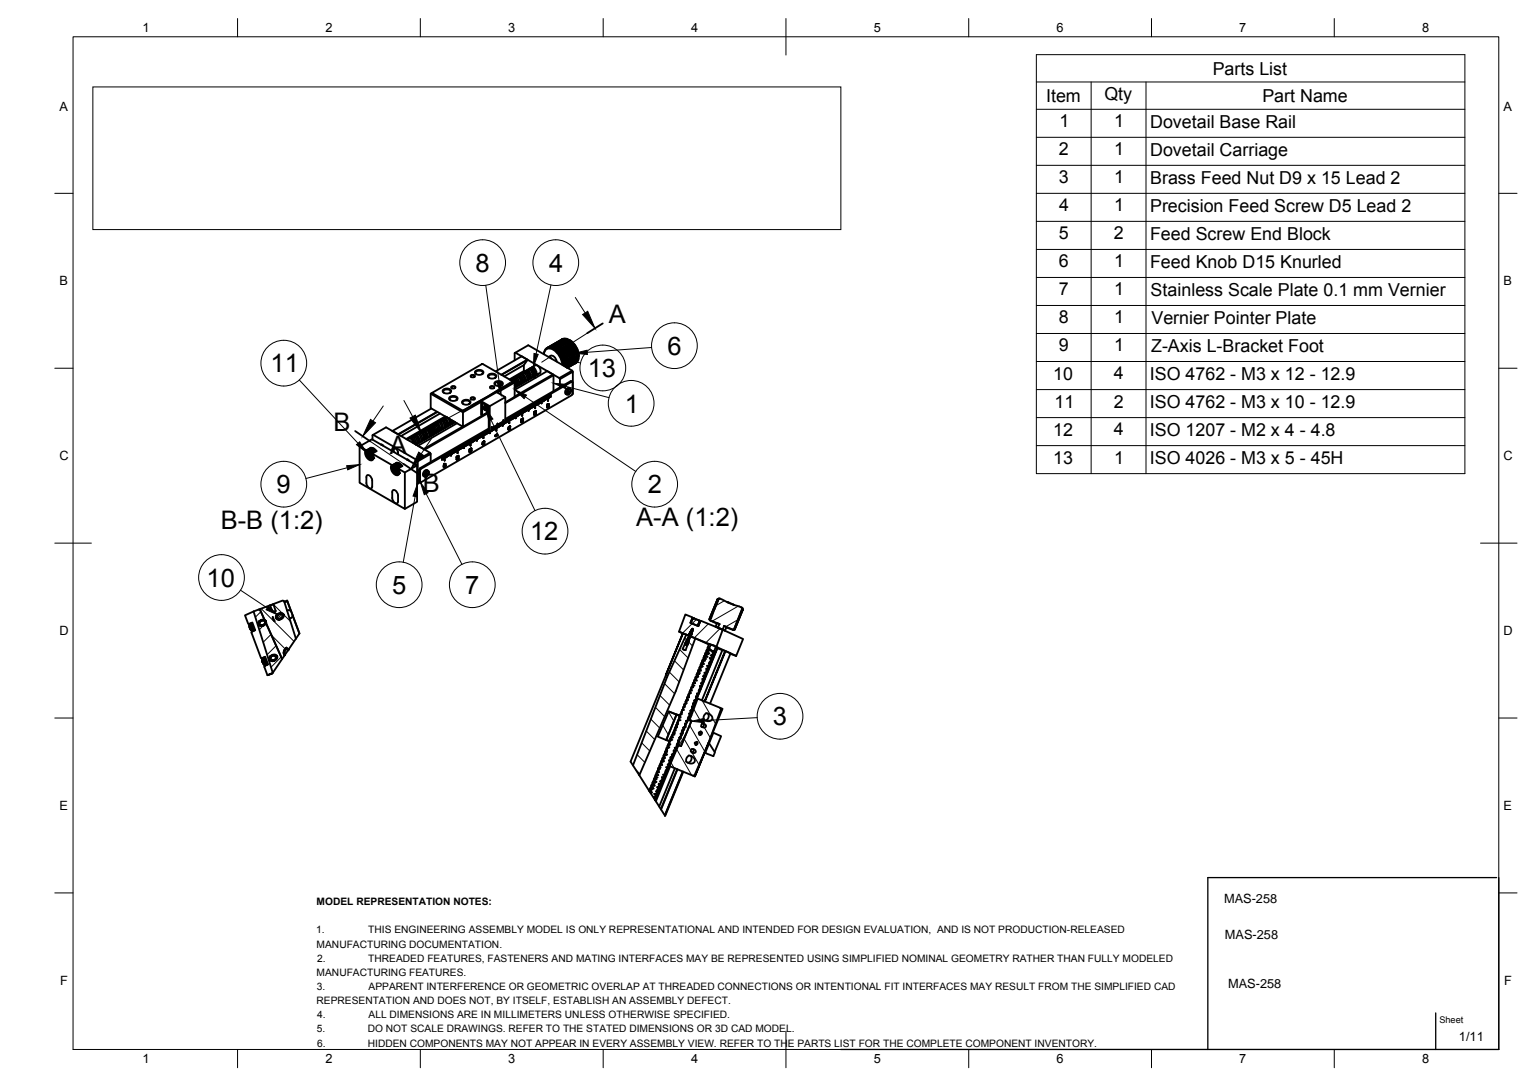
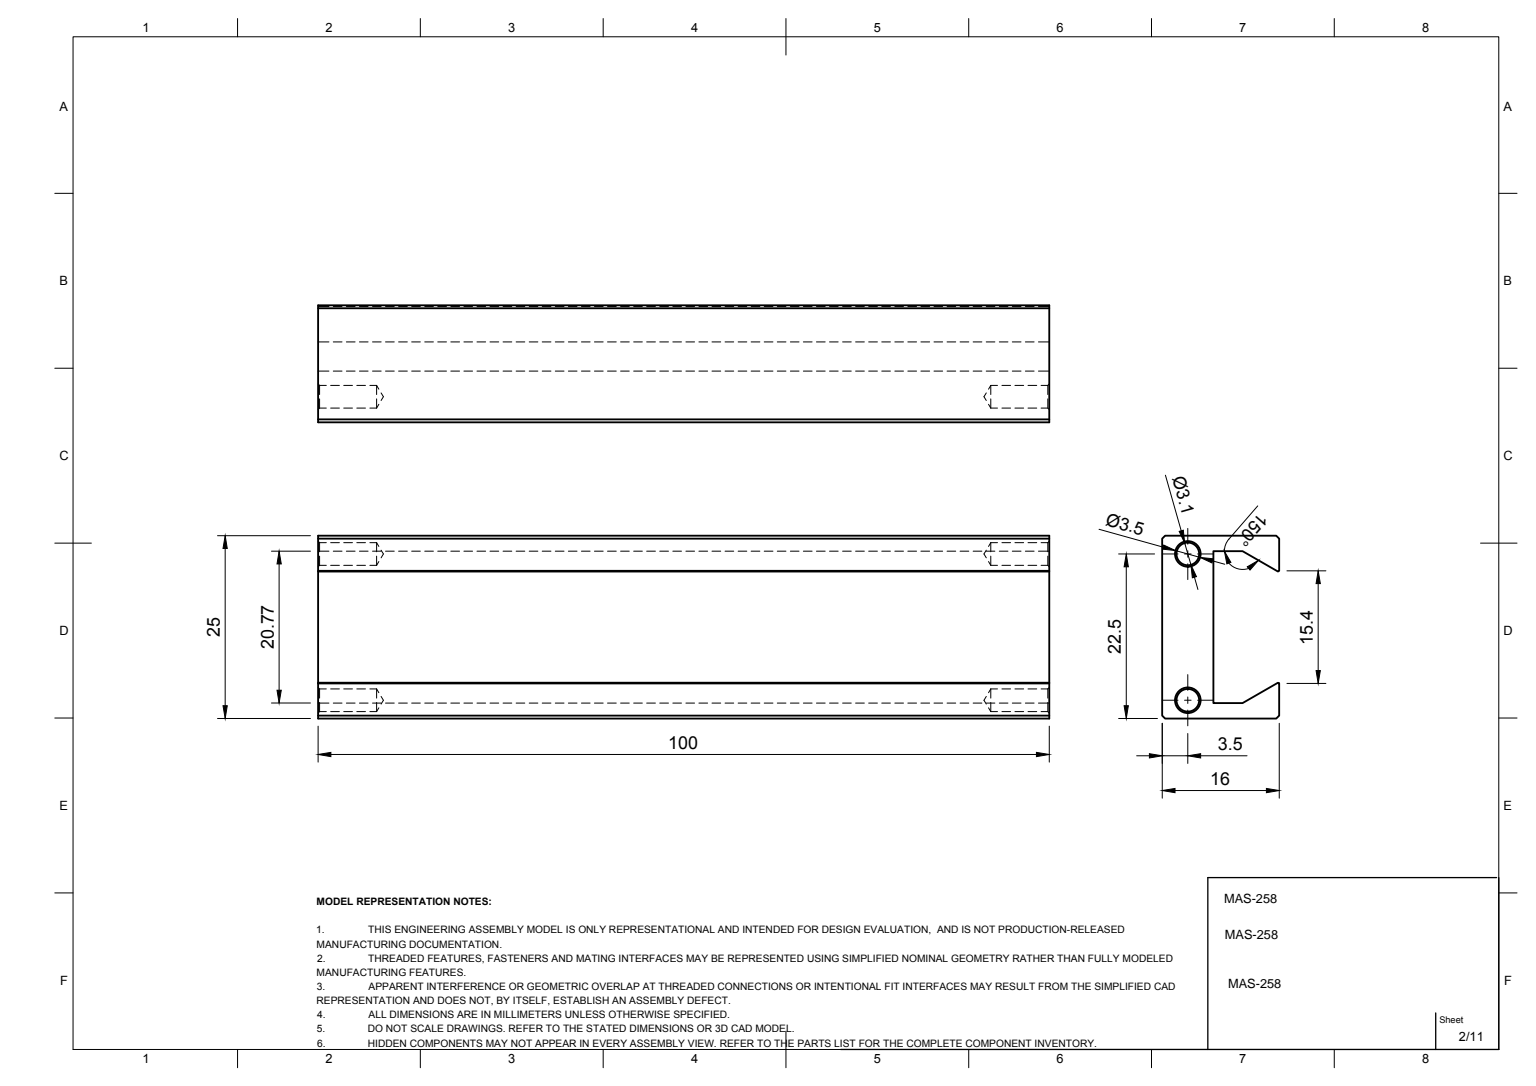
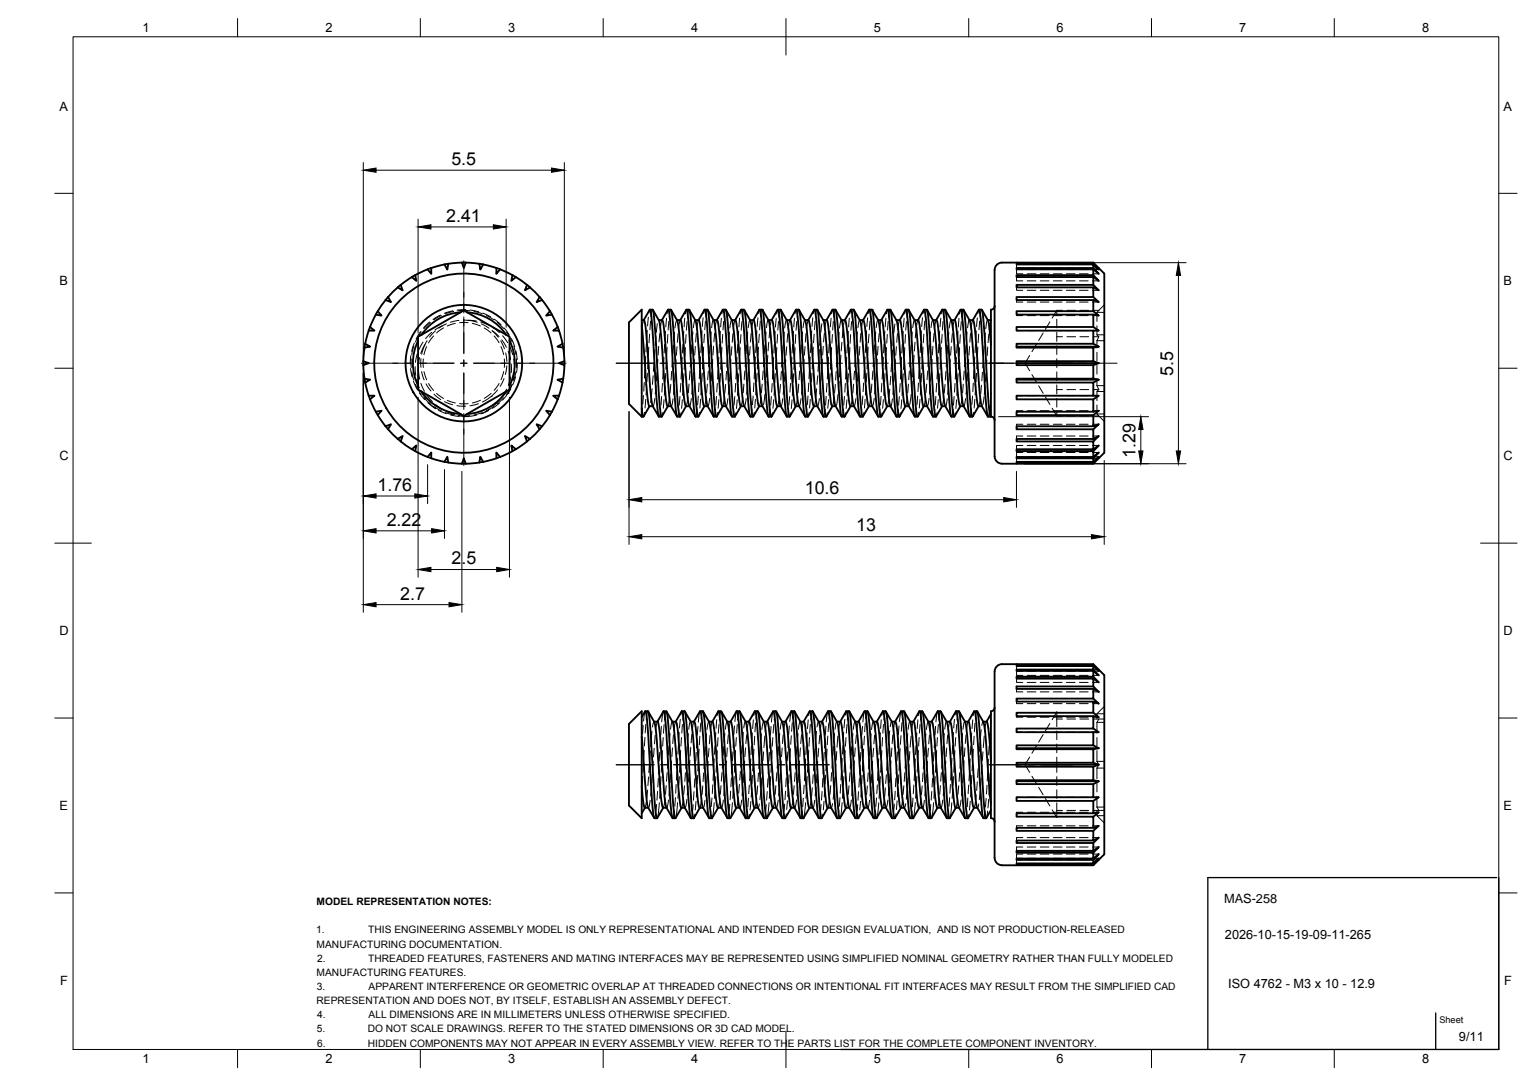
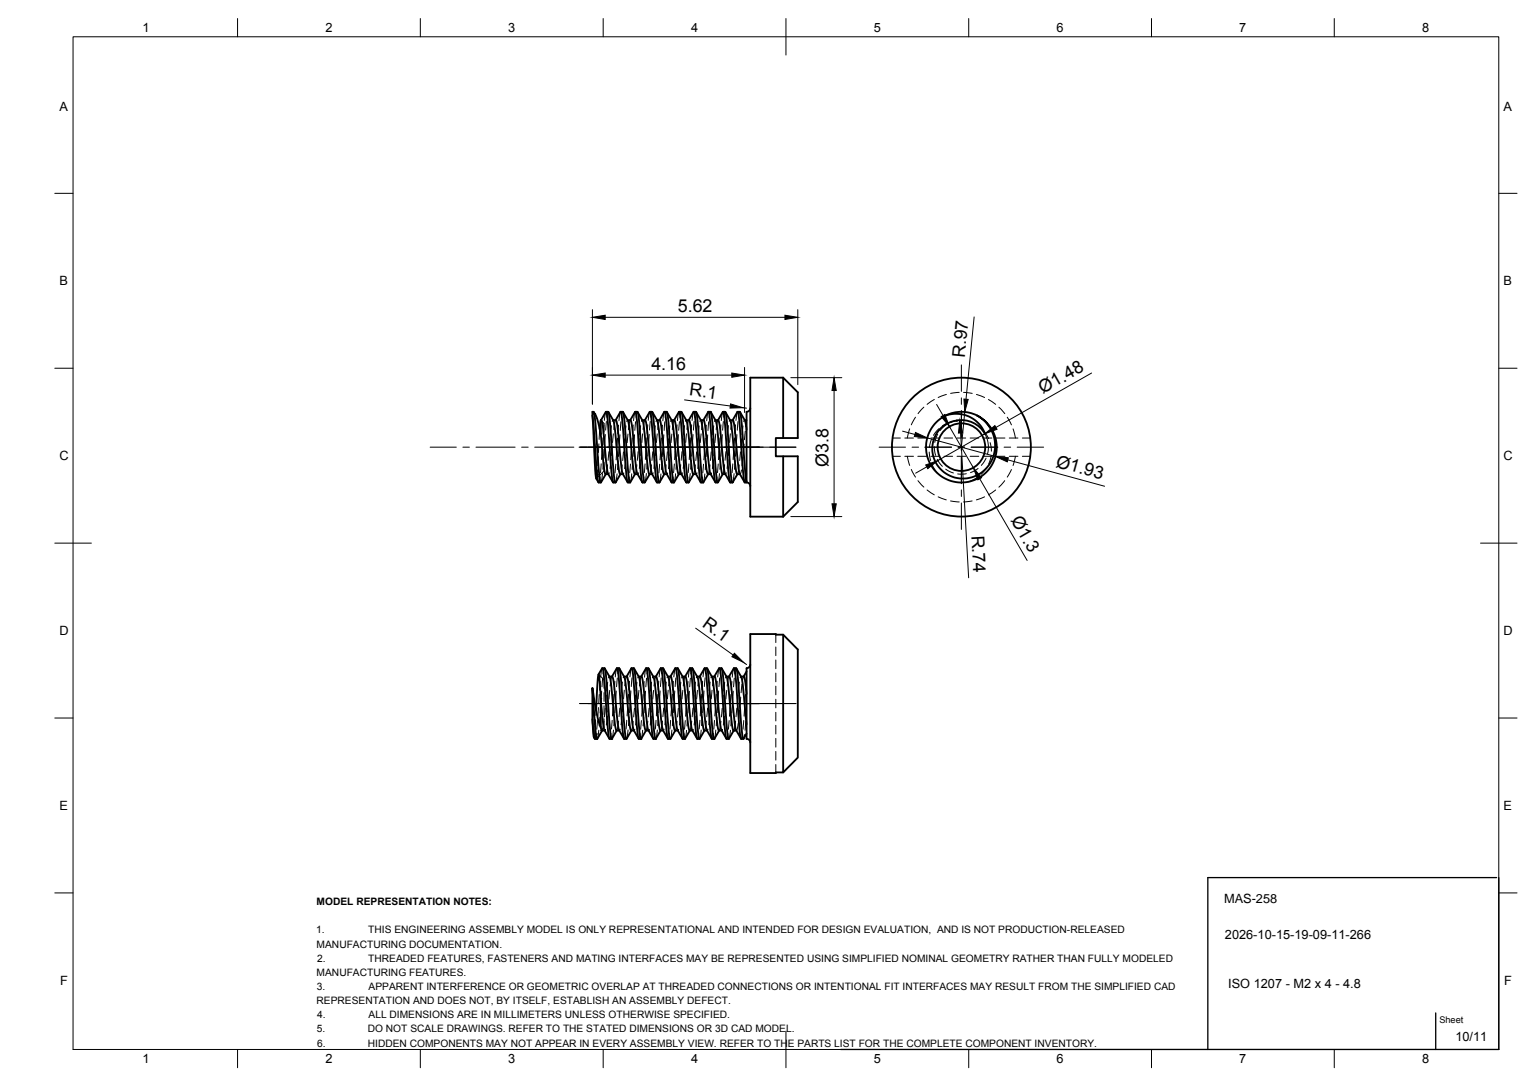
ISO-10303-21;
HEADER;
/* Generated by software containing ST-Developer
 * from STEP Tools, Inc. (www.steptools.com) 
 */

FILE_DESCRIPTION(
/* description */ (''),
/* implementation_level */ '2;1');

FILE_NAME(
/* name */ 'MAS-258',
/* time_stamp */ '2026-10-15T12:29:06-07:00',
/* author */ (''),
/* organization */ (''),
/* preprocessor_version */ 'ST-DEVELOPER v20.2',
/* originating_system */ 'Autodesk Translation Framework v15.15.0.0',
/* authorisation */ '');

FILE_SCHEMA (('AUTOMOTIVE_DESIGN { 1 0 10303 214 3 1 1 }'));
ENDSEC;

DATA;
#10=MECHANICAL_DESIGN_GEOMETRIC_PRESENTATION_REPRESENTATION('',(#1739,#1740,
#1741,#1742,#1743,#1744,#1745,#1746,#1747,#1748,#1749,#1750,#1751),#135282);
#11=ITEM_DEFINED_TRANSFORMATION($,$,#32233,#34203);
#12=ITEM_DEFINED_TRANSFORMATION($,$,#32276,#34204);
#13=ITEM_DEFINED_TRANSFORMATION($,$,#32384,#34205);
#14=ITEM_DEFINED_TRANSFORMATION($,$,#32403,#34206);
#15=ITEM_DEFINED_TRANSFORMATION($,$,#33493,#34207);
#16=ITEM_DEFINED_TRANSFORMATION($,$,#32477,#34208);
#17=ITEM_DEFINED_TRANSFORMATION($,$,#32757,#34209);
#18=ITEM_DEFINED_TRANSFORMATION($,$,#33287,#34210);
#19=ITEM_DEFINED_TRANSFORMATION($,$,#33359,#34211);
#20=ITEM_DEFINED_TRANSFORMATION($,$,#33555,#34212);
#21=ITEM_DEFINED_TRANSFORMATION($,$,#33856,#34213);
#22=ITEM_DEFINED_TRANSFORMATION($,$,#34149,#34214);
#23=ITEM_DEFINED_TRANSFORMATION($,$,#33412,#34215);
#24=ITEM_DEFINED_TRANSFORMATION($,$,#33493,#34216);
#25=ITEM_DEFINED_TRANSFORMATION($,$,#33555,#34217);
#26=ITEM_DEFINED_TRANSFORMATION($,$,#33555,#34218);
#27=ITEM_DEFINED_TRANSFORMATION($,$,#33555,#34219);
#28=ITEM_DEFINED_TRANSFORMATION($,$,#33856,#34220);
#29=ITEM_DEFINED_TRANSFORMATION($,$,#34149,#34221);
#30=ITEM_DEFINED_TRANSFORMATION($,$,#34149,#34222);
#31=ITEM_DEFINED_TRANSFORMATION($,$,#34149,#34223);
#32=(
REPRESENTATION_RELATIONSHIP($,$,#135337,#135336)
REPRESENTATION_RELATIONSHIP_WITH_TRANSFORMATION(#11)
SHAPE_REPRESENTATION_RELATIONSHIP()
);
#33=(
REPRESENTATION_RELATIONSHIP($,$,#135338,#135336)
REPRESENTATION_RELATIONSHIP_WITH_TRANSFORMATION(#12)
SHAPE_REPRESENTATION_RELATIONSHIP()
);
#34=(
REPRESENTATION_RELATIONSHIP($,$,#135339,#135336)
REPRESENTATION_RELATIONSHIP_WITH_TRANSFORMATION(#13)
SHAPE_REPRESENTATION_RELATIONSHIP()
);
#35=(
REPRESENTATION_RELATIONSHIP($,$,#135340,#135336)
REPRESENTATION_RELATIONSHIP_WITH_TRANSFORMATION(#14)
SHAPE_REPRESENTATION_RELATIONSHIP()
);
#36=(
REPRESENTATION_RELATIONSHIP($,$,#135346,#135336)
REPRESENTATION_RELATIONSHIP_WITH_TRANSFORMATION(#15)
SHAPE_REPRESENTATION_RELATIONSHIP()
);
#37=(
REPRESENTATION_RELATIONSHIP($,$,#135341,#135336)
REPRESENTATION_RELATIONSHIP_WITH_TRANSFORMATION(#16)
SHAPE_REPRESENTATION_RELATIONSHIP()
);
#38=(
REPRESENTATION_RELATIONSHIP($,$,#135342,#135336)
REPRESENTATION_RELATIONSHIP_WITH_TRANSFORMATION(#17)
SHAPE_REPRESENTATION_RELATIONSHIP()
);
#39=(
REPRESENTATION_RELATIONSHIP($,$,#135343,#135336)
REPRESENTATION_RELATIONSHIP_WITH_TRANSFORMATION(#18)
SHAPE_REPRESENTATION_RELATIONSHIP()
);
#40=(
REPRESENTATION_RELATIONSHIP($,$,#135344,#135336)
REPRESENTATION_RELATIONSHIP_WITH_TRANSFORMATION(#19)
SHAPE_REPRESENTATION_RELATIONSHIP()
);
#41=(
REPRESENTATION_RELATIONSHIP($,$,#135347,#135336)
REPRESENTATION_RELATIONSHIP_WITH_TRANSFORMATION(#20)
SHAPE_REPRESENTATION_RELATIONSHIP()
);
#42=(
REPRESENTATION_RELATIONSHIP($,$,#135348,#135336)
REPRESENTATION_RELATIONSHIP_WITH_TRANSFORMATION(#21)
SHAPE_REPRESENTATION_RELATIONSHIP()
);
#43=(
REPRESENTATION_RELATIONSHIP($,$,#135349,#135336)
REPRESENTATION_RELATIONSHIP_WITH_TRANSFORMATION(#22)
SHAPE_REPRESENTATION_RELATIONSHIP()
);
#44=(
REPRESENTATION_RELATIONSHIP($,$,#135345,#135336)
REPRESENTATION_RELATIONSHIP_WITH_TRANSFORMATION(#23)
SHAPE_REPRESENTATION_RELATIONSHIP()
);
#45=(
REPRESENTATION_RELATIONSHIP($,$,#135346,#135336)
REPRESENTATION_RELATIONSHIP_WITH_TRANSFORMATION(#24)
SHAPE_REPRESENTATION_RELATIONSHIP()
);
#46=(
REPRESENTATION_RELATIONSHIP($,$,#135347,#135336)
REPRESENTATION_RELATIONSHIP_WITH_TRANSFORMATION(#25)
SHAPE_REPRESENTATION_RELATIONSHIP()
);
#47=(
REPRESENTATION_RELATIONSHIP($,$,#135347,#135336)
REPRESENTATION_RELATIONSHIP_WITH_TRANSFORMATION(#26)
SHAPE_REPRESENTATION_RELATIONSHIP()
);
#48=(
REPRESENTATION_RELATIONSHIP($,$,#135347,#135336)
REPRESENTATION_RELATIONSHIP_WITH_TRANSFORMATION(#27)
SHAPE_REPRESENTATION_RELATIONSHIP()
);
#49=(
REPRESENTATION_RELATIONSHIP($,$,#135348,#135336)
REPRESENTATION_RELATIONSHIP_WITH_TRANSFORMATION(#28)
SHAPE_REPRESENTATION_RELATIONSHIP()
);
#50=(
REPRESENTATION_RELATIONSHIP($,$,#135349,#135336)
REPRESENTATION_RELATIONSHIP_WITH_TRANSFORMATION(#29)
SHAPE_REPRESENTATION_RELATIONSHIP()
);
#51=(
REPRESENTATION_RELATIONSHIP($,$,#135349,#135336)
REPRESENTATION_RELATIONSHIP_WITH_TRANSFORMATION(#30)
SHAPE_REPRESENTATION_RELATIONSHIP()
);
#52=(
REPRESENTATION_RELATIONSHIP($,$,#135349,#135336)
REPRESENTATION_RELATIONSHIP_WITH_TRANSFORMATION(#31)
SHAPE_REPRESENTATION_RELATIONSHIP()
);
#53=CONTEXT_DEPENDENT_SHAPE_REPRESENTATION(#32,#135315);
#54=CONTEXT_DEPENDENT_SHAPE_REPRESENTATION(#33,#135316);
#55=CONTEXT_DEPENDENT_SHAPE_REPRESENTATION(#34,#135317);
#56=CONTEXT_DEPENDENT_SHAPE_REPRESENTATION(#35,#135318);
#57=CONTEXT_DEPENDENT_SHAPE_REPRESENTATION(#36,#135319);
#58=CONTEXT_DEPENDENT_SHAPE_REPRESENTATION(#37,#135320);
#59=CONTEXT_DEPENDENT_SHAPE_REPRESENTATION(#38,#135321);
#60=CONTEXT_DEPENDENT_SHAPE_REPRESENTATION(#39,#135322);
#61=CONTEXT_DEPENDENT_SHAPE_REPRESENTATION(#40,#135323);
#62=CONTEXT_DEPENDENT_SHAPE_REPRESENTATION(#41,#135324);
#63=CONTEXT_DEPENDENT_SHAPE_REPRESENTATION(#42,#135325);
#64=CONTEXT_DEPENDENT_SHAPE_REPRESENTATION(#43,#135326);
#65=CONTEXT_DEPENDENT_SHAPE_REPRESENTATION(#44,#135327);
#66=CONTEXT_DEPENDENT_SHAPE_REPRESENTATION(#45,#135328);
#67=CONTEXT_DEPENDENT_SHAPE_REPRESENTATION(#46,#135329);
#68=CONTEXT_DEPENDENT_SHAPE_REPRESENTATION(#47,#135330);
#69=CONTEXT_DEPENDENT_SHAPE_REPRESENTATION(#48,#135331);
#70=CONTEXT_DEPENDENT_SHAPE_REPRESENTATION(#49,#135332);
#71=CONTEXT_DEPENDENT_SHAPE_REPRESENTATION(#50,#135333);
#72=CONTEXT_DEPENDENT_SHAPE_REPRESENTATION(#51,#135334);
#73=CONTEXT_DEPENDENT_SHAPE_REPRESENTATION(#52,#135335);
#74=NEXT_ASSEMBLY_USAGE_OCCURRENCE('Dovetail Base Rail:1',
'Dovetail Base Rail:1','Dovetail Base Rail:1',#135351,#135352,
'Dovetail Base Rail:1');
#75=NEXT_ASSEMBLY_USAGE_OCCURRENCE('Dovetail Carriage:1',
'Dovetail Carriage:1','Dovetail Carriage:1',#135351,#135353,
'Dovetail Carriage:1');
#76=NEXT_ASSEMBLY_USAGE_OCCURRENCE('Brass Feed Nut D9 x 15 Lead 2:1',
'Brass Feed Nut D9 x 15 Lead 2:1','Brass Feed Nut D9 x 15 Lead 2:1',#135351,
#135354,'Brass Feed Nut D9 x 15 Lead 2:1');
#77=NEXT_ASSEMBLY_USAGE_OCCURRENCE('Precision Feed Screw D5 Lead 2:1',
'Precision Feed Screw D5 Lead 2:1','Precision Feed Screw D5 Lead 2:1',#135351,
#135355,'Precision Feed Screw D5 Lead 2:1');
#78=NEXT_ASSEMBLY_USAGE_OCCURRENCE('Feed Screw End Block:1',
'Feed Screw End Block:1','Feed Screw End Block:1',#135351,#135361,
'Feed Screw End Block:1');
#79=NEXT_ASSEMBLY_USAGE_OCCURRENCE('Feed Knob D15 Knurled:1',
'Feed Knob D15 Knurled:1','Feed Knob D15 Knurled:1',#135351,#135356,
'Feed Knob D15 Knurled:1');
#80=NEXT_ASSEMBLY_USAGE_OCCURRENCE(
'Stainless Scale Plate 0.1 mm Vernier:1',
'Stainless Scale Plate 0.1 mm Vernier:1',
'Stainless Scale Plate 0.1 mm Vernier:1',#135351,#135357,
'Stainless Scale Plate 0.1 mm Vernier:1');
#81=NEXT_ASSEMBLY_USAGE_OCCURRENCE('Vernier Pointer Plate:1',
'Vernier Pointer Plate:1','Vernier Pointer Plate:1',#135351,#135358,
'Vernier Pointer Plate:1');
#82=NEXT_ASSEMBLY_USAGE_OCCURRENCE('Z-Axis L-Bracket Foot:1',
'Z-Axis L-Bracket Foot:1','Z-Axis L-Bracket Foot:1',#135351,#135359,
'Z-Axis L-Bracket Foot:1');
#83=NEXT_ASSEMBLY_USAGE_OCCURRENCE('ISO 4762 - M3 x 12 - 12.9:1',
'ISO 4762 - M3 x 12 - 12.9:1','ISO 4762 - M3 x 12 - 12.9:1',#135351,#135362,
'ISO 4762 - M3 x 12 - 12.9:1');
#84=NEXT_ASSEMBLY_USAGE_OCCURRENCE('ISO 4762 - M3 x 10 - 12.9:1',
'ISO 4762 - M3 x 10 - 12.9:1','ISO 4762 - M3 x 10 - 12.9:1',#135351,#135363,
'ISO 4762 - M3 x 10 - 12.9:1');
#85=NEXT_ASSEMBLY_USAGE_OCCURRENCE('ISO 1207 - M2 x 4 - 4.8:1',
'ISO 1207 - M2 x 4 - 4.8:1','ISO 1207 - M2 x 4 - 4.8:1',#135351,#135364,
'ISO 1207 - M2 x 4 - 4.8:1');
#86=NEXT_ASSEMBLY_USAGE_OCCURRENCE('ISO 4026 - M3 x 5 - 45H:1',
'ISO 4026 - M3 x 5 - 45H:1','ISO 4026 - M3 x 5 - 45H:1',#135351,#135360,
'ISO 4026 - M3 x 5 - 45H:1');
#87=NEXT_ASSEMBLY_USAGE_OCCURRENCE('Feed Screw End Block:2',
'Feed Screw End Block:2','Feed Screw End Block:2',#135351,#135361,
'Feed Screw End Block:2');
#88=NEXT_ASSEMBLY_USAGE_OCCURRENCE('ISO 4762 - M3 x 12 - 12.9:2',
'ISO 4762 - M3 x 12 - 12.9:2','ISO 4762 - M3 x 12 - 12.9:2',#135351,#135362,
'ISO 4762 - M3 x 12 - 12.9:2');
#89=NEXT_ASSEMBLY_USAGE_OCCURRENCE('ISO 4762 - M3 x 12 - 12.9:3',
'ISO 4762 - M3 x 12 - 12.9:3','ISO 4762 - M3 x 12 - 12.9:3',#135351,#135362,
'ISO 4762 - M3 x 12 - 12.9:3');
#90=NEXT_ASSEMBLY_USAGE_OCCURRENCE('ISO 4762 - M3 x 12 - 12.9:4',
'ISO 4762 - M3 x 12 - 12.9:4','ISO 4762 - M3 x 12 - 12.9:4',#135351,#135362,
'ISO 4762 - M3 x 12 - 12.9:4');
#91=NEXT_ASSEMBLY_USAGE_OCCURRENCE('ISO 4762 - M3 x 10 - 12.9:2',
'ISO 4762 - M3 x 10 - 12.9:2','ISO 4762 - M3 x 10 - 12.9:2',#135351,#135363,
'ISO 4762 - M3 x 10 - 12.9:2');
#92=NEXT_ASSEMBLY_USAGE_OCCURRENCE('ISO 1207 - M2 x 4 - 4.8:2',
'ISO 1207 - M2 x 4 - 4.8:2','ISO 1207 - M2 x 4 - 4.8:2',#135351,#135364,
'ISO 1207 - M2 x 4 - 4.8:2');
#93=NEXT_ASSEMBLY_USAGE_OCCURRENCE('ISO 1207 - M2 x 4 - 4.8:3',
'ISO 1207 - M2 x 4 - 4.8:3','ISO 1207 - M2 x 4 - 4.8:3',#135351,#135364,
'ISO 1207 - M2 x 4 - 4.8:3');
#94=NEXT_ASSEMBLY_USAGE_OCCURRENCE('ISO 1207 - M2 x 4 - 4.8:4',
'ISO 1207 - M2 x 4 - 4.8:4','ISO 1207 - M2 x 4 - 4.8:4',#135351,#135364,
'ISO 1207 - M2 x 4 - 4.8:4');
#95=TOROIDAL_SURFACE('',#33614,1.5635,0.1);
#96=TOROIDAL_SURFACE('',#33808,2.55,0.2);
#97=TOROIDAL_SURFACE('',#33907,1.5635,0.1);
#98=TOROIDAL_SURFACE('',#34101,2.55,0.2);
#99=TOROIDAL_SURFACE('',#34180,1.06675,0.1);
#100=(
BOUNDED_CURVE()
B_SPLINE_CURVE(2,(#76990,#76991,#76992),.UNSPECIFIED.,.F.,.F.)
B_SPLINE_CURVE_WITH_KNOTS((3,3),(0.557415897727321,0.585832740635072),
 .UNSPECIFIED.)
CURVE()
GEOMETRIC_REPRESENTATION_ITEM()
RATIONAL_B_SPLINE_CURVE((1.06,1.03152938818342,1.))
REPRESENTATION_ITEM('')
);
#101=(
BOUNDED_CURVE()
B_SPLINE_CURVE(2,(#76996,#76997,#76998),.UNSPECIFIED.,.F.,.F.)
B_SPLINE_CURVE_WITH_KNOTS((3,3),(0.,0.0284168429077509),.UNSPECIFIED.)
CURVE()
GEOMETRIC_REPRESENTATION_ITEM()
RATIONAL_B_SPLINE_CURVE((1.,1.03152938818342,1.06))
REPRESENTATION_ITEM('')
);
#102=(
BOUNDED_CURVE()
B_SPLINE_CURVE(2,(#77032,#77033,#77034),.UNSPECIFIED.,.F.,.F.)
B_SPLINE_CURVE_WITH_KNOTS((3,3),(0.557415897727321,0.585832740635072),
 .UNSPECIFIED.)
CURVE()
GEOMETRIC_REPRESENTATION_ITEM()
RATIONAL_B_SPLINE_CURVE((1.06,1.03152938818342,1.))
REPRESENTATION_ITEM('')
);
#103=(
BOUNDED_CURVE()
B_SPLINE_CURVE(2,(#77036,#77037,#77038),.UNSPECIFIED.,.F.,.F.)
B_SPLINE_CURVE_WITH_KNOTS((3,3),(0.,0.028416842907751),.UNSPECIFIED.)
CURVE()
GEOMETRIC_REPRESENTATION_ITEM()
RATIONAL_B_SPLINE_CURVE((1.,1.03152938818342,1.06))
REPRESENTATION_ITEM('')
);
#104=(
BOUNDED_CURVE()
B_SPLINE_CURVE(2,(#84021,#84022,#84023),.UNSPECIFIED.,.F.,.F.)
B_SPLINE_CURVE_WITH_KNOTS((3,3),(0.,0.0136874154102722),.UNSPECIFIED.)
CURVE()
GEOMETRIC_REPRESENTATION_ITEM()
RATIONAL_B_SPLINE_CURVE((1.,1.00669106236244,1.00897713804967))
REPRESENTATION_ITEM('')
);
#105=(
BOUNDED_CURVE()
B_SPLINE_CURVE(2,(#84027,#84028,#84029),.UNSPECIFIED.,.F.,.F.)
B_SPLINE_CURVE_WITH_KNOTS((3,3),(0.0278942541126666,0.0415816695229379),
 .UNSPECIFIED.)
CURVE()
GEOMETRIC_REPRESENTATION_ITEM()
RATIONAL_B_SPLINE_CURVE((1.00897713804926,1.00669106236213,1.))
REPRESENTATION_ITEM('')
);
#106=(
BOUNDED_CURVE()
B_SPLINE_CURVE(2,(#84031,#84032,#84033),.UNSPECIFIED.,.F.,.F.)
B_SPLINE_CURVE_WITH_KNOTS((3,3),(0.,0.0136874154102634),.UNSPECIFIED.)
CURVE()
GEOMETRIC_REPRESENTATION_ITEM()
RATIONAL_B_SPLINE_CURVE((1.,1.00669106236278,1.00897713805013))
REPRESENTATION_ITEM('')
);
#107=(
BOUNDED_CURVE()
B_SPLINE_CURVE(2,(#84037,#84038,#84039),.UNSPECIFIED.,.F.,.F.)
B_SPLINE_CURVE_WITH_KNOTS((3,3),(0.0278942541126795,0.04158166952294),
 .UNSPECIFIED.)
CURVE()
GEOMETRIC_REPRESENTATION_ITEM()
RATIONAL_B_SPLINE_CURVE((1.00897713805013,1.00669106236278,1.))
REPRESENTATION_ITEM('')
);
#108=(
BOUNDED_CURVE()
B_SPLINE_CURVE(2,(#84041,#84042,#84043),.UNSPECIFIED.,.F.,.F.)
B_SPLINE_CURVE_WITH_KNOTS((3,3),(0.,0.0136874154102606),.UNSPECIFIED.)
CURVE()
GEOMETRIC_REPRESENTATION_ITEM()
RATIONAL_B_SPLINE_CURVE((1.,1.00669106236282,1.00897713805019))
REPRESENTATION_ITEM('')
);
#109=(
BOUNDED_CURVE()
B_SPLINE_CURVE(2,(#84047,#84048,#84049),.UNSPECIFIED.,.F.,.F.)
B_SPLINE_CURVE_WITH_KNOTS((3,3),(0.0278942541126748,0.0415816695229379),
 .UNSPECIFIED.)
CURVE()
GEOMETRIC_REPRESENTATION_ITEM()
RATIONAL_B_SPLINE_CURVE((1.00897713805094,1.00669106236338,1.))
REPRESENTATION_ITEM('')
);
#110=(
BOUNDED_CURVE()
B_SPLINE_CURVE(2,(#84051,#84052,#84053),.UNSPECIFIED.,.F.,.F.)
B_SPLINE_CURVE_WITH_KNOTS((3,3),(0.,0.0136874154102637),.UNSPECIFIED.)
CURVE()
GEOMETRIC_REPRESENTATION_ITEM()
RATIONAL_B_SPLINE_CURVE((1.,1.00669106236329,1.00897713805081))
REPRESENTATION_ITEM('')
);
#111=(
BOUNDED_CURVE()
B_SPLINE_CURVE(2,(#84057,#84058,#84059),.UNSPECIFIED.,.F.,.F.)
B_SPLINE_CURVE_WITH_KNOTS((3,3),(0.0278942541126709,0.0415816695229372),
 .UNSPECIFIED.)
CURVE()
GEOMETRIC_REPRESENTATION_ITEM()
RATIONAL_B_SPLINE_CURVE((1.0089771380492,1.00669106236209,1.))
REPRESENTATION_ITEM('')
);
#112=(
BOUNDED_CURVE()
B_SPLINE_CURVE(2,(#84061,#84062,#84063),.UNSPECIFIED.,.F.,.F.)
B_SPLINE_CURVE_WITH_KNOTS((3,3),(0.,0.0136874154102607),.UNSPECIFIED.)
CURVE()
GEOMETRIC_REPRESENTATION_ITEM()
RATIONAL_B_SPLINE_CURVE((1.,1.00669106236278,1.00897713805013))
REPRESENTATION_ITEM('')
);
#113=(
BOUNDED_CURVE()
B_SPLINE_CURVE(2,(#84067,#84068,#84069),.UNSPECIFIED.,.F.,.F.)
B_SPLINE_CURVE_WITH_KNOTS((3,3),(0.0278942541126766,0.04158166952294),
 .UNSPECIFIED.)
CURVE()
GEOMETRIC_REPRESENTATION_ITEM()
RATIONAL_B_SPLINE_CURVE((1.00897713805013,1.00669106236278,1.))
REPRESENTATION_ITEM('')
);
#114=(
BOUNDED_CURVE()
B_SPLINE_CURVE(2,(#84071,#84072,#84073),.UNSPECIFIED.,.F.,.F.)
B_SPLINE_CURVE_WITH_KNOTS((3,3),(0.,0.0136874154102674),.UNSPECIFIED.)
CURVE()
GEOMETRIC_REPRESENTATION_ITEM()
RATIONAL_B_SPLINE_CURVE((1.,1.0066910623627,1.00897713805002))
REPRESENTATION_ITEM('')
);
#115=(
BOUNDED_CURVE()
B_SPLINE_CURVE(2,(#84076,#84077,#84078),.UNSPECIFIED.,.F.,.F.)
B_SPLINE_CURVE_WITH_KNOTS((3,3),(0.0278942541126671,0.0415816695229421),
 .UNSPECIFIED.)
CURVE()
GEOMETRIC_REPRESENTATION_ITEM()
RATIONAL_B_SPLINE_CURVE((1.00897713804893,1.00669106236189,1.))
REPRESENTATION_ITEM('')
);
#116=(
BOUNDED_CURVE()
B_SPLINE_CURVE(2,(#106679,#106680,#106681),.UNSPECIFIED.,.F.,.F.)
B_SPLINE_CURVE_WITH_KNOTS((3,3),(0.,0.0211644268265385),.UNSPECIFIED.)
CURVE()
GEOMETRIC_REPRESENTATION_ITEM()
RATIONAL_B_SPLINE_CURVE((1.,1.0009097917251,1.00093939181347))
REPRESENTATION_ITEM('')
);
#117=(
BOUNDED_CURVE()
B_SPLINE_CURVE(2,(#106685,#106686,#106687),.UNSPECIFIED.,.F.,.F.)
B_SPLINE_CURVE_WITH_KNOTS((3,3),(0.022587909800554,0.0437523366271111),
 .UNSPECIFIED.)
CURVE()
GEOMETRIC_REPRESENTATION_ITEM()
RATIONAL_B_SPLINE_CURVE((1.00093939181258,1.00090979172423,1.))
REPRESENTATION_ITEM('')
);
#118=(
BOUNDED_CURVE()
B_SPLINE_CURVE(2,(#106982,#106983,#106984),.UNSPECIFIED.,.F.,.F.)
B_SPLINE_CURVE_WITH_KNOTS((3,3),(0.,0.0211644268265826),.UNSPECIFIED.)
CURVE()
GEOMETRIC_REPRESENTATION_ITEM()
RATIONAL_B_SPLINE_CURVE((1.,1.00090979172134,1.00093939180958))
REPRESENTATION_ITEM('')
);
#119=(
BOUNDED_CURVE()
B_SPLINE_CURVE(2,(#106986,#106987,#106988),.UNSPECIFIED.,.F.,.F.)
B_SPLINE_CURVE_WITH_KNOTS((3,3),(0.0225879098005743,0.043752336627111),
 .UNSPECIFIED.)
CURVE()
GEOMETRIC_REPRESENTATION_ITEM()
RATIONAL_B_SPLINE_CURVE((1.00093939181478,1.00090979172637,1.))
REPRESENTATION_ITEM('')
);
#120=(
BOUNDED_CURVE()
B_SPLINE_CURVE(2,(#106993,#106994,#106995),.UNSPECIFIED.,.F.,.F.)
B_SPLINE_CURVE_WITH_KNOTS((3,3),(0.0225879098005881,0.043752336627111),
 .UNSPECIFIED.)
CURVE()
GEOMETRIC_REPRESENTATION_ITEM()
RATIONAL_B_SPLINE_CURVE((1.00093939180782,1.00090979171963,1.))
REPRESENTATION_ITEM('')
);
#121=(
BOUNDED_CURVE()
B_SPLINE_CURVE(2,(#106997,#106998,#106999),.UNSPECIFIED.,.F.,.F.)
B_SPLINE_CURVE_WITH_KNOTS((3,3),(0.,0.021164426826593),.UNSPECIFIED.)
CURVE()
GEOMETRIC_REPRESENTATION_ITEM()
RATIONAL_B_SPLINE_CURVE((1.,1.0009097917242,1.00093939181253))
REPRESENTATION_ITEM('')
);
#122=(
BOUNDED_CURVE()
B_SPLINE_CURVE(2,(#107000,#107001,#107002),.UNSPECIFIED.,.F.,.F.)
B_SPLINE_CURVE_WITH_KNOTS((3,3),(0.0225879098005839,0.0437523366271112),
 .UNSPECIFIED.)
CURVE()
GEOMETRIC_REPRESENTATION_ITEM()
RATIONAL_B_SPLINE_CURVE((1.00093939180822,1.00090979172002,1.))
REPRESENTATION_ITEM('')
);
#123=(
BOUNDED_CURVE()
B_SPLINE_CURVE(2,(#107004,#107005,#107006),.UNSPECIFIED.,.F.,.F.)
B_SPLINE_CURVE_WITH_KNOTS((3,3),(0.,0.0211644268265428),.UNSPECIFIED.)
CURVE()
GEOMETRIC_REPRESENTATION_ITEM()
RATIONAL_B_SPLINE_CURVE((1.,1.00090979172612,1.00093939181452))
REPRESENTATION_ITEM('')
);
#124=(
BOUNDED_CURVE()
B_SPLINE_CURVE(2,(#107007,#107008,#107009),.UNSPECIFIED.,.F.,.F.)
B_SPLINE_CURVE_WITH_KNOTS((3,3),(0.0225879098005574,0.0437523366271111),
 .UNSPECIFIED.)
CURVE()
GEOMETRIC_REPRESENTATION_ITEM()
RATIONAL_B_SPLINE_CURVE((1.00093939181255,1.00090979172421,1.))
REPRESENTATION_ITEM('')
);
#125=(
BOUNDED_CURVE()
B_SPLINE_CURVE(2,(#107011,#107012,#107013),.UNSPECIFIED.,.F.,.F.)
B_SPLINE_CURVE_WITH_KNOTS((3,3),(0.,0.0211644268266003),.UNSPECIFIED.)
CURVE()
GEOMETRIC_REPRESENTATION_ITEM()
RATIONAL_B_SPLINE_CURVE((1.,1.0009097917207,1.00093939180893))
REPRESENTATION_ITEM('')
);
#126=(
BOUNDED_CURVE()
B_SPLINE_CURVE(2,(#107014,#107015,#107016),.UNSPECIFIED.,.F.,.F.)
B_SPLINE_CURVE_WITH_KNOTS((3,3),(0.022587909800539,0.0437523366271111),
 .UNSPECIFIED.)
CURVE()
GEOMETRIC_REPRESENTATION_ITEM()
RATIONAL_B_SPLINE_CURVE((1.00093939181091,1.00090979172262,1.))
REPRESENTATION_ITEM('')
);
#127=(
BOUNDED_CURVE()
B_SPLINE_CURVE(2,(#107018,#107019,#107020),.UNSPECIFIED.,.F.,.F.)
B_SPLINE_CURVE_WITH_KNOTS((3,3),(0.,0.0211644268266019),.UNSPECIFIED.)
CURVE()
GEOMETRIC_REPRESENTATION_ITEM()
RATIONAL_B_SPLINE_CURVE((1.,1.0009097917251,1.00093939181347))
REPRESENTATION_ITEM('')
);
#128=(
BOUNDED_CURVE()
B_SPLINE_CURVE(2,(#107021,#107022,#107023),.UNSPECIFIED.,.F.,.F.)
B_SPLINE_CURVE_WITH_KNOTS((3,3),(0.0225879098005394,0.0437523366271111),
 .UNSPECIFIED.)
CURVE()
GEOMETRIC_REPRESENTATION_ITEM()
RATIONAL_B_SPLINE_CURVE((1.00093939181174,1.00090979172342,1.))
REPRESENTATION_ITEM('')
);
#129=(
BOUNDED_CURVE()
B_SPLINE_CURVE(2,(#107025,#107026,#107027),.UNSPECIFIED.,.F.,.F.)
B_SPLINE_CURVE_WITH_KNOTS((3,3),(0.,0.0211644268265645),.UNSPECIFIED.)
CURVE()
GEOMETRIC_REPRESENTATION_ITEM()
RATIONAL_B_SPLINE_CURVE((1.,1.00090979172128,1.00093939180953))
REPRESENTATION_ITEM('')
);
#130=(
BOUNDED_CURVE()
B_SPLINE_CURVE(2,(#107028,#107029,#107030),.UNSPECIFIED.,.F.,.F.)
B_SPLINE_CURVE_WITH_KNOTS((3,3),(0.0225879098005151,0.0437523366271111),
 .UNSPECIFIED.)
CURVE()
GEOMETRIC_REPRESENTATION_ITEM()
RATIONAL_B_SPLINE_CURVE((1.00093939181449,1.00090979172609,1.))
REPRESENTATION_ITEM('')
);
#131=(
BOUNDED_CURVE()
B_SPLINE_CURVE(2,(#107032,#107033,#107034),.UNSPECIFIED.,.F.,.F.)
B_SPLINE_CURVE_WITH_KNOTS((3,3),(0.,0.0211644268266015),.UNSPECIFIED.)
CURVE()
GEOMETRIC_REPRESENTATION_ITEM()
RATIONAL_B_SPLINE_CURVE((1.,1.00090979172521,1.00093939181358))
REPRESENTATION_ITEM('')
);
#132=(
BOUNDED_CURVE()
B_SPLINE_CURVE(2,(#107035,#107036,#107037),.UNSPECIFIED.,.F.,.F.)
B_SPLINE_CURVE_WITH_KNOTS((3,3),(0.0225879098005801,0.043752336627111),
 .UNSPECIFIED.)
CURVE()
GEOMETRIC_REPRESENTATION_ITEM()
RATIONAL_B_SPLINE_CURVE((1.00093939181248,1.00090979172414,1.))
REPRESENTATION_ITEM('')
);
#133=(
BOUNDED_CURVE()
B_SPLINE_CURVE(2,(#107039,#107040,#107041),.UNSPECIFIED.,.F.,.F.)
B_SPLINE_CURVE_WITH_KNOTS((3,3),(0.,0.0211644268265639),.UNSPECIFIED.)
CURVE()
GEOMETRIC_REPRESENTATION_ITEM()
RATIONAL_B_SPLINE_CURVE((1.,1.0009097917241,1.00093939181243))
REPRESENTATION_ITEM('')
);
#134=(
BOUNDED_CURVE()
B_SPLINE_CURVE(2,(#107042,#107043,#107044),.UNSPECIFIED.,.F.,.F.)
B_SPLINE_CURVE_WITH_KNOTS((3,3),(0.0225879098005415,0.043752336627111),
 .UNSPECIFIED.)
CURVE()
GEOMETRIC_REPRESENTATION_ITEM()
RATIONAL_B_SPLINE_CURVE((1.00093939181382,1.00090979172544,1.))
REPRESENTATION_ITEM('')
);
#135=(
BOUNDED_CURVE()
B_SPLINE_CURVE(2,(#107046,#107047,#107048),.UNSPECIFIED.,.F.,.F.)
B_SPLINE_CURVE_WITH_KNOTS((3,3),(0.,0.0211644268265226),.UNSPECIFIED.)
CURVE()
GEOMETRIC_REPRESENTATION_ITEM()
RATIONAL_B_SPLINE_CURVE((1.,1.00090979172353,1.00093939181185))
REPRESENTATION_ITEM('')
);
#136=(
BOUNDED_CURVE()
B_SPLINE_CURVE(2,(#107049,#107050,#107051),.UNSPECIFIED.,.F.,.F.)
B_SPLINE_CURVE_WITH_KNOTS((3,3),(0.0225879098005697,0.0437523366271111),
 .UNSPECIFIED.)
CURVE()
GEOMETRIC_REPRESENTATION_ITEM()
RATIONAL_B_SPLINE_CURVE((1.00093939181054,1.00090979172226,1.))
REPRESENTATION_ITEM('')
);
#137=(
BOUNDED_CURVE()
B_SPLINE_CURVE(2,(#107053,#107054,#107055),.UNSPECIFIED.,.F.,.F.)
B_SPLINE_CURVE_WITH_KNOTS((3,3),(0.,0.0211644268265259),.UNSPECIFIED.)
CURVE()
GEOMETRIC_REPRESENTATION_ITEM()
RATIONAL_B_SPLINE_CURVE((1.,1.00090979172262,1.00093939181091))
REPRESENTATION_ITEM('')
);
#138=(
BOUNDED_CURVE()
B_SPLINE_CURVE(2,(#107056,#107057,#107058),.UNSPECIFIED.,.F.,.F.)
B_SPLINE_CURVE_WITH_KNOTS((3,3),(0.0225879098005805,0.0437523366271111),
 .UNSPECIFIED.)
CURVE()
GEOMETRIC_REPRESENTATION_ITEM()
RATIONAL_B_SPLINE_CURVE((1.00093939181205,1.00090979172372,1.))
REPRESENTATION_ITEM('')
);
#139=(
BOUNDED_CURVE()
B_SPLINE_CURVE(2,(#107060,#107061,#107062),.UNSPECIFIED.,.F.,.F.)
B_SPLINE_CURVE_WITH_KNOTS((3,3),(0.,0.0211644268265664),.UNSPECIFIED.)
CURVE()
GEOMETRIC_REPRESENTATION_ITEM()
RATIONAL_B_SPLINE_CURVE((1.,1.0009097917218,1.00093939181006))
REPRESENTATION_ITEM('')
);
#140=(
BOUNDED_CURVE()
B_SPLINE_CURVE(2,(#107063,#107064,#107065),.UNSPECIFIED.,.F.,.F.)
B_SPLINE_CURVE_WITH_KNOTS((3,3),(0.0225879098005396,0.0437523366271112),
 .UNSPECIFIED.)
CURVE()
GEOMETRIC_REPRESENTATION_ITEM()
RATIONAL_B_SPLINE_CURVE((1.00093939181164,1.00090979172332,1.))
REPRESENTATION_ITEM('')
);
#141=(
BOUNDED_CURVE()
B_SPLINE_CURVE(2,(#107067,#107068,#107069),.UNSPECIFIED.,.F.,.F.)
B_SPLINE_CURVE_WITH_KNOTS((3,3),(0.,0.0211644268266089),.UNSPECIFIED.)
CURVE()
GEOMETRIC_REPRESENTATION_ITEM()
RATIONAL_B_SPLINE_CURVE((1.,1.0009097917234,1.00093939181171))
REPRESENTATION_ITEM('')
);
#142=(
BOUNDED_CURVE()
B_SPLINE_CURVE(2,(#107070,#107071,#107072),.UNSPECIFIED.,.F.,.F.)
B_SPLINE_CURVE_WITH_KNOTS((3,3),(0.0225879098005792,0.0437523366271112),
 .UNSPECIFIED.)
CURVE()
GEOMETRIC_REPRESENTATION_ITEM()
RATIONAL_B_SPLINE_CURVE((1.00093939181186,1.00090979172354,1.))
REPRESENTATION_ITEM('')
);
#143=(
BOUNDED_CURVE()
B_SPLINE_CURVE(2,(#107074,#107075,#107076),.UNSPECIFIED.,.F.,.F.)
B_SPLINE_CURVE_WITH_KNOTS((3,3),(0.,0.0211644268265289),.UNSPECIFIED.)
CURVE()
GEOMETRIC_REPRESENTATION_ITEM()
RATIONAL_B_SPLINE_CURVE((1.,1.00090979172507,1.00093939181344))
REPRESENTATION_ITEM('')
);
#144=(
BOUNDED_CURVE()
B_SPLINE_CURVE(2,(#107077,#107078,#107079),.UNSPECIFIED.,.F.,.F.)
B_SPLINE_CURVE_WITH_KNOTS((3,3),(0.0225879098005381,0.0437523366271112),
 .UNSPECIFIED.)
CURVE()
GEOMETRIC_REPRESENTATION_ITEM()
RATIONAL_B_SPLINE_CURVE((1.00093939181048,1.0009097917222,1.))
REPRESENTATION_ITEM('')
);
#145=(
BOUNDED_CURVE()
B_SPLINE_CURVE(2,(#107081,#107082,#107083),.UNSPECIFIED.,.F.,.F.)
B_SPLINE_CURVE_WITH_KNOTS((3,3),(0.,0.0211644268266039),.UNSPECIFIED.)
CURVE()
GEOMETRIC_REPRESENTATION_ITEM()
RATIONAL_B_SPLINE_CURVE((1.,1.00090979172139,1.00093939180963))
REPRESENTATION_ITEM('')
);
#146=(
BOUNDED_CURVE()
B_SPLINE_CURVE(2,(#107084,#107085,#107086),.UNSPECIFIED.,.F.,.F.)
B_SPLINE_CURVE_WITH_KNOTS((3,3),(0.0225879098005447,0.043752336627111),
 .UNSPECIFIED.)
CURVE()
GEOMETRIC_REPRESENTATION_ITEM()
RATIONAL_B_SPLINE_CURVE((1.00093939180967,1.00090979172142,1.))
REPRESENTATION_ITEM('')
);
#147=(
BOUNDED_CURVE()
B_SPLINE_CURVE(2,(#107088,#107089,#107090),.UNSPECIFIED.,.F.,.F.)
B_SPLINE_CURVE_WITH_KNOTS((3,3),(0.,0.021164426826594),.UNSPECIFIED.)
CURVE()
GEOMETRIC_REPRESENTATION_ITEM()
RATIONAL_B_SPLINE_CURVE((1.,1.00090979172174,1.00093939181))
REPRESENTATION_ITEM('')
);
#148=(
BOUNDED_CURVE()
B_SPLINE_CURVE(2,(#107091,#107092,#107093),.UNSPECIFIED.,.F.,.F.)
B_SPLINE_CURVE_WITH_KNOTS((3,3),(0.0225879098005432,0.043752336627111),
 .UNSPECIFIED.)
CURVE()
GEOMETRIC_REPRESENTATION_ITEM()
RATIONAL_B_SPLINE_CURVE((1.00093939180984,1.00090979172158,1.))
REPRESENTATION_ITEM('')
);
#149=(
BOUNDED_CURVE()
B_SPLINE_CURVE(2,(#107095,#107096,#107097),.UNSPECIFIED.,.F.,.F.)
B_SPLINE_CURVE_WITH_KNOTS((3,3),(0.,0.0211644268265628),.UNSPECIFIED.)
CURVE()
GEOMETRIC_REPRESENTATION_ITEM()
RATIONAL_B_SPLINE_CURVE((1.,1.00090979172392,1.00093939181225))
REPRESENTATION_ITEM('')
);
#150=(
BOUNDED_CURVE()
B_SPLINE_CURVE(2,(#107098,#107099,#107100),.UNSPECIFIED.,.F.,.F.)
B_SPLINE_CURVE_WITH_KNOTS((3,3),(0.0225879098005512,0.043752336627111),
 .UNSPECIFIED.)
CURVE()
GEOMETRIC_REPRESENTATION_ITEM()
RATIONAL_B_SPLINE_CURVE((1.00093939181024,1.00090979172197,1.))
REPRESENTATION_ITEM('')
);
#151=(
BOUNDED_CURVE()
B_SPLINE_CURVE(2,(#107102,#107103,#107104),.UNSPECIFIED.,.F.,.F.)
B_SPLINE_CURVE_WITH_KNOTS((3,3),(0.,0.0211644268265179),.UNSPECIFIED.)
CURVE()
GEOMETRIC_REPRESENTATION_ITEM()
RATIONAL_B_SPLINE_CURVE((1.,1.00090979172158,1.00093939180984))
REPRESENTATION_ITEM('')
);
#152=(
BOUNDED_CURVE()
B_SPLINE_CURVE(2,(#107105,#107106,#107107),.UNSPECIFIED.,.F.,.F.)
B_SPLINE_CURVE_WITH_KNOTS((3,3),(0.0225879098005361,0.043752336627111),
 .UNSPECIFIED.)
CURVE()
GEOMETRIC_REPRESENTATION_ITEM()
RATIONAL_B_SPLINE_CURVE((1.00093939181327,1.00090979172491,1.))
REPRESENTATION_ITEM('')
);
#153=(
BOUNDED_CURVE()
B_SPLINE_CURVE(2,(#107109,#107110,#107111),.UNSPECIFIED.,.F.,.F.)
B_SPLINE_CURVE_WITH_KNOTS((3,3),(0.,0.0211644268265286),.UNSPECIFIED.)
CURVE()
GEOMETRIC_REPRESENTATION_ITEM()
RATIONAL_B_SPLINE_CURVE((1.,1.00090979172298,1.00093939181129))
REPRESENTATION_ITEM('')
);
#154=(
BOUNDED_CURVE()
B_SPLINE_CURVE(2,(#107112,#107113,#107114),.UNSPECIFIED.,.F.,.F.)
B_SPLINE_CURVE_WITH_KNOTS((3,3),(0.0225879098005504,0.043752336627111),
 .UNSPECIFIED.)
CURVE()
GEOMETRIC_REPRESENTATION_ITEM()
RATIONAL_B_SPLINE_CURVE((1.00093939181167,1.00090979172335,1.))
REPRESENTATION_ITEM('')
);
#155=(
BOUNDED_CURVE()
B_SPLINE_CURVE(2,(#107116,#107117,#107118),.UNSPECIFIED.,.F.,.F.)
B_SPLINE_CURVE_WITH_KNOTS((3,3),(0.,0.0211644268266161),.UNSPECIFIED.)
CURVE()
GEOMETRIC_REPRESENTATION_ITEM()
RATIONAL_B_SPLINE_CURVE((1.,1.00090979172455,1.0009393918129))
REPRESENTATION_ITEM('')
);
#156=(
BOUNDED_CURVE()
B_SPLINE_CURVE(2,(#107119,#107120,#107121),.UNSPECIFIED.,.F.,.F.)
B_SPLINE_CURVE_WITH_KNOTS((3,3),(0.0225879098004947,0.0437523366271108),
 .UNSPECIFIED.)
CURVE()
GEOMETRIC_REPRESENTATION_ITEM()
RATIONAL_B_SPLINE_CURVE((1.0009393918129,1.00090979172455,1.))
REPRESENTATION_ITEM('')
);
#157=(
BOUNDED_CURVE()
B_SPLINE_CURVE(2,(#107123,#107124,#107125),.UNSPECIFIED.,.F.,.F.)
B_SPLINE_CURVE_WITH_KNOTS((3,3),(0.,0.0211644268265652),.UNSPECIFIED.)
CURVE()
GEOMETRIC_REPRESENTATION_ITEM()
RATIONAL_B_SPLINE_CURVE((1.,1.00090979172294,1.00093939181124))
REPRESENTATION_ITEM('')
);
#158=(
BOUNDED_CURVE()
B_SPLINE_CURVE(2,(#107126,#107127,#107128),.UNSPECIFIED.,.F.,.F.)
B_SPLINE_CURVE_WITH_KNOTS((3,3),(0.0225879098005252,0.043752336627111),
 .UNSPECIFIED.)
CURVE()
GEOMETRIC_REPRESENTATION_ITEM()
RATIONAL_B_SPLINE_CURVE((1.00093939181149,1.00090979172318,1.))
REPRESENTATION_ITEM('')
);
#159=(
BOUNDED_CURVE()
B_SPLINE_CURVE(2,(#107130,#107131,#107132),.UNSPECIFIED.,.F.,.F.)
B_SPLINE_CURVE_WITH_KNOTS((3,3),(0.,0.0211644268265705),.UNSPECIFIED.)
CURVE()
GEOMETRIC_REPRESENTATION_ITEM()
RATIONAL_B_SPLINE_CURVE((1.,1.00090979172216,1.00093939181044))
REPRESENTATION_ITEM('')
);
#160=(
BOUNDED_CURVE()
B_SPLINE_CURVE(2,(#107133,#107134,#107135),.UNSPECIFIED.,.F.,.F.)
B_SPLINE_CURVE_WITH_KNOTS((3,3),(0.0225879098005481,0.043752336627111),
 .UNSPECIFIED.)
CURVE()
GEOMETRIC_REPRESENTATION_ITEM()
RATIONAL_B_SPLINE_CURVE((1.00093939181285,1.0009097917245,1.))
REPRESENTATION_ITEM('')
);
#161=(
BOUNDED_CURVE()
B_SPLINE_CURVE(2,(#107137,#107138,#107139),.UNSPECIFIED.,.F.,.F.)
B_SPLINE_CURVE_WITH_KNOTS((3,3),(0.,0.0211644268265925),.UNSPECIFIED.)
CURVE()
GEOMETRIC_REPRESENTATION_ITEM()
RATIONAL_B_SPLINE_CURVE((1.,1.0009097917218,1.00093939181007))
REPRESENTATION_ITEM('')
);
#162=(
BOUNDED_CURVE()
B_SPLINE_CURVE(2,(#107140,#107141,#107142),.UNSPECIFIED.,.F.,.F.)
B_SPLINE_CURVE_WITH_KNOTS((3,3),(0.0225879098005822,0.0437523366271111),
 .UNSPECIFIED.)
CURVE()
GEOMETRIC_REPRESENTATION_ITEM()
RATIONAL_B_SPLINE_CURVE((1.00093939181221,1.00090979172388,1.))
REPRESENTATION_ITEM('')
);
#163=(
BOUNDED_CURVE()
B_SPLINE_CURVE(2,(#107144,#107145,#107146),.UNSPECIFIED.,.F.,.F.)
B_SPLINE_CURVE_WITH_KNOTS((3,3),(0.,0.0211644268265208),.UNSPECIFIED.)
CURVE()
GEOMETRIC_REPRESENTATION_ITEM()
RATIONAL_B_SPLINE_CURVE((1.,1.00090979172231,1.00093939181059))
REPRESENTATION_ITEM('')
);
#164=(
BOUNDED_CURVE()
B_SPLINE_CURVE(2,(#107147,#107148,#107149),.UNSPECIFIED.,.F.,.F.)
B_SPLINE_CURVE_WITH_KNOTS((3,3),(0.0225879098005163,0.043752336627111),
 .UNSPECIFIED.)
CURVE()
GEOMETRIC_REPRESENTATION_ITEM()
RATIONAL_B_SPLINE_CURVE((1.00093939181029,1.00090979172202,1.))
REPRESENTATION_ITEM('')
);
#165=(
BOUNDED_CURVE()
B_SPLINE_CURVE(2,(#107151,#107152,#107153),.UNSPECIFIED.,.F.,.F.)
B_SPLINE_CURVE_WITH_KNOTS((3,3),(0.,0.0211644268265845),.UNSPECIFIED.)
CURVE()
GEOMETRIC_REPRESENTATION_ITEM()
RATIONAL_B_SPLINE_CURVE((1.,1.00090979172432,1.00093939181266))
REPRESENTATION_ITEM('')
);
#166=(
BOUNDED_CURVE()
B_SPLINE_CURVE(2,(#107154,#107155,#107156),.UNSPECIFIED.,.F.,.F.)
B_SPLINE_CURVE_WITH_KNOTS((3,3),(0.0225879098005664,0.043752336627111),
 .UNSPECIFIED.)
CURVE()
GEOMETRIC_REPRESENTATION_ITEM()
RATIONAL_B_SPLINE_CURVE((1.0009393918107,1.00090979172242,1.))
REPRESENTATION_ITEM('')
);
#167=(
BOUNDED_CURVE()
B_SPLINE_CURVE(2,(#107158,#107159,#107160),.UNSPECIFIED.,.F.,.F.)
B_SPLINE_CURVE_WITH_KNOTS((3,3),(0.,0.0211644268265342),.UNSPECIFIED.)
CURVE()
GEOMETRIC_REPRESENTATION_ITEM()
RATIONAL_B_SPLINE_CURVE((1.,1.00090979172415,1.00093939181249))
REPRESENTATION_ITEM('')
);
#168=(
BOUNDED_CURVE()
B_SPLINE_CURVE(2,(#107161,#107162,#107163),.UNSPECIFIED.,.F.,.F.)
B_SPLINE_CURVE_WITH_KNOTS((3,3),(0.0225879098005407,0.043752336627111),
 .UNSPECIFIED.)
CURVE()
GEOMETRIC_REPRESENTATION_ITEM()
RATIONAL_B_SPLINE_CURVE((1.00093939181109,1.0009097917228,1.))
REPRESENTATION_ITEM('')
);
#169=(
BOUNDED_CURVE()
B_SPLINE_CURVE(2,(#107165,#107166,#107167),.UNSPECIFIED.,.F.,.F.)
B_SPLINE_CURVE_WITH_KNOTS((3,3),(0.,0.0211644268265271),.UNSPECIFIED.)
CURVE()
GEOMETRIC_REPRESENTATION_ITEM()
RATIONAL_B_SPLINE_CURVE((1.,1.00090979172368,1.00093939181201))
REPRESENTATION_ITEM('')
);
#170=(
BOUNDED_CURVE()
B_SPLINE_CURVE(2,(#107168,#107169,#107170),.UNSPECIFIED.,.F.,.F.)
B_SPLINE_CURVE_WITH_KNOTS((3,3),(0.0225879098005404,0.0437523366271111),
 .UNSPECIFIED.)
CURVE()
GEOMETRIC_REPRESENTATION_ITEM()
RATIONAL_B_SPLINE_CURVE((1.00093939181205,1.00090979172373,1.))
REPRESENTATION_ITEM('')
);
#171=(
BOUNDED_CURVE()
B_SPLINE_CURVE(2,(#107172,#107173,#107174),.UNSPECIFIED.,.F.,.F.)
B_SPLINE_CURVE_WITH_KNOTS((3,3),(0.,0.0211644268265742),.UNSPECIFIED.)
CURVE()
GEOMETRIC_REPRESENTATION_ITEM()
RATIONAL_B_SPLINE_CURVE((1.,1.00090979172235,1.00093939181063))
REPRESENTATION_ITEM('')
);
#172=(
BOUNDED_CURVE()
B_SPLINE_CURVE(2,(#107175,#107176,#107177),.UNSPECIFIED.,.F.,.F.)
B_SPLINE_CURVE_WITH_KNOTS((3,3),(0.0225879098005505,0.0437523366271111),
 .UNSPECIFIED.)
CURVE()
GEOMETRIC_REPRESENTATION_ITEM()
RATIONAL_B_SPLINE_CURVE((1.00093939181362,1.00090979172525,1.))
REPRESENTATION_ITEM('')
);
#173=(
BOUNDED_CURVE()
B_SPLINE_CURVE(2,(#107179,#107180,#107181),.UNSPECIFIED.,.F.,.F.)
B_SPLINE_CURVE_WITH_KNOTS((3,3),(0.,0.0211644268265471),.UNSPECIFIED.)
CURVE()
GEOMETRIC_REPRESENTATION_ITEM()
RATIONAL_B_SPLINE_CURVE((1.,1.00090979172441,1.00093939181276))
REPRESENTATION_ITEM('')
);
#174=(
BOUNDED_CURVE()
B_SPLINE_CURVE(2,(#107182,#107183,#107184),.UNSPECIFIED.,.F.,.F.)
B_SPLINE_CURVE_WITH_KNOTS((3,3),(0.0225879098005329,0.0437523366271112),
 .UNSPECIFIED.)
CURVE()
GEOMETRIC_REPRESENTATION_ITEM()
RATIONAL_B_SPLINE_CURVE((1.00093939181116,1.00090979172287,1.))
REPRESENTATION_ITEM('')
);
#175=(
BOUNDED_CURVE()
B_SPLINE_CURVE(2,(#107186,#107187,#107188),.UNSPECIFIED.,.F.,.F.)
B_SPLINE_CURVE_WITH_KNOTS((3,3),(0.,0.021164426826566),.UNSPECIFIED.)
CURVE()
GEOMETRIC_REPRESENTATION_ITEM()
RATIONAL_B_SPLINE_CURVE((1.,1.00090979172296,1.00093939181126))
REPRESENTATION_ITEM('')
);
#176=(
BOUNDED_CURVE()
B_SPLINE_CURVE(2,(#107189,#107190,#107191),.UNSPECIFIED.,.F.,.F.)
B_SPLINE_CURVE_WITH_KNOTS((3,3),(0.0225879098005499,0.0437523366271111),
 .UNSPECIFIED.)
CURVE()
GEOMETRIC_REPRESENTATION_ITEM()
RATIONAL_B_SPLINE_CURVE((1.0009393918127,1.00090979172436,1.))
REPRESENTATION_ITEM('')
);
#177=(
BOUNDED_CURVE()
B_SPLINE_CURVE(2,(#107193,#107194,#107195),.UNSPECIFIED.,.F.,.F.)
B_SPLINE_CURVE_WITH_KNOTS((3,3),(0.,0.0211644268265843),.UNSPECIFIED.)
CURVE()
GEOMETRIC_REPRESENTATION_ITEM()
RATIONAL_B_SPLINE_CURVE((1.,1.00090979172607,1.00093939181447))
REPRESENTATION_ITEM('')
);
#178=(
BOUNDED_CURVE()
B_SPLINE_CURVE(2,(#107196,#107197,#107198),.UNSPECIFIED.,.F.,.F.)
B_SPLINE_CURVE_WITH_KNOTS((3,3),(0.0225879098005132,0.0437523366271111),
 .UNSPECIFIED.)
CURVE()
GEOMETRIC_REPRESENTATION_ITEM()
RATIONAL_B_SPLINE_CURVE((1.00093939181137,1.00090979172306,1.))
REPRESENTATION_ITEM('')
);
#179=(
BOUNDED_CURVE()
B_SPLINE_CURVE(2,(#107200,#107201,#107202),.UNSPECIFIED.,.F.,.F.)
B_SPLINE_CURVE_WITH_KNOTS((3,3),(0.,0.0211644268266212),.UNSPECIFIED.)
CURVE()
GEOMETRIC_REPRESENTATION_ITEM()
RATIONAL_B_SPLINE_CURVE((1.,1.00090979172711,1.00093939181555))
REPRESENTATION_ITEM('')
);
#180=(
BOUNDED_CURVE()
B_SPLINE_CURVE(2,(#107203,#107204,#107205),.UNSPECIFIED.,.F.,.F.)
B_SPLINE_CURVE_WITH_KNOTS((3,3),(0.0225879098005048,0.0437523366271112),
 .UNSPECIFIED.)
CURVE()
GEOMETRIC_REPRESENTATION_ITEM()
RATIONAL_B_SPLINE_CURVE((1.00093939181225,1.00090979172392,1.))
REPRESENTATION_ITEM('')
);
#181=(
BOUNDED_CURVE()
B_SPLINE_CURVE(2,(#107207,#107208,#107209),.UNSPECIFIED.,.F.,.F.)
B_SPLINE_CURVE_WITH_KNOTS((3,3),(0.,0.0211644268265508),.UNSPECIFIED.)
CURVE()
GEOMETRIC_REPRESENTATION_ITEM()
RATIONAL_B_SPLINE_CURVE((1.,1.0009097917239,1.00093939181223))
REPRESENTATION_ITEM('')
);
#182=(
BOUNDED_CURVE()
B_SPLINE_CURVE(2,(#107210,#107211,#107212),.UNSPECIFIED.,.F.,.F.)
B_SPLINE_CURVE_WITH_KNOTS((3,3),(0.0225879098005375,0.0437523366271112),
 .UNSPECIFIED.)
CURVE()
GEOMETRIC_REPRESENTATION_ITEM()
RATIONAL_B_SPLINE_CURVE((1.00093939181233,1.000909791724,1.))
REPRESENTATION_ITEM('')
);
#183=(
BOUNDED_CURVE()
B_SPLINE_CURVE(2,(#107214,#107215,#107216),.UNSPECIFIED.,.F.,.F.)
B_SPLINE_CURVE_WITH_KNOTS((3,3),(0.,0.0211644268265515),.UNSPECIFIED.)
CURVE()
GEOMETRIC_REPRESENTATION_ITEM()
RATIONAL_B_SPLINE_CURVE((1.,1.00090979172704,1.00093939181547))
REPRESENTATION_ITEM('')
);
#184=(
BOUNDED_CURVE()
B_SPLINE_CURVE(2,(#107217,#107218,#107219),.UNSPECIFIED.,.F.,.F.)
B_SPLINE_CURVE_WITH_KNOTS((3,3),(0.022587909800513,0.043752336627111),
 .UNSPECIFIED.)
CURVE()
GEOMETRIC_REPRESENTATION_ITEM()
RATIONAL_B_SPLINE_CURVE((1.00093939181505,1.00090979172663,1.))
REPRESENTATION_ITEM('')
);
#185=(
BOUNDED_CURVE()
B_SPLINE_CURVE(2,(#107221,#107222,#107223),.UNSPECIFIED.,.F.,.F.)
B_SPLINE_CURVE_WITH_KNOTS((3,3),(0.,0.0211644268265743),.UNSPECIFIED.)
CURVE()
GEOMETRIC_REPRESENTATION_ITEM()
RATIONAL_B_SPLINE_CURVE((1.,1.00090979171876,1.00093939180693))
REPRESENTATION_ITEM('')
);
#186=(
BOUNDED_CURVE()
B_SPLINE_CURVE(2,(#107224,#107225,#107226),.UNSPECIFIED.,.F.,.F.)
B_SPLINE_CURVE_WITH_KNOTS((3,3),(0.0225879098005165,0.0437523366271111),
 .UNSPECIFIED.)
CURVE()
GEOMETRIC_REPRESENTATION_ITEM()
RATIONAL_B_SPLINE_CURVE((1.00093939181478,1.00090979172637,1.))
REPRESENTATION_ITEM('')
);
#187=(
BOUNDED_CURVE()
B_SPLINE_CURVE(2,(#107227,#107228,#107229),.UNSPECIFIED.,.F.,.F.)
B_SPLINE_CURVE_WITH_KNOTS((3,3),(0.,0.0211644268265909),.UNSPECIFIED.)
CURVE()
GEOMETRIC_REPRESENTATION_ITEM()
RATIONAL_B_SPLINE_CURVE((1.,1.00090979172334,1.00093939181166))
REPRESENTATION_ITEM('')
);
#188=(
BOUNDED_CURVE()
B_SPLINE_CURVE(2,(#107479,#107480,#107481),.UNSPECIFIED.,.F.,.F.)
B_SPLINE_CURVE_WITH_KNOTS((3,3),(0.,0.0126130588257607),.UNSPECIFIED.)
CURVE()
GEOMETRIC_REPRESENTATION_ITEM()
RATIONAL_B_SPLINE_CURVE((1.,1.00234596681281,1.00329298027609))
REPRESENTATION_ITEM('')
);
#189=(
BOUNDED_CURVE()
B_SPLINE_CURVE(2,(#107485,#107486,#107487),.UNSPECIFIED.,.F.,.F.)
B_SPLINE_CURVE_WITH_KNOTS((3,3),(0.0296897347922136,0.0423027936179772),
 .UNSPECIFIED.)
CURVE()
GEOMETRIC_REPRESENTATION_ITEM()
RATIONAL_B_SPLINE_CURVE((1.00329298027575,1.00234596681257,1.))
REPRESENTATION_ITEM('')
);
#190=(
BOUNDED_CURVE()
B_SPLINE_CURVE(2,(#107489,#107490,#107491),.UNSPECIFIED.,.F.,.F.)
B_SPLINE_CURVE_WITH_KNOTS((3,3),(0.,0.0126130588257611),.UNSPECIFIED.)
CURVE()
GEOMETRIC_REPRESENTATION_ITEM()
RATIONAL_B_SPLINE_CURVE((1.,1.00234596681276,1.00329298027602))
REPRESENTATION_ITEM('')
);
#191=(
BOUNDED_CURVE()
B_SPLINE_CURVE(2,(#107495,#107496,#107497),.UNSPECIFIED.,.F.,.F.)
B_SPLINE_CURVE_WITH_KNOTS((3,3),(0.0296897347922145,0.0423027936179771),
 .UNSPECIFIED.)
CURVE()
GEOMETRIC_REPRESENTATION_ITEM()
RATIONAL_B_SPLINE_CURVE((1.00329298027584,1.00234596681264,1.))
REPRESENTATION_ITEM('')
);
#192=(
BOUNDED_CURVE()
B_SPLINE_CURVE(2,(#107499,#107500,#107501),.UNSPECIFIED.,.F.,.F.)
B_SPLINE_CURVE_WITH_KNOTS((3,3),(0.,0.0126130588257613),.UNSPECIFIED.)
CURVE()
GEOMETRIC_REPRESENTATION_ITEM()
RATIONAL_B_SPLINE_CURVE((1.,1.00234596681274,1.00329298027598))
REPRESENTATION_ITEM('')
);
#193=(
BOUNDED_CURVE()
B_SPLINE_CURVE(2,(#107505,#107506,#107507),.UNSPECIFIED.,.F.,.F.)
B_SPLINE_CURVE_WITH_KNOTS((3,3),(0.0296897347922162,0.0423027936179772),
 .UNSPECIFIED.)
CURVE()
GEOMETRIC_REPRESENTATION_ITEM()
RATIONAL_B_SPLINE_CURVE((1.00329298027606,1.00234596681279,1.))
REPRESENTATION_ITEM('')
);
#194=(
BOUNDED_CURVE()
B_SPLINE_CURVE(2,(#107509,#107510,#107511),.UNSPECIFIED.,.F.,.F.)
B_SPLINE_CURVE_WITH_KNOTS((3,3),(0.,0.0126130588257623),.UNSPECIFIED.)
CURVE()
GEOMETRIC_REPRESENTATION_ITEM()
RATIONAL_B_SPLINE_CURVE((1.,1.00234596681267,1.00329298027589))
REPRESENTATION_ITEM('')
);
#195=(
BOUNDED_CURVE()
B_SPLINE_CURVE(2,(#107515,#107516,#107517),.UNSPECIFIED.,.F.,.F.)
B_SPLINE_CURVE_WITH_KNOTS((3,3),(0.0296897347922159,0.0423027936179772),
 .UNSPECIFIED.)
CURVE()
GEOMETRIC_REPRESENTATION_ITEM()
RATIONAL_B_SPLINE_CURVE((1.00329298027606,1.00234596681279,1.))
REPRESENTATION_ITEM('')
);
#196=(
BOUNDED_CURVE()
B_SPLINE_CURVE(2,(#107519,#107520,#107521),.UNSPECIFIED.,.F.,.F.)
B_SPLINE_CURVE_WITH_KNOTS((3,3),(0.,0.0126130588257623),.UNSPECIFIED.)
CURVE()
GEOMETRIC_REPRESENTATION_ITEM()
RATIONAL_B_SPLINE_CURVE((1.,1.00234596681271,1.00329298027594))
REPRESENTATION_ITEM('')
);
#197=(
BOUNDED_CURVE()
B_SPLINE_CURVE(2,(#107525,#107526,#107527),.UNSPECIFIED.,.F.,.F.)
B_SPLINE_CURVE_WITH_KNOTS((3,3),(0.0296897347922137,0.0423027936179772),
 .UNSPECIFIED.)
CURVE()
GEOMETRIC_REPRESENTATION_ITEM()
RATIONAL_B_SPLINE_CURVE((1.00329298027579,1.0023459668126,1.))
REPRESENTATION_ITEM('')
);
#198=(
BOUNDED_CURVE()
B_SPLINE_CURVE(2,(#107529,#107530,#107531),.UNSPECIFIED.,.F.,.F.)
B_SPLINE_CURVE_WITH_KNOTS((3,3),(0.,0.0126130588257624),.UNSPECIFIED.)
CURVE()
GEOMETRIC_REPRESENTATION_ITEM()
RATIONAL_B_SPLINE_CURVE((1.,1.00234596681265,1.00329298027586))
REPRESENTATION_ITEM('')
);
#199=(
BOUNDED_CURVE()
B_SPLINE_CURVE(2,(#107534,#107535,#107536),.UNSPECIFIED.,.F.,.F.)
B_SPLINE_CURVE_WITH_KNOTS((3,3),(0.0296897347922151,0.0423027936179771),
 .UNSPECIFIED.)
CURVE()
GEOMETRIC_REPRESENTATION_ITEM()
RATIONAL_B_SPLINE_CURVE((1.00329298027587,1.00234596681266,1.))
REPRESENTATION_ITEM('')
);
#200=(
BOUNDED_CURVE()
B_SPLINE_CURVE(2,(#125959,#125960,#125961),.UNSPECIFIED.,.F.,.F.)
B_SPLINE_CURVE_WITH_KNOTS((3,3),(0.,0.0211644268265626),.UNSPECIFIED.)
CURVE()
GEOMETRIC_REPRESENTATION_ITEM()
RATIONAL_B_SPLINE_CURVE((1.,1.00090979172689,1.00093939181531))
REPRESENTATION_ITEM('')
);
#201=(
BOUNDED_CURVE()
B_SPLINE_CURVE(2,(#125965,#125966,#125967),.UNSPECIFIED.,.F.,.F.)
B_SPLINE_CURVE_WITH_KNOTS((3,3),(0.0225879098005429,0.0437523366271117),
 .UNSPECIFIED.)
CURVE()
GEOMETRIC_REPRESENTATION_ITEM()
RATIONAL_B_SPLINE_CURVE((1.00093939181021,1.00090979172194,1.))
REPRESENTATION_ITEM('')
);
#202=(
BOUNDED_CURVE()
B_SPLINE_CURVE(2,(#126262,#126263,#126264),.UNSPECIFIED.,.F.,.F.)
B_SPLINE_CURVE_WITH_KNOTS((3,3),(0.,0.0211644268265449),.UNSPECIFIED.)
CURVE()
GEOMETRIC_REPRESENTATION_ITEM()
RATIONAL_B_SPLINE_CURVE((1.,1.00090979172393,1.00093939181226))
REPRESENTATION_ITEM('')
);
#203=(
BOUNDED_CURVE()
B_SPLINE_CURVE(2,(#126266,#126267,#126268),.UNSPECIFIED.,.F.,.F.)
B_SPLINE_CURVE_WITH_KNOTS((3,3),(0.0225879098005501,0.0437523366271115),
 .UNSPECIFIED.)
CURVE()
GEOMETRIC_REPRESENTATION_ITEM()
RATIONAL_B_SPLINE_CURVE((1.00093939181012,1.00090979172185,1.))
REPRESENTATION_ITEM('')
);
#204=(
BOUNDED_CURVE()
B_SPLINE_CURVE(2,(#126273,#126274,#126275),.UNSPECIFIED.,.F.,.F.)
B_SPLINE_CURVE_WITH_KNOTS((3,3),(0.0225879098005831,0.0437523366271112),
 .UNSPECIFIED.)
CURVE()
GEOMETRIC_REPRESENTATION_ITEM()
RATIONAL_B_SPLINE_CURVE((1.0009393918114,1.0009097917231,1.))
REPRESENTATION_ITEM('')
);
#205=(
BOUNDED_CURVE()
B_SPLINE_CURVE(2,(#126277,#126278,#126279),.UNSPECIFIED.,.F.,.F.)
B_SPLINE_CURVE_WITH_KNOTS((3,3),(0.,0.0211644268265669),.UNSPECIFIED.)
CURVE()
GEOMETRIC_REPRESENTATION_ITEM()
RATIONAL_B_SPLINE_CURVE((1.,1.00090979172267,1.00093939181096))
REPRESENTATION_ITEM('')
);
#206=(
BOUNDED_CURVE()
B_SPLINE_CURVE(2,(#126280,#126281,#126282),.UNSPECIFIED.,.F.,.F.)
B_SPLINE_CURVE_WITH_KNOTS((3,3),(0.0225879098005253,0.0437523366271112),
 .UNSPECIFIED.)
CURVE()
GEOMETRIC_REPRESENTATION_ITEM()
RATIONAL_B_SPLINE_CURVE((1.00093939180879,1.00090979172056,1.))
REPRESENTATION_ITEM('')
);
#207=(
BOUNDED_CURVE()
B_SPLINE_CURVE(2,(#126284,#126285,#126286),.UNSPECIFIED.,.F.,.F.)
B_SPLINE_CURVE_WITH_KNOTS((3,3),(0.,0.0211644268265721),.UNSPECIFIED.)
CURVE()
GEOMETRIC_REPRESENTATION_ITEM()
RATIONAL_B_SPLINE_CURVE((1.,1.00090979172631,1.00093939181472))
REPRESENTATION_ITEM('')
);
#208=(
BOUNDED_CURVE()
B_SPLINE_CURVE(2,(#126287,#126288,#126289),.UNSPECIFIED.,.F.,.F.)
B_SPLINE_CURVE_WITH_KNOTS((3,3),(0.0225879098005649,0.043752336627111),
 .UNSPECIFIED.)
CURVE()
GEOMETRIC_REPRESENTATION_ITEM()
RATIONAL_B_SPLINE_CURVE((1.00093939180692,1.00090979171876,1.))
REPRESENTATION_ITEM('')
);
#209=(
BOUNDED_CURVE()
B_SPLINE_CURVE(2,(#126291,#126292,#126293),.UNSPECIFIED.,.F.,.F.)
B_SPLINE_CURVE_WITH_KNOTS((3,3),(0.,0.0211644268265702),.UNSPECIFIED.)
CURVE()
GEOMETRIC_REPRESENTATION_ITEM()
RATIONAL_B_SPLINE_CURVE((1.,1.00090979172334,1.00093939181166))
REPRESENTATION_ITEM('')
);
#210=(
BOUNDED_CURVE()
B_SPLINE_CURVE(2,(#126294,#126295,#126296),.UNSPECIFIED.,.F.,.F.)
B_SPLINE_CURVE_WITH_KNOTS((3,3),(0.0225879098005071,0.0437523366271112),
 .UNSPECIFIED.)
CURVE()
GEOMETRIC_REPRESENTATION_ITEM()
RATIONAL_B_SPLINE_CURVE((1.00093939181505,1.00090979172663,1.))
REPRESENTATION_ITEM('')
);
#211=(
BOUNDED_CURVE()
B_SPLINE_CURVE(2,(#126298,#126299,#126300),.UNSPECIFIED.,.F.,.F.)
B_SPLINE_CURVE_WITH_KNOTS((3,3),(0.,0.0211644268265989),.UNSPECIFIED.)
CURVE()
GEOMETRIC_REPRESENTATION_ITEM()
RATIONAL_B_SPLINE_CURVE((1.,1.00090979172892,1.00093939181741))
REPRESENTATION_ITEM('')
);
#212=(
BOUNDED_CURVE()
B_SPLINE_CURVE(2,(#126301,#126302,#126303),.UNSPECIFIED.,.F.,.F.)
B_SPLINE_CURVE_WITH_KNOTS((3,3),(0.0225879098005698,0.043752336627111),
 .UNSPECIFIED.)
CURVE()
GEOMETRIC_REPRESENTATION_ITEM()
RATIONAL_B_SPLINE_CURVE((1.00093939181504,1.00090979172662,1.))
REPRESENTATION_ITEM('')
);
#213=(
BOUNDED_CURVE()
B_SPLINE_CURVE(2,(#126305,#126306,#126307),.UNSPECIFIED.,.F.,.F.)
B_SPLINE_CURVE_WITH_KNOTS((3,3),(0.,0.0211644268265459),.UNSPECIFIED.)
CURVE()
GEOMETRIC_REPRESENTATION_ITEM()
RATIONAL_B_SPLINE_CURVE((1.,1.00090979172781,1.00093939181627))
REPRESENTATION_ITEM('')
);
#214=(
BOUNDED_CURVE()
B_SPLINE_CURVE(2,(#126308,#126309,#126310),.UNSPECIFIED.,.F.,.F.)
B_SPLINE_CURVE_WITH_KNOTS((3,3),(0.0225879098004806,0.043752336627111),
 .UNSPECIFIED.)
CURVE()
GEOMETRIC_REPRESENTATION_ITEM()
RATIONAL_B_SPLINE_CURVE((1.00093939180982,1.00090979172157,1.))
REPRESENTATION_ITEM('')
);
#215=(
BOUNDED_CURVE()
B_SPLINE_CURVE(2,(#126312,#126313,#126314),.UNSPECIFIED.,.F.,.F.)
B_SPLINE_CURVE_WITH_KNOTS((3,3),(0.,0.0211644268265575),.UNSPECIFIED.)
CURVE()
GEOMETRIC_REPRESENTATION_ITEM()
RATIONAL_B_SPLINE_CURVE((1.,1.00090979172714,1.00093939181558))
REPRESENTATION_ITEM('')
);
#216=(
BOUNDED_CURVE()
B_SPLINE_CURVE(2,(#126315,#126316,#126317),.UNSPECIFIED.,.F.,.F.)
B_SPLINE_CURVE_WITH_KNOTS((3,3),(0.0225879098005155,0.0437523366271111),
 .UNSPECIFIED.)
CURVE()
GEOMETRIC_REPRESENTATION_ITEM()
RATIONAL_B_SPLINE_CURVE((1.0009393918136,1.00090979172523,1.))
REPRESENTATION_ITEM('')
);
#217=(
BOUNDED_CURVE()
B_SPLINE_CURVE(2,(#126319,#126320,#126321),.UNSPECIFIED.,.F.,.F.)
B_SPLINE_CURVE_WITH_KNOTS((3,3),(0.,0.0211644268265217),.UNSPECIFIED.)
CURVE()
GEOMETRIC_REPRESENTATION_ITEM()
RATIONAL_B_SPLINE_CURVE((1.,1.00090979172259,1.00093939181088))
REPRESENTATION_ITEM('')
);
#218=(
BOUNDED_CURVE()
B_SPLINE_CURVE(2,(#126322,#126323,#126324),.UNSPECIFIED.,.F.,.F.)
B_SPLINE_CURVE_WITH_KNOTS((3,3),(0.0225879098004986,0.043752336627111),
 .UNSPECIFIED.)
CURVE()
GEOMETRIC_REPRESENTATION_ITEM()
RATIONAL_B_SPLINE_CURVE((1.00093939181162,1.00090979172331,1.))
REPRESENTATION_ITEM('')
);
#219=(
BOUNDED_CURVE()
B_SPLINE_CURVE(2,(#126326,#126327,#126328),.UNSPECIFIED.,.F.,.F.)
B_SPLINE_CURVE_WITH_KNOTS((3,3),(0.,0.0211644268265753),.UNSPECIFIED.)
CURVE()
GEOMETRIC_REPRESENTATION_ITEM()
RATIONAL_B_SPLINE_CURVE((1.,1.00090979172494,1.00093939181331))
REPRESENTATION_ITEM('')
);
#220=(
BOUNDED_CURVE()
B_SPLINE_CURVE(2,(#126329,#126330,#126331),.UNSPECIFIED.,.F.,.F.)
B_SPLINE_CURVE_WITH_KNOTS((3,3),(0.02258790980058,0.043752336627111),
 .UNSPECIFIED.)
CURVE()
GEOMETRIC_REPRESENTATION_ITEM()
RATIONAL_B_SPLINE_CURVE((1.00093939181509,1.00090979172667,1.))
REPRESENTATION_ITEM('')
);
#221=(
BOUNDED_CURVE()
B_SPLINE_CURVE(2,(#126333,#126334,#126335),.UNSPECIFIED.,.F.,.F.)
B_SPLINE_CURVE_WITH_KNOTS((3,3),(0.,0.0211644268265208),.UNSPECIFIED.)
CURVE()
GEOMETRIC_REPRESENTATION_ITEM()
RATIONAL_B_SPLINE_CURVE((1.,1.0009097917237,1.00093939181202))
REPRESENTATION_ITEM('')
);
#222=(
BOUNDED_CURVE()
B_SPLINE_CURVE(2,(#126336,#126337,#126338),.UNSPECIFIED.,.F.,.F.)
B_SPLINE_CURVE_WITH_KNOTS((3,3),(0.022587909800591,0.0437523366271109),
 .UNSPECIFIED.)
CURVE()
GEOMETRIC_REPRESENTATION_ITEM()
RATIONAL_B_SPLINE_CURVE((1.0009393918133,1.00090979172493,1.))
REPRESENTATION_ITEM('')
);
#223=(
BOUNDED_CURVE()
B_SPLINE_CURVE(2,(#126340,#126341,#126342),.UNSPECIFIED.,.F.,.F.)
B_SPLINE_CURVE_WITH_KNOTS((3,3),(0.,0.0211644268265324),.UNSPECIFIED.)
CURVE()
GEOMETRIC_REPRESENTATION_ITEM()
RATIONAL_B_SPLINE_CURVE((1.,1.00090979172547,1.00093939181385))
REPRESENTATION_ITEM('')
);
#224=(
BOUNDED_CURVE()
B_SPLINE_CURVE(2,(#126343,#126344,#126345),.UNSPECIFIED.,.F.,.F.)
B_SPLINE_CURVE_WITH_KNOTS((3,3),(0.0225879098005774,0.0437523366271109),
 .UNSPECIFIED.)
CURVE()
GEOMETRIC_REPRESENTATION_ITEM()
RATIONAL_B_SPLINE_CURVE((1.00093939181154,1.00090979172323,1.))
REPRESENTATION_ITEM('')
);
#225=(
BOUNDED_CURVE()
B_SPLINE_CURVE(2,(#126347,#126348,#126349),.UNSPECIFIED.,.F.,.F.)
B_SPLINE_CURVE_WITH_KNOTS((3,3),(0.,0.0211644268266055),.UNSPECIFIED.)
CURVE()
GEOMETRIC_REPRESENTATION_ITEM()
RATIONAL_B_SPLINE_CURVE((1.,1.00090979172398,1.00093939181232))
REPRESENTATION_ITEM('')
);
#226=(
BOUNDED_CURVE()
B_SPLINE_CURVE(2,(#126350,#126351,#126352),.UNSPECIFIED.,.F.,.F.)
B_SPLINE_CURVE_WITH_KNOTS((3,3),(0.0225879098005268,0.043752336627111),
 .UNSPECIFIED.)
CURVE()
GEOMETRIC_REPRESENTATION_ITEM()
RATIONAL_B_SPLINE_CURVE((1.00093939181403,1.00090979172564,1.))
REPRESENTATION_ITEM('')
);
#227=(
BOUNDED_CURVE()
B_SPLINE_CURVE(2,(#126354,#126355,#126356),.UNSPECIFIED.,.F.,.F.)
B_SPLINE_CURVE_WITH_KNOTS((3,3),(0.,0.0211644268265998),.UNSPECIFIED.)
CURVE()
GEOMETRIC_REPRESENTATION_ITEM()
RATIONAL_B_SPLINE_CURVE((1.,1.00090979172202,1.00093939181029))
REPRESENTATION_ITEM('')
);
#228=(
BOUNDED_CURVE()
B_SPLINE_CURVE(2,(#126357,#126358,#126359),.UNSPECIFIED.,.F.,.F.)
B_SPLINE_CURVE_WITH_KNOTS((3,3),(0.0225879098005115,0.0437523366271109),
 .UNSPECIFIED.)
CURVE()
GEOMETRIC_REPRESENTATION_ITEM()
RATIONAL_B_SPLINE_CURVE((1.00093939181353,1.00090979172516,1.))
REPRESENTATION_ITEM('')
);
#229=(
BOUNDED_CURVE()
B_SPLINE_CURVE(2,(#126361,#126362,#126363),.UNSPECIFIED.,.F.,.F.)
B_SPLINE_CURVE_WITH_KNOTS((3,3),(0.,0.0211644268266192),.UNSPECIFIED.)
CURVE()
GEOMETRIC_REPRESENTATION_ITEM()
RATIONAL_B_SPLINE_CURVE((1.,1.00090979172386,1.00093939181218))
REPRESENTATION_ITEM('')
);
#230=(
BOUNDED_CURVE()
B_SPLINE_CURVE(2,(#126364,#126365,#126366),.UNSPECIFIED.,.F.,.F.)
B_SPLINE_CURVE_WITH_KNOTS((3,3),(0.0225879098005691,0.0437523366271108),
 .UNSPECIFIED.)
CURVE()
GEOMETRIC_REPRESENTATION_ITEM()
RATIONAL_B_SPLINE_CURVE((1.00093939181287,1.00090979172452,1.))
REPRESENTATION_ITEM('')
);
#231=(
BOUNDED_CURVE()
B_SPLINE_CURVE(2,(#126368,#126369,#126370),.UNSPECIFIED.,.F.,.F.)
B_SPLINE_CURVE_WITH_KNOTS((3,3),(0.,0.0211644268265309),.UNSPECIFIED.)
CURVE()
GEOMETRIC_REPRESENTATION_ITEM()
RATIONAL_B_SPLINE_CURVE((1.,1.00090979172246,1.00093939181075))
REPRESENTATION_ITEM('')
);
#232=(
BOUNDED_CURVE()
B_SPLINE_CURVE(2,(#126371,#126372,#126373),.UNSPECIFIED.,.F.,.F.)
B_SPLINE_CURVE_WITH_KNOTS((3,3),(0.0225879098005445,0.0437523366271108),
 .UNSPECIFIED.)
CURVE()
GEOMETRIC_REPRESENTATION_ITEM()
RATIONAL_B_SPLINE_CURVE((1.00093939181122,1.00090979172292,1.))
REPRESENTATION_ITEM('')
);
#233=(
BOUNDED_CURVE()
B_SPLINE_CURVE(2,(#126375,#126376,#126377),.UNSPECIFIED.,.F.,.F.)
B_SPLINE_CURVE_WITH_KNOTS((3,3),(0.,0.0211644268266054),.UNSPECIFIED.)
CURVE()
GEOMETRIC_REPRESENTATION_ITEM()
RATIONAL_B_SPLINE_CURVE((1.,1.0009097917244,1.00093939181275))
REPRESENTATION_ITEM('')
);
#234=(
BOUNDED_CURVE()
B_SPLINE_CURVE(2,(#126378,#126379,#126380),.UNSPECIFIED.,.F.,.F.)
B_SPLINE_CURVE_WITH_KNOTS((3,3),(0.0225879098005202,0.0437523366271108),
 .UNSPECIFIED.)
CURVE()
GEOMETRIC_REPRESENTATION_ITEM()
RATIONAL_B_SPLINE_CURVE((1.00093939181333,1.00090979172497,1.))
REPRESENTATION_ITEM('')
);
#235=(
BOUNDED_CURVE()
B_SPLINE_CURVE(2,(#126382,#126383,#126384),.UNSPECIFIED.,.F.,.F.)
B_SPLINE_CURVE_WITH_KNOTS((3,3),(0.,0.0211644268265328),.UNSPECIFIED.)
CURVE()
GEOMETRIC_REPRESENTATION_ITEM()
RATIONAL_B_SPLINE_CURVE((1.,1.00090979172326,1.00093939181157))
REPRESENTATION_ITEM('')
);
#236=(
BOUNDED_CURVE()
B_SPLINE_CURVE(2,(#126385,#126386,#126387),.UNSPECIFIED.,.F.,.F.)
B_SPLINE_CURVE_WITH_KNOTS((3,3),(0.0225879098004953,0.0437523366271108),
 .UNSPECIFIED.)
CURVE()
GEOMETRIC_REPRESENTATION_ITEM()
RATIONAL_B_SPLINE_CURVE((1.0009393918111,1.00090979172281,1.))
REPRESENTATION_ITEM('')
);
#237=(
BOUNDED_CURVE()
B_SPLINE_CURVE(2,(#126389,#126390,#126391),.UNSPECIFIED.,.F.,.F.)
B_SPLINE_CURVE_WITH_KNOTS((3,3),(0.,0.0211644268265412),.UNSPECIFIED.)
CURVE()
GEOMETRIC_REPRESENTATION_ITEM()
RATIONAL_B_SPLINE_CURVE((1.,1.00090979172431,1.00093939181265))
REPRESENTATION_ITEM('')
);
#238=(
BOUNDED_CURVE()
B_SPLINE_CURVE(2,(#126392,#126393,#126394),.UNSPECIFIED.,.F.,.F.)
B_SPLINE_CURVE_WITH_KNOTS((3,3),(0.0225879098005734,0.0437523366271109),
 .UNSPECIFIED.)
CURVE()
GEOMETRIC_REPRESENTATION_ITEM()
RATIONAL_B_SPLINE_CURVE((1.00093939181328,1.00090979172492,1.))
REPRESENTATION_ITEM('')
);
#239=(
BOUNDED_CURVE()
B_SPLINE_CURVE(2,(#126396,#126397,#126398),.UNSPECIFIED.,.F.,.F.)
B_SPLINE_CURVE_WITH_KNOTS((3,3),(0.,0.0211644268265644),.UNSPECIFIED.)
CURVE()
GEOMETRIC_REPRESENTATION_ITEM()
RATIONAL_B_SPLINE_CURVE((1.,1.00090979172253,1.00093939181082))
REPRESENTATION_ITEM('')
);
#240=(
BOUNDED_CURVE()
B_SPLINE_CURVE(2,(#126399,#126400,#126401),.UNSPECIFIED.,.F.,.F.)
B_SPLINE_CURVE_WITH_KNOTS((3,3),(0.0225879098005465,0.0437523366271109),
 .UNSPECIFIED.)
CURVE()
GEOMETRIC_REPRESENTATION_ITEM()
RATIONAL_B_SPLINE_CURVE((1.00093939181082,1.00090979172253,1.))
REPRESENTATION_ITEM('')
);
#241=(
BOUNDED_CURVE()
B_SPLINE_CURVE(2,(#126403,#126404,#126405),.UNSPECIFIED.,.F.,.F.)
B_SPLINE_CURVE_WITH_KNOTS((3,3),(0.,0.0211644268265949),.UNSPECIFIED.)
CURVE()
GEOMETRIC_REPRESENTATION_ITEM()
RATIONAL_B_SPLINE_CURVE((1.,1.00090979172025,1.00093939180846))
REPRESENTATION_ITEM('')
);
#242=(
BOUNDED_CURVE()
B_SPLINE_CURVE(2,(#126406,#126407,#126408),.UNSPECIFIED.,.F.,.F.)
B_SPLINE_CURVE_WITH_KNOTS((3,3),(0.0225879098005516,0.0437523366271116),
 .UNSPECIFIED.)
CURVE()
GEOMETRIC_REPRESENTATION_ITEM()
RATIONAL_B_SPLINE_CURVE((1.00093939180938,1.00090979172114,1.))
REPRESENTATION_ITEM('')
);
#243=(
BOUNDED_CURVE()
B_SPLINE_CURVE(2,(#126410,#126411,#126412),.UNSPECIFIED.,.F.,.F.)
B_SPLINE_CURVE_WITH_KNOTS((3,3),(0.,0.0211644268265594),.UNSPECIFIED.)
CURVE()
GEOMETRIC_REPRESENTATION_ITEM()
RATIONAL_B_SPLINE_CURVE((1.,1.0009097917224,1.00093939181069))
REPRESENTATION_ITEM('')
);
#244=(
BOUNDED_CURVE()
B_SPLINE_CURVE(2,(#126413,#126414,#126415),.UNSPECIFIED.,.F.,.F.)
B_SPLINE_CURVE_WITH_KNOTS((3,3),(0.0225879098004988,0.0437523366271116),
 .UNSPECIFIED.)
CURVE()
GEOMETRIC_REPRESENTATION_ITEM()
RATIONAL_B_SPLINE_CURVE((1.00093939180876,1.00090979172054,1.))
REPRESENTATION_ITEM('')
);
#245=(
BOUNDED_CURVE()
B_SPLINE_CURVE(2,(#126417,#126418,#126419),.UNSPECIFIED.,.F.,.F.)
B_SPLINE_CURVE_WITH_KNOTS((3,3),(0.,0.0211644268266144),.UNSPECIFIED.)
CURVE()
GEOMETRIC_REPRESENTATION_ITEM()
RATIONAL_B_SPLINE_CURVE((1.,1.00090979172203,1.0009393918103))
REPRESENTATION_ITEM('')
);
#246=(
BOUNDED_CURVE()
B_SPLINE_CURVE(2,(#126420,#126421,#126422),.UNSPECIFIED.,.F.,.F.)
B_SPLINE_CURVE_WITH_KNOTS((3,3),(0.0225879098005803,0.0437523366271115),
 .UNSPECIFIED.)
CURVE()
GEOMETRIC_REPRESENTATION_ITEM()
RATIONAL_B_SPLINE_CURVE((1.00093939181596,1.00090979172751,1.))
REPRESENTATION_ITEM('')
);
#247=(
BOUNDED_CURVE()
B_SPLINE_CURVE(2,(#126424,#126425,#126426),.UNSPECIFIED.,.F.,.F.)
B_SPLINE_CURVE_WITH_KNOTS((3,3),(0.,0.0211644268265443),.UNSPECIFIED.)
CURVE()
GEOMETRIC_REPRESENTATION_ITEM()
RATIONAL_B_SPLINE_CURVE((1.,1.00090979171957,1.00093939180776))
REPRESENTATION_ITEM('')
);
#248=(
BOUNDED_CURVE()
B_SPLINE_CURVE(2,(#126427,#126428,#126429),.UNSPECIFIED.,.F.,.F.)
B_SPLINE_CURVE_WITH_KNOTS((3,3),(0.0225879098005492,0.0437523366271114),
 .UNSPECIFIED.)
CURVE()
GEOMETRIC_REPRESENTATION_ITEM()
RATIONAL_B_SPLINE_CURVE((1.00093939181166,1.00090979172334,1.))
REPRESENTATION_ITEM('')
);
#249=(
BOUNDED_CURVE()
B_SPLINE_CURVE(2,(#126431,#126432,#126433),.UNSPECIFIED.,.F.,.F.)
B_SPLINE_CURVE_WITH_KNOTS((3,3),(0.,0.0211644268265569),.UNSPECIFIED.)
CURVE()
GEOMETRIC_REPRESENTATION_ITEM()
RATIONAL_B_SPLINE_CURVE((1.,1.00090979172576,1.00093939181416))
REPRESENTATION_ITEM('')
);
#250=(
BOUNDED_CURVE()
B_SPLINE_CURVE(2,(#126434,#126435,#126436),.UNSPECIFIED.,.F.,.F.)
B_SPLINE_CURVE_WITH_KNOTS((3,3),(0.0225879098005114,0.0437523366271113),
 .UNSPECIFIED.)
CURVE()
GEOMETRIC_REPRESENTATION_ITEM()
RATIONAL_B_SPLINE_CURVE((1.00093939181229,1.00090979172396,1.))
REPRESENTATION_ITEM('')
);
#251=(
BOUNDED_CURVE()
B_SPLINE_CURVE(2,(#126438,#126439,#126440),.UNSPECIFIED.,.F.,.F.)
B_SPLINE_CURVE_WITH_KNOTS((3,3),(0.,0.021164426826552),.UNSPECIFIED.)
CURVE()
GEOMETRIC_REPRESENTATION_ITEM()
RATIONAL_B_SPLINE_CURVE((1.,1.00090979172362,1.00093939181195))
REPRESENTATION_ITEM('')
);
#252=(
BOUNDED_CURVE()
B_SPLINE_CURVE(2,(#126441,#126442,#126443),.UNSPECIFIED.,.F.,.F.)
B_SPLINE_CURVE_WITH_KNOTS((3,3),(0.0225879098005811,0.0437523366271113),
 .UNSPECIFIED.)
CURVE()
GEOMETRIC_REPRESENTATION_ITEM()
RATIONAL_B_SPLINE_CURVE((1.00093939181488,1.00090979172647,1.))
REPRESENTATION_ITEM('')
);
#253=(
BOUNDED_CURVE()
B_SPLINE_CURVE(2,(#126445,#126446,#126447),.UNSPECIFIED.,.F.,.F.)
B_SPLINE_CURVE_WITH_KNOTS((3,3),(0.,0.0211644268265175),.UNSPECIFIED.)
CURVE()
GEOMETRIC_REPRESENTATION_ITEM()
RATIONAL_B_SPLINE_CURVE((1.,1.00090979172709,1.00093939181552))
REPRESENTATION_ITEM('')
);
#254=(
BOUNDED_CURVE()
B_SPLINE_CURVE(2,(#126448,#126449,#126450),.UNSPECIFIED.,.F.,.F.)
B_SPLINE_CURVE_WITH_KNOTS((3,3),(0.0225879098005324,0.0437523366271115),
 .UNSPECIFIED.)
CURVE()
GEOMETRIC_REPRESENTATION_ITEM()
RATIONAL_B_SPLINE_CURVE((1.00093939180857,1.00090979172035,1.))
REPRESENTATION_ITEM('')
);
#255=(
BOUNDED_CURVE()
B_SPLINE_CURVE(2,(#126452,#126453,#126454),.UNSPECIFIED.,.F.,.F.)
B_SPLINE_CURVE_WITH_KNOTS((3,3),(0.,0.0211644268265537),.UNSPECIFIED.)
CURVE()
GEOMETRIC_REPRESENTATION_ITEM()
RATIONAL_B_SPLINE_CURVE((1.,1.00090979172547,1.00093939181385))
REPRESENTATION_ITEM('')
);
#256=(
BOUNDED_CURVE()
B_SPLINE_CURVE(2,(#126455,#126456,#126457),.UNSPECIFIED.,.F.,.F.)
B_SPLINE_CURVE_WITH_KNOTS((3,3),(0.022587909800574,0.0437523366271114),
 .UNSPECIFIED.)
CURVE()
GEOMETRIC_REPRESENTATION_ITEM()
RATIONAL_B_SPLINE_CURVE((1.00093939181312,1.00090979172476,1.))
REPRESENTATION_ITEM('')
);
#257=(
BOUNDED_CURVE()
B_SPLINE_CURVE(2,(#126459,#126460,#126461),.UNSPECIFIED.,.F.,.F.)
B_SPLINE_CURVE_WITH_KNOTS((3,3),(0.,0.021164426826543),.UNSPECIFIED.)
CURVE()
GEOMETRIC_REPRESENTATION_ITEM()
RATIONAL_B_SPLINE_CURVE((1.,1.00090979172432,1.00093939181266))
REPRESENTATION_ITEM('')
);
#258=(
BOUNDED_CURVE()
B_SPLINE_CURVE(2,(#126462,#126463,#126464),.UNSPECIFIED.,.F.,.F.)
B_SPLINE_CURVE_WITH_KNOTS((3,3),(0.0225879098005786,0.0437523366271112),
 .UNSPECIFIED.)
CURVE()
GEOMETRIC_REPRESENTATION_ITEM()
RATIONAL_B_SPLINE_CURVE((1.00093939181221,1.00090979172388,1.))
REPRESENTATION_ITEM('')
);
#259=(
BOUNDED_CURVE()
B_SPLINE_CURVE(2,(#126466,#126467,#126468),.UNSPECIFIED.,.F.,.F.)
B_SPLINE_CURVE_WITH_KNOTS((3,3),(0.,0.0211644268266067),.UNSPECIFIED.)
CURVE()
GEOMETRIC_REPRESENTATION_ITEM()
RATIONAL_B_SPLINE_CURVE((1.,1.00090979172414,1.00093939181248))
REPRESENTATION_ITEM('')
);
#260=(
BOUNDED_CURVE()
B_SPLINE_CURVE(2,(#126469,#126470,#126471),.UNSPECIFIED.,.F.,.F.)
B_SPLINE_CURVE_WITH_KNOTS((3,3),(0.0225879098005837,0.0437523366271114),
 .UNSPECIFIED.)
CURVE()
GEOMETRIC_REPRESENTATION_ITEM()
RATIONAL_B_SPLINE_CURVE((1.00093939181515,1.00090979172673,1.))
REPRESENTATION_ITEM('')
);
#261=(
BOUNDED_CURVE()
B_SPLINE_CURVE(2,(#126473,#126474,#126475),.UNSPECIFIED.,.F.,.F.)
B_SPLINE_CURVE_WITH_KNOTS((3,3),(0.,0.021164426826571),.UNSPECIFIED.)
CURVE()
GEOMETRIC_REPRESENTATION_ITEM()
RATIONAL_B_SPLINE_CURVE((1.,1.00090979172479,1.00093939181314))
REPRESENTATION_ITEM('')
);
#262=(
BOUNDED_CURVE()
B_SPLINE_CURVE(2,(#126476,#126477,#126478),.UNSPECIFIED.,.F.,.F.)
B_SPLINE_CURVE_WITH_KNOTS((3,3),(0.0225879098005185,0.0437523366271113),
 .UNSPECIFIED.)
CURVE()
GEOMETRIC_REPRESENTATION_ITEM()
RATIONAL_B_SPLINE_CURVE((1.00093939181435,1.00090979172595,1.))
REPRESENTATION_ITEM('')
);
#263=(
BOUNDED_CURVE()
B_SPLINE_CURVE(2,(#126480,#126481,#126482),.UNSPECIFIED.,.F.,.F.)
B_SPLINE_CURVE_WITH_KNOTS((3,3),(0.,0.0211644268264922),.UNSPECIFIED.)
CURVE()
GEOMETRIC_REPRESENTATION_ITEM()
RATIONAL_B_SPLINE_CURVE((1.,1.00090979172566,1.00093939181405))
REPRESENTATION_ITEM('')
);
#264=(
BOUNDED_CURVE()
B_SPLINE_CURVE(2,(#126483,#126484,#126485),.UNSPECIFIED.,.F.,.F.)
B_SPLINE_CURVE_WITH_KNOTS((3,3),(0.0225879098005469,0.0437523366271113),
 .UNSPECIFIED.)
CURVE()
GEOMETRIC_REPRESENTATION_ITEM()
RATIONAL_B_SPLINE_CURVE((1.00093939181638,1.00090979172792,1.))
REPRESENTATION_ITEM('')
);
#265=(
BOUNDED_CURVE()
B_SPLINE_CURVE(2,(#126487,#126488,#126489),.UNSPECIFIED.,.F.,.F.)
B_SPLINE_CURVE_WITH_KNOTS((3,3),(0.,0.021164426826593),.UNSPECIFIED.)
CURVE()
GEOMETRIC_REPRESENTATION_ITEM()
RATIONAL_B_SPLINE_CURVE((1.,1.00090979171923,1.00093939180741))
REPRESENTATION_ITEM('')
);
#266=(
BOUNDED_CURVE()
B_SPLINE_CURVE(2,(#126490,#126491,#126492),.UNSPECIFIED.,.F.,.F.)
B_SPLINE_CURVE_WITH_KNOTS((3,3),(0.0225879098005747,0.0437523366271113),
 .UNSPECIFIED.)
CURVE()
GEOMETRIC_REPRESENTATION_ITEM()
RATIONAL_B_SPLINE_CURVE((1.00093939181217,1.00090979172384,1.))
REPRESENTATION_ITEM('')
);
#267=(
BOUNDED_CURVE()
B_SPLINE_CURVE(2,(#126494,#126495,#126496),.UNSPECIFIED.,.F.,.F.)
B_SPLINE_CURVE_WITH_KNOTS((3,3),(0.,0.0211644268265413),.UNSPECIFIED.)
CURVE()
GEOMETRIC_REPRESENTATION_ITEM()
RATIONAL_B_SPLINE_CURVE((1.,1.00090979172347,1.00093939181179))
REPRESENTATION_ITEM('')
);
#268=(
BOUNDED_CURVE()
B_SPLINE_CURVE(2,(#126497,#126498,#126499),.UNSPECIFIED.,.F.,.F.)
B_SPLINE_CURVE_WITH_KNOTS((3,3),(0.022587909800513,0.043752336627111),
 .UNSPECIFIED.)
CURVE()
GEOMETRIC_REPRESENTATION_ITEM()
RATIONAL_B_SPLINE_CURVE((1.00093939181455,1.00090979172615,1.))
REPRESENTATION_ITEM('')
);
#269=(
BOUNDED_CURVE()
B_SPLINE_CURVE(2,(#126501,#126502,#126503),.UNSPECIFIED.,.F.,.F.)
B_SPLINE_CURVE_WITH_KNOTS((3,3),(0.,0.0211644268266052),.UNSPECIFIED.)
CURVE()
GEOMETRIC_REPRESENTATION_ITEM()
RATIONAL_B_SPLINE_CURVE((1.,1.00090979172484,1.0009393918132))
REPRESENTATION_ITEM('')
);
#270=(
BOUNDED_CURVE()
B_SPLINE_CURVE(2,(#126504,#126505,#126506),.UNSPECIFIED.,.F.,.F.)
B_SPLINE_CURVE_WITH_KNOTS((3,3),(0.0225879098004969,0.043752336627111),
 .UNSPECIFIED.)
CURVE()
GEOMETRIC_REPRESENTATION_ITEM()
RATIONAL_B_SPLINE_CURVE((1.00093939181429,1.0009097917259,1.))
REPRESENTATION_ITEM('')
);
#271=(
BOUNDED_CURVE()
B_SPLINE_CURVE(2,(#126507,#126508,#126509),.UNSPECIFIED.,.F.,.F.)
B_SPLINE_CURVE_WITH_KNOTS((3,3),(0.,0.0211644268265307),.UNSPECIFIED.)
CURVE()
GEOMETRIC_REPRESENTATION_ITEM()
RATIONAL_B_SPLINE_CURVE((1.,1.00090979172321,1.00093939181152))
REPRESENTATION_ITEM('')
);
#272=(
BOUNDED_CURVE()
B_SPLINE_CURVE(2,(#126759,#126760,#126761),.UNSPECIFIED.,.F.,.F.)
B_SPLINE_CURVE_WITH_KNOTS((3,3),(0.,0.0126130588257612),.UNSPECIFIED.)
CURVE()
GEOMETRIC_REPRESENTATION_ITEM()
RATIONAL_B_SPLINE_CURVE((1.,1.00234596681272,1.00329298027596))
REPRESENTATION_ITEM('')
);
#273=(
BOUNDED_CURVE()
B_SPLINE_CURVE(2,(#126765,#126766,#126767),.UNSPECIFIED.,.F.,.F.)
B_SPLINE_CURVE_WITH_KNOTS((3,3),(0.0296897347922144,0.0423027936179771),
 .UNSPECIFIED.)
CURVE()
GEOMETRIC_REPRESENTATION_ITEM()
RATIONAL_B_SPLINE_CURVE((1.00329298027586,1.00234596681265,1.))
REPRESENTATION_ITEM('')
);
#274=(
BOUNDED_CURVE()
B_SPLINE_CURVE(2,(#126769,#126770,#126771),.UNSPECIFIED.,.F.,.F.)
B_SPLINE_CURVE_WITH_KNOTS((3,3),(0.,0.0126130588257635),.UNSPECIFIED.)
CURVE()
GEOMETRIC_REPRESENTATION_ITEM()
RATIONAL_B_SPLINE_CURVE((1.,1.00234596681256,1.00329298027573))
REPRESENTATION_ITEM('')
);
#275=(
BOUNDED_CURVE()
B_SPLINE_CURVE(2,(#126775,#126776,#126777),.UNSPECIFIED.,.F.,.F.)
B_SPLINE_CURVE_WITH_KNOTS((3,3),(0.0296897347922126,0.0423027936179773),
 .UNSPECIFIED.)
CURVE()
GEOMETRIC_REPRESENTATION_ITEM()
RATIONAL_B_SPLINE_CURVE((1.00329298027557,1.00234596681244,1.))
REPRESENTATION_ITEM('')
);
#276=(
BOUNDED_CURVE()
B_SPLINE_CURVE(2,(#126779,#126780,#126781),.UNSPECIFIED.,.F.,.F.)
B_SPLINE_CURVE_WITH_KNOTS((3,3),(0.,0.0126130588257643),.UNSPECIFIED.)
CURVE()
GEOMETRIC_REPRESENTATION_ITEM()
RATIONAL_B_SPLINE_CURVE((1.,1.00234596681249,1.00329298027564))
REPRESENTATION_ITEM('')
);
#277=(
BOUNDED_CURVE()
B_SPLINE_CURVE(2,(#126785,#126786,#126787),.UNSPECIFIED.,.F.,.F.)
B_SPLINE_CURVE_WITH_KNOTS((3,3),(0.029689734792213,0.0423027936179773),
 .UNSPECIFIED.)
CURVE()
GEOMETRIC_REPRESENTATION_ITEM()
RATIONAL_B_SPLINE_CURVE((1.00329298027556,1.00234596681243,1.))
REPRESENTATION_ITEM('')
);
#278=(
BOUNDED_CURVE()
B_SPLINE_CURVE(2,(#126789,#126790,#126791),.UNSPECIFIED.,.F.,.F.)
B_SPLINE_CURVE_WITH_KNOTS((3,3),(0.,0.0126130588257614),.UNSPECIFIED.)
CURVE()
GEOMETRIC_REPRESENTATION_ITEM()
RATIONAL_B_SPLINE_CURVE((1.,1.00234596681274,1.00329298027599))
REPRESENTATION_ITEM('')
);
#279=(
BOUNDED_CURVE()
B_SPLINE_CURVE(2,(#126795,#126796,#126797),.UNSPECIFIED.,.F.,.F.)
B_SPLINE_CURVE_WITH_KNOTS((3,3),(0.0296897347922119,0.0423027936179772),
 .UNSPECIFIED.)
CURVE()
GEOMETRIC_REPRESENTATION_ITEM()
RATIONAL_B_SPLINE_CURVE((1.00329298027552,1.00234596681241,1.))
REPRESENTATION_ITEM('')
);
#280=(
BOUNDED_CURVE()
B_SPLINE_CURVE(2,(#126799,#126800,#126801),.UNSPECIFIED.,.F.,.F.)
B_SPLINE_CURVE_WITH_KNOTS((3,3),(0.,0.0126130588257625),.UNSPECIFIED.)
CURVE()
GEOMETRIC_REPRESENTATION_ITEM()
RATIONAL_B_SPLINE_CURVE((1.,1.00234596681265,1.00329298027587))
REPRESENTATION_ITEM('')
);
#281=(
BOUNDED_CURVE()
B_SPLINE_CURVE(2,(#126805,#126806,#126807),.UNSPECIFIED.,.F.,.F.)
B_SPLINE_CURVE_WITH_KNOTS((3,3),(0.0296897347922142,0.0423027936179773),
 .UNSPECIFIED.)
CURVE()
GEOMETRIC_REPRESENTATION_ITEM()
RATIONAL_B_SPLINE_CURVE((1.00329298027579,1.0023459668126,1.))
REPRESENTATION_ITEM('')
);
#282=(
BOUNDED_CURVE()
B_SPLINE_CURVE(2,(#126809,#126810,#126811),.UNSPECIFIED.,.F.,.F.)
B_SPLINE_CURVE_WITH_KNOTS((3,3),(0.,0.0126130588257623),.UNSPECIFIED.)
CURVE()
GEOMETRIC_REPRESENTATION_ITEM()
RATIONAL_B_SPLINE_CURVE((1.,1.00234596681269,1.00329298027592))
REPRESENTATION_ITEM('')
);
#283=(
BOUNDED_CURVE()
B_SPLINE_CURVE(2,(#126814,#126815,#126816),.UNSPECIFIED.,.F.,.F.)
B_SPLINE_CURVE_WITH_KNOTS((3,3),(0.0296897347922153,0.042302793617977),
 .UNSPECIFIED.)
CURVE()
GEOMETRIC_REPRESENTATION_ITEM()
RATIONAL_B_SPLINE_CURVE((1.00329298027599,1.00234596681274,1.))
REPRESENTATION_ITEM('')
);
#284=(
BOUNDED_CURVE()
B_SPLINE_CURVE(2,(#135195,#135196,#135197),.UNSPECIFIED.,.F.,.F.)
B_SPLINE_CURVE_WITH_KNOTS((3,3),(0.231010318517618,0.279990879997656),
 .UNSPECIFIED.)
CURVE()
GEOMETRIC_REPRESENTATION_ITEM()
RATIONAL_B_SPLINE_CURVE((1.22678406090041,1.21136642152085,1.17921561612836))
REPRESENTATION_ITEM('')
);
#285=(
BOUNDED_CURVE()
B_SPLINE_CURVE(2,(#135200,#135201,#135202),.UNSPECIFIED.,.F.,.F.)
B_SPLINE_CURVE_WITH_KNOTS((3,3),(0.0917701333748426,0.140750694854882),
 .UNSPECIFIED.)
CURVE()
GEOMETRIC_REPRESENTATION_ITEM()
RATIONAL_B_SPLINE_CURVE((1.17921561612829,1.21136642152077,1.22678406090031))
REPRESENTATION_ITEM('')
);
#286=(
BOUNDED_CURVE()
B_SPLINE_CURVE(2,(#135207,#135208,#135209),.UNSPECIFIED.,.F.,.F.)
B_SPLINE_CURVE_WITH_KNOTS((3,3),(0.231010318517594,0.279990879997634),
 .UNSPECIFIED.)
CURVE()
GEOMETRIC_REPRESENTATION_ITEM()
RATIONAL_B_SPLINE_CURVE((1.22678406090031,1.21136642152077,1.17921561612829))
REPRESENTATION_ITEM('')
);
#287=(
BOUNDED_CURVE()
B_SPLINE_CURVE(2,(#135213,#135214,#135215),.UNSPECIFIED.,.F.,.F.)
B_SPLINE_CURVE_WITH_KNOTS((3,3),(0.0917701333748425,0.140750694854882),
 .UNSPECIFIED.)
CURVE()
GEOMETRIC_REPRESENTATION_ITEM()
RATIONAL_B_SPLINE_CURVE((1.17921561612829,1.21136642152077,1.22678406090031))
REPRESENTATION_ITEM('')
);
#288=ELLIPSE('',#32479,2.77064105207217,1.55);
#289=ELLIPSE('',#32480,5.61755465834429,1.55);
#290=ELLIPSE('',#32481,3.66529504339038,1.55);
#291=ELLIPSE('',#32482,3.66529504339038,1.55);
#292=ELLIPSE('',#32483,5.6175546583443,1.55);
#293=ELLIPSE('',#32484,2.77064105207217,1.55);
#294=ELLIPSE('',#32485,2.77064105207217,1.55);
#295=ELLIPSE('',#32486,5.6175546583443,1.55);
#296=ELLIPSE('',#32487,3.66529504339038,1.55);
#297=ELLIPSE('',#32488,3.66529504339038,1.55);
#298=ELLIPSE('',#32489,5.61755465834429,1.55);
#299=ELLIPSE('',#32490,2.77064105207217,1.55);
#300=ELLIPSE('',#33382,2.40416305603426,1.7);
#301=ELLIPSE('',#33386,2.40416305603426,1.7);
#302=ELLIPSE('',#33391,3.18198051533946,2.25);
#303=ELLIPSE('',#33399,3.18198051533947,2.25);
#304=B_SPLINE_SURFACE_WITH_KNOTS('',3,3,((#48705,#48706,#48707,#48708,#48709,
#48710,#48711,#48712,#48713,#48714,#48715,#48716,#48717,#48718,#48719,#48720,
#48721,#48722,#48723,#48724,#48725,#48726,#48727,#48728,#48729,#48730,#48731,
#48732,#48733,#48734,#48735,#48736,#48737,#48738,#48739),(#48740,#48741,
#48742,#48743,#48744,#48745,#48746,#48747,#48748,#48749,#48750,#48751,#48752,
#48753,#48754,#48755,#48756,#48757,#48758,#48759,#48760,#48761,#48762,#48763,
#48764,#48765,#48766,#48767,#48768,#48769,#48770,#48771,#48772,#48773,#48774),
(#48775,#48776,#48777,#48778,#48779,#48780,#48781,#48782,#48783,#48784,
#48785,#48786,#48787,#48788,#48789,#48790,#48791,#48792,#48793,#48794,#48795,
#48796,#48797,#48798,#48799,#48800,#48801,#48802,#48803,#48804,#48805,#48806,
#48807,#48808,#48809),(#48810,#48811,#48812,#48813,#48814,#48815,#48816,
#48817,#48818,#48819,#48820,#48821,#48822,#48823,#48824,#48825,#48826,#48827,
#48828,#48829,#48830,#48831,#48832,#48833,#48834,#48835,#48836,#48837,#48838,
#48839,#48840,#48841,#48842,#48843,#48844)),.UNSPECIFIED.,.F.,.F.,.F.,(4,
4),(4,1,1,1,1,1,1,1,1,1,1,1,1,1,1,1,1,1,1,1,1,1,1,1,1,1,1,1,1,1,1,1,4),
(0.,0.0601216701678314),(0.958497295273323,0.960061197080218,0.961540412003173,
0.964498841849082,0.967457271694992,0.970415701540902,0.970600603406271,
0.970785505271641,0.971155309002379,0.971894916463857,0.973374131386812,
0.974113738848289,0.974853346309767,0.976332561232722,0.977811776155676,
0.979290991078631,0.980770206001586,0.982249420924541,0.984221707488481,
0.986193994052421,0.988166280616361,0.989152423898331,0.989645495539316,
0.989892031359808,0.990015299270054,0.990076933225178,0.990138567180301,
0.99211085374424,0.99408314030818,0.995562355231135,0.99704157015409,0.998520785077045,
1.00008475653519),.UNSPECIFIED.);
#305=B_SPLINE_SURFACE_WITH_KNOTS('',3,3,((#49300,#49301,#49302,#49303,#49304,
#49305,#49306,#49307,#49308,#49309,#49310,#49311,#49312,#49313,#49314,#49315,
#49316,#49317,#49318,#49319,#49320,#49321,#49322,#49323,#49324,#49325,#49326,
#49327,#49328,#49329,#49330,#49331,#49332,#49333,#49334,#49335,#49336),
(#49337,#49338,#49339,#49340,#49341,#49342,#49343,#49344,#49345,#49346,
#49347,#49348,#49349,#49350,#49351,#49352,#49353,#49354,#49355,#49356,#49357,
#49358,#49359,#49360,#49361,#49362,#49363,#49364,#49365,#49366,#49367,#49368,
#49369,#49370,#49371,#49372,#49373),(#49374,#49375,#49376,#49377,#49378,
#49379,#49380,#49381,#49382,#49383,#49384,#49385,#49386,#49387,#49388,#49389,
#49390,#49391,#49392,#49393,#49394,#49395,#49396,#49397,#49398,#49399,#49400,
#49401,#49402,#49403,#49404,#49405,#49406,#49407,#49408,#49409,#49410),
(#49411,#49412,#49413,#49414,#49415,#49416,#49417,#49418,#49419,#49420,
#49421,#49422,#49423,#49424,#49425,#49426,#49427,#49428,#49429,#49430,#49431,
#49432,#49433,#49434,#49435,#49436,#49437,#49438,#49439,#49440,#49441,#49442,
#49443,#49444,#49445,#49446,#49447)),.UNSPECIFIED.,.F.,.F.,.F.,(4,4),(4,
1,1,1,1,1,1,1,1,1,1,1,1,1,1,1,1,1,1,1,1,1,1,1,1,1,1,1,1,1,1,1,1,1,4),(-0.0004131206956421,
0.0600746011189307),(-0.000245952479762335,0.0018432399144214,0.00368647982884281,
0.00552971974326421,0.00737295965768562,0.00983061287691415,0.0122882660961427,
0.013517092705757,0.0141315060105641,0.0144387126629677,0.0147459193153712,
0.0172035725345998,0.0196612257538283,0.0221188789730568,0.0245765321922854,
0.0258053588018997,0.0270341854115139,0.0294918386307425,0.0307206652403567,
0.031949491849971,0.0344071450691995,0.0352263628089424,0.0368647982884281,
0.0393224515076566,0.0399368648124638,0.0405512781172709,0.0417801047268852,
0.0430089313364994,0.0436233446413066,0.0439305512937101,0.0442377579461137,
0.0460809978605351,0.0479242377749565,0.0497674776893779,0.0518564147280488),
 .UNSPECIFIED.);
#306=B_SPLINE_SURFACE_WITH_KNOTS('',3,3,((#49706,#49707,#49708,#49709,#49710,
#49711,#49712,#49713,#49714,#49715,#49716,#49717,#49718,#49719,#49720,#49721,
#49722,#49723,#49724,#49725,#49726,#49727,#49728,#49729,#49730,#49731,#49732,
#49733,#49734,#49735,#49736,#49737,#49738,#49739,#49740,#49741,#49742,#49743,
#49744,#49745,#49746,#49747,#49748,#49749,#49750,#49751,#49752,#49753,#49754,
#49755,#49756,#49757,#49758,#49759,#49760,#49761,#49762,#49763,#49764,#49765,
#49766,#49767),(#49768,#49769,#49770,#49771,#49772,#49773,#49774,#49775,
#49776,#49777,#49778,#49779,#49780,#49781,#49782,#49783,#49784,#49785,#49786,
#49787,#49788,#49789,#49790,#49791,#49792,#49793,#49794,#49795,#49796,#49797,
#49798,#49799,#49800,#49801,#49802,#49803,#49804,#49805,#49806,#49807,#49808,
#49809,#49810,#49811,#49812,#49813,#49814,#49815,#49816,#49817,#49818,#49819,
#49820,#49821,#49822,#49823,#49824,#49825,#49826,#49827,#49828,#49829),
(#49830,#49831,#49832,#49833,#49834,#49835,#49836,#49837,#49838,#49839,
#49840,#49841,#49842,#49843,#49844,#49845,#49846,#49847,#49848,#49849,#49850,
#49851,#49852,#49853,#49854,#49855,#49856,#49857,#49858,#49859,#49860,#49861,
#49862,#49863,#49864,#49865,#49866,#49867,#49868,#49869,#49870,#49871,#49872,
#49873,#49874,#49875,#49876,#49877,#49878,#49879,#49880,#49881,#49882,#49883,
#49884,#49885,#49886,#49887,#49888,#49889,#49890,#49891),(#49892,#49893,
#49894,#49895,#49896,#49897,#49898,#49899,#49900,#49901,#49902,#49903,#49904,
#49905,#49906,#49907,#49908,#49909,#49910,#49911,#49912,#49913,#49914,#49915,
#49916,#49917,#49918,#49919,#49920,#49921,#49922,#49923,#49924,#49925,#49926,
#49927,#49928,#49929,#49930,#49931,#49932,#49933,#49934,#49935,#49936,#49937,
#49938,#49939,#49940,#49941,#49942,#49943,#49944,#49945,#49946,#49947,#49948,
#49949,#49950,#49951,#49952,#49953)),.UNSPECIFIED.,.F.,.F.,.F.,(4,4),(4,
1,1,1,1,1,1,1,1,1,1,1,1,1,1,1,1,1,1,1,1,1,1,1,1,1,1,1,1,1,1,1,1,1,1,1,1,
1,1,1,1,1,1,1,1,1,1,1,1,1,1,1,1,1,1,1,1,1,1,4),(-0.000719064234915953,0.0600510031832868),
(0.116699315494241,0.118587303856748,0.120430777434874,0.122274251012999,
0.124117724591124,0.125961198169249,0.127804671747374,0.1296481453255,0.131491618903625,
0.133949583674458,0.134564074867167,0.135178566059875,0.136407548445292,
0.138865513216126,0.141323477986959,0.143781442757793,0.146239407528626,
0.148082881106752,0.149926354684877,0.151769828263002,0.153613301841127,
0.155456775419252,0.157300248997378,0.159143722575503,0.160987196153628,
0.162830669731753,0.164674143309878,0.166517616888004,0.168361090466129,
0.170204564044254,0.172048037622379,0.173891511200504,0.17573498477863,
0.178192949549463,0.180650914320297,0.18310887909113,0.185566843861964,
0.186795826247381,0.188024808632798,0.190482773403631,0.191711755789048,
0.192940738174465,0.193247983770819,0.193555229367173,0.194169720559882,
0.19478421175259,0.195398702945298,0.197856667716132,0.200314632486966,
0.201953275667521,0.205230562028633,0.205691430423164,0.207074035606758,
0.208917509184883,0.210760982763008,0.212604456341134,0.214447929919259,
0.216291403497384,0.218134877075509,0.220431769292195),.UNSPECIFIED.);
#307=B_SPLINE_SURFACE_WITH_KNOTS('',3,3,((#50568,#50569,#50570,#50571,#50572,
#50573,#50574,#50575,#50576,#50577,#50578,#50579,#50580,#50581,#50582,#50583,
#50584,#50585,#50586,#50587,#50588,#50589,#50590,#50591,#50592,#50593,#50594,
#50595,#50596,#50597,#50598,#50599,#50600,#50601,#50602,#50603,#50604,#50605,
#50606,#50607,#50608,#50609,#50610,#50611,#50612,#50613,#50614,#50615,#50616,
#50617,#50618,#50619,#50620,#50621,#50622,#50623,#50624,#50625,#50626,#50627,
#50628,#50629,#50630,#50631,#50632,#50633,#50634,#50635,#50636),(#50637,
#50638,#50639,#50640,#50641,#50642,#50643,#50644,#50645,#50646,#50647,#50648,
#50649,#50650,#50651,#50652,#50653,#50654,#50655,#50656,#50657,#50658,#50659,
#50660,#50661,#50662,#50663,#50664,#50665,#50666,#50667,#50668,#50669,#50670,
#50671,#50672,#50673,#50674,#50675,#50676,#50677,#50678,#50679,#50680,#50681,
#50682,#50683,#50684,#50685,#50686,#50687,#50688,#50689,#50690,#50691,#50692,
#50693,#50694,#50695,#50696,#50697,#50698,#50699,#50700,#50701,#50702,#50703,
#50704,#50705),(#50706,#50707,#50708,#50709,#50710,#50711,#50712,#50713,
#50714,#50715,#50716,#50717,#50718,#50719,#50720,#50721,#50722,#50723,#50724,
#50725,#50726,#50727,#50728,#50729,#50730,#50731,#50732,#50733,#50734,#50735,
#50736,#50737,#50738,#50739,#50740,#50741,#50742,#50743,#50744,#50745,#50746,
#50747,#50748,#50749,#50750,#50751,#50752,#50753,#50754,#50755,#50756,#50757,
#50758,#50759,#50760,#50761,#50762,#50763,#50764,#50765,#50766,#50767,#50768,
#50769,#50770,#50771,#50772,#50773,#50774),(#50775,#50776,#50777,#50778,
#50779,#50780,#50781,#50782,#50783,#50784,#50785,#50786,#50787,#50788,#50789,
#50790,#50791,#50792,#50793,#50794,#50795,#50796,#50797,#50798,#50799,#50800,
#50801,#50802,#50803,#50804,#50805,#50806,#50807,#50808,#50809,#50810,#50811,
#50812,#50813,#50814,#50815,#50816,#50817,#50818,#50819,#50820,#50821,#50822,
#50823,#50824,#50825,#50826,#50827,#50828,#50829,#50830,#50831,#50832,#50833,
#50834,#50835,#50836,#50837,#50838,#50839,#50840,#50841,#50842,#50843)),
 .UNSPECIFIED.,.F.,.F.,.F.,(4,4),(4,1,1,1,1,1,1,1,1,1,1,1,1,1,1,1,1,1,1,
1,1,1,1,1,1,1,1,1,1,1,1,1,1,1,1,1,1,1,1,1,1,1,1,1,1,1,1,1,1,1,1,1,1,1,1,
1,1,1,1,1,1,1,1,1,1,1,4),(-0.000304659761922948,0.0600640983517747),(0.285071931319951,
0.286954925748233,0.288798399656758,0.290641873565284,0.292485347473809,
0.294328821382334,0.296172295290859,0.298015769199385,0.29985924310791,
0.302317208319277,0.304775173530644,0.307233138742011,0.309076612650536,
0.310920086559061,0.312763560467587,0.314607034376112,0.316450508284637,
0.318293982193163,0.319215719147425,0.320137456101688,0.320828758817385,
0.32105919305595,0.321520061533082,0.321750495771647,0.321980930010213,
0.32428527239587,0.325667877827264,0.328433088690051,0.329354825644314,
0.331198299552839,0.333041773461365,0.33488524736989,0.336728721278415,
0.337189589755546,0.337650458232678,0.33857219518694,0.339493932141203,
0.340415669095466,0.342259143003991,0.344102616912516,0.345946090821041,
0.347789564729567,0.349633038638092,0.351476512546617,0.352091003849459,
0.35239824950088,0.352705495152301,0.353934477757984,0.356392442969351,
0.357621425575035,0.358235916877876,0.358850408180718,0.361308373392085,
0.363766338603452,0.366224303814819,0.368682269026186,0.370320912500431,
0.371959555974676,0.37359819944892,0.375441673357445,0.377285147265971,
0.379128621174496,0.380972095083021,0.382815568991547,0.384659042900072,
0.386502516808597,0.388345990717122),.UNSPECIFIED.);
#308=B_SPLINE_SURFACE_WITH_KNOTS('',3,3,((#52114,#52115,#52116,#52117,#52118,
#52119,#52120,#52121,#52122,#52123,#52124,#52125,#52126,#52127,#52128,#52129,
#52130,#52131,#52132,#52133,#52134,#52135,#52136,#52137,#52138,#52139,#52140,
#52141,#52142,#52143,#52144,#52145,#52146,#52147,#52148,#52149,#52150,#52151,
#52152,#52153,#52154,#52155,#52156,#52157,#52158,#52159,#52160,#52161,#52162,
#52163,#52164,#52165,#52166,#52167,#52168,#52169,#52170,#52171,#52172,#52173,
#52174,#52175,#52176),(#52177,#52178,#52179,#52180,#52181,#52182,#52183,
#52184,#52185,#52186,#52187,#52188,#52189,#52190,#52191,#52192,#52193,#52194,
#52195,#52196,#52197,#52198,#52199,#52200,#52201,#52202,#52203,#52204,#52205,
#52206,#52207,#52208,#52209,#52210,#52211,#52212,#52213,#52214,#52215,#52216,
#52217,#52218,#52219,#52220,#52221,#52222,#52223,#52224,#52225,#52226,#52227,
#52228,#52229,#52230,#52231,#52232,#52233,#52234,#52235,#52236,#52237,#52238,
#52239),(#52240,#52241,#52242,#52243,#52244,#52245,#52246,#52247,#52248,
#52249,#52250,#52251,#52252,#52253,#52254,#52255,#52256,#52257,#52258,#52259,
#52260,#52261,#52262,#52263,#52264,#52265,#52266,#52267,#52268,#52269,#52270,
#52271,#52272,#52273,#52274,#52275,#52276,#52277,#52278,#52279,#52280,#52281,
#52282,#52283,#52284,#52285,#52286,#52287,#52288,#52289,#52290,#52291,#52292,
#52293,#52294,#52295,#52296,#52297,#52298,#52299,#52300,#52301,#52302),
(#52303,#52304,#52305,#52306,#52307,#52308,#52309,#52310,#52311,#52312,
#52313,#52314,#52315,#52316,#52317,#52318,#52319,#52320,#52321,#52322,#52323,
#52324,#52325,#52326,#52327,#52328,#52329,#52330,#52331,#52332,#52333,#52334,
#52335,#52336,#52337,#52338,#52339,#52340,#52341,#52342,#52343,#52344,#52345,
#52346,#52347,#52348,#52349,#52350,#52351,#52352,#52353,#52354,#52355,#52356,
#52357,#52358,#52359,#52360,#52361,#52362,#52363,#52364,#52365)),
 .UNSPECIFIED.,.F.,.F.,.F.,(4,4),(4,1,1,1,1,1,1,1,1,1,1,1,1,1,1,1,1,1,1,
1,1,1,1,1,1,1,1,1,1,1,1,1,1,1,1,1,1,1,1,1,1,1,1,1,1,1,1,1,1,1,1,1,1,1,1,
1,1,1,1,1,4),(-0.000669329015107292,0.0600896068960631),(0.453390084310778,
0.45532256751791,0.457166041104501,0.459009514691093,0.460852988277684,
0.462696461864275,0.464539935450866,0.466383409037458,0.468226882624049,
0.470684847406171,0.473142812188293,0.475600776970414,0.478058741752536,
0.480516706534658,0.48297467131678,0.484818144903371,0.486661618489962,
0.488505092076554,0.490348565663145,0.492192039249736,0.494035512836328,
0.495878986422919,0.49772246000951,0.498183328406158,0.498644196802806,
0.499565933596102,0.501409407182693,0.503252880769284,0.505096354355876,
0.506939827942467,0.507400696339115,0.508783301529058,0.510626775115649,
0.512470248702241,0.514928213484362,0.517386178266484,0.519844143048606,
0.522302107830728,0.52476007261285,0.527218037394971,0.529676002177093,
0.530290493372624,0.530904984568154,0.531519475763684,0.532133966959215,
0.534591931741337,0.535820914132398,0.537049896523458,0.53868853971154,
0.540327182899621,0.541965826087702,0.542887562880998,0.543809299674293,
0.544731036467589,0.545652773260885,0.547496246847476,0.549339720434067,
0.551183194020659,0.55302666760725,0.554870141193841,0.55716859910234),
 .UNSPECIFIED.);
#309=B_SPLINE_SURFACE_WITH_KNOTS('',3,3,((#53368,#53369,#53370,#53371,#53372,
#53373,#53374,#53375,#53376,#53377,#53378,#53379,#53380,#53381,#53382,#53383,
#53384,#53385,#53386,#53387,#53388,#53389,#53390,#53391,#53392,#53393,#53394,
#53395,#53396,#53397,#53398,#53399,#53400,#53401,#53402,#53403,#53404,#53405,
#53406,#53407,#53408,#53409,#53410,#53411,#53412,#53413,#53414,#53415,#53416,
#53417,#53418,#53419,#53420,#53421,#53422,#53423,#53424),(#53425,#53426,
#53427,#53428,#53429,#53430,#53431,#53432,#53433,#53434,#53435,#53436,#53437,
#53438,#53439,#53440,#53441,#53442,#53443,#53444,#53445,#53446,#53447,#53448,
#53449,#53450,#53451,#53452,#53453,#53454,#53455,#53456,#53457,#53458,#53459,
#53460,#53461,#53462,#53463,#53464,#53465,#53466,#53467,#53468,#53469,#53470,
#53471,#53472,#53473,#53474,#53475,#53476,#53477,#53478,#53479,#53480,#53481),
(#53482,#53483,#53484,#53485,#53486,#53487,#53488,#53489,#53490,#53491,
#53492,#53493,#53494,#53495,#53496,#53497,#53498,#53499,#53500,#53501,#53502,
#53503,#53504,#53505,#53506,#53507,#53508,#53509,#53510,#53511,#53512,#53513,
#53514,#53515,#53516,#53517,#53518,#53519,#53520,#53521,#53522,#53523,#53524,
#53525,#53526,#53527,#53528,#53529,#53530,#53531,#53532,#53533,#53534,#53535,
#53536,#53537,#53538),(#53539,#53540,#53541,#53542,#53543,#53544,#53545,
#53546,#53547,#53548,#53549,#53550,#53551,#53552,#53553,#53554,#53555,#53556,
#53557,#53558,#53559,#53560,#53561,#53562,#53563,#53564,#53565,#53566,#53567,
#53568,#53569,#53570,#53571,#53572,#53573,#53574,#53575,#53576,#53577,#53578,
#53579,#53580,#53581,#53582,#53583,#53584,#53585,#53586,#53587,#53588,#53589,
#53590,#53591,#53592,#53593,#53594,#53595)),.UNSPECIFIED.,.F.,.F.,.F.,(4,
4),(4,1,1,1,1,1,1,1,1,1,1,1,1,1,1,1,1,1,1,1,1,1,1,1,1,1,1,1,1,1,1,1,1,1,
1,1,1,1,1,1,1,1,1,1,1,1,1,1,1,1,1,1,1,1,4),(-0.000398179937811476,0.0600544212357538),
(0.621792488306161,0.623690199736931,0.625533673395834,0.627377147054738,
0.629220620713642,0.631064094372546,0.63290756803145,0.634751041690353,
0.636594515349257,0.639052480227795,0.641510445106334,0.643968409984872,
0.646426374863411,0.648884339741949,0.651342304620487,0.653185778279391,
0.655029251938295,0.657333594011925,0.658716199256103,0.660559672915006,
0.66240314657391,0.663324883403362,0.666090093891718,0.667933567550621,
0.669777041209525,0.671620514868429,0.673463988527333,0.674846593771511,
0.675307462186237,0.677150935845141,0.678994409504044,0.680837883162948,
0.683295848041487,0.685753812920025,0.688211777798563,0.690669742677102,
0.69312770755564,0.695585672434178,0.698043637312717,0.700501602191255,
0.701730584630524,0.702959567069794,0.703574058289428,0.705417531948332,
0.707056175200691,0.710333461705409,0.711716066949587,0.712176935364313,
0.714020409023216,0.71586388268212,0.717707356341024,0.719550829999928,
0.721394303658832,0.723237777317735,0.725081250976639),.UNSPECIFIED.);
#310=B_SPLINE_SURFACE_WITH_KNOTS('',3,3,((#55419,#55420,#55421,#55422,#55423,
#55424,#55425,#55426,#55427,#55428,#55429,#55430,#55431,#55432,#55433,#55434,
#55435,#55436,#55437,#55438,#55439,#55440,#55441,#55442,#55443,#55444,#55445,
#55446,#55447,#55448,#55449,#55450,#55451,#55452,#55453,#55454,#55455,#55456,
#55457,#55458,#55459,#55460,#55461,#55462,#55463,#55464,#55465,#55466,#55467,
#55468,#55469,#55470,#55471,#55472,#55473,#55474,#55475,#55476),(#55477,
#55478,#55479,#55480,#55481,#55482,#55483,#55484,#55485,#55486,#55487,#55488,
#55489,#55490,#55491,#55492,#55493,#55494,#55495,#55496,#55497,#55498,#55499,
#55500,#55501,#55502,#55503,#55504,#55505,#55506,#55507,#55508,#55509,#55510,
#55511,#55512,#55513,#55514,#55515,#55516,#55517,#55518,#55519,#55520,#55521,
#55522,#55523,#55524,#55525,#55526,#55527,#55528,#55529,#55530,#55531,#55532,
#55533,#55534),(#55535,#55536,#55537,#55538,#55539,#55540,#55541,#55542,
#55543,#55544,#55545,#55546,#55547,#55548,#55549,#55550,#55551,#55552,#55553,
#55554,#55555,#55556,#55557,#55558,#55559,#55560,#55561,#55562,#55563,#55564,
#55565,#55566,#55567,#55568,#55569,#55570,#55571,#55572,#55573,#55574,#55575,
#55576,#55577,#55578,#55579,#55580,#55581,#55582,#55583,#55584,#55585,#55586,
#55587,#55588,#55589,#55590,#55591,#55592),(#55593,#55594,#55595,#55596,
#55597,#55598,#55599,#55600,#55601,#55602,#55603,#55604,#55605,#55606,#55607,
#55608,#55609,#55610,#55611,#55612,#55613,#55614,#55615,#55616,#55617,#55618,
#55619,#55620,#55621,#55622,#55623,#55624,#55625,#55626,#55627,#55628,#55629,
#55630,#55631,#55632,#55633,#55634,#55635,#55636,#55637,#55638,#55639,#55640,
#55641,#55642,#55643,#55644,#55645,#55646,#55647,#55648,#55649,#55650)),
 .UNSPECIFIED.,.F.,.F.,.F.,(4,4),(4,1,1,1,1,1,1,1,1,1,1,1,1,1,1,1,1,1,1,
1,1,1,1,1,1,1,1,1,1,1,1,1,1,1,1,1,1,1,1,1,1,1,1,1,1,1,1,1,1,1,1,1,1,1,1,
4),(-4.02403031655857E-6,0.09969297120439),(0.91568008989925,0.918757739489292,
0.9217667121008,0.924775684712307,0.927784657323815,0.92979063906482,0.931796620805825,
0.93380260254683,0.935307088852584,0.936811575158338,0.939820547769846,
0.940071295487471,0.940322043205097,0.940823538640348,0.940948912499161,
0.941074286357974,0.9413250340756,0.941575781793225,0.941701155652038,0.941826529510851,
0.942495190091186,0.943832511251856,0.944166841542024,0.944501171832191,
0.945169832412526,0.945838492992861,0.946507153573196,0.947844474733866,
0.949850456474872,0.951856438215877,0.953862419956882,0.955868401697887,
0.957874383438892,0.959880365179897,0.9608833560504,0.961886346920902,0.962889337791405,
0.963892328661908,0.966901301273415,0.969910273884923,0.972919246496431,
0.975928219107938,0.977432705413692,0.978937191719446,0.9804416780252,0.981946164330954,
0.983450650636708,0.984955136942461,0.986459623248215,0.987964109553969,
0.989468595859723,0.990973082165477,0.993982054776985,0.996991027388492,
0.998495513694246,1.00000605975256),.UNSPECIFIED.);
#311=B_SPLINE_SURFACE_WITH_KNOTS('',3,3,((#56234,#56235,#56236,#56237,#56238,
#56239,#56240,#56241,#56242,#56243,#56244,#56245,#56246,#56247,#56248,#56249,
#56250,#56251,#56252,#56253,#56254,#56255,#56256,#56257,#56258,#56259),
(#56260,#56261,#56262,#56263,#56264,#56265,#56266,#56267,#56268,#56269,
#56270,#56271,#56272,#56273,#56274,#56275,#56276,#56277,#56278,#56279,#56280,
#56281,#56282,#56283,#56284,#56285),(#56286,#56287,#56288,#56289,#56290,
#56291,#56292,#56293,#56294,#56295,#56296,#56297,#56298,#56299,#56300,#56301,
#56302,#56303,#56304,#56305,#56306,#56307,#56308,#56309,#56310,#56311),
(#56312,#56313,#56314,#56315,#56316,#56317,#56318,#56319,#56320,#56321,
#56322,#56323,#56324,#56325,#56326,#56327,#56328,#56329,#56330,#56331,#56332,
#56333,#56334,#56335,#56336,#56337)),.UNSPECIFIED.,.F.,.F.,.F.,(4,4),(4,
1,1,1,1,1,1,1,1,1,1,1,1,1,1,1,1,1,1,1,1,1,1,4),(-0.000160794326669428,0.0629206068794883),
(-0.000160794326669428,0.00204857271922254,0.00409714543844508,0.00614571815766761,
0.00819429087689015,0.00827964807352442,0.0083650052701587,0.00853571966342724,
0.00887714844996433,0.00956000602303851,0.0109257211691869,0.0122914363153352,
0.0136571514614836,0.0150228666076319,0.0163885817537803,0.0174128681133916,
0.0184371544730028,0.0194614408326141,0.0199735840124197,0.0204857271922254,
0.0225342999114479,0.0245828726306705,0.026631445349893,0.0288407216756201),
 .UNSPECIFIED.);
#312=B_SPLINE_SURFACE_WITH_KNOTS('',3,3,((#56339,#56340,#56341,#56342,#56343,
#56344,#56345,#56346,#56347,#56348,#56349,#56350,#56351,#56352,#56353,#56354,
#56355,#56356,#56357,#56358,#56359,#56360,#56361,#56362,#56363,#56364,#56365,
#56366,#56367,#56368,#56369,#56370,#56371,#56372,#56373,#56374,#56375,#56376,
#56377,#56378,#56379,#56380,#56381,#56382,#56383,#56384,#56385,#56386,#56387,
#56388,#56389,#56390,#56391,#56392,#56393,#56394,#56395,#56396,#56397,#56398,
#56399,#56400,#56401,#56402),(#56403,#56404,#56405,#56406,#56407,#56408,
#56409,#56410,#56411,#56412,#56413,#56414,#56415,#56416,#56417,#56418,#56419,
#56420,#56421,#56422,#56423,#56424,#56425,#56426,#56427,#56428,#56429,#56430,
#56431,#56432,#56433,#56434,#56435,#56436,#56437,#56438,#56439,#56440,#56441,
#56442,#56443,#56444,#56445,#56446,#56447,#56448,#56449,#56450,#56451,#56452,
#56453,#56454,#56455,#56456,#56457,#56458,#56459,#56460,#56461,#56462,#56463,
#56464,#56465,#56466),(#56467,#56468,#56469,#56470,#56471,#56472,#56473,
#56474,#56475,#56476,#56477,#56478,#56479,#56480,#56481,#56482,#56483,#56484,
#56485,#56486,#56487,#56488,#56489,#56490,#56491,#56492,#56493,#56494,#56495,
#56496,#56497,#56498,#56499,#56500,#56501,#56502,#56503,#56504,#56505,#56506,
#56507,#56508,#56509,#56510,#56511,#56512,#56513,#56514,#56515,#56516,#56517,
#56518,#56519,#56520,#56521,#56522,#56523,#56524,#56525,#56526,#56527,#56528,
#56529,#56530),(#56531,#56532,#56533,#56534,#56535,#56536,#56537,#56538,
#56539,#56540,#56541,#56542,#56543,#56544,#56545,#56546,#56547,#56548,#56549,
#56550,#56551,#56552,#56553,#56554,#56555,#56556,#56557,#56558,#56559,#56560,
#56561,#56562,#56563,#56564,#56565,#56566,#56567,#56568,#56569,#56570,#56571,
#56572,#56573,#56574,#56575,#56576,#56577,#56578,#56579,#56580,#56581,#56582,
#56583,#56584,#56585,#56586,#56587,#56588,#56589,#56590,#56591,#56592,#56593,
#56594)),.UNSPECIFIED.,.F.,.F.,.F.,(4,4),(4,1,1,1,1,1,1,1,1,1,1,1,1,1,1,
1,1,1,1,1,1,1,1,1,1,1,1,1,1,1,1,1,1,1,1,1,1,1,1,1,1,1,1,1,1,1,1,1,1,1,1,
1,1,1,1,1,1,1,1,1,1,4),(-9.26332648532586E-5,0.0996768470183328),(0.0738580961833418,
0.076109515853017,0.0783083908329088,0.0805072658128007,0.0827061407926925,
0.0849050157725843,0.0871038907524762,0.089302765732368,0.0915016407122598,
0.0944334740187823,0.0958993906720435,0.0973653073253047,0.100297140631827,
0.10322897393835,0.106160807244872,0.109092640551394,0.111291515531286,
0.113490390511178,0.11568926549107,0.117888140470962,0.120087015450854,
0.122285890430745,0.124484765410637,0.126683640390529,0.128882515370421,
0.131081390350313,0.133280265330205,0.135479140310096,0.137678015289988,
0.13987689026988,0.142075765249772,0.144274640229664,0.145740556882925,
0.147206473536186,0.147939431862817,0.150138306842709,0.153070140149231,
0.156001973455754,0.158933806762276,0.161865640068798,0.162598598395429,
0.16333155672206,0.16406451504869,0.164797473375321,0.167729306681843,0.170661139988366,
0.172127056641627,0.172860014968258,0.173592973294888,0.17554752883257,
0.17603616771699,0.176524806601411,0.177502084370251,0.179456639907933,
0.181655514887825,0.183854389867717,0.186053264847609,0.1882521398275,0.190451014807392,
0.192649889787284,0.194848764767176,0.197140249031834),.UNSPECIFIED.);
#313=B_SPLINE_SURFACE_WITH_KNOTS('',3,3,((#57145,#57146,#57147,#57148,#57149,
#57150,#57151,#57152,#57153,#57154,#57155,#57156,#57157,#57158,#57159,#57160,
#57161,#57162,#57163,#57164,#57165,#57166,#57167,#57168,#57169,#57170,#57171,
#57172,#57173,#57174,#57175,#57176,#57177,#57178,#57179,#57180,#57181,#57182,
#57183,#57184,#57185,#57186,#57187,#57188,#57189,#57190,#57191,#57192,#57193,
#57194,#57195,#57196,#57197,#57198,#57199,#57200,#57201,#57202,#57203,#57204,
#57205,#57206,#57207,#57208,#57209,#57210,#57211,#57212,#57213),(#57214,
#57215,#57216,#57217,#57218,#57219,#57220,#57221,#57222,#57223,#57224,#57225,
#57226,#57227,#57228,#57229,#57230,#57231,#57232,#57233,#57234,#57235,#57236,
#57237,#57238,#57239,#57240,#57241,#57242,#57243,#57244,#57245,#57246,#57247,
#57248,#57249,#57250,#57251,#57252,#57253,#57254,#57255,#57256,#57257,#57258,
#57259,#57260,#57261,#57262,#57263,#57264,#57265,#57266,#57267,#57268,#57269,
#57270,#57271,#57272,#57273,#57274,#57275,#57276,#57277,#57278,#57279,#57280,
#57281,#57282),(#57283,#57284,#57285,#57286,#57287,#57288,#57289,#57290,
#57291,#57292,#57293,#57294,#57295,#57296,#57297,#57298,#57299,#57300,#57301,
#57302,#57303,#57304,#57305,#57306,#57307,#57308,#57309,#57310,#57311,#57312,
#57313,#57314,#57315,#57316,#57317,#57318,#57319,#57320,#57321,#57322,#57323,
#57324,#57325,#57326,#57327,#57328,#57329,#57330,#57331,#57332,#57333,#57334,
#57335,#57336,#57337,#57338,#57339,#57340,#57341,#57342,#57343,#57344,#57345,
#57346,#57347,#57348,#57349,#57350,#57351),(#57352,#57353,#57354,#57355,
#57356,#57357,#57358,#57359,#57360,#57361,#57362,#57363,#57364,#57365,#57366,
#57367,#57368,#57369,#57370,#57371,#57372,#57373,#57374,#57375,#57376,#57377,
#57378,#57379,#57380,#57381,#57382,#57383,#57384,#57385,#57386,#57387,#57388,
#57389,#57390,#57391,#57392,#57393,#57394,#57395,#57396,#57397,#57398,#57399,
#57400,#57401,#57402,#57403,#57404,#57405,#57406,#57407,#57408,#57409,#57410,
#57411,#57412,#57413,#57414,#57415,#57416,#57417,#57418,#57419,#57420)),
 .UNSPECIFIED.,.F.,.F.,.F.,(4,4),(4,1,1,1,1,1,1,1,1,1,1,1,1,1,1,1,1,1,1,
1,1,1,1,1,1,1,1,1,1,1,1,1,1,1,1,1,1,1,1,1,1,1,1,1,1,1,1,1,1,1,1,1,1,1,1,
1,1,1,1,1,1,1,1,1,1,1,4),(0.,0.0996711058249781),(0.242231595226055,0.244477134072873,
0.246676009090878,0.248874884108883,0.251073759126888,0.253272634144893,
0.255471509162898,0.257670384180903,0.259869259198908,0.262801092556248,
0.264267009234918,0.264999967574253,0.265732925913588,0.267198842592258,
0.268664759270928,0.270130675949598,0.271596592628268,0.274528425985608,
0.277460259342948,0.279659134360953,0.281858009378958,0.284056884396963,
0.286255759414968,0.288454634432973,0.290653509450978,0.29175294695998,
0.292852384468983,0.293951821977985,0.295051259486988,0.297250134504992,
0.299449009522997,0.301647884541002,0.303846759559007,0.306045634577012,
0.308244509595017,0.310443384613022,0.312642259631027,0.315574092988367,
0.318505926345707,0.321437759703047,0.324369593060387,0.327301426417727,
0.330233259775067,0.331699176453737,0.332432134793072,0.33279861396274,
0.333165093132407,0.336096926489747,0.337562843168417,0.339028759847087,
0.341960593204427,0.343915148775987,0.345869704347547,0.347824259919107,
0.348373978673608,0.348648838050859,0.348923697428109,0.349473416182611,
0.350023134937112,0.351122572446114,0.352222009955117,0.354420884973122,
0.356619759991127,0.358818635009132,0.361017510027137,0.363216385045142,
0.365415260063147),.UNSPECIFIED.);
#314=B_SPLINE_SURFACE_WITH_KNOTS('',3,3,((#57977,#57978,#57979,#57980,#57981,
#57982,#57983,#57984,#57985,#57986,#57987,#57988,#57989,#57990,#57991,#57992,
#57993,#57994,#57995,#57996,#57997,#57998,#57999,#58000,#58001,#58002,#58003,
#58004,#58005,#58006,#58007,#58008,#58009,#58010,#58011,#58012,#58013,#58014,
#58015,#58016,#58017,#58018,#58019,#58020,#58021,#58022,#58023,#58024,#58025,
#58026,#58027,#58028,#58029,#58030,#58031,#58032,#58033,#58034,#58035,#58036,
#58037,#58038,#58039,#58040),(#58041,#58042,#58043,#58044,#58045,#58046,
#58047,#58048,#58049,#58050,#58051,#58052,#58053,#58054,#58055,#58056,#58057,
#58058,#58059,#58060,#58061,#58062,#58063,#58064,#58065,#58066,#58067,#58068,
#58069,#58070,#58071,#58072,#58073,#58074,#58075,#58076,#58077,#58078,#58079,
#58080,#58081,#58082,#58083,#58084,#58085,#58086,#58087,#58088,#58089,#58090,
#58091,#58092,#58093,#58094,#58095,#58096,#58097,#58098,#58099,#58100,#58101,
#58102,#58103,#58104),(#58105,#58106,#58107,#58108,#58109,#58110,#58111,
#58112,#58113,#58114,#58115,#58116,#58117,#58118,#58119,#58120,#58121,#58122,
#58123,#58124,#58125,#58126,#58127,#58128,#58129,#58130,#58131,#58132,#58133,
#58134,#58135,#58136,#58137,#58138,#58139,#58140,#58141,#58142,#58143,#58144,
#58145,#58146,#58147,#58148,#58149,#58150,#58151,#58152,#58153,#58154,#58155,
#58156,#58157,#58158,#58159,#58160,#58161,#58162,#58163,#58164,#58165,#58166,
#58167,#58168),(#58169,#58170,#58171,#58172,#58173,#58174,#58175,#58176,
#58177,#58178,#58179,#58180,#58181,#58182,#58183,#58184,#58185,#58186,#58187,
#58188,#58189,#58190,#58191,#58192,#58193,#58194,#58195,#58196,#58197,#58198,
#58199,#58200,#58201,#58202,#58203,#58204,#58205,#58206,#58207,#58208,#58209,
#58210,#58211,#58212,#58213,#58214,#58215,#58216,#58217,#58218,#58219,#58220,
#58221,#58222,#58223,#58224,#58225,#58226,#58227,#58228,#58229,#58230,#58231,
#58232)),.UNSPECIFIED.,.F.,.F.,.F.,(4,4),(4,1,1,1,1,1,1,1,1,1,1,1,1,1,1,
1,1,1,1,1,1,1,1,1,1,1,1,1,1,1,1,1,1,1,1,1,1,1,1,1,1,1,1,1,1,1,1,1,1,1,1,
1,1,1,1,1,1,1,1,1,1,4),(-0.000238498840641111,0.099639560690363),(0.410645887791668,
0.412844762664804,0.415043637537941,0.417242512411078,0.419441387284215,
0.421640262157351,0.423839137030488,0.426038011903625,0.428236886776761,
0.43019144221955,0.431168719940944,0.434100553105126,0.437032386269308,
0.439964219433491,0.442896052597673,0.445827885761855,0.448759718926038,
0.45169155209022,0.454623385254402,0.457555218418585,0.460487051582767,
0.463418884746949,0.465617759620086,0.467816634493223,0.470015509366359,
0.472214384239496,0.474413259112633,0.47661213398577,0.478811008858906,
0.481009883732043,0.48320875860518,0.485407633478317,0.487606508351453,
0.48980538322459,0.491271299806681,0.491454539379443,0.491637778952204,
0.492004258097727,0.492737216388773,0.494203132970864,0.495669049552955,
0.496402007844,0.497134966135046,0.497318205707807,0.497501445280569,0.497867924426092,
0.498600882717137,0.50153271588132,0.504464549045502,0.507396382209684,
0.510328215373866,0.512282770816655,0.514237326259443,0.516191881702231,
0.518390756575368,0.520589631448505,0.522788506321641,0.524987381194778,
0.527186256067915,0.529385130941052,0.531584005814188,0.533782880687325),
 .UNSPECIFIED.);
#315=B_SPLINE_SURFACE_WITH_KNOTS('',3,3,((#58270,#58271,#58272,#58273,#58274,
#58275,#58276,#58277,#58278,#58279,#58280,#58281,#58282,#58283,#58284,#58285,
#58286,#58287,#58288,#58289,#58290,#58291,#58292,#58293,#58294,#58295,#58296,
#58297,#58298,#58299,#58300,#58301,#58302,#58303,#58304,#58305,#58306,#58307,
#58308,#58309,#58310,#58311,#58312,#58313,#58314,#58315,#58316,#58317,#58318,
#58319,#58320,#58321,#58322,#58323,#58324,#58325,#58326,#58327,#58328,#58329,
#58330,#58331,#58332),(#58333,#58334,#58335,#58336,#58337,#58338,#58339,
#58340,#58341,#58342,#58343,#58344,#58345,#58346,#58347,#58348,#58349,#58350,
#58351,#58352,#58353,#58354,#58355,#58356,#58357,#58358,#58359,#58360,#58361,
#58362,#58363,#58364,#58365,#58366,#58367,#58368,#58369,#58370,#58371,#58372,
#58373,#58374,#58375,#58376,#58377,#58378,#58379,#58380,#58381,#58382,#58383,
#58384,#58385,#58386,#58387,#58388,#58389,#58390,#58391,#58392,#58393,#58394,
#58395),(#58396,#58397,#58398,#58399,#58400,#58401,#58402,#58403,#58404,
#58405,#58406,#58407,#58408,#58409,#58410,#58411,#58412,#58413,#58414,#58415,
#58416,#58417,#58418,#58419,#58420,#58421,#58422,#58423,#58424,#58425,#58426,
#58427,#58428,#58429,#58430,#58431,#58432,#58433,#58434,#58435,#58436,#58437,
#58438,#58439,#58440,#58441,#58442,#58443,#58444,#58445,#58446,#58447,#58448,
#58449,#58450,#58451,#58452,#58453,#58454,#58455,#58456,#58457,#58458),
(#58459,#58460,#58461,#58462,#58463,#58464,#58465,#58466,#58467,#58468,
#58469,#58470,#58471,#58472,#58473,#58474,#58475,#58476,#58477,#58478,#58479,
#58480,#58481,#58482,#58483,#58484,#58485,#58486,#58487,#58488,#58489,#58490,
#58491,#58492,#58493,#58494,#58495,#58496,#58497,#58498,#58499,#58500,#58501,
#58502,#58503,#58504,#58505,#58506,#58507,#58508,#58509,#58510,#58511,#58512,
#58513,#58514,#58515,#58516,#58517,#58518,#58519,#58520,#58521)),
 .UNSPECIFIED.,.F.,.F.,.F.,(4,4),(4,1,1,1,1,1,1,1,1,1,1,1,1,1,1,1,1,1,1,
1,1,1,1,1,1,1,1,1,1,1,1,1,1,1,1,1,1,1,1,1,1,1,1,1,1,1,1,1,1,1,1,1,1,1,1,
1,1,1,1,1,4),(-0.000257012103592972,0.0996242942258564),(0.579013511076644,
0.581212386019991,0.583411260963338,0.585610135906685,0.587809010850032,
0.590007885793379,0.592206760736727,0.594405635680074,0.596604510623421,
0.599536343881217,0.602468177139013,0.605400010396809,0.605949729132646,
0.607598885340156,0.609797760283503,0.61199663522685,0.614195510170197,
0.616394385113544,0.618593260056891,0.620792135000238,0.621891572471912,
0.622991009943585,0.625922843201381,0.627388759830279,0.629587634773626,
0.631786509716973,0.633985384660321,0.636184259603668,0.637650176232566,
0.640582009490362,0.642780884433709,0.644979759377056,0.647178634320403,
0.64937750926375,0.651576384207097,0.653775259150444,0.655974134093791,
0.658173009037138,0.659638925666036,0.660371883980485,0.661104842294934,
0.662570758923832,0.66403667555273,0.665502592181628,0.666235550496078,
0.666968508810526,0.669900342068322,0.672832175326119,0.675764008583915,
0.678695841841711,0.680650397346908,0.682604952852106,0.684559508357303,
0.68675838330065,0.688957258243997,0.691156133187344,0.693355008130691,
0.695553883074038,0.697752758017385,0.699951632960732,0.702150507904079),
 .UNSPECIFIED.);
#316=B_SPLINE_SURFACE_WITH_KNOTS('',3,3,((#58563,#58564,#58565,#58566,#58567,
#58568,#58569,#58570,#58571,#58572,#58573,#58574,#58575,#58576,#58577,#58578,
#58579,#58580,#58581,#58582,#58583,#58584,#58585,#58586,#58587,#58588,#58589,
#58590,#58591,#58592,#58593,#58594,#58595,#58596,#58597,#58598,#58599,#58600,
#58601,#58602,#58603,#58604,#58605,#58606,#58607,#58608,#58609,#58610,#58611,
#58612,#58613,#58614,#58615,#58616,#58617,#58618,#58619),(#58620,#58621,
#58622,#58623,#58624,#58625,#58626,#58627,#58628,#58629,#58630,#58631,#58632,
#58633,#58634,#58635,#58636,#58637,#58638,#58639,#58640,#58641,#58642,#58643,
#58644,#58645,#58646,#58647,#58648,#58649,#58650,#58651,#58652,#58653,#58654,
#58655,#58656,#58657,#58658,#58659,#58660,#58661,#58662,#58663,#58664,#58665,
#58666,#58667,#58668,#58669,#58670,#58671,#58672,#58673,#58674,#58675,#58676),
(#58677,#58678,#58679,#58680,#58681,#58682,#58683,#58684,#58685,#58686,
#58687,#58688,#58689,#58690,#58691,#58692,#58693,#58694,#58695,#58696,#58697,
#58698,#58699,#58700,#58701,#58702,#58703,#58704,#58705,#58706,#58707,#58708,
#58709,#58710,#58711,#58712,#58713,#58714,#58715,#58716,#58717,#58718,#58719,
#58720,#58721,#58722,#58723,#58724,#58725,#58726,#58727,#58728,#58729,#58730,
#58731,#58732,#58733),(#58734,#58735,#58736,#58737,#58738,#58739,#58740,
#58741,#58742,#58743,#58744,#58745,#58746,#58747,#58748,#58749,#58750,#58751,
#58752,#58753,#58754,#58755,#58756,#58757,#58758,#58759,#58760,#58761,#58762,
#58763,#58764,#58765,#58766,#58767,#58768,#58769,#58770,#58771,#58772,#58773,
#58774,#58775,#58776,#58777,#58778,#58779,#58780,#58781,#58782,#58783,#58784,
#58785,#58786,#58787,#58788,#58789,#58790)),.UNSPECIFIED.,.F.,.F.,.F.,(4,
4),(4,1,1,1,1,1,1,1,1,1,1,1,1,1,1,1,1,1,1,1,1,1,1,1,1,1,1,1,1,1,1,1,1,1,
1,1,1,1,1,1,1,1,1,1,1,1,1,1,1,1,1,1,1,1,4),(-0.000347032421316872,0.099675803785384),
(0.747330707309962,0.749580010757179,0.751778885415099,0.753977760073019,
0.756176634730939,0.758375509388859,0.760574384046779,0.762773258704699,
0.764972133362619,0.767903966239845,0.769369882678459,0.770835799117072,
0.773767631994299,0.776699464871526,0.779631297748752,0.782563130625979,
0.784762005283899,0.786960879941819,0.789159754599739,0.791358629257659,
0.793557503915579,0.795756378573499,0.797955253231419,0.800154127889339,
0.802353002547259,0.804551877205179,0.806750751863099,0.808949626521019,
0.811148501178939,0.813347375836859,0.815546250494779,0.817745125152699,
0.819943999810619,0.822142874468539,0.823608790907153,0.826540623784379,
0.828739498442299,0.830938373100219,0.833137247758139,0.835336122416059,
0.837534997073979,0.8397338717319,0.84193274638982,0.84413162104774,0.847063453924966,
0.849995286802193,0.85292711967942,0.85512599433734,0.85732486899526,0.85952374365318,
0.8617226183111,0.86392149296902,0.86612036762694,0.86831924228486,0.87051811694278),
 .UNSPECIFIED.);
#317=B_SPLINE_SURFACE_WITH_KNOTS('',3,3,((#60620,#60621,#60622,#60623,#60624,
#60625,#60626,#60627,#60628,#60629,#60630,#60631,#60632,#60633,#60634,#60635,
#60636,#60637,#60638,#60639,#60640,#60641,#60642,#60643,#60644,#60645,#60646,
#60647,#60648,#60649,#60650,#60651,#60652,#60653,#60654,#60655,#60656,#60657,
#60658,#60659,#60660,#60661,#60662,#60663,#60664,#60665,#60666,#60667,#60668,
#60669,#60670,#60671,#60672,#60673,#60674,#60675,#60676,#60677,#60678,#60679,
#60680,#60681,#60682,#60683,#60684,#60685,#60686,#60687,#60688,#60689,#60690,
#60691,#60692,#60693,#60694,#60695,#60696,#60697,#60698,#60699,#60700,#60701,
#60702),(#60703,#60704,#60705,#60706,#60707,#60708,#60709,#60710,#60711,
#60712,#60713,#60714,#60715,#60716,#60717,#60718,#60719,#60720,#60721,#60722,
#60723,#60724,#60725,#60726,#60727,#60728,#60729,#60730,#60731,#60732,#60733,
#60734,#60735,#60736,#60737,#60738,#60739,#60740,#60741,#60742,#60743,#60744,
#60745,#60746,#60747,#60748,#60749,#60750,#60751,#60752,#60753,#60754,#60755,
#60756,#60757,#60758,#60759,#60760,#60761,#60762,#60763,#60764,#60765,#60766,
#60767,#60768,#60769,#60770,#60771,#60772,#60773,#60774,#60775,#60776,#60777,
#60778,#60779,#60780,#60781,#60782,#60783,#60784,#60785),(#60786,#60787,
#60788,#60789,#60790,#60791,#60792,#60793,#60794,#60795,#60796,#60797,#60798,
#60799,#60800,#60801,#60802,#60803,#60804,#60805,#60806,#60807,#60808,#60809,
#60810,#60811,#60812,#60813,#60814,#60815,#60816,#60817,#60818,#60819,#60820,
#60821,#60822,#60823,#60824,#60825,#60826,#60827,#60828,#60829,#60830,#60831,
#60832,#60833,#60834,#60835,#60836,#60837,#60838,#60839,#60840,#60841,#60842,
#60843,#60844,#60845,#60846,#60847,#60848,#60849,#60850,#60851,#60852,#60853,
#60854,#60855,#60856,#60857,#60858,#60859,#60860,#60861,#60862,#60863,#60864,
#60865,#60866,#60867,#60868),(#60869,#60870,#60871,#60872,#60873,#60874,
#60875,#60876,#60877,#60878,#60879,#60880,#60881,#60882,#60883,#60884,#60885,
#60886,#60887,#60888,#60889,#60890,#60891,#60892,#60893,#60894,#60895,#60896,
#60897,#60898,#60899,#60900,#60901,#60902,#60903,#60904,#60905,#60906,#60907,
#60908,#60909,#60910,#60911,#60912,#60913,#60914,#60915,#60916,#60917,#60918,
#60919,#60920,#60921,#60922,#60923,#60924,#60925,#60926,#60927,#60928,#60929,
#60930,#60931,#60932,#60933,#60934,#60935,#60936,#60937,#60938,#60939,#60940,
#60941,#60942,#60943,#60944,#60945,#60946,#60947,#60948,#60949,#60950,#60951)),
 .UNSPECIFIED.,.F.,.F.,.F.,(4,4),(4,1,1,1,1,1,1,1,1,1,1,1,1,1,1,1,1,1,1,
1,1,1,1,1,1,1,1,1,1,1,1,1,1,1,1,1,1,1,1,1,1,1,1,1,1,1,1,1,1,1,1,1,1,1,1,
1,1,1,1,1,1,1,1,1,1,1,1,1,1,1,1,1,1,1,1,1,1,1,1,1,4),(-0.000191727474006969,
0.120034558936103),(0.0144970658303938,0.0170193973464053,0.0195077183395957,
0.021996039332786,0.0244843603259764,0.0269726813191668,0.0294610023123572,
0.0319493233055476,0.034437644298738,0.0366494851815739,0.0388613260644098,
0.0410731669472457,0.0427320476093726,0.0443909282714996,0.0460498089336265,
0.0477086895957534,0.0493675702578804,0.0510264509200073,0.0526853315821342,
0.0535147719131977,0.0543442122442611,0.0560030929063881,0.057661973568515,
0.0593208542306419,0.0605650147272371,0.0609797348927689,0.0626386155548958,
0.0642974962170227,0.0659563768791496,0.0676152575412766,0.0680299777068083,
0.06844469787234,0.0692741382034035,0.0709330188655304,0.0725918995276573,
0.0742507801897843,0.0759096608519112,0.0775685415140381,0.0792274221761651,
0.080886302838292,0.0825451835004189,0.0842040641625458,0.0858629448246728,
0.0875218254867997,0.0891807061489266,0.0908395868110536,0.0924984674731805,
0.0941573481353074,0.0958162287974343,0.0974751094595613,0.0991339901216882,
0.100792870783815,0.102451751445942,0.104110632108069,0.105769512770196,
0.107428393432323,0.109640234315159,0.111852075197995,0.114063916080831,
0.114893356411894,0.115722796742957,0.117381677405084,0.119040558067211,
0.120699438729338,0.122358319391465,0.124017200053592,0.125676080715719,
0.127334961377846,0.128440881819264,0.129546802260682,0.131758643143518,
0.132864563584936,0.133970484026354,0.136458805019544,0.138947126012734,
0.141435447005925,0.143923767999115,0.146412088992306,0.148900409985496,
0.151388730978686,0.154068779445884),.UNSPECIFIED.);
#318=B_SPLINE_SURFACE_WITH_KNOTS('',3,3,((#61850,#61851,#61852,#61853,#61854,
#61855,#61856,#61857,#61858,#61859,#61860,#61861,#61862,#61863,#61864,#61865,
#61866,#61867,#61868,#61869,#61870,#61871,#61872,#61873,#61874,#61875,#61876,
#61877,#61878,#61879,#61880,#61881,#61882,#61883,#61884,#61885,#61886,#61887,
#61888,#61889,#61890,#61891,#61892,#61893,#61894,#61895,#61896,#61897,#61898,
#61899,#61900,#61901,#61902,#61903,#61904,#61905,#61906,#61907,#61908,#61909,
#61910,#61911,#61912,#61913,#61914,#61915,#61916,#61917,#61918,#61919,#61920,
#61921,#61922,#61923,#61924,#61925,#61926,#61927,#61928,#61929,#61930,#61931,
#61932,#61933,#61934,#61935,#61936,#61937,#61938),(#61939,#61940,#61941,
#61942,#61943,#61944,#61945,#61946,#61947,#61948,#61949,#61950,#61951,#61952,
#61953,#61954,#61955,#61956,#61957,#61958,#61959,#61960,#61961,#61962,#61963,
#61964,#61965,#61966,#61967,#61968,#61969,#61970,#61971,#61972,#61973,#61974,
#61975,#61976,#61977,#61978,#61979,#61980,#61981,#61982,#61983,#61984,#61985,
#61986,#61987,#61988,#61989,#61990,#61991,#61992,#61993,#61994,#61995,#61996,
#61997,#61998,#61999,#62000,#62001,#62002,#62003,#62004,#62005,#62006,#62007,
#62008,#62009,#62010,#62011,#62012,#62013,#62014,#62015,#62016,#62017,#62018,
#62019,#62020,#62021,#62022,#62023,#62024,#62025,#62026,#62027),(#62028,
#62029,#62030,#62031,#62032,#62033,#62034,#62035,#62036,#62037,#62038,#62039,
#62040,#62041,#62042,#62043,#62044,#62045,#62046,#62047,#62048,#62049,#62050,
#62051,#62052,#62053,#62054,#62055,#62056,#62057,#62058,#62059,#62060,#62061,
#62062,#62063,#62064,#62065,#62066,#62067,#62068,#62069,#62070,#62071,#62072,
#62073,#62074,#62075,#62076,#62077,#62078,#62079,#62080,#62081,#62082,#62083,
#62084,#62085,#62086,#62087,#62088,#62089,#62090,#62091,#62092,#62093,#62094,
#62095,#62096,#62097,#62098,#62099,#62100,#62101,#62102,#62103,#62104,#62105,
#62106,#62107,#62108,#62109,#62110,#62111,#62112,#62113,#62114,#62115,#62116),
(#62117,#62118,#62119,#62120,#62121,#62122,#62123,#62124,#62125,#62126,
#62127,#62128,#62129,#62130,#62131,#62132,#62133,#62134,#62135,#62136,#62137,
#62138,#62139,#62140,#62141,#62142,#62143,#62144,#62145,#62146,#62147,#62148,
#62149,#62150,#62151,#62152,#62153,#62154,#62155,#62156,#62157,#62158,#62159,
#62160,#62161,#62162,#62163,#62164,#62165,#62166,#62167,#62168,#62169,#62170,
#62171,#62172,#62173,#62174,#62175,#62176,#62177,#62178,#62179,#62180,#62181,
#62182,#62183,#62184,#62185,#62186,#62187,#62188,#62189,#62190,#62191,#62192,
#62193,#62194,#62195,#62196,#62197,#62198,#62199,#62200,#62201,#62202,#62203,
#62204,#62205)),.UNSPECIFIED.,.F.,.F.,.F.,(4,4),(4,1,1,1,1,1,1,1,1,1,1,
1,1,1,1,1,1,1,1,1,1,1,1,1,1,1,1,1,1,1,1,1,1,1,1,1,1,1,1,1,1,1,1,1,1,1,1,
1,1,1,1,1,1,1,1,1,1,1,1,1,1,1,1,1,1,1,1,1,1,1,1,1,1,1,1,1,1,1,1,1,1,1,1,
1,1,1,4),(-0.000343847952555671,0.120053031443545),(0.18284601578435,0.185387336016129,
0.187875651349888,0.190363966683647,0.192852282017407,0.194096439684286,
0.195340597351166,0.196584755018045,0.197828912684925,0.200317228018684,
0.201561385685564,0.202805543352443,0.204464420241616,0.206123297130789,
0.207782174019962,0.209441050909135,0.211099927798308,0.21275880468748,
0.214417681576653,0.21524712002124,0.215869198854679,0.216076558465826,
0.217735435354999,0.219394312244172,0.221053189133344,0.222712066022517,
0.22437094291169,0.226029819800863,0.227135737726978,0.229347573579209,
0.229900532542266,0.230453491505324,0.231559409431439,0.233771245283669,
0.2359830811359,0.237641958025073,0.239300834914246,0.240959711803418,0.242618588692591,
0.244277465581764,0.245936342470937,0.24759521936011,0.249254096249282,
0.250912973138455,0.252571850027628,0.254230726916801,0.255889603805974,
0.258101439658204,0.260313275510435,0.262525111362665,0.26363102928878,
0.264736947214895,0.266948783067126,0.269160618919356,0.270819495808529,
0.272478372697702,0.274966688031461,0.275796126476048,0.27745500336522,
0.279113880254393,0.280772757143566,0.282431634032739,0.284090510921912,
0.285749387811084,0.286578826255671,0.287408264700257,0.288237703144844,
0.28906714158943,0.291140737700896,0.292384895367776,0.294043772256949,
0.295702649146121,0.297914484998352,0.300126320850582,0.30067927981364,
0.302338156702813,0.302960235536253,0.303582314369692,0.304826472036572,
0.307314787370331,0.308558945037211,0.30980310270409,0.31229141803785,0.314779733371609,
0.317268048705368,0.319756364039127,0.322588480100517),.UNSPECIFIED.);
#319=B_SPLINE_SURFACE_WITH_KNOTS('',3,3,((#63143,#63144,#63145,#63146,#63147,
#63148,#63149,#63150,#63151,#63152,#63153,#63154,#63155,#63156,#63157,#63158,
#63159,#63160,#63161,#63162,#63163,#63164,#63165,#63166,#63167,#63168,#63169,
#63170,#63171,#63172,#63173,#63174,#63175,#63176,#63177,#63178,#63179,#63180,
#63181,#63182,#63183,#63184,#63185,#63186,#63187,#63188,#63189,#63190,#63191,
#63192,#63193,#63194,#63195,#63196,#63197,#63198,#63199,#63200,#63201,#63202,
#63203,#63204,#63205,#63206,#63207,#63208,#63209,#63210,#63211,#63212,#63213,
#63214,#63215,#63216,#63217,#63218,#63219,#63220,#63221,#63222,#63223,#63224,
#63225,#63226),(#63227,#63228,#63229,#63230,#63231,#63232,#63233,#63234,
#63235,#63236,#63237,#63238,#63239,#63240,#63241,#63242,#63243,#63244,#63245,
#63246,#63247,#63248,#63249,#63250,#63251,#63252,#63253,#63254,#63255,#63256,
#63257,#63258,#63259,#63260,#63261,#63262,#63263,#63264,#63265,#63266,#63267,
#63268,#63269,#63270,#63271,#63272,#63273,#63274,#63275,#63276,#63277,#63278,
#63279,#63280,#63281,#63282,#63283,#63284,#63285,#63286,#63287,#63288,#63289,
#63290,#63291,#63292,#63293,#63294,#63295,#63296,#63297,#63298,#63299,#63300,
#63301,#63302,#63303,#63304,#63305,#63306,#63307,#63308,#63309,#63310),
(#63311,#63312,#63313,#63314,#63315,#63316,#63317,#63318,#63319,#63320,
#63321,#63322,#63323,#63324,#63325,#63326,#63327,#63328,#63329,#63330,#63331,
#63332,#63333,#63334,#63335,#63336,#63337,#63338,#63339,#63340,#63341,#63342,
#63343,#63344,#63345,#63346,#63347,#63348,#63349,#63350,#63351,#63352,#63353,
#63354,#63355,#63356,#63357,#63358,#63359,#63360,#63361,#63362,#63363,#63364,
#63365,#63366,#63367,#63368,#63369,#63370,#63371,#63372,#63373,#63374,#63375,
#63376,#63377,#63378,#63379,#63380,#63381,#63382,#63383,#63384,#63385,#63386,
#63387,#63388,#63389,#63390,#63391,#63392,#63393,#63394),(#63395,#63396,
#63397,#63398,#63399,#63400,#63401,#63402,#63403,#63404,#63405,#63406,#63407,
#63408,#63409,#63410,#63411,#63412,#63413,#63414,#63415,#63416,#63417,#63418,
#63419,#63420,#63421,#63422,#63423,#63424,#63425,#63426,#63427,#63428,#63429,
#63430,#63431,#63432,#63433,#63434,#63435,#63436,#63437,#63438,#63439,#63440,
#63441,#63442,#63443,#63444,#63445,#63446,#63447,#63448,#63449,#63450,#63451,
#63452,#63453,#63454,#63455,#63456,#63457,#63458,#63459,#63460,#63461,#63462,
#63463,#63464,#63465,#63466,#63467,#63468,#63469,#63470,#63471,#63472,#63473,
#63474,#63475,#63476,#63477,#63478)),.UNSPECIFIED.,.F.,.F.,.F.,(4,4),(4,
1,1,1,1,1,1,1,1,1,1,1,1,1,1,1,1,1,1,1,1,1,1,1,1,1,1,1,1,1,1,1,1,1,1,1,1,
1,1,1,1,1,1,1,1,1,1,1,1,1,1,1,1,1,1,1,1,1,1,1,1,1,1,1,1,1,1,1,1,1,1,1,1,
1,1,1,1,1,1,1,1,4),(-0.000608094264401172,0.120053332327022),(0.35121353206522,
0.353754974599999,0.356243289735703,0.358731604871407,0.361219920007111,
0.363708235142815,0.364952392710666,0.366196550278518,0.368684865414222,
0.369929022982074,0.371173180549926,0.372832057307062,0.374490934064198,
0.376149810821334,0.37780868757847,0.379467564335606,0.381126441092742,
0.382785317849878,0.384444194607014,0.385273632985582,0.38610307136415,
0.387761948121286,0.389420824878422,0.391079701635558,0.392738578392693,
0.394397455149829,0.396056331906965,0.397715208664101,0.398821126502192,
0.399927044340283,0.402138880016464,0.404350715692645,0.406009592449781,
0.407668469206917,0.409327345964053,0.410986222721189,0.412645099478325,
0.414303976235461,0.415133414614029,0.415962852992597,0.416792291371165,
0.417621729749733,0.419280606506868,0.420939483264004,0.42259836002114,
0.424257236778276,0.426469072454458,0.428680908130639,0.43089274380682,
0.433104579483001,0.435316415159183,0.436422332997273,0.437528250835364,
0.4391871275925,0.440846004349636,0.442504881106772,0.444163757863908,0.445822634621044,
0.447481511378179,0.447896230567463,0.449140388135315,0.450799264892451,
0.452458141649587,0.454117018406723,0.455775895163859,0.457434771920995,
0.459093648678131,0.460752525435267,0.462411402192403,0.464070278949539,
0.46628211462572,0.468493950301901,0.470705785978083,0.471949943545935,
0.473194101113787,0.47568241624949,0.478170731385194,0.480659046520898,
0.483147361656602,0.485635676792306,0.48812399192801,0.491010307170531),
 .UNSPECIFIED.);
#320=B_SPLINE_SURFACE_WITH_KNOTS('',3,3,((#64056,#64057,#64058,#64059,#64060,
#64061,#64062,#64063,#64064,#64065,#64066,#64067,#64068,#64069,#64070,#64071,
#64072,#64073,#64074,#64075,#64076,#64077,#64078,#64079,#64080,#64081,#64082,
#64083,#64084,#64085,#64086,#64087,#64088,#64089,#64090,#64091,#64092,#64093,
#64094,#64095,#64096,#64097,#64098,#64099,#64100,#64101,#64102,#64103,#64104,
#64105,#64106,#64107,#64108,#64109,#64110,#64111,#64112,#64113,#64114,#64115,
#64116,#64117,#64118,#64119,#64120,#64121,#64122,#64123,#64124,#64125,#64126,
#64127,#64128,#64129,#64130,#64131,#64132,#64133,#64134,#64135,#64136,#64137,
#64138,#64139,#64140,#64141),(#64142,#64143,#64144,#64145,#64146,#64147,
#64148,#64149,#64150,#64151,#64152,#64153,#64154,#64155,#64156,#64157,#64158,
#64159,#64160,#64161,#64162,#64163,#64164,#64165,#64166,#64167,#64168,#64169,
#64170,#64171,#64172,#64173,#64174,#64175,#64176,#64177,#64178,#64179,#64180,
#64181,#64182,#64183,#64184,#64185,#64186,#64187,#64188,#64189,#64190,#64191,
#64192,#64193,#64194,#64195,#64196,#64197,#64198,#64199,#64200,#64201,#64202,
#64203,#64204,#64205,#64206,#64207,#64208,#64209,#64210,#64211,#64212,#64213,
#64214,#64215,#64216,#64217,#64218,#64219,#64220,#64221,#64222,#64223,#64224,
#64225,#64226,#64227),(#64228,#64229,#64230,#64231,#64232,#64233,#64234,
#64235,#64236,#64237,#64238,#64239,#64240,#64241,#64242,#64243,#64244,#64245,
#64246,#64247,#64248,#64249,#64250,#64251,#64252,#64253,#64254,#64255,#64256,
#64257,#64258,#64259,#64260,#64261,#64262,#64263,#64264,#64265,#64266,#64267,
#64268,#64269,#64270,#64271,#64272,#64273,#64274,#64275,#64276,#64277,#64278,
#64279,#64280,#64281,#64282,#64283,#64284,#64285,#64286,#64287,#64288,#64289,
#64290,#64291,#64292,#64293,#64294,#64295,#64296,#64297,#64298,#64299,#64300,
#64301,#64302,#64303,#64304,#64305,#64306,#64307,#64308,#64309,#64310,#64311,
#64312,#64313),(#64314,#64315,#64316,#64317,#64318,#64319,#64320,#64321,
#64322,#64323,#64324,#64325,#64326,#64327,#64328,#64329,#64330,#64331,#64332,
#64333,#64334,#64335,#64336,#64337,#64338,#64339,#64340,#64341,#64342,#64343,
#64344,#64345,#64346,#64347,#64348,#64349,#64350,#64351,#64352,#64353,#64354,
#64355,#64356,#64357,#64358,#64359,#64360,#64361,#64362,#64363,#64364,#64365,
#64366,#64367,#64368,#64369,#64370,#64371,#64372,#64373,#64374,#64375,#64376,
#64377,#64378,#64379,#64380,#64381,#64382,#64383,#64384,#64385,#64386,#64387,
#64388,#64389,#64390,#64391,#64392,#64393,#64394,#64395,#64396,#64397,#64398,
#64399)),.UNSPECIFIED.,.F.,.F.,.F.,(4,4),(4,1,1,1,1,1,1,1,1,1,1,1,1,1,1,
1,1,1,1,1,1,1,1,1,1,1,1,1,1,1,1,1,1,1,1,1,1,1,1,1,1,1,1,1,1,1,1,1,1,1,1,
1,1,1,1,1,1,1,1,1,1,1,1,1,1,1,1,1,1,1,1,1,1,1,1,1,1,1,1,1,1,1,1,4),(-0.0004813933155718,
0.120112165916443),(0.519522122356523,0.522122603429753,0.524610918586542,
0.527099233743331,0.52958754890012,0.532075864056908,0.534564179213697,
0.537052494370486,0.539540809527275,0.541199686298467,0.54285856306966,
0.544517439840852,0.546176316612045,0.547835193383237,0.548664631768834,
0.54949407015443,0.551152946925622,0.551982385311219,0.552397104504017,
0.552604464100416,0.552811823696815,0.5561295772392,0.559447330781585,0.561106207552778,
0.56276508432397,0.566082837866355,0.566290197462754,0.566497557059153,
0.566912276251951,0.567741714637548,0.568571153023144,0.56940059140874,
0.571059468179933,0.572718344951125,0.574377221722318,0.57603609849351,
0.577694975264703,0.579353852035895,0.581012728807088,0.58267160557828,
0.584330482349473,0.585989359120665,0.587648235891858,0.58930711266305,
0.590965989434243,0.592624866205435,0.594836701900359,0.597048537595282,
0.599260373290205,0.600366291137667,0.600919250061398,0.601472208985129,
0.604789962527514,0.605895880374975,0.607554757146168,0.60921363391736,
0.610872510688553,0.612531387459745,0.614190264230938,0.615849141002131,
0.616263860194929,0.616678579387727,0.617508017773323,0.619166894544516,
0.620825771315708,0.622484648086901,0.624143524858093,0.625802401629286,
0.627461278400478,0.629120155171671,0.630779031942863,0.632437908714056,
0.634649744408979,0.636861580103902,0.639073415798826,0.64031757337722,
0.641561730955615,0.644050046112403,0.646538361269192,0.649026676425981,
0.65151499158277,0.654003306739558,0.656491621896347,0.659296609515059),
 .UNSPECIFIED.);
#321=B_SPLINE_SURFACE_WITH_KNOTS('',3,3,((#65370,#65371,#65372,#65373,#65374,
#65375,#65376,#65377,#65378,#65379,#65380,#65381,#65382,#65383,#65384,#65385,
#65386,#65387,#65388,#65389,#65390,#65391,#65392,#65393,#65394,#65395,#65396,
#65397,#65398,#65399,#65400,#65401,#65402,#65403,#65404,#65405,#65406,#65407,
#65408,#65409,#65410,#65411,#65412,#65413,#65414,#65415,#65416,#65417,#65418,
#65419,#65420,#65421,#65422,#65423,#65424,#65425,#65426,#65427,#65428,#65429,
#65430,#65431,#65432,#65433,#65434,#65435,#65436,#65437,#65438,#65439,#65440,
#65441,#65442,#65443,#65444,#65445,#65446,#65447,#65448,#65449,#65450,#65451,
#65452,#65453,#65454,#65455,#65456,#65457,#65458,#65459,#65460),(#65461,
#65462,#65463,#65464,#65465,#65466,#65467,#65468,#65469,#65470,#65471,#65472,
#65473,#65474,#65475,#65476,#65477,#65478,#65479,#65480,#65481,#65482,#65483,
#65484,#65485,#65486,#65487,#65488,#65489,#65490,#65491,#65492,#65493,#65494,
#65495,#65496,#65497,#65498,#65499,#65500,#65501,#65502,#65503,#65504,#65505,
#65506,#65507,#65508,#65509,#65510,#65511,#65512,#65513,#65514,#65515,#65516,
#65517,#65518,#65519,#65520,#65521,#65522,#65523,#65524,#65525,#65526,#65527,
#65528,#65529,#65530,#65531,#65532,#65533,#65534,#65535,#65536,#65537,#65538,
#65539,#65540,#65541,#65542,#65543,#65544,#65545,#65546,#65547,#65548,#65549,
#65550,#65551),(#65552,#65553,#65554,#65555,#65556,#65557,#65558,#65559,
#65560,#65561,#65562,#65563,#65564,#65565,#65566,#65567,#65568,#65569,#65570,
#65571,#65572,#65573,#65574,#65575,#65576,#65577,#65578,#65579,#65580,#65581,
#65582,#65583,#65584,#65585,#65586,#65587,#65588,#65589,#65590,#65591,#65592,
#65593,#65594,#65595,#65596,#65597,#65598,#65599,#65600,#65601,#65602,#65603,
#65604,#65605,#65606,#65607,#65608,#65609,#65610,#65611,#65612,#65613,#65614,
#65615,#65616,#65617,#65618,#65619,#65620,#65621,#65622,#65623,#65624,#65625,
#65626,#65627,#65628,#65629,#65630,#65631,#65632,#65633,#65634,#65635,#65636,
#65637,#65638,#65639,#65640,#65641,#65642),(#65643,#65644,#65645,#65646,
#65647,#65648,#65649,#65650,#65651,#65652,#65653,#65654,#65655,#65656,#65657,
#65658,#65659,#65660,#65661,#65662,#65663,#65664,#65665,#65666,#65667,#65668,
#65669,#65670,#65671,#65672,#65673,#65674,#65675,#65676,#65677,#65678,#65679,
#65680,#65681,#65682,#65683,#65684,#65685,#65686,#65687,#65688,#65689,#65690,
#65691,#65692,#65693,#65694,#65695,#65696,#65697,#65698,#65699,#65700,#65701,
#65702,#65703,#65704,#65705,#65706,#65707,#65708,#65709,#65710,#65711,#65712,
#65713,#65714,#65715,#65716,#65717,#65718,#65719,#65720,#65721,#65722,#65723,
#65724,#65725,#65726,#65727,#65728,#65729,#65730,#65731,#65732,#65733)),
 .UNSPECIFIED.,.F.,.F.,.F.,(4,4),(4,1,1,1,1,1,1,1,1,1,1,1,1,1,1,1,1,1,1,
1,1,1,1,1,1,1,1,1,1,1,1,1,1,1,1,1,1,1,1,1,1,1,1,1,1,1,1,1,1,1,1,1,1,1,1,
1,1,1,1,1,1,1,1,1,1,1,1,1,1,1,1,1,1,1,1,1,1,1,1,1,1,1,1,1,1,1,1,1,4),(-0.000337432449522167,
0.120000000000001),(0.688001912782254,0.690490227769403,0.692978542756553,
0.695466857743702,0.697955172730851,0.700443487718,0.702931802705149,0.705420117692299,
0.707908432679448,0.710120268223581,0.712332103767713,0.714543939311846,
0.716202815969945,0.717861692628045,0.719520569286144,0.721179445944244,
0.722838322602343,0.724497199260443,0.726156075918542,0.727814952576642,
0.729473829234741,0.731132705892841,0.73279158255094,0.73445045920904,0.736109335867139,
0.737768212525239,0.739427089183338,0.741085965841438,0.742191883613504,
0.74329780138557,0.745509636929703,0.747721472473835,0.749933308017968,
0.752145143562101,0.753251061334167,0.7538040202202,0.754080499663217,0.754356979106233,
0.757674732422432,0.759333609080532,0.760992485738631,0.761407204903156,
0.761821924067681,0.762651362396731,0.763480800725781,0.76431023905483,
0.76513967738388,0.76596911571293,0.766798554041979,0.767627992371029,0.769286869029129,
0.770945745687228,0.772604622345328,0.774263499003427,0.775922375661527,
0.777581252319626,0.779240128977726,0.780899005635825,0.783110841179958,
0.78532267672409,0.787534512268223,0.789193388926323,0.790852265584422,
0.792511142242522,0.794170018900621,0.79582889555872,0.79748777221682,0.798731929710395,
0.800805525533019,0.802464402191118,0.804123278849218,0.804537998013743,
0.805782155507317,0.807441032165417,0.808063110912204,0.808685189658991,
0.809929347152566,0.811173504646141,0.812417662139715,0.814905977126865,
0.817394292114014,0.817705331487407,0.818638449607588,0.819882607101163,
0.821126764594738,0.822370922088312,0.8229930008351,0.824859237075461,0.827347552062611),
 .UNSPECIFIED.);
#322=B_SPLINE_SURFACE_WITH_KNOTS('',3,3,((#65787,#65788,#65789,#65790,#65791,
#65792,#65793,#65794,#65795,#65796,#65797),(#65798,#65799,#65800,#65801,
#65802,#65803,#65804,#65805,#65806,#65807,#65808),(#65809,#65810,#65811,
#65812,#65813,#65814,#65815,#65816,#65817,#65818,#65819),(#65820,#65821,
#65822,#65823,#65824,#65825,#65826,#65827,#65828,#65829,#65830)),
 .UNSPECIFIED.,.F.,.F.,.F.,(4,4),(4,1,1,1,1,1,1,1,4),(0.05527911728358,
0.0996900551293098),(0.981477459445449,0.984165788573041,0.986804823810868,
0.989443859048694,0.992082894286521,0.994721929524347,0.997360964762174,
0.998680482381087,1.00004977012262),.UNSPECIFIED.);
#323=B_SPLINE_SURFACE_WITH_KNOTS('',3,3,((#65831,#65832,#65833,#65834,#65835,
#65836,#65837,#65838,#65839,#65840,#65841,#65842,#65843,#65844,#65845,#65846,
#65847,#65848,#65849,#65850,#65851,#65852,#65853,#65854,#65855,#65856,#65857,
#65858,#65859,#65860,#65861,#65862,#65863,#65864,#65865,#65866,#65867,#65868,
#65869,#65870,#65871,#65872,#65873,#65874,#65875,#65876),(#65877,#65878,
#65879,#65880,#65881,#65882,#65883,#65884,#65885,#65886,#65887,#65888,#65889,
#65890,#65891,#65892,#65893,#65894,#65895,#65896,#65897,#65898,#65899,#65900,
#65901,#65902,#65903,#65904,#65905,#65906,#65907,#65908,#65909,#65910,#65911,
#65912,#65913,#65914,#65915,#65916,#65917,#65918,#65919,#65920,#65921,#65922),
(#65923,#65924,#65925,#65926,#65927,#65928,#65929,#65930,#65931,#65932,
#65933,#65934,#65935,#65936,#65937,#65938,#65939,#65940,#65941,#65942,#65943,
#65944,#65945,#65946,#65947,#65948,#65949,#65950,#65951,#65952,#65953,#65954,
#65955,#65956,#65957,#65958,#65959,#65960,#65961,#65962,#65963,#65964,#65965,
#65966,#65967,#65968),(#65969,#65970,#65971,#65972,#65973,#65974,#65975,
#65976,#65977,#65978,#65979,#65980,#65981,#65982,#65983,#65984,#65985,#65986,
#65987,#65988,#65989,#65990,#65991,#65992,#65993,#65994,#65995,#65996,#65997,
#65998,#65999,#66000,#66001,#66002,#66003,#66004,#66005,#66006,#66007,#66008,
#66009,#66010,#66011,#66012,#66013,#66014)),.UNSPECIFIED.,.F.,.F.,.F.,(4,
4),(4,1,1,1,1,1,1,1,1,1,1,1,1,1,1,1,1,1,1,1,1,1,1,1,1,1,1,1,1,1,1,1,1,1,
1,1,1,1,1,1,1,1,1,4),(-0.000533053460610251,0.0996242942258564),(0.,0.00168771915268776,
0.00337543830537552,0.00675087661075104,0.0101263149161266,0.0135017532215021,
0.0157520454250858,0.0180023376286695,0.0202526298322531,0.0219403489849409,
0.0236280681376287,0.0253157872903164,0.0270035064430042,0.0292537986465879,
0.0315040908501715,0.0337543830537552,0.0360046752573389,0.0382549674609226,
0.0405052596645063,0.0427555518680899,0.0450058440716736,0.0472561362752573,
0.049506428478841,0.0517567206824247,0.0540070128860084,0.0556947320386961,
0.0573824511913839,0.0590701703440716,0.0607578894967594,0.0641333278021349,
0.0658210469548227,0.0675087661075104,0.0691964852601982,0.070884204412886,
0.0725719235655737,0.0742596427182615,0.0765099349218452,0.0787602271254289,
0.0810105193290125,0.0843859576343881,0.0877613959397636,0.0911368342451391,
0.0928245533978269,0.0945122725505146),.UNSPECIFIED.);
#324=B_SPLINE_SURFACE_WITH_KNOTS('',3,3,((#66016,#66017,#66018,#66019,#66020,
#66021,#66022,#66023,#66024,#66025,#66026,#66027,#66028,#66029,#66030,#66031,
#66032,#66033,#66034,#66035,#66036,#66037,#66038,#66039,#66040,#66041,#66042,
#66043,#66044,#66045,#66046,#66047,#66048,#66049,#66050,#66051,#66052,#66053,
#66054,#66055,#66056,#66057,#66058,#66059,#66060,#66061,#66062,#66063,#66064,
#66065,#66066,#66067,#66068,#66069,#66070,#66071,#66072,#66073,#66074,#66075,
#66076,#66077,#66078),(#66079,#66080,#66081,#66082,#66083,#66084,#66085,
#66086,#66087,#66088,#66089,#66090,#66091,#66092,#66093,#66094,#66095,#66096,
#66097,#66098,#66099,#66100,#66101,#66102,#66103,#66104,#66105,#66106,#66107,
#66108,#66109,#66110,#66111,#66112,#66113,#66114,#66115,#66116,#66117,#66118,
#66119,#66120,#66121,#66122,#66123,#66124,#66125,#66126,#66127,#66128,#66129,
#66130,#66131,#66132,#66133,#66134,#66135,#66136,#66137,#66138,#66139,#66140,
#66141),(#66142,#66143,#66144,#66145,#66146,#66147,#66148,#66149,#66150,
#66151,#66152,#66153,#66154,#66155,#66156,#66157,#66158,#66159,#66160,#66161,
#66162,#66163,#66164,#66165,#66166,#66167,#66168,#66169,#66170,#66171,#66172,
#66173,#66174,#66175,#66176,#66177,#66178,#66179,#66180,#66181,#66182,#66183,
#66184,#66185,#66186,#66187,#66188,#66189,#66190,#66191,#66192,#66193,#66194,
#66195,#66196,#66197,#66198,#66199,#66200,#66201,#66202,#66203,#66204),
(#66205,#66206,#66207,#66208,#66209,#66210,#66211,#66212,#66213,#66214,
#66215,#66216,#66217,#66218,#66219,#66220,#66221,#66222,#66223,#66224,#66225,
#66226,#66227,#66228,#66229,#66230,#66231,#66232,#66233,#66234,#66235,#66236,
#66237,#66238,#66239,#66240,#66241,#66242,#66243,#66244,#66245,#66246,#66247,
#66248,#66249,#66250,#66251,#66252,#66253,#66254,#66255,#66256,#66257,#66258,
#66259,#66260,#66261,#66262,#66263,#66264,#66265,#66266,#66267)),
 .UNSPECIFIED.,.F.,.F.,.F.,(4,4),(4,1,1,1,1,1,1,1,1,1,1,1,1,1,1,1,1,1,1,
1,1,1,1,1,1,1,1,1,1,1,1,1,1,1,1,1,1,1,1,1,1,1,1,1,1,1,1,1,1,1,1,1,1,1,1,
1,1,1,1,1,4),(-0.000237162028320192,0.0996382913295698),(0.139688666527305,
0.141888509865,0.144088353202694,0.146288196540389,0.148488039878084,0.150687883215779,
0.152887726553474,0.155087569891169,0.157287413228864,0.160220537679124,
0.163153662129384,0.164620224354514,0.166086786579644,0.167553348804774,
0.169019911029903,0.171953035480163,0.174886159930423,0.177086003268118,
0.179285846605813,0.181485689943508,0.183685533281203,0.184235494115627,
0.18478545495005,0.185885376618898,0.188085219956593,0.190285063294288,
0.192484906631983,0.194684749969677,0.196884593307372,0.199084436645067,
0.200184358313915,0.200734319148339,0.201284279982762,0.203484123320457,
0.205683966658152,0.207883809995847,0.210083653333542,0.213016777783802,
0.215949902234062,0.218883026684322,0.221816151134581,0.224749275584841,
0.227682400035101,0.229148962260231,0.230615524485361,0.233548648935621,
0.236481773385881,0.239414897836141,0.241370314136314,0.243325730436487,
0.244303438586574,0.245281146736661,0.246381068405508,0.247480990074355,
0.24968083341205,0.251880676749745,0.25408052008744,0.256280363425135,0.25848020676283,
0.260680050100525,0.26287989343822),.UNSPECIFIED.);
#325=B_SPLINE_SURFACE_WITH_KNOTS('',3,3,((#66268,#66269,#66270,#66271,#66272,
#66273,#66274,#66275,#66276,#66277,#66278,#66279,#66280,#66281,#66282,#66283,
#66284,#66285,#66286,#66287,#66288,#66289,#66290,#66291,#66292,#66293,#66294,
#66295,#66296,#66297,#66298,#66299,#66300,#66301,#66302,#66303,#66304,#66305,
#66306,#66307,#66308,#66309,#66310,#66311,#66312,#66313,#66314,#66315,#66316,
#66317,#66318,#66319,#66320,#66321,#66322,#66323,#66324,#66325,#66326,#66327,
#66328,#66329,#66330,#66331),(#66332,#66333,#66334,#66335,#66336,#66337,
#66338,#66339,#66340,#66341,#66342,#66343,#66344,#66345,#66346,#66347,#66348,
#66349,#66350,#66351,#66352,#66353,#66354,#66355,#66356,#66357,#66358,#66359,
#66360,#66361,#66362,#66363,#66364,#66365,#66366,#66367,#66368,#66369,#66370,
#66371,#66372,#66373,#66374,#66375,#66376,#66377,#66378,#66379,#66380,#66381,
#66382,#66383,#66384,#66385,#66386,#66387,#66388,#66389,#66390,#66391,#66392,
#66393,#66394,#66395),(#66396,#66397,#66398,#66399,#66400,#66401,#66402,
#66403,#66404,#66405,#66406,#66407,#66408,#66409,#66410,#66411,#66412,#66413,
#66414,#66415,#66416,#66417,#66418,#66419,#66420,#66421,#66422,#66423,#66424,
#66425,#66426,#66427,#66428,#66429,#66430,#66431,#66432,#66433,#66434,#66435,
#66436,#66437,#66438,#66439,#66440,#66441,#66442,#66443,#66444,#66445,#66446,
#66447,#66448,#66449,#66450,#66451,#66452,#66453,#66454,#66455,#66456,#66457,
#66458,#66459),(#66460,#66461,#66462,#66463,#66464,#66465,#66466,#66467,
#66468,#66469,#66470,#66471,#66472,#66473,#66474,#66475,#66476,#66477,#66478,
#66479,#66480,#66481,#66482,#66483,#66484,#66485,#66486,#66487,#66488,#66489,
#66490,#66491,#66492,#66493,#66494,#66495,#66496,#66497,#66498,#66499,#66500,
#66501,#66502,#66503,#66504,#66505,#66506,#66507,#66508,#66509,#66510,#66511,
#66512,#66513,#66514,#66515,#66516,#66517,#66518,#66519,#66520,#66521,#66522,
#66523)),.UNSPECIFIED.,.F.,.F.,.F.,(4,4),(4,1,1,1,1,1,1,1,1,1,1,1,1,1,1,
1,1,1,1,1,1,1,1,1,1,1,1,1,1,1,1,1,1,1,1,1,1,1,1,1,1,1,1,1,1,1,1,1,1,1,1,
1,1,1,1,1,1,1,1,1,1,4),(-0.000173676366152087,0.0996748635808412),(0.308005718430657,
0.310256131102317,0.312455974418993,0.314655817735668,0.316855661052343,
0.319055504369019,0.321255347685694,0.323455191002369,0.325655034319044,
0.327610450600534,0.329565866882023,0.331521283163512,0.334454407585746,
0.337387532007979,0.340320656430213,0.343253780852447,0.343437101128836,
0.343620421405226,0.343987061958005,0.344353702510784,0.344720343063564,
0.346186905274681,0.349120029696914,0.352053154119148,0.354252997435823,
0.356452840752499,0.358652684069174,0.360852527385849,0.363052370702524,
0.3652522140192,0.367452057335875,0.36965190065255,0.371851743969226,0.374051587285901,
0.376251430602576,0.376801391431745,0.377351352260914,0.378451273919252,
0.381384398341485,0.384317522763719,0.387250647185953,0.390183771608187,
0.39311689603042,0.396050020452654,0.398983144874888,0.401916269297121,
0.404849393719355,0.406315955930472,0.407782518141589,0.409737934423078,
0.409982361458264,0.41022678849345,0.411693350704567,0.413648766986056,
0.415848610302732,0.418048453619407,0.420248296936082,0.422448140252758,
0.424647983569433,0.426847826886108,0.429047670202784,0.431421189885611),
 .UNSPECIFIED.);
#326=B_SPLINE_SURFACE_WITH_KNOTS('',3,3,((#66524,#66525,#66526,#66527,#66528,
#66529,#66530,#66531,#66532,#66533,#66534,#66535,#66536,#66537,#66538,#66539,
#66540,#66541,#66542,#66543,#66544,#66545,#66546,#66547,#66548,#66549,#66550,
#66551,#66552,#66553,#66554,#66555,#66556,#66557,#66558,#66559,#66560,#66561,
#66562,#66563,#66564,#66565,#66566,#66567,#66568,#66569,#66570,#66571,#66572,
#66573,#66574,#66575,#66576,#66577,#66578,#66579,#66580,#66581,#66582,#66583,
#66584,#66585),(#66586,#66587,#66588,#66589,#66590,#66591,#66592,#66593,
#66594,#66595,#66596,#66597,#66598,#66599,#66600,#66601,#66602,#66603,#66604,
#66605,#66606,#66607,#66608,#66609,#66610,#66611,#66612,#66613,#66614,#66615,
#66616,#66617,#66618,#66619,#66620,#66621,#66622,#66623,#66624,#66625,#66626,
#66627,#66628,#66629,#66630,#66631,#66632,#66633,#66634,#66635,#66636,#66637,
#66638,#66639,#66640,#66641,#66642,#66643,#66644,#66645,#66646,#66647),
(#66648,#66649,#66650,#66651,#66652,#66653,#66654,#66655,#66656,#66657,
#66658,#66659,#66660,#66661,#66662,#66663,#66664,#66665,#66666,#66667,#66668,
#66669,#66670,#66671,#66672,#66673,#66674,#66675,#66676,#66677,#66678,#66679,
#66680,#66681,#66682,#66683,#66684,#66685,#66686,#66687,#66688,#66689,#66690,
#66691,#66692,#66693,#66694,#66695,#66696,#66697,#66698,#66699,#66700,#66701,
#66702,#66703,#66704,#66705,#66706,#66707,#66708,#66709),(#66710,#66711,
#66712,#66713,#66714,#66715,#66716,#66717,#66718,#66719,#66720,#66721,#66722,
#66723,#66724,#66725,#66726,#66727,#66728,#66729,#66730,#66731,#66732,#66733,
#66734,#66735,#66736,#66737,#66738,#66739,#66740,#66741,#66742,#66743,#66744,
#66745,#66746,#66747,#66748,#66749,#66750,#66751,#66752,#66753,#66754,#66755,
#66756,#66757,#66758,#66759,#66760,#66761,#66762,#66763,#66764,#66765,#66766,
#66767,#66768,#66769,#66770,#66771)),.UNSPECIFIED.,.F.,.F.,.F.,(4,4),(4,
1,1,1,1,1,1,1,1,1,1,1,1,1,1,1,1,1,1,1,1,1,1,1,1,1,1,1,1,1,1,1,1,1,1,1,1,
1,1,1,1,1,1,1,1,1,1,1,1,1,1,1,1,1,1,1,1,1,1,4),(-0.000483778271071483,0.0996401519239673),
(0.476423916058673,0.478623759221241,0.480823602383808,0.483023445546375,
0.485223288708942,0.487423131871509,0.489622975034076,0.491822818196643,
0.49402266135921,0.495978077503714,0.497933493648219,0.499888909792723,
0.502822034009479,0.505755158226235,0.508688282442991,0.511621406659747,
0.514554530876503,0.51748765509326,0.518220936147449,0.518954217201638,
0.519687498255827,0.520420779310016,0.522620622472583,0.52482046563515,
0.527020308797717,0.529220151960284,0.531419995122852,0.533619838285419,
0.535819681447986,0.538019524610553,0.54021936777312,0.542419210935687,
0.544619054098254,0.546818897260821,0.549018740423388,0.551218583585956,
0.554151707802712,0.55561826991109,0.557818113073657,0.560017956236224,
0.562217799398791,0.564417642561358,0.566617485723925,0.568817328886493,
0.57101717204906,0.573217015211627,0.576150139428383,0.579083263645139,
0.582016387861895,0.583116309443179,0.583666270233821,0.584216231024462,
0.585316152605746,0.586416074187029,0.588615917349597,0.590815760512164,
0.593015603674731,0.595215446837298,0.597415289999865,0.599615133162432),
 .UNSPECIFIED.);
#327=B_SPLINE_SURFACE_WITH_KNOTS('',3,3,((#66772,#66773,#66774,#66775,#66776,
#66777,#66778,#66779,#66780,#66781,#66782,#66783,#66784,#66785,#66786,#66787,
#66788,#66789,#66790,#66791,#66792,#66793,#66794,#66795,#66796,#66797,#66798,
#66799,#66800,#66801,#66802,#66803,#66804,#66805,#66806,#66807,#66808,#66809,
#66810,#66811,#66812,#66813,#66814,#66815,#66816,#66817,#66818,#66819,#66820,
#66821,#66822,#66823,#66824,#66825,#66826,#66827,#66828),(#66829,#66830,
#66831,#66832,#66833,#66834,#66835,#66836,#66837,#66838,#66839,#66840,#66841,
#66842,#66843,#66844,#66845,#66846,#66847,#66848,#66849,#66850,#66851,#66852,
#66853,#66854,#66855,#66856,#66857,#66858,#66859,#66860,#66861,#66862,#66863,
#66864,#66865,#66866,#66867,#66868,#66869,#66870,#66871,#66872,#66873,#66874,
#66875,#66876,#66877,#66878,#66879,#66880,#66881,#66882,#66883,#66884,#66885),
(#66886,#66887,#66888,#66889,#66890,#66891,#66892,#66893,#66894,#66895,
#66896,#66897,#66898,#66899,#66900,#66901,#66902,#66903,#66904,#66905,#66906,
#66907,#66908,#66909,#66910,#66911,#66912,#66913,#66914,#66915,#66916,#66917,
#66918,#66919,#66920,#66921,#66922,#66923,#66924,#66925,#66926,#66927,#66928,
#66929,#66930,#66931,#66932,#66933,#66934,#66935,#66936,#66937,#66938,#66939,
#66940,#66941,#66942),(#66943,#66944,#66945,#66946,#66947,#66948,#66949,
#66950,#66951,#66952,#66953,#66954,#66955,#66956,#66957,#66958,#66959,#66960,
#66961,#66962,#66963,#66964,#66965,#66966,#66967,#66968,#66969,#66970,#66971,
#66972,#66973,#66974,#66975,#66976,#66977,#66978,#66979,#66980,#66981,#66982,
#66983,#66984,#66985,#66986,#66987,#66988,#66989,#66990,#66991,#66992,#66993,
#66994,#66995,#66996,#66997,#66998,#66999)),.UNSPECIFIED.,.F.,.F.,.F.,(4,
4),(4,1,1,1,1,1,1,1,1,1,1,1,1,1,1,1,1,1,1,1,1,1,1,1,1,1,1,1,1,1,1,1,1,1,
1,1,1,1,1,1,1,1,1,1,1,1,1,1,1,1,1,1,1,1,4),(-0.000295720647117127,0.0996668285717888),
(0.64474900998943,0.64699138736001,0.649191230384658,0.651391073409306,
0.653590916433954,0.655790759458603,0.657990602483251,0.660190445507899,
0.662390288532547,0.665323412565411,0.666789974581843,0.668256536598275,
0.67118966063114,0.674122784664004,0.677055908696868,0.679989032729732,
0.68218887575438,0.684388718779029,0.686588561803677,0.688788404828325,
0.690988247852973,0.693188090877621,0.695387933902269,0.697587776926917,
0.699787619951565,0.701987462976214,0.704187306000862,0.70638714902551,
0.708586992050158,0.710786835074806,0.712986678099454,0.715186521124103,
0.717386364148751,0.719586207173399,0.721052769189831,0.723985893222695,
0.726185736247343,0.728385579271991,0.730585422296639,0.732785265321288,
0.734985108345936,0.737184951370584,0.739384794395232,0.74158463741988,
0.744517761452744,0.747450885485609,0.750384009518473,0.752583852543121,
0.754783695567769,0.756983538592417,0.759183381617065,0.761383224641714,
0.763583067666362,0.76578291069101,0.768130417569294),.UNSPECIFIED.);
#328=B_SPLINE_SURFACE_WITH_KNOTS('',3,3,((#67000,#67001,#67002,#67003,#67004,
#67005,#67006,#67007,#67008,#67009,#67010,#67011,#67012,#67013,#67014,#67015,
#67016,#67017,#67018,#67019,#67020,#67021,#67022,#67023,#67024,#67025,#67026,
#67027,#67028,#67029,#67030,#67031,#67032,#67033,#67034,#67035,#67036,#67037,
#67038,#67039,#67040,#67041,#67042,#67043,#67044,#67045,#67046,#67047,#67048,
#67049,#67050,#67051,#67052,#67053,#67054,#67055,#67056,#67057,#67058,#67059,
#67060,#67061,#67062,#67063,#67064,#67065,#67066),(#67067,#67068,#67069,
#67070,#67071,#67072,#67073,#67074,#67075,#67076,#67077,#67078,#67079,#67080,
#67081,#67082,#67083,#67084,#67085,#67086,#67087,#67088,#67089,#67090,#67091,
#67092,#67093,#67094,#67095,#67096,#67097,#67098,#67099,#67100,#67101,#67102,
#67103,#67104,#67105,#67106,#67107,#67108,#67109,#67110,#67111,#67112,#67113,
#67114,#67115,#67116,#67117,#67118,#67119,#67120,#67121,#67122,#67123,#67124,
#67125,#67126,#67127,#67128,#67129,#67130,#67131,#67132,#67133),(#67134,
#67135,#67136,#67137,#67138,#67139,#67140,#67141,#67142,#67143,#67144,#67145,
#67146,#67147,#67148,#67149,#67150,#67151,#67152,#67153,#67154,#67155,#67156,
#67157,#67158,#67159,#67160,#67161,#67162,#67163,#67164,#67165,#67166,#67167,
#67168,#67169,#67170,#67171,#67172,#67173,#67174,#67175,#67176,#67177,#67178,
#67179,#67180,#67181,#67182,#67183,#67184,#67185,#67186,#67187,#67188,#67189,
#67190,#67191,#67192,#67193,#67194,#67195,#67196,#67197,#67198,#67199,#67200),
(#67201,#67202,#67203,#67204,#67205,#67206,#67207,#67208,#67209,#67210,
#67211,#67212,#67213,#67214,#67215,#67216,#67217,#67218,#67219,#67220,#67221,
#67222,#67223,#67224,#67225,#67226,#67227,#67228,#67229,#67230,#67231,#67232,
#67233,#67234,#67235,#67236,#67237,#67238,#67239,#67240,#67241,#67242,#67243,
#67244,#67245,#67246,#67247,#67248,#67249,#67250,#67251,#67252,#67253,#67254,
#67255,#67256,#67257,#67258,#67259,#67260,#67261,#67262,#67263,#67264,#67265,
#67266,#67267)),.UNSPECIFIED.,.F.,.F.,.F.,(4,4),(4,1,1,1,1,1,1,1,1,1,1,
1,1,1,1,1,1,1,1,1,1,1,1,1,1,1,1,1,1,1,1,1,1,1,1,1,1,1,1,1,1,1,1,1,1,1,1,
1,1,1,1,1,1,1,1,1,1,1,1,1,1,1,1,1,4),(-0.000370856902642016,0.0600414511958849),
(0.79017342904027,0.792057831484434,0.793901305088964,0.795744778693493,
0.797588252298022,0.799431725902551,0.800353462704815,0.801275199507079,
0.803118673111608,0.804962146716138,0.807420111522176,0.809878076328215,
0.812336041134254,0.814179514738783,0.816022988343312,0.817866461947841,
0.81970993555237,0.820631672354634,0.821553409156899,0.822475145959163,
0.823396882761428,0.825240356365957,0.827083829970486,0.828312812373505,
0.830770777179544,0.832614250784073,0.834457724388602,0.836301197993131,
0.83814467159766,0.839373654000679,0.841831618806718,0.842753355608982,
0.843675092411247,0.845518566015776,0.84644030281804,0.847362039620305,
0.849205513224834,0.851048986829363,0.852892460433892,0.854735934038421,
0.85657940764295,0.857808390045969,0.859037372448988,0.859651863650498,
0.860266354852008,0.861495337255027,0.862724319658047,0.863338810859556,
0.863953302061066,0.866411266867105,0.868869231673143,0.871327196479182,
0.872556178882201,0.873785161285221,0.875423804489247,0.877062447693272,
0.878701090897298,0.880544564501827,0.882388038106356,0.884231511710885,
0.886074985315414,0.887918458919943,0.889761932524472,0.891605406129001,
0.893665144683499),.UNSPECIFIED.);
#329=B_SPLINE_SURFACE_WITH_KNOTS('',3,3,((#67326,#67327,#67328,#67329,#67330,
#67331,#67332,#67333,#67334,#67335,#67336,#67337,#67338,#67339,#67340,#67341,
#67342,#67343,#67344,#67345,#67346,#67347,#67348,#67349,#67350,#67351,#67352,
#67353,#67354,#67355,#67356,#67357,#67358,#67359,#67360,#67361,#67362,#67363,
#67364,#67365,#67366,#67367,#67368,#67369,#67370,#67371,#67372,#67373,#67374,
#67375,#67376,#67377,#67378,#67379,#67380,#67381,#67382,#67383,#67384,#67385,
#67386,#67387,#67388,#67389,#67390,#67391,#67392,#67393,#67394,#67395,#67396,
#67397,#67398,#67399,#67400,#67401,#67402,#67403,#67404,#67405,#67406,#67407,
#67408,#67409,#67410,#67411,#67412,#67413),(#67414,#67415,#67416,#67417,
#67418,#67419,#67420,#67421,#67422,#67423,#67424,#67425,#67426,#67427,#67428,
#67429,#67430,#67431,#67432,#67433,#67434,#67435,#67436,#67437,#67438,#67439,
#67440,#67441,#67442,#67443,#67444,#67445,#67446,#67447,#67448,#67449,#67450,
#67451,#67452,#67453,#67454,#67455,#67456,#67457,#67458,#67459,#67460,#67461,
#67462,#67463,#67464,#67465,#67466,#67467,#67468,#67469,#67470,#67471,#67472,
#67473,#67474,#67475,#67476,#67477,#67478,#67479,#67480,#67481,#67482,#67483,
#67484,#67485,#67486,#67487,#67488,#67489,#67490,#67491,#67492,#67493,#67494,
#67495,#67496,#67497,#67498,#67499,#67500,#67501),(#67502,#67503,#67504,
#67505,#67506,#67507,#67508,#67509,#67510,#67511,#67512,#67513,#67514,#67515,
#67516,#67517,#67518,#67519,#67520,#67521,#67522,#67523,#67524,#67525,#67526,
#67527,#67528,#67529,#67530,#67531,#67532,#67533,#67534,#67535,#67536,#67537,
#67538,#67539,#67540,#67541,#67542,#67543,#67544,#67545,#67546,#67547,#67548,
#67549,#67550,#67551,#67552,#67553,#67554,#67555,#67556,#67557,#67558,#67559,
#67560,#67561,#67562,#67563,#67564,#67565,#67566,#67567,#67568,#67569,#67570,
#67571,#67572,#67573,#67574,#67575,#67576,#67577,#67578,#67579,#67580,#67581,
#67582,#67583,#67584,#67585,#67586,#67587,#67588,#67589),(#67590,#67591,
#67592,#67593,#67594,#67595,#67596,#67597,#67598,#67599,#67600,#67601,#67602,
#67603,#67604,#67605,#67606,#67607,#67608,#67609,#67610,#67611,#67612,#67613,
#67614,#67615,#67616,#67617,#67618,#67619,#67620,#67621,#67622,#67623,#67624,
#67625,#67626,#67627,#67628,#67629,#67630,#67631,#67632,#67633,#67634,#67635,
#67636,#67637,#67638,#67639,#67640,#67641,#67642,#67643,#67644,#67645,#67646,
#67647,#67648,#67649,#67650,#67651,#67652,#67653,#67654,#67655,#67656,#67657,
#67658,#67659,#67660,#67661,#67662,#67663,#67664,#67665,#67666,#67667,#67668,
#67669,#67670,#67671,#67672,#67673,#67674,#67675,#67676,#67677)),
 .UNSPECIFIED.,.F.,.F.,.F.,(4,4),(4,1,1,1,1,1,1,1,1,1,1,1,1,1,1,1,1,1,1,
1,1,1,1,1,1,1,1,1,1,1,1,1,1,1,1,1,1,1,1,1,1,1,1,1,1,1,1,1,1,1,1,1,1,1,1,
1,1,1,1,1,1,1,1,1,1,1,1,1,1,1,1,1,1,1,1,1,1,1,1,1,1,1,1,1,1,4),(-0.000543361608291823,
0.0996242942258564),(0.813159172043207,0.815359014876381,0.817558857709555,
0.819758700542729,0.821958543375904,0.824158386209078,0.826358229042252,
0.828558071875427,0.830757914708601,0.832224476597384,0.833691038486167,
0.83515760037495,0.835890881319341,0.836624162263733,0.837357443208124,
0.839557286041298,0.841757128874473,0.843956971707647,0.846156814540821,
0.848356657373996,0.85055650020717,0.852756343040344,0.853856264456931,
0.854956185873519,0.857156028706693,0.857889309651084,0.858622590595476,
0.859355871539867,0.860089152484259,0.86082243342865,0.861555714373042,
0.862655635789629,0.863755557206216,0.864855478622803,0.86595540003939,
0.868155242872565,0.870355085705739,0.871821647594522,0.874754771372088,
0.875854692788675,0.876954614205262,0.879154457038436,0.880254378455023,
0.880804339163317,0.881079319517464,0.881354299871611,0.883554142704785,
0.885753985537959,0.887953828371133,0.890153671204308,0.892353514037482,
0.89253683427358,0.892628494391629,0.892720154509678,0.893086794981873,
0.893820075926265,0.895286637815048,0.896753199703831,0.898219761592614,
0.898953042537005,0.899136362773103,0.899319683009201,0.899686323481397,
0.900052963953592,0.900419604425788,0.901152885370179,0.902619447258962,
0.904086009147745,0.905552571036528,0.907019132925311,0.908485694814094,
0.909952256702877,0.91141881859166,0.912885380480442,0.914840796332153,
0.916796212183863,0.917773920109719,0.918751628035574,0.920951470868748,
0.923151313701923,0.925351156535097,0.927550999368271,0.929750842201446,
0.93195068503462,0.934150527867794,0.936473459753071),.UNSPECIFIED.);
#330=B_SPLINE_SURFACE_WITH_KNOTS('',3,3,((#68645,#68646,#68647,#68648,#68649,
#68650,#68651,#68652,#68653,#68654,#68655,#68656,#68657,#68658,#68659,#68660,
#68661,#68662,#68663,#68664,#68665,#68666,#68667,#68668,#68669,#68670,#68671,
#68672,#68673,#68674,#68675,#68676,#68677,#68678,#68679,#68680,#68681,#68682,
#68683,#68684,#68685,#68686,#68687,#68688,#68689,#68690,#68691,#68692,#68693,
#68694,#68695,#68696,#68697,#68698,#68699,#68700,#68701,#68702,#68703,#68704,
#68705,#68706,#68707,#68708,#68709,#68710,#68711,#68712,#68713,#68714,#68715,
#68716,#68717,#68718,#68719,#68720,#68721,#68722,#68723,#68724,#68725,#68726,
#68727,#68728),(#68729,#68730,#68731,#68732,#68733,#68734,#68735,#68736,
#68737,#68738,#68739,#68740,#68741,#68742,#68743,#68744,#68745,#68746,#68747,
#68748,#68749,#68750,#68751,#68752,#68753,#68754,#68755,#68756,#68757,#68758,
#68759,#68760,#68761,#68762,#68763,#68764,#68765,#68766,#68767,#68768,#68769,
#68770,#68771,#68772,#68773,#68774,#68775,#68776,#68777,#68778,#68779,#68780,
#68781,#68782,#68783,#68784,#68785,#68786,#68787,#68788,#68789,#68790,#68791,
#68792,#68793,#68794,#68795,#68796,#68797,#68798,#68799,#68800,#68801,#68802,
#68803,#68804,#68805,#68806,#68807,#68808,#68809,#68810,#68811,#68812),
(#68813,#68814,#68815,#68816,#68817,#68818,#68819,#68820,#68821,#68822,
#68823,#68824,#68825,#68826,#68827,#68828,#68829,#68830,#68831,#68832,#68833,
#68834,#68835,#68836,#68837,#68838,#68839,#68840,#68841,#68842,#68843,#68844,
#68845,#68846,#68847,#68848,#68849,#68850,#68851,#68852,#68853,#68854,#68855,
#68856,#68857,#68858,#68859,#68860,#68861,#68862,#68863,#68864,#68865,#68866,
#68867,#68868,#68869,#68870,#68871,#68872,#68873,#68874,#68875,#68876,#68877,
#68878,#68879,#68880,#68881,#68882,#68883,#68884,#68885,#68886,#68887,#68888,
#68889,#68890,#68891,#68892,#68893,#68894,#68895,#68896),(#68897,#68898,
#68899,#68900,#68901,#68902,#68903,#68904,#68905,#68906,#68907,#68908,#68909,
#68910,#68911,#68912,#68913,#68914,#68915,#68916,#68917,#68918,#68919,#68920,
#68921,#68922,#68923,#68924,#68925,#68926,#68927,#68928,#68929,#68930,#68931,
#68932,#68933,#68934,#68935,#68936,#68937,#68938,#68939,#68940,#68941,#68942,
#68943,#68944,#68945,#68946,#68947,#68948,#68949,#68950,#68951,#68952,#68953,
#68954,#68955,#68956,#68957,#68958,#68959,#68960,#68961,#68962,#68963,#68964,
#68965,#68966,#68967,#68968,#68969,#68970,#68971,#68972,#68973,#68974,#68975,
#68976,#68977,#68978,#68979,#68980)),.UNSPECIFIED.,.F.,.F.,.F.,(4,4),(4,
1,1,1,1,1,1,1,1,1,1,1,1,1,1,1,1,1,1,1,1,1,1,1,1,1,1,1,1,1,1,1,1,1,1,1,1,
1,1,1,1,1,1,1,1,1,1,1,1,1,1,1,1,1,1,1,1,1,1,1,1,1,1,1,1,1,1,1,1,1,1,1,1,
1,1,1,1,1,1,1,1,4),(-0.000202954762976394,0.120064235496532),(0.85630617939849,
0.858856990877825,0.861344437291952,0.86383188370608,0.866319330120207,
0.868806776534335,0.871294222948462,0.872537946155526,0.87378166936259,
0.875025392569654,0.876269115776718,0.878480179255942,0.880691242735167,
0.882902306214391,0.886218901433228,0.889535496652065,0.891193794261483,
0.892852091870902,0.89451038948032,0.896168687089739,0.896997835894448,
0.897826984699157,0.899485282308575,0.900314431113284,0.901143579917994,
0.901558154320348,0.901972728722703,0.902801877527412,0.906118472746249,
0.906947621550958,0.907776770355667,0.909435067965086,0.91164613144431,
0.913857194923535,0.916068258402759,0.917173790142372,0.918279321881984,
0.920490385361208,0.922701448840433,0.924359746449851,0.92601804405927,
0.927676341668688,0.929334639278107,0.930163788082816,0.930992936887525,
0.931822085692234,0.932651234496943,0.933065808899298,0.933480383301653,
0.934309532106362,0.935138680911071,0.935553255313426,0.93596782971578,
0.939284424934617,0.942601020153454,0.945917615372291,0.949234210591127,
0.951445274070352,0.953656337549576,0.955867401028801,0.957525698638219,
0.959183996247638,0.960842293857056,0.962500591466475,0.964158889075893,
0.965817186685311,0.96747548429473,0.968304633099439,0.968719207501794,
0.969133781904148,0.972450377122985,0.974108674732403,0.975766972341822,
0.978254418755949,0.980741865170077,0.983229311584205,0.984473034791268,
0.985716757998332,0.98820420441246,0.990691650826587,0.993179097240715,
0.995869498417819),.UNSPECIFIED.);
#331=B_SPLINE_SURFACE_WITH_KNOTS('',2,1,((#69951,#69952),(#69953,#69954),
(#69955,#69956)),.UNSPECIFIED.,.F.,.F.,.F.,(3,3),(2,2),(0.,1.),(0.,0.0172800000000002),
 .UNSPECIFIED.);
#332=B_SPLINE_SURFACE_WITH_KNOTS('',2,1,((#69969,#69970),(#69971,#69972),
(#69973,#69974)),.UNSPECIFIED.,.F.,.F.,.F.,(3,3),(2,2),(0.,1.),(0.,0.0172800000000002),
 .UNSPECIFIED.);
#333=B_SPLINE_SURFACE_WITH_KNOTS('',2,1,((#69984,#69985),(#69986,#69987),
(#69988,#69989)),.UNSPECIFIED.,.F.,.F.,.F.,(3,3),(2,2),(0.,1.),(0.,0.0172800000000002),
 .UNSPECIFIED.);
#334=B_SPLINE_SURFACE_WITH_KNOTS('',2,1,((#69999,#70000),(#70001,#70002),
(#70003,#70004)),.UNSPECIFIED.,.F.,.F.,.F.,(3,3),(2,2),(0.,1.),(0.,0.0172800000000002),
 .UNSPECIFIED.);
#335=B_SPLINE_SURFACE_WITH_KNOTS('',2,1,((#70014,#70015),(#70016,#70017),
(#70018,#70019)),.UNSPECIFIED.,.F.,.F.,.F.,(3,3),(2,2),(0.,1.),(0.,0.0172800000000002),
 .UNSPECIFIED.);
#336=B_SPLINE_SURFACE_WITH_KNOTS('',2,1,((#70029,#70030),(#70031,#70032),
(#70033,#70034)),.UNSPECIFIED.,.F.,.F.,.F.,(3,3),(2,2),(0.,1.),(0.,0.0172800000000002),
 .UNSPECIFIED.);
#337=B_SPLINE_SURFACE_WITH_KNOTS('',2,1,((#70044,#70045),(#70046,#70047),
(#70048,#70049)),.UNSPECIFIED.,.F.,.F.,.F.,(3,3),(2,2),(0.,1.),(0.,0.0172800000000002),
 .UNSPECIFIED.);
#338=B_SPLINE_SURFACE_WITH_KNOTS('',2,1,((#70059,#70060),(#70061,#70062),
(#70063,#70064)),.UNSPECIFIED.,.F.,.F.,.F.,(3,3),(2,2),(0.,1.),(0.,0.0172800000000002),
 .UNSPECIFIED.);
#339=B_SPLINE_SURFACE_WITH_KNOTS('',2,1,((#70071,#70072),(#70073,#70074),
(#70075,#70076)),.UNSPECIFIED.,.F.,.F.,.F.,(3,3),(2,2),(0.,1.),(0.,0.0172800000000002),
 .UNSPECIFIED.);
#340=B_SPLINE_SURFACE_WITH_KNOTS('',2,1,((#70089,#70090),(#70091,#70092),
(#70093,#70094)),.UNSPECIFIED.,.F.,.F.,.F.,(3,3),(2,2),(0.,1.),(0.,0.0172800000000002),
 .UNSPECIFIED.);
#341=B_SPLINE_SURFACE_WITH_KNOTS('',2,1,((#70104,#70105),(#70106,#70107),
(#70108,#70109)),.UNSPECIFIED.,.F.,.F.,.F.,(3,3),(2,2),(0.,1.),(0.,0.0172800000000002),
 .UNSPECIFIED.);
#342=B_SPLINE_SURFACE_WITH_KNOTS('',2,1,((#70119,#70120),(#70121,#70122),
(#70123,#70124)),.UNSPECIFIED.,.F.,.F.,.F.,(3,3),(2,2),(0.,1.),(0.,0.0172800000000002),
 .UNSPECIFIED.);
#343=B_SPLINE_SURFACE_WITH_KNOTS('',2,1,((#70134,#70135),(#70136,#70137),
(#70138,#70139)),.UNSPECIFIED.,.F.,.F.,.F.,(3,3),(2,2),(0.,1.),(0.,0.0172800000000002),
 .UNSPECIFIED.);
#344=B_SPLINE_SURFACE_WITH_KNOTS('',2,1,((#70149,#70150),(#70151,#70152),
(#70153,#70154)),.UNSPECIFIED.,.F.,.F.,.F.,(3,3),(2,2),(0.,1.),(0.,0.0172800000000002),
 .UNSPECIFIED.);
#345=B_SPLINE_SURFACE_WITH_KNOTS('',2,1,((#70164,#70165),(#70166,#70167),
(#70168,#70169)),.UNSPECIFIED.,.F.,.F.,.F.,(3,3),(2,2),(0.,1.),(0.,0.0172800000000002),
 .UNSPECIFIED.);
#346=B_SPLINE_SURFACE_WITH_KNOTS('',2,1,((#70179,#70180),(#70181,#70182),
(#70183,#70184)),.UNSPECIFIED.,.F.,.F.,.F.,(3,3),(2,2),(0.,1.),(0.,0.0172800000000002),
 .UNSPECIFIED.);
#347=B_SPLINE_SURFACE_WITH_KNOTS('',2,1,((#70194,#70195),(#70196,#70197),
(#70198,#70199)),.UNSPECIFIED.,.F.,.F.,.F.,(3,3),(2,2),(0.,1.),(0.,0.0172800000000002),
 .UNSPECIFIED.);
#348=B_SPLINE_SURFACE_WITH_KNOTS('',2,1,((#70209,#70210),(#70211,#70212),
(#70213,#70214)),.UNSPECIFIED.,.F.,.F.,.F.,(3,3),(2,2),(0.,1.),(0.,0.0172800000000002),
 .UNSPECIFIED.);
#349=B_SPLINE_SURFACE_WITH_KNOTS('',2,1,((#70224,#70225),(#70226,#70227),
(#70228,#70229)),.UNSPECIFIED.,.F.,.F.,.F.,(3,3),(2,2),(0.,1.),(0.,0.0172800000000002),
 .UNSPECIFIED.);
#350=B_SPLINE_SURFACE_WITH_KNOTS('',2,1,((#70239,#70240),(#70241,#70242),
(#70243,#70244)),.UNSPECIFIED.,.F.,.F.,.F.,(3,3),(2,2),(0.,1.),(0.,0.0172800000000002),
 .UNSPECIFIED.);
#351=B_SPLINE_SURFACE_WITH_KNOTS('',2,1,((#70339,#70340),(#70341,#70342),
(#70343,#70344)),.UNSPECIFIED.,.F.,.F.,.F.,(3,3),(2,2),(0.,1.),(0.,0.0172800000000002),
 .UNSPECIFIED.);
#352=B_SPLINE_SURFACE_WITH_KNOTS('',2,1,((#70357,#70358),(#70359,#70360),
(#70361,#70362)),.UNSPECIFIED.,.F.,.F.,.F.,(3,3),(2,2),(0.,1.),(0.,0.0172800000000002),
 .UNSPECIFIED.);
#353=B_SPLINE_SURFACE_WITH_KNOTS('',2,1,((#70372,#70373),(#70374,#70375),
(#70376,#70377)),.UNSPECIFIED.,.F.,.F.,.F.,(3,3),(2,2),(0.,1.),(0.,0.0172800000000002),
 .UNSPECIFIED.);
#354=B_SPLINE_SURFACE_WITH_KNOTS('',2,1,((#70387,#70388),(#70389,#70390),
(#70391,#70392)),.UNSPECIFIED.,.F.,.F.,.F.,(3,3),(2,2),(0.,1.),(0.,0.0172800000000002),
 .UNSPECIFIED.);
#355=B_SPLINE_SURFACE_WITH_KNOTS('',2,1,((#70402,#70403),(#70404,#70405),
(#70406,#70407)),.UNSPECIFIED.,.F.,.F.,.F.,(3,3),(2,2),(0.,1.),(0.,0.0172800000000002),
 .UNSPECIFIED.);
#356=B_SPLINE_SURFACE_WITH_KNOTS('',2,1,((#70417,#70418),(#70419,#70420),
(#70421,#70422)),.UNSPECIFIED.,.F.,.F.,.F.,(3,3),(2,2),(0.,1.),(0.,0.0172800000000002),
 .UNSPECIFIED.);
#357=B_SPLINE_SURFACE_WITH_KNOTS('',2,1,((#70432,#70433),(#70434,#70435),
(#70436,#70437)),.UNSPECIFIED.,.F.,.F.,.F.,(3,3),(2,2),(0.,1.),(0.,0.0172800000000002),
 .UNSPECIFIED.);
#358=B_SPLINE_SURFACE_WITH_KNOTS('',2,1,((#70447,#70448),(#70449,#70450),
(#70451,#70452)),.UNSPECIFIED.,.F.,.F.,.F.,(3,3),(2,2),(0.,1.),(0.,0.0172800000000002),
 .UNSPECIFIED.);
#359=B_SPLINE_SURFACE_WITH_KNOTS('',2,1,((#70459,#70460),(#70461,#70462),
(#70463,#70464)),.UNSPECIFIED.,.F.,.F.,.F.,(3,3),(2,2),(0.,1.),(0.,0.0172800000000002),
 .UNSPECIFIED.);
#360=B_SPLINE_SURFACE_WITH_KNOTS('',2,1,((#70477,#70478),(#70479,#70480),
(#70481,#70482)),.UNSPECIFIED.,.F.,.F.,.F.,(3,3),(2,2),(0.,1.),(0.,0.0172800000000002),
 .UNSPECIFIED.);
#361=B_SPLINE_SURFACE_WITH_KNOTS('',2,1,((#70492,#70493),(#70494,#70495),
(#70496,#70497)),.UNSPECIFIED.,.F.,.F.,.F.,(3,3),(2,2),(0.,1.),(0.,0.0172800000000002),
 .UNSPECIFIED.);
#362=B_SPLINE_SURFACE_WITH_KNOTS('',2,1,((#70507,#70508),(#70509,#70510),
(#70511,#70512)),.UNSPECIFIED.,.F.,.F.,.F.,(3,3),(2,2),(0.,1.),(0.,0.0172800000000002),
 .UNSPECIFIED.);
#363=B_SPLINE_SURFACE_WITH_KNOTS('',2,1,((#70522,#70523),(#70524,#70525),
(#70526,#70527)),.UNSPECIFIED.,.F.,.F.,.F.,(3,3),(2,2),(0.,1.),(0.,0.0172800000000002),
 .UNSPECIFIED.);
#364=B_SPLINE_SURFACE_WITH_KNOTS('',2,1,((#70537,#70538),(#70539,#70540),
(#70541,#70542)),.UNSPECIFIED.,.F.,.F.,.F.,(3,3),(2,2),(0.,1.),(0.,0.0172800000000002),
 .UNSPECIFIED.);
#365=B_SPLINE_SURFACE_WITH_KNOTS('',2,1,((#70552,#70553),(#70554,#70555),
(#70556,#70557)),.UNSPECIFIED.,.F.,.F.,.F.,(3,3),(2,2),(0.,1.),(0.,0.0172800000000002),
 .UNSPECIFIED.);
#366=B_SPLINE_SURFACE_WITH_KNOTS('',2,1,((#70567,#70568),(#70569,#70570),
(#70571,#70572)),.UNSPECIFIED.,.F.,.F.,.F.,(3,3),(2,2),(0.,1.),(0.,0.0172800000000002),
 .UNSPECIFIED.);
#367=B_SPLINE_SURFACE_WITH_KNOTS('',2,1,((#70582,#70583),(#70584,#70585),
(#70586,#70587)),.UNSPECIFIED.,.F.,.F.,.F.,(3,3),(2,2),(0.,1.),(0.,0.0172800000000002),
 .UNSPECIFIED.);
#368=B_SPLINE_SURFACE_WITH_KNOTS('',2,1,((#70597,#70598),(#70599,#70600),
(#70601,#70602)),.UNSPECIFIED.,.F.,.F.,.F.,(3,3),(2,2),(0.,1.),(0.,0.0172800000000002),
 .UNSPECIFIED.);
#369=B_SPLINE_SURFACE_WITH_KNOTS('',2,1,((#70612,#70613),(#70614,#70615),
(#70616,#70617)),.UNSPECIFIED.,.F.,.F.,.F.,(3,3),(2,2),(0.,1.),(0.,0.0172800000000002),
 .UNSPECIFIED.);
#370=B_SPLINE_SURFACE_WITH_KNOTS('',2,1,((#70627,#70628),(#70629,#70630),
(#70631,#70632)),.UNSPECIFIED.,.F.,.F.,.F.,(3,3),(2,2),(0.,1.),(0.,0.0172800000000002),
 .UNSPECIFIED.);
#371=B_SPLINE_SURFACE_WITH_KNOTS('',2,1,((#70640,#70641),(#70642,#70643),
(#70644,#70645)),.UNSPECIFIED.,.F.,.F.,.F.,(3,3),(2,2),(0.,1.),(0.,0.0172800000000002),
 .UNSPECIFIED.);
#372=B_SPLINE_SURFACE_WITH_KNOTS('',2,1,((#70658,#70659),(#70660,#70661),
(#70662,#70663)),.UNSPECIFIED.,.F.,.F.,.F.,(3,3),(2,2),(0.,1.),(0.,0.0172800000000002),
 .UNSPECIFIED.);
#373=B_SPLINE_SURFACE_WITH_KNOTS('',2,1,((#70673,#70674),(#70675,#70676),
(#70677,#70678)),.UNSPECIFIED.,.F.,.F.,.F.,(3,3),(2,2),(0.,1.),(0.,0.0172800000000002),
 .UNSPECIFIED.);
#374=B_SPLINE_SURFACE_WITH_KNOTS('',2,1,((#70688,#70689),(#70690,#70691),
(#70692,#70693)),.UNSPECIFIED.,.F.,.F.,.F.,(3,3),(2,2),(0.,1.),(0.,0.0172800000000002),
 .UNSPECIFIED.);
#375=B_SPLINE_SURFACE_WITH_KNOTS('',2,1,((#70703,#70704),(#70705,#70706),
(#70707,#70708)),.UNSPECIFIED.,.F.,.F.,.F.,(3,3),(2,2),(0.,1.),(0.,0.0172800000000002),
 .UNSPECIFIED.);
#376=B_SPLINE_SURFACE_WITH_KNOTS('',2,1,((#70718,#70719),(#70720,#70721),
(#70722,#70723)),.UNSPECIFIED.,.F.,.F.,.F.,(3,3),(2,2),(0.,1.),(0.,0.0172800000000002),
 .UNSPECIFIED.);
#377=B_SPLINE_SURFACE_WITH_KNOTS('',2,1,((#70733,#70734),(#70735,#70736),
(#70737,#70738)),.UNSPECIFIED.,.F.,.F.,.F.,(3,3),(2,2),(0.,1.),(0.,0.0172800000000002),
 .UNSPECIFIED.);
#378=B_SPLINE_SURFACE_WITH_KNOTS('',2,1,((#70748,#70749),(#70750,#70751),
(#70752,#70753)),.UNSPECIFIED.,.F.,.F.,.F.,(3,3),(2,2),(0.,1.),(0.,0.0172800000000002),
 .UNSPECIFIED.);
#379=B_SPLINE_SURFACE_WITH_KNOTS('',2,1,((#70763,#70764),(#70765,#70766),
(#70767,#70768)),.UNSPECIFIED.,.F.,.F.,.F.,(3,3),(2,2),(0.,1.),(0.,0.0172800000000002),
 .UNSPECIFIED.);
#380=B_SPLINE_SURFACE_WITH_KNOTS('',2,1,((#70778,#70779),(#70780,#70781),
(#70782,#70783)),.UNSPECIFIED.,.F.,.F.,.F.,(3,3),(2,2),(0.,1.),(0.,0.0172800000000002),
 .UNSPECIFIED.);
#381=B_SPLINE_SURFACE_WITH_KNOTS('',2,1,((#70793,#70794),(#70795,#70796),
(#70797,#70798)),.UNSPECIFIED.,.F.,.F.,.F.,(3,3),(2,2),(0.,1.),(0.,0.0172800000000002),
 .UNSPECIFIED.);
#382=B_SPLINE_SURFACE_WITH_KNOTS('',2,1,((#70808,#70809),(#70810,#70811),
(#70812,#70813)),.UNSPECIFIED.,.F.,.F.,.F.,(3,3),(2,2),(0.,1.),(0.,0.0172800000000002),
 .UNSPECIFIED.);
#383=B_SPLINE_SURFACE_WITH_KNOTS('',2,1,((#70829,#70830),(#70831,#70832),
(#70833,#70834)),.UNSPECIFIED.,.F.,.F.,.F.,(3,3),(2,2),(0.,1.),(0.,0.0172800000000002),
 .UNSPECIFIED.);
#384=B_SPLINE_SURFACE_WITH_KNOTS('',2,1,((#70844,#70845),(#70846,#70847),
(#70848,#70849)),.UNSPECIFIED.,.F.,.F.,.F.,(3,3),(2,2),(0.,1.),(0.,0.0172800000000002),
 .UNSPECIFIED.);
#385=B_SPLINE_SURFACE_WITH_KNOTS('',2,1,((#70859,#70860),(#70861,#70862),
(#70863,#70864)),.UNSPECIFIED.,.F.,.F.,.F.,(3,3),(2,2),(0.,1.),(0.,0.0172800000000002),
 .UNSPECIFIED.);
#386=B_SPLINE_SURFACE_WITH_KNOTS('',2,1,((#70874,#70875),(#70876,#70877),
(#70878,#70879)),.UNSPECIFIED.,.F.,.F.,.F.,(3,3),(2,2),(0.,1.),(0.,0.0172800000000002),
 .UNSPECIFIED.);
#387=B_SPLINE_SURFACE_WITH_KNOTS('',2,1,((#70889,#70890),(#70891,#70892),
(#70893,#70894)),.UNSPECIFIED.,.F.,.F.,.F.,(3,3),(2,2),(0.,1.),(0.,0.0172800000000002),
 .UNSPECIFIED.);
#388=B_SPLINE_SURFACE_WITH_KNOTS('',2,1,((#70904,#70905),(#70906,#70907),
(#70908,#70909)),.UNSPECIFIED.,.F.,.F.,.F.,(3,3),(2,2),(0.,1.),(0.,0.0172800000000002),
 .UNSPECIFIED.);
#389=B_SPLINE_SURFACE_WITH_KNOTS('',2,1,((#70919,#70920),(#70921,#70922),
(#70923,#70924)),.UNSPECIFIED.,.F.,.F.,.F.,(3,3),(2,2),(0.,1.),(0.,0.0172800000000002),
 .UNSPECIFIED.);
#390=B_SPLINE_SURFACE_WITH_KNOTS('',2,1,((#70940,#70941),(#70942,#70943),
(#70944,#70945)),.UNSPECIFIED.,.F.,.F.,.F.,(3,3),(2,2),(0.,1.),(0.,0.0172800000000002),
 .UNSPECIFIED.);
#391=B_SPLINE_SURFACE_WITH_KNOTS('',2,1,((#70955,#70956),(#70957,#70958),
(#70959,#70960)),.UNSPECIFIED.,.F.,.F.,.F.,(3,3),(2,2),(0.,1.),(0.,0.0172800000000002),
 .UNSPECIFIED.);
#392=B_SPLINE_SURFACE_WITH_KNOTS('',2,1,((#70970,#70971),(#70972,#70973),
(#70974,#70975)),.UNSPECIFIED.,.F.,.F.,.F.,(3,3),(2,2),(0.,1.),(0.,0.0172800000000002),
 .UNSPECIFIED.);
#393=B_SPLINE_SURFACE_WITH_KNOTS('',2,1,((#70985,#70986),(#70987,#70988),
(#70989,#70990)),.UNSPECIFIED.,.F.,.F.,.F.,(3,3),(2,2),(0.,1.),(0.,0.0172800000000002),
 .UNSPECIFIED.);
#394=B_SPLINE_SURFACE_WITH_KNOTS('',2,1,((#71000,#71001),(#71002,#71003),
(#71004,#71005)),.UNSPECIFIED.,.F.,.F.,.F.,(3,3),(2,2),(0.,1.),(0.,0.0172800000000002),
 .UNSPECIFIED.);
#395=B_SPLINE_SURFACE_WITH_KNOTS('',2,1,((#71015,#71016),(#71017,#71018),
(#71019,#71020)),.UNSPECIFIED.,.F.,.F.,.F.,(3,3),(2,2),(0.,1.),(0.,0.0172800000000002),
 .UNSPECIFIED.);
#396=B_SPLINE_SURFACE_WITH_KNOTS('',2,1,((#71030,#71031),(#71032,#71033),
(#71034,#71035)),.UNSPECIFIED.,.F.,.F.,.F.,(3,3),(2,2),(0.,1.),(0.,0.0172800000000002),
 .UNSPECIFIED.);
#397=B_SPLINE_SURFACE_WITH_KNOTS('',2,1,((#71051,#71052),(#71053,#71054),
(#71055,#71056)),.UNSPECIFIED.,.F.,.F.,.F.,(3,3),(2,2),(0.,1.),(0.,0.0172800000000002),
 .UNSPECIFIED.);
#398=B_SPLINE_SURFACE_WITH_KNOTS('',2,1,((#71065,#71066),(#71067,#71068),
(#71069,#71070)),.UNSPECIFIED.,.F.,.F.,.F.,(3,3),(2,2),(0.,1.),(0.,0.0172800000000002),
 .UNSPECIFIED.);
#399=B_SPLINE_SURFACE_WITH_KNOTS('',2,1,((#71083,#71084),(#71085,#71086),
(#71087,#71088)),.UNSPECIFIED.,.F.,.F.,.F.,(3,3),(2,2),(0.,1.),(0.,0.0172800000000002),
 .UNSPECIFIED.);
#400=B_SPLINE_SURFACE_WITH_KNOTS('',2,1,((#71098,#71099),(#71100,#71101),
(#71102,#71103)),.UNSPECIFIED.,.F.,.F.,.F.,(3,3),(2,2),(0.,1.),(0.,0.0172800000000002),
 .UNSPECIFIED.);
#401=B_SPLINE_SURFACE_WITH_KNOTS('',2,1,((#71113,#71114),(#71115,#71116),
(#71117,#71118)),.UNSPECIFIED.,.F.,.F.,.F.,(3,3),(2,2),(0.,1.),(0.,0.0172800000000002),
 .UNSPECIFIED.);
#402=B_SPLINE_SURFACE_WITH_KNOTS('',2,1,((#71128,#71129),(#71130,#71131),
(#71132,#71133)),.UNSPECIFIED.,.F.,.F.,.F.,(3,3),(2,2),(0.,1.),(0.,0.0172800000000002),
 .UNSPECIFIED.);
#403=B_SPLINE_SURFACE_WITH_KNOTS('',2,1,((#71143,#71144),(#71145,#71146),
(#71147,#71148)),.UNSPECIFIED.,.F.,.F.,.F.,(3,3),(2,2),(0.,1.),(0.,0.0172800000000002),
 .UNSPECIFIED.);
#404=B_SPLINE_SURFACE_WITH_KNOTS('',2,1,((#71158,#71159),(#71160,#71161),
(#71162,#71163)),.UNSPECIFIED.,.F.,.F.,.F.,(3,3),(2,2),(0.,1.),(0.,0.0172800000000002),
 .UNSPECIFIED.);
#405=B_SPLINE_SURFACE_WITH_KNOTS('',2,1,((#71173,#71174),(#71175,#71176),
(#71177,#71178)),.UNSPECIFIED.,.F.,.F.,.F.,(3,3),(2,2),(0.,1.),(0.,0.0172800000000002),
 .UNSPECIFIED.);
#406=B_SPLINE_SURFACE_WITH_KNOTS('',2,1,((#71185,#71186),(#71187,#71188),
(#71189,#71190)),.UNSPECIFIED.,.F.,.F.,.F.,(3,3),(2,2),(0.,1.),(0.,0.0172800000000002),
 .UNSPECIFIED.);
#407=B_SPLINE_SURFACE_WITH_KNOTS('',2,1,((#71203,#71204),(#71205,#71206),
(#71207,#71208)),.UNSPECIFIED.,.F.,.F.,.F.,(3,3),(2,2),(0.,1.),(0.,0.0172800000000002),
 .UNSPECIFIED.);
#408=B_SPLINE_SURFACE_WITH_KNOTS('',2,1,((#71218,#71219),(#71220,#71221),
(#71222,#71223)),.UNSPECIFIED.,.F.,.F.,.F.,(3,3),(2,2),(0.,1.),(0.,0.0172800000000002),
 .UNSPECIFIED.);
#409=B_SPLINE_SURFACE_WITH_KNOTS('',2,1,((#71233,#71234),(#71235,#71236),
(#71237,#71238)),.UNSPECIFIED.,.F.,.F.,.F.,(3,3),(2,2),(0.,1.),(0.,0.0172800000000002),
 .UNSPECIFIED.);
#410=B_SPLINE_SURFACE_WITH_KNOTS('',2,1,((#71248,#71249),(#71250,#71251),
(#71252,#71253)),.UNSPECIFIED.,.F.,.F.,.F.,(3,3),(2,2),(0.,1.),(0.,0.0172800000000002),
 .UNSPECIFIED.);
#411=B_SPLINE_SURFACE_WITH_KNOTS('',2,1,((#71263,#71264),(#71265,#71266),
(#71267,#71268)),.UNSPECIFIED.,.F.,.F.,.F.,(3,3),(2,2),(0.,1.),(0.,0.0172800000000002),
 .UNSPECIFIED.);
#412=B_SPLINE_SURFACE_WITH_KNOTS('',2,1,((#71278,#71279),(#71280,#71281),
(#71282,#71283)),.UNSPECIFIED.,.F.,.F.,.F.,(3,3),(2,2),(0.,1.),(0.,0.0172800000000002),
 .UNSPECIFIED.);
#413=B_SPLINE_SURFACE_WITH_KNOTS('',2,1,((#71293,#71294),(#71295,#71296),
(#71297,#71298)),.UNSPECIFIED.,.F.,.F.,.F.,(3,3),(2,2),(0.,1.),(0.,0.0172800000000002),
 .UNSPECIFIED.);
#414=B_SPLINE_SURFACE_WITH_KNOTS('',2,1,((#71308,#71309),(#71310,#71311),
(#71312,#71313)),.UNSPECIFIED.,.F.,.F.,.F.,(3,3),(2,2),(0.,1.),(0.,0.0172800000000002),
 .UNSPECIFIED.);
#415=B_SPLINE_SURFACE_WITH_KNOTS('',2,1,((#71323,#71324),(#71325,#71326),
(#71327,#71328)),.UNSPECIFIED.,.F.,.F.,.F.,(3,3),(2,2),(0.,1.),(0.,0.0172800000000002),
 .UNSPECIFIED.);
#416=B_SPLINE_SURFACE_WITH_KNOTS('',2,1,((#71338,#71339),(#71340,#71341),
(#71342,#71343)),.UNSPECIFIED.,.F.,.F.,.F.,(3,3),(2,2),(0.,1.),(0.,0.0172800000000002),
 .UNSPECIFIED.);
#417=B_SPLINE_SURFACE_WITH_KNOTS('',2,1,((#71353,#71354),(#71355,#71356),
(#71357,#71358)),.UNSPECIFIED.,.F.,.F.,.F.,(3,3),(2,2),(0.,1.),(0.,0.0172800000000002),
 .UNSPECIFIED.);
#418=B_SPLINE_SURFACE_WITH_KNOTS('',2,1,((#71366,#71367),(#71368,#71369),
(#71370,#71371)),.UNSPECIFIED.,.F.,.F.,.F.,(3,3),(2,2),(0.,1.),(0.,0.0172800000000002),
 .UNSPECIFIED.);
#419=B_SPLINE_SURFACE_WITH_KNOTS('',2,1,((#71384,#71385),(#71386,#71387),
(#71388,#71389)),.UNSPECIFIED.,.F.,.F.,.F.,(3,3),(2,2),(0.,1.),(0.,0.0172800000000002),
 .UNSPECIFIED.);
#420=B_SPLINE_SURFACE_WITH_KNOTS('',2,1,((#71399,#71400),(#71401,#71402),
(#71403,#71404)),.UNSPECIFIED.,.F.,.F.,.F.,(3,3),(2,2),(0.,1.),(0.,0.0172800000000002),
 .UNSPECIFIED.);
#421=B_SPLINE_SURFACE_WITH_KNOTS('',2,1,((#71414,#71415),(#71416,#71417),
(#71418,#71419)),.UNSPECIFIED.,.F.,.F.,.F.,(3,3),(2,2),(0.,1.),(0.,0.0172800000000002),
 .UNSPECIFIED.);
#422=B_SPLINE_SURFACE_WITH_KNOTS('',2,1,((#71429,#71430),(#71431,#71432),
(#71433,#71434)),.UNSPECIFIED.,.F.,.F.,.F.,(3,3),(2,2),(0.,1.),(0.,0.0172800000000002),
 .UNSPECIFIED.);
#423=B_SPLINE_SURFACE_WITH_KNOTS('',2,1,((#71444,#71445),(#71446,#71447),
(#71448,#71449)),.UNSPECIFIED.,.F.,.F.,.F.,(3,3),(2,2),(0.,1.),(0.,0.0172800000000002),
 .UNSPECIFIED.);
#424=B_SPLINE_SURFACE_WITH_KNOTS('',2,1,((#71459,#71460),(#71461,#71462),
(#71463,#71464)),.UNSPECIFIED.,.F.,.F.,.F.,(3,3),(2,2),(0.,1.),(0.,0.0172800000000002),
 .UNSPECIFIED.);
#425=B_SPLINE_SURFACE_WITH_KNOTS('',2,1,((#71474,#71475),(#71476,#71477),
(#71478,#71479)),.UNSPECIFIED.,.F.,.F.,.F.,(3,3),(2,2),(0.,1.),(0.,0.0172800000000002),
 .UNSPECIFIED.);
#426=B_SPLINE_SURFACE_WITH_KNOTS('',2,1,((#71489,#71490),(#71491,#71492),
(#71493,#71494)),.UNSPECIFIED.,.F.,.F.,.F.,(3,3),(2,2),(0.,1.),(0.,0.0172800000000002),
 .UNSPECIFIED.);
#427=B_SPLINE_SURFACE_WITH_KNOTS('',2,1,((#71510,#71511),(#71512,#71513),
(#71514,#71515)),.UNSPECIFIED.,.F.,.F.,.F.,(3,3),(2,2),(0.,1.),(0.,0.0172800000000002),
 .UNSPECIFIED.);
#428=B_SPLINE_SURFACE_WITH_KNOTS('',2,1,((#71525,#71526),(#71527,#71528),
(#71529,#71530)),.UNSPECIFIED.,.F.,.F.,.F.,(3,3),(2,2),(0.,1.),(0.,0.0172800000000002),
 .UNSPECIFIED.);
#429=B_SPLINE_SURFACE_WITH_KNOTS('',2,1,((#71540,#71541),(#71542,#71543),
(#71544,#71545)),.UNSPECIFIED.,.F.,.F.,.F.,(3,3),(2,2),(0.,1.),(0.,0.0172800000000002),
 .UNSPECIFIED.);
#430=B_SPLINE_SURFACE_WITH_KNOTS('',2,1,((#71555,#71556),(#71557,#71558),
(#71559,#71560)),.UNSPECIFIED.,.F.,.F.,.F.,(3,3),(2,2),(0.,1.),(0.,0.0172800000000002),
 .UNSPECIFIED.);
#431=B_SPLINE_SURFACE_WITH_KNOTS('',2,1,((#71570,#71571),(#71572,#71573),
(#71574,#71575)),.UNSPECIFIED.,.F.,.F.,.F.,(3,3),(2,2),(0.,1.),(0.,0.0172800000000002),
 .UNSPECIFIED.);
#432=B_SPLINE_SURFACE_WITH_KNOTS('',2,1,((#71585,#71586),(#71587,#71588),
(#71589,#71590)),.UNSPECIFIED.,.F.,.F.,.F.,(3,3),(2,2),(0.,1.),(0.,0.0172800000000002),
 .UNSPECIFIED.);
#433=B_SPLINE_SURFACE_WITH_KNOTS('',2,1,((#71600,#71601),(#71602,#71603),
(#71604,#71605)),.UNSPECIFIED.,.F.,.F.,.F.,(3,3),(2,2),(0.,1.),(0.,0.0172800000000002),
 .UNSPECIFIED.);
#434=B_SPLINE_SURFACE_WITH_KNOTS('',2,1,((#71615,#71616),(#71617,#71618),
(#71619,#71620)),.UNSPECIFIED.,.F.,.F.,.F.,(3,3),(2,2),(0.,1.),(0.,0.0172800000000002),
 .UNSPECIFIED.);
#435=B_SPLINE_SURFACE_WITH_KNOTS('',2,1,((#71630,#71631),(#71632,#71633),
(#71634,#71635)),.UNSPECIFIED.,.F.,.F.,.F.,(3,3),(2,2),(0.,1.),(0.,0.0172800000000002),
 .UNSPECIFIED.);
#436=B_SPLINE_SURFACE_WITH_KNOTS('',2,1,((#71662,#71663),(#71664,#71665),
(#71666,#71667)),.UNSPECIFIED.,.F.,.F.,.F.,(3,3),(2,2),(0.,1.),(0.,0.0172800000000002),
 .UNSPECIFIED.);
#437=B_SPLINE_SURFACE_WITH_KNOTS('',2,1,((#71680,#71681),(#71682,#71683),
(#71684,#71685)),.UNSPECIFIED.,.F.,.F.,.F.,(3,3),(2,2),(0.,1.),(0.,0.0172800000000002),
 .UNSPECIFIED.);
#438=B_SPLINE_SURFACE_WITH_KNOTS('',2,1,((#71695,#71696),(#71697,#71698),
(#71699,#71700)),.UNSPECIFIED.,.F.,.F.,.F.,(3,3),(2,2),(0.,1.),(0.,0.0172800000000002),
 .UNSPECIFIED.);
#439=B_SPLINE_SURFACE_WITH_KNOTS('',2,1,((#71710,#71711),(#71712,#71713),
(#71714,#71715)),.UNSPECIFIED.,.F.,.F.,.F.,(3,3),(2,2),(0.,1.),(0.,0.0172800000000002),
 .UNSPECIFIED.);
#440=B_SPLINE_SURFACE_WITH_KNOTS('',2,1,((#71725,#71726),(#71727,#71728),
(#71729,#71730)),.UNSPECIFIED.,.F.,.F.,.F.,(3,3),(2,2),(0.,1.),(0.,0.0172800000000002),
 .UNSPECIFIED.);
#441=B_SPLINE_SURFACE_WITH_KNOTS('',2,1,((#71740,#71741),(#71742,#71743),
(#71744,#71745)),.UNSPECIFIED.,.F.,.F.,.F.,(3,3),(2,2),(0.,1.),(0.,0.0172800000000002),
 .UNSPECIFIED.);
#442=B_SPLINE_SURFACE_WITH_KNOTS('',2,1,((#71755,#71756),(#71757,#71758),
(#71759,#71760)),.UNSPECIFIED.,.F.,.F.,.F.,(3,3),(2,2),(0.,1.),(0.,0.0172800000000002),
 .UNSPECIFIED.);
#443=B_SPLINE_SURFACE_WITH_KNOTS('',2,1,((#71770,#71771),(#71772,#71773),
(#71774,#71775)),.UNSPECIFIED.,.F.,.F.,.F.,(3,3),(2,2),(0.,1.),(0.,0.0172800000000002),
 .UNSPECIFIED.);
#444=B_SPLINE_SURFACE_WITH_KNOTS('',2,1,((#71782,#71783),(#71784,#71785),
(#71786,#71787)),.UNSPECIFIED.,.F.,.F.,.F.,(3,3),(2,2),(0.,1.),(0.,0.0172800000000002),
 .UNSPECIFIED.);
#445=B_SPLINE_SURFACE_WITH_KNOTS('',2,1,((#71800,#71801),(#71802,#71803),
(#71804,#71805)),.UNSPECIFIED.,.F.,.F.,.F.,(3,3),(2,2),(0.,1.),(0.,0.0172800000000002),
 .UNSPECIFIED.);
#446=B_SPLINE_SURFACE_WITH_KNOTS('',2,1,((#71815,#71816),(#71817,#71818),
(#71819,#71820)),.UNSPECIFIED.,.F.,.F.,.F.,(3,3),(2,2),(0.,1.),(0.,0.0172800000000002),
 .UNSPECIFIED.);
#447=B_SPLINE_SURFACE_WITH_KNOTS('',2,1,((#71830,#71831),(#71832,#71833),
(#71834,#71835)),.UNSPECIFIED.,.F.,.F.,.F.,(3,3),(2,2),(0.,1.),(0.,0.0172800000000002),
 .UNSPECIFIED.);
#448=B_SPLINE_SURFACE_WITH_KNOTS('',2,1,((#71845,#71846),(#71847,#71848),
(#71849,#71850)),.UNSPECIFIED.,.F.,.F.,.F.,(3,3),(2,2),(0.,1.),(0.,0.0172800000000002),
 .UNSPECIFIED.);
#449=B_SPLINE_SURFACE_WITH_KNOTS('',2,1,((#71860,#71861),(#71862,#71863),
(#71864,#71865)),.UNSPECIFIED.,.F.,.F.,.F.,(3,3),(2,2),(0.,1.),(0.,0.0172800000000002),
 .UNSPECIFIED.);
#450=B_SPLINE_SURFACE_WITH_KNOTS('',2,1,((#71875,#71876),(#71877,#71878),
(#71879,#71880)),.UNSPECIFIED.,.F.,.F.,.F.,(3,3),(2,2),(0.,1.),(0.,0.0172800000000002),
 .UNSPECIFIED.);
#451=B_SPLINE_SURFACE_WITH_KNOTS('',2,1,((#71890,#71891),(#71892,#71893),
(#71894,#71895)),.UNSPECIFIED.,.F.,.F.,.F.,(3,3),(2,2),(0.,1.),(0.,0.0172800000000002),
 .UNSPECIFIED.);
#452=B_SPLINE_SURFACE_WITH_KNOTS('',2,1,((#71905,#71906),(#71907,#71908),
(#71909,#71910)),.UNSPECIFIED.,.F.,.F.,.F.,(3,3),(2,2),(0.,1.),(0.,0.0172800000000002),
 .UNSPECIFIED.);
#453=B_SPLINE_SURFACE_WITH_KNOTS('',2,1,((#71920,#71921),(#71922,#71923),
(#71924,#71925)),.UNSPECIFIED.,.F.,.F.,.F.,(3,3),(2,2),(0.,1.),(0.,0.0172800000000002),
 .UNSPECIFIED.);
#454=B_SPLINE_SURFACE_WITH_KNOTS('',2,1,((#71935,#71936),(#71937,#71938),
(#71939,#71940)),.UNSPECIFIED.,.F.,.F.,.F.,(3,3),(2,2),(0.,1.),(0.,0.0172800000000002),
 .UNSPECIFIED.);
#455=B_SPLINE_SURFACE_WITH_KNOTS('',2,1,((#71950,#71951),(#71952,#71953),
(#71954,#71955)),.UNSPECIFIED.,.F.,.F.,.F.,(3,3),(2,2),(0.,1.),(0.,0.0172800000000002),
 .UNSPECIFIED.);
#456=B_SPLINE_SURFACE_WITH_KNOTS('',2,1,((#71972,#71973),(#71974,#71975),
(#71976,#71977)),.UNSPECIFIED.,.F.,.F.,.F.,(3,3),(2,2),(0.,1.),(0.,0.0172800000000002),
 .UNSPECIFIED.);
#457=B_SPLINE_SURFACE_WITH_KNOTS('',2,1,((#71987,#71988),(#71989,#71990),
(#71991,#71992)),.UNSPECIFIED.,.F.,.F.,.F.,(3,3),(2,2),(0.,1.),(0.,0.0172800000000002),
 .UNSPECIFIED.);
#458=B_SPLINE_SURFACE_WITH_KNOTS('',2,1,((#72008,#72009),(#72010,#72011),
(#72012,#72013)),.UNSPECIFIED.,.F.,.F.,.F.,(3,3),(2,2),(0.,1.),(0.,0.0172800000000002),
 .UNSPECIFIED.);
#459=B_SPLINE_SURFACE_WITH_KNOTS('',2,1,((#72023,#72024),(#72025,#72026),
(#72027,#72028)),.UNSPECIFIED.,.F.,.F.,.F.,(3,3),(2,2),(0.,1.),(0.,0.0172800000000002),
 .UNSPECIFIED.);
#460=B_SPLINE_SURFACE_WITH_KNOTS('',2,1,((#72055,#72056),(#72057,#72058),
(#72059,#72060)),.UNSPECIFIED.,.F.,.F.,.F.,(3,3),(2,2),(0.,1.),(0.,0.0172800000000002),
 .UNSPECIFIED.);
#461=B_SPLINE_SURFACE_WITH_KNOTS('',2,1,((#72073,#72074),(#72075,#72076),
(#72077,#72078)),.UNSPECIFIED.,.F.,.F.,.F.,(3,3),(2,2),(0.,1.),(0.,0.0172800000000002),
 .UNSPECIFIED.);
#462=B_SPLINE_SURFACE_WITH_KNOTS('',2,1,((#72088,#72089),(#72090,#72091),
(#72092,#72093)),.UNSPECIFIED.,.F.,.F.,.F.,(3,3),(2,2),(0.,1.),(0.,0.0172800000000002),
 .UNSPECIFIED.);
#463=B_SPLINE_SURFACE_WITH_KNOTS('',2,1,((#72103,#72104),(#72105,#72106),
(#72107,#72108)),.UNSPECIFIED.,.F.,.F.,.F.,(3,3),(2,2),(0.,1.),(0.,0.0172800000000002),
 .UNSPECIFIED.);
#464=B_SPLINE_SURFACE_WITH_KNOTS('',2,1,((#72118,#72119),(#72120,#72121),
(#72122,#72123)),.UNSPECIFIED.,.F.,.F.,.F.,(3,3),(2,2),(0.,1.),(0.,0.0172800000000002),
 .UNSPECIFIED.);
#465=B_SPLINE_SURFACE_WITH_KNOTS('',2,1,((#72133,#72134),(#72135,#72136),
(#72137,#72138)),.UNSPECIFIED.,.F.,.F.,.F.,(3,3),(2,2),(0.,1.),(0.,0.0172800000000002),
 .UNSPECIFIED.);
#466=B_SPLINE_SURFACE_WITH_KNOTS('',2,1,((#72148,#72149),(#72150,#72151),
(#72152,#72153)),.UNSPECIFIED.,.F.,.F.,.F.,(3,3),(2,2),(0.,1.),(0.,0.0172800000000002),
 .UNSPECIFIED.);
#467=B_SPLINE_SURFACE_WITH_KNOTS('',2,1,((#72163,#72164),(#72165,#72166),
(#72167,#72168)),.UNSPECIFIED.,.F.,.F.,.F.,(3,3),(2,2),(0.,1.),(0.,0.0172800000000002),
 .UNSPECIFIED.);
#468=B_SPLINE_SURFACE_WITH_KNOTS('',2,1,((#72175,#72176),(#72177,#72178),
(#72179,#72180)),.UNSPECIFIED.,.F.,.F.,.F.,(3,3),(2,2),(0.,1.),(0.,0.0172800000000002),
 .UNSPECIFIED.);
#469=B_SPLINE_SURFACE_WITH_KNOTS('',2,1,((#72193,#72194),(#72195,#72196),
(#72197,#72198)),.UNSPECIFIED.,.F.,.F.,.F.,(3,3),(2,2),(0.,1.),(0.,0.0172800000000002),
 .UNSPECIFIED.);
#470=B_SPLINE_SURFACE_WITH_KNOTS('',2,1,((#72208,#72209),(#72210,#72211),
(#72212,#72213)),.UNSPECIFIED.,.F.,.F.,.F.,(3,3),(2,2),(0.,1.),(0.,0.0172800000000002),
 .UNSPECIFIED.);
#471=B_SPLINE_SURFACE_WITH_KNOTS('',2,1,((#72223,#72224),(#72225,#72226),
(#72227,#72228)),.UNSPECIFIED.,.F.,.F.,.F.,(3,3),(2,2),(0.,1.),(0.,0.0172800000000002),
 .UNSPECIFIED.);
#472=B_SPLINE_SURFACE_WITH_KNOTS('',2,1,((#72238,#72239),(#72240,#72241),
(#72242,#72243)),.UNSPECIFIED.,.F.,.F.,.F.,(3,3),(2,2),(0.,1.),(0.,0.0172800000000002),
 .UNSPECIFIED.);
#473=B_SPLINE_SURFACE_WITH_KNOTS('',2,1,((#72253,#72254),(#72255,#72256),
(#72257,#72258)),.UNSPECIFIED.,.F.,.F.,.F.,(3,3),(2,2),(0.,1.),(0.,0.0172800000000002),
 .UNSPECIFIED.);
#474=B_SPLINE_SURFACE_WITH_KNOTS('',2,1,((#72268,#72269),(#72270,#72271),
(#72272,#72273)),.UNSPECIFIED.,.F.,.F.,.F.,(3,3),(2,2),(0.,1.),(0.,0.0172800000000002),
 .UNSPECIFIED.);
#475=B_SPLINE_SURFACE_WITH_KNOTS('',2,1,((#72283,#72284),(#72285,#72286),
(#72287,#72288)),.UNSPECIFIED.,.F.,.F.,.F.,(3,3),(2,2),(0.,1.),(0.,0.0172800000000002),
 .UNSPECIFIED.);
#476=B_SPLINE_SURFACE_WITH_KNOTS('',2,1,((#72298,#72299),(#72300,#72301),
(#72302,#72303)),.UNSPECIFIED.,.F.,.F.,.F.,(3,3),(2,2),(0.,1.),(0.,0.0172800000000002),
 .UNSPECIFIED.);
#477=B_SPLINE_SURFACE_WITH_KNOTS('',2,1,((#72313,#72314),(#72315,#72316),
(#72317,#72318)),.UNSPECIFIED.,.F.,.F.,.F.,(3,3),(2,2),(0.,1.),(0.,0.0172800000000002),
 .UNSPECIFIED.);
#478=B_SPLINE_SURFACE_WITH_KNOTS('',2,1,((#72328,#72329),(#72330,#72331),
(#72332,#72333)),.UNSPECIFIED.,.F.,.F.,.F.,(3,3),(2,2),(0.,1.),(0.,0.0172800000000002),
 .UNSPECIFIED.);
#479=B_SPLINE_SURFACE_WITH_KNOTS('',2,1,((#72343,#72344),(#72345,#72346),
(#72347,#72348)),.UNSPECIFIED.,.F.,.F.,.F.,(3,3),(2,2),(0.,1.),(0.,0.0172800000000002),
 .UNSPECIFIED.);
#480=B_SPLINE_SURFACE_WITH_KNOTS('',2,1,((#72357,#72358),(#72359,#72360),
(#72361,#72362)),.UNSPECIFIED.,.F.,.F.,.F.,(3,3),(2,2),(0.,1.),(0.,0.0172800000000002),
 .UNSPECIFIED.);
#481=B_SPLINE_SURFACE_WITH_KNOTS('',2,1,((#72375,#72376),(#72377,#72378),
(#72379,#72380)),.UNSPECIFIED.,.F.,.F.,.F.,(3,3),(2,2),(0.,1.),(0.,0.0172800000000002),
 .UNSPECIFIED.);
#482=B_SPLINE_SURFACE_WITH_KNOTS('',2,1,((#72390,#72391),(#72392,#72393),
(#72394,#72395)),.UNSPECIFIED.,.F.,.F.,.F.,(3,3),(2,2),(0.,1.),(0.,0.0172800000000002),
 .UNSPECIFIED.);
#483=B_SPLINE_SURFACE_WITH_KNOTS('',2,1,((#72405,#72406),(#72407,#72408),
(#72409,#72410)),.UNSPECIFIED.,.F.,.F.,.F.,(3,3),(2,2),(0.,1.),(0.,0.0172800000000002),
 .UNSPECIFIED.);
#484=B_SPLINE_SURFACE_WITH_KNOTS('',2,1,((#72420,#72421),(#72422,#72423),
(#72424,#72425)),.UNSPECIFIED.,.F.,.F.,.F.,(3,3),(2,2),(0.,1.),(0.,0.0172800000000002),
 .UNSPECIFIED.);
#485=B_SPLINE_SURFACE_WITH_KNOTS('',2,1,((#72435,#72436),(#72437,#72438),
(#72439,#72440)),.UNSPECIFIED.,.F.,.F.,.F.,(3,3),(2,2),(0.,1.),(0.,0.0172800000000002),
 .UNSPECIFIED.);
#486=B_SPLINE_SURFACE_WITH_KNOTS('',2,1,((#72450,#72451),(#72452,#72453),
(#72454,#72455)),.UNSPECIFIED.,.F.,.F.,.F.,(3,3),(2,2),(0.,1.),(0.,0.0172800000000002),
 .UNSPECIFIED.);
#487=B_SPLINE_SURFACE_WITH_KNOTS('',2,1,((#72465,#72466),(#72467,#72468),
(#72469,#72470)),.UNSPECIFIED.,.F.,.F.,.F.,(3,3),(2,2),(0.,1.),(0.,0.0172800000000002),
 .UNSPECIFIED.);
#488=B_SPLINE_SURFACE_WITH_KNOTS('',2,1,((#72477,#72478),(#72479,#72480),
(#72481,#72482)),.UNSPECIFIED.,.F.,.F.,.F.,(3,3),(2,2),(0.,1.),(0.,0.0172800000000002),
 .UNSPECIFIED.);
#489=B_SPLINE_SURFACE_WITH_KNOTS('',2,1,((#72495,#72496),(#72497,#72498),
(#72499,#72500)),.UNSPECIFIED.,.F.,.F.,.F.,(3,3),(2,2),(0.,1.),(0.,0.0172800000000002),
 .UNSPECIFIED.);
#490=B_SPLINE_SURFACE_WITH_KNOTS('',2,1,((#72510,#72511),(#72512,#72513),
(#72514,#72515)),.UNSPECIFIED.,.F.,.F.,.F.,(3,3),(2,2),(0.,1.),(0.,0.0172800000000002),
 .UNSPECIFIED.);
#491=B_SPLINE_SURFACE_WITH_KNOTS('',2,1,((#72525,#72526),(#72527,#72528),
(#72529,#72530)),.UNSPECIFIED.,.F.,.F.,.F.,(3,3),(2,2),(0.,1.),(0.,0.0172800000000002),
 .UNSPECIFIED.);
#492=B_SPLINE_SURFACE_WITH_KNOTS('',2,1,((#72540,#72541),(#72542,#72543),
(#72544,#72545)),.UNSPECIFIED.,.F.,.F.,.F.,(3,3),(2,2),(0.,1.),(0.,0.0172800000000002),
 .UNSPECIFIED.);
#493=B_SPLINE_SURFACE_WITH_KNOTS('',2,1,((#72555,#72556),(#72557,#72558),
(#72559,#72560)),.UNSPECIFIED.,.F.,.F.,.F.,(3,3),(2,2),(0.,1.),(0.,0.0172800000000002),
 .UNSPECIFIED.);
#494=B_SPLINE_SURFACE_WITH_KNOTS('',2,1,((#72570,#72571),(#72572,#72573),
(#72574,#72575)),.UNSPECIFIED.,.F.,.F.,.F.,(3,3),(2,2),(0.,1.),(0.,0.0172800000000002),
 .UNSPECIFIED.);
#495=B_SPLINE_SURFACE_WITH_KNOTS('',2,1,((#72585,#72586),(#72587,#72588),
(#72589,#72590)),.UNSPECIFIED.,.F.,.F.,.F.,(3,3),(2,2),(0.,1.),(0.,0.0172800000000002),
 .UNSPECIFIED.);
#496=B_SPLINE_SURFACE_WITH_KNOTS('',2,1,((#72600,#72601),(#72602,#72603),
(#72604,#72605)),.UNSPECIFIED.,.F.,.F.,.F.,(3,3),(2,2),(0.,1.),(0.,0.0172800000000002),
 .UNSPECIFIED.);
#497=B_SPLINE_SURFACE_WITH_KNOTS('',2,1,((#72615,#72616),(#72617,#72618),
(#72619,#72620)),.UNSPECIFIED.,.F.,.F.,.F.,(3,3),(2,2),(0.,1.),(0.,0.0172800000000002),
 .UNSPECIFIED.);
#498=B_SPLINE_SURFACE_WITH_KNOTS('',2,1,((#72630,#72631),(#72632,#72633),
(#72634,#72635)),.UNSPECIFIED.,.F.,.F.,.F.,(3,3),(2,2),(0.,1.),(0.,0.0172800000000002),
 .UNSPECIFIED.);
#499=B_SPLINE_SURFACE_WITH_KNOTS('',2,1,((#72645,#72646),(#72647,#72648),
(#72649,#72650)),.UNSPECIFIED.,.F.,.F.,.F.,(3,3),(2,2),(0.,1.),(0.,0.0172800000000002),
 .UNSPECIFIED.);
#500=B_SPLINE_SURFACE_WITH_KNOTS('',2,1,((#72667,#72668),(#72669,#72670),
(#72671,#72672)),.UNSPECIFIED.,.F.,.F.,.F.,(3,3),(2,2),(0.,1.),(0.,0.0172800000000002),
 .UNSPECIFIED.);
#501=B_SPLINE_SURFACE_WITH_KNOTS('',2,1,((#72682,#72683),(#72684,#72685),
(#72686,#72687)),.UNSPECIFIED.,.F.,.F.,.F.,(3,3),(2,2),(0.,1.),(0.,0.0172800000000002),
 .UNSPECIFIED.);
#502=B_SPLINE_SURFACE_WITH_KNOTS('',2,1,((#72703,#72704),(#72705,#72706),
(#72707,#72708)),.UNSPECIFIED.,.F.,.F.,.F.,(3,3),(2,2),(0.,1.),(0.,0.0172800000000002),
 .UNSPECIFIED.);
#503=B_SPLINE_SURFACE_WITH_KNOTS('',2,1,((#72718,#72719),(#72720,#72721),
(#72722,#72723)),.UNSPECIFIED.,.F.,.F.,.F.,(3,3),(2,2),(0.,1.),(0.,0.0172800000000002),
 .UNSPECIFIED.);
#504=B_SPLINE_SURFACE_WITH_KNOTS('',2,1,((#72750,#72751),(#72752,#72753),
(#72754,#72755)),.UNSPECIFIED.,.F.,.F.,.F.,(3,3),(2,2),(0.,1.),(0.,0.0172800000000002),
 .UNSPECIFIED.);
#505=B_SPLINE_SURFACE_WITH_KNOTS('',2,1,((#72768,#72769),(#72770,#72771),
(#72772,#72773)),.UNSPECIFIED.,.F.,.F.,.F.,(3,3),(2,2),(0.,1.),(0.,0.0172800000000002),
 .UNSPECIFIED.);
#506=B_SPLINE_SURFACE_WITH_KNOTS('',2,1,((#72783,#72784),(#72785,#72786),
(#72787,#72788)),.UNSPECIFIED.,.F.,.F.,.F.,(3,3),(2,2),(0.,1.),(0.,0.0172800000000002),
 .UNSPECIFIED.);
#507=B_SPLINE_SURFACE_WITH_KNOTS('',2,1,((#72798,#72799),(#72800,#72801),
(#72802,#72803)),.UNSPECIFIED.,.F.,.F.,.F.,(3,3),(2,2),(0.,1.),(0.,0.0172800000000002),
 .UNSPECIFIED.);
#508=B_SPLINE_SURFACE_WITH_KNOTS('',2,1,((#72813,#72814),(#72815,#72816),
(#72817,#72818)),.UNSPECIFIED.,.F.,.F.,.F.,(3,3),(2,2),(0.,1.),(0.,0.0172800000000002),
 .UNSPECIFIED.);
#509=B_SPLINE_SURFACE_WITH_KNOTS('',2,1,((#72828,#72829),(#72830,#72831),
(#72832,#72833)),.UNSPECIFIED.,.F.,.F.,.F.,(3,3),(2,2),(0.,1.),(0.,0.0172800000000002),
 .UNSPECIFIED.);
#510=B_SPLINE_SURFACE_WITH_KNOTS('',2,1,((#72843,#72844),(#72845,#72846),
(#72847,#72848)),.UNSPECIFIED.,.F.,.F.,.F.,(3,3),(2,2),(0.,1.),(0.,0.0172800000000002),
 .UNSPECIFIED.);
#511=B_SPLINE_SURFACE_WITH_KNOTS('',2,1,((#72858,#72859),(#72860,#72861),
(#72862,#72863)),.UNSPECIFIED.,.F.,.F.,.F.,(3,3),(2,2),(0.,1.),(0.,0.0172800000000002),
 .UNSPECIFIED.);
#512=B_SPLINE_SURFACE_WITH_KNOTS('',2,1,((#72870,#72871),(#72872,#72873),
(#72874,#72875)),.UNSPECIFIED.,.F.,.F.,.F.,(3,3),(2,2),(0.,1.),(0.,0.0172800000000002),
 .UNSPECIFIED.);
#513=B_SPLINE_SURFACE_WITH_KNOTS('',2,1,((#72888,#72889),(#72890,#72891),
(#72892,#72893)),.UNSPECIFIED.,.F.,.F.,.F.,(3,3),(2,2),(0.,1.),(0.,0.0172800000000002),
 .UNSPECIFIED.);
#514=B_SPLINE_SURFACE_WITH_KNOTS('',2,1,((#72903,#72904),(#72905,#72906),
(#72907,#72908)),.UNSPECIFIED.,.F.,.F.,.F.,(3,3),(2,2),(0.,1.),(0.,0.0172800000000002),
 .UNSPECIFIED.);
#515=B_SPLINE_SURFACE_WITH_KNOTS('',2,1,((#72918,#72919),(#72920,#72921),
(#72922,#72923)),.UNSPECIFIED.,.F.,.F.,.F.,(3,3),(2,2),(0.,1.),(0.,0.0172800000000002),
 .UNSPECIFIED.);
#516=B_SPLINE_SURFACE_WITH_KNOTS('',2,1,((#72933,#72934),(#72935,#72936),
(#72937,#72938)),.UNSPECIFIED.,.F.,.F.,.F.,(3,3),(2,2),(0.,1.),(0.,0.0172800000000002),
 .UNSPECIFIED.);
#517=B_SPLINE_SURFACE_WITH_KNOTS('',2,1,((#72948,#72949),(#72950,#72951),
(#72952,#72953)),.UNSPECIFIED.,.F.,.F.,.F.,(3,3),(2,2),(0.,1.),(0.,0.0172800000000002),
 .UNSPECIFIED.);
#518=B_SPLINE_SURFACE_WITH_KNOTS('',2,1,((#72963,#72964),(#72965,#72966),
(#72967,#72968)),.UNSPECIFIED.,.F.,.F.,.F.,(3,3),(2,2),(0.,1.),(0.,0.0172800000000002),
 .UNSPECIFIED.);
#519=B_SPLINE_SURFACE_WITH_KNOTS('',2,1,((#72978,#72979),(#72980,#72981),
(#72982,#72983)),.UNSPECIFIED.,.F.,.F.,.F.,(3,3),(2,2),(0.,1.),(0.,0.0172800000000002),
 .UNSPECIFIED.);
#520=B_SPLINE_SURFACE_WITH_KNOTS('',2,1,((#72993,#72994),(#72995,#72996),
(#72997,#72998)),.UNSPECIFIED.,.F.,.F.,.F.,(3,3),(2,2),(0.,1.),(0.,0.0172800000000002),
 .UNSPECIFIED.);
#521=B_SPLINE_SURFACE_WITH_KNOTS('',2,1,((#73008,#73009),(#73010,#73011),
(#73012,#73013)),.UNSPECIFIED.,.F.,.F.,.F.,(3,3),(2,2),(0.,1.),(0.,0.0172800000000002),
 .UNSPECIFIED.);
#522=B_SPLINE_SURFACE_WITH_KNOTS('',2,1,((#73023,#73024),(#73025,#73026),
(#73027,#73028)),.UNSPECIFIED.,.F.,.F.,.F.,(3,3),(2,2),(0.,1.),(0.,0.0172800000000002),
 .UNSPECIFIED.);
#523=B_SPLINE_SURFACE_WITH_KNOTS('',2,1,((#73038,#73039),(#73040,#73041),
(#73042,#73043)),.UNSPECIFIED.,.F.,.F.,.F.,(3,3),(2,2),(0.,1.),(0.,0.0172800000000002),
 .UNSPECIFIED.);
#524=B_SPLINE_SURFACE_WITH_KNOTS('',2,1,((#73051,#73052),(#73053,#73054),
(#73055,#73056)),.UNSPECIFIED.,.F.,.F.,.F.,(3,3),(2,2),(0.,1.),(0.,0.0172800000000002),
 .UNSPECIFIED.);
#525=B_SPLINE_SURFACE_WITH_KNOTS('',2,1,((#73069,#73070),(#73071,#73072),
(#73073,#73074)),.UNSPECIFIED.,.F.,.F.,.F.,(3,3),(2,2),(0.,1.),(0.,0.0172800000000002),
 .UNSPECIFIED.);
#526=B_SPLINE_SURFACE_WITH_KNOTS('',2,1,((#73084,#73085),(#73086,#73087),
(#73088,#73089)),.UNSPECIFIED.,.F.,.F.,.F.,(3,3),(2,2),(0.,1.),(0.,0.0172800000000002),
 .UNSPECIFIED.);
#527=B_SPLINE_SURFACE_WITH_KNOTS('',2,1,((#73099,#73100),(#73101,#73102),
(#73103,#73104)),.UNSPECIFIED.,.F.,.F.,.F.,(3,3),(2,2),(0.,1.),(0.,0.0172800000000002),
 .UNSPECIFIED.);
#528=B_SPLINE_SURFACE_WITH_KNOTS('',2,1,((#73114,#73115),(#73116,#73117),
(#73118,#73119)),.UNSPECIFIED.,.F.,.F.,.F.,(3,3),(2,2),(0.,1.),(0.,0.0172800000000002),
 .UNSPECIFIED.);
#529=B_SPLINE_SURFACE_WITH_KNOTS('',2,1,((#73129,#73130),(#73131,#73132),
(#73133,#73134)),.UNSPECIFIED.,.F.,.F.,.F.,(3,3),(2,2),(0.,1.),(0.,0.0172800000000002),
 .UNSPECIFIED.);
#530=B_SPLINE_SURFACE_WITH_KNOTS('',2,1,((#73144,#73145),(#73146,#73147),
(#73148,#73149)),.UNSPECIFIED.,.F.,.F.,.F.,(3,3),(2,2),(0.,1.),(0.,0.0172800000000002),
 .UNSPECIFIED.);
#531=B_SPLINE_SURFACE_WITH_KNOTS('',2,1,((#73159,#73160),(#73161,#73162),
(#73163,#73164)),.UNSPECIFIED.,.F.,.F.,.F.,(3,3),(2,2),(0.,1.),(0.,0.0172800000000002),
 .UNSPECIFIED.);
#532=B_SPLINE_SURFACE_WITH_KNOTS('',2,1,((#73174,#73175),(#73176,#73177),
(#73178,#73179)),.UNSPECIFIED.,.F.,.F.,.F.,(3,3),(2,2),(0.,1.),(0.,0.0172800000000002),
 .UNSPECIFIED.);
#533=B_SPLINE_SURFACE_WITH_KNOTS('',2,1,((#73195,#73196),(#73197,#73198),
(#73199,#73200)),.UNSPECIFIED.,.F.,.F.,.F.,(3,3),(2,2),(0.,1.),(0.,0.0172800000000002),
 .UNSPECIFIED.);
#534=B_SPLINE_SURFACE_WITH_KNOTS('',2,1,((#73210,#73211),(#73212,#73213),
(#73214,#73215)),.UNSPECIFIED.,.F.,.F.,.F.,(3,3),(2,2),(0.,1.),(0.,0.0172800000000002),
 .UNSPECIFIED.);
#535=B_SPLINE_SURFACE_WITH_KNOTS('',2,1,((#73225,#73226),(#73227,#73228),
(#73229,#73230)),.UNSPECIFIED.,.F.,.F.,.F.,(3,3),(2,2),(0.,1.),(0.,0.0172800000000002),
 .UNSPECIFIED.);
#536=B_SPLINE_SURFACE_WITH_KNOTS('',2,1,((#73240,#73241),(#73242,#73243),
(#73244,#73245)),.UNSPECIFIED.,.F.,.F.,.F.,(3,3),(2,2),(0.,1.),(0.,0.0172800000000002),
 .UNSPECIFIED.);
#537=B_SPLINE_SURFACE_WITH_KNOTS('',2,1,((#73255,#73256),(#73257,#73258),
(#73259,#73260)),.UNSPECIFIED.,.F.,.F.,.F.,(3,3),(2,2),(0.,1.),(0.,0.0172800000000002),
 .UNSPECIFIED.);
#538=B_SPLINE_SURFACE_WITH_KNOTS('',2,1,((#73270,#73271),(#73272,#73273),
(#73274,#73275)),.UNSPECIFIED.,.F.,.F.,.F.,(3,3),(2,2),(0.,1.),(0.,0.0172800000000002),
 .UNSPECIFIED.);
#539=B_SPLINE_SURFACE_WITH_KNOTS('',2,1,((#73285,#73286),(#73287,#73288),
(#73289,#73290)),.UNSPECIFIED.,.F.,.F.,.F.,(3,3),(2,2),(0.,1.),(0.,0.0172800000000002),
 .UNSPECIFIED.);
#540=B_SPLINE_SURFACE_WITH_KNOTS('',2,1,((#73300,#73301),(#73302,#73303),
(#73304,#73305)),.UNSPECIFIED.,.F.,.F.,.F.,(3,3),(2,2),(0.,1.),(0.,0.0172800000000002),
 .UNSPECIFIED.);
#541=B_SPLINE_SURFACE_WITH_KNOTS('',2,1,((#73315,#73316),(#73317,#73318),
(#73319,#73320)),.UNSPECIFIED.,.F.,.F.,.F.,(3,3),(2,2),(0.,1.),(0.,0.0172800000000002),
 .UNSPECIFIED.);
#542=B_SPLINE_SURFACE_WITH_KNOTS('',2,1,((#73347,#73348),(#73349,#73350),
(#73351,#73352)),.UNSPECIFIED.,.F.,.F.,.F.,(3,3),(2,2),(0.,1.),(0.,0.0172800000000002),
 .UNSPECIFIED.);
#543=B_SPLINE_SURFACE_WITH_KNOTS('',2,1,((#73365,#73366),(#73367,#73368),
(#73369,#73370)),.UNSPECIFIED.,.F.,.F.,.F.,(3,3),(2,2),(0.,1.),(0.,0.0172800000000002),
 .UNSPECIFIED.);
#544=B_SPLINE_SURFACE_WITH_KNOTS('',2,1,((#73380,#73381),(#73382,#73383),
(#73384,#73385)),.UNSPECIFIED.,.F.,.F.,.F.,(3,3),(2,2),(0.,1.),(0.,0.0172800000000002),
 .UNSPECIFIED.);
#545=B_SPLINE_SURFACE_WITH_KNOTS('',2,1,((#73395,#73396),(#73397,#73398),
(#73399,#73400)),.UNSPECIFIED.,.F.,.F.,.F.,(3,3),(2,2),(0.,1.),(0.,0.0172800000000002),
 .UNSPECIFIED.);
#546=B_SPLINE_SURFACE_WITH_KNOTS('',2,1,((#73410,#73411),(#73412,#73413),
(#73414,#73415)),.UNSPECIFIED.,.F.,.F.,.F.,(3,3),(2,2),(0.,1.),(0.,0.0172800000000002),
 .UNSPECIFIED.);
#547=B_SPLINE_SURFACE_WITH_KNOTS('',2,1,((#73425,#73426),(#73427,#73428),
(#73429,#73430)),.UNSPECIFIED.,.F.,.F.,.F.,(3,3),(2,2),(0.,1.),(0.,0.0172800000000002),
 .UNSPECIFIED.);
#548=B_SPLINE_SURFACE_WITH_KNOTS('',2,1,((#73440,#73441),(#73442,#73443),
(#73444,#73445)),.UNSPECIFIED.,.F.,.F.,.F.,(3,3),(2,2),(0.,1.),(0.,0.0172800000000002),
 .UNSPECIFIED.);
#549=B_SPLINE_SURFACE_WITH_KNOTS('',2,1,((#73455,#73456),(#73457,#73458),
(#73459,#73460)),.UNSPECIFIED.,.F.,.F.,.F.,(3,3),(2,2),(0.,1.),(0.,0.0172800000000002),
 .UNSPECIFIED.);
#550=B_SPLINE_SURFACE_WITH_KNOTS('',2,1,((#73467,#73468),(#73469,#73470),
(#73471,#73472)),.UNSPECIFIED.,.F.,.F.,.F.,(3,3),(2,2),(0.,1.),(0.,0.0172800000000002),
 .UNSPECIFIED.);
#551=B_SPLINE_SURFACE_WITH_KNOTS('',2,1,((#73485,#73486),(#73487,#73488),
(#73489,#73490)),.UNSPECIFIED.,.F.,.F.,.F.,(3,3),(2,2),(0.,1.),(0.,0.0172800000000002),
 .UNSPECIFIED.);
#552=B_SPLINE_SURFACE_WITH_KNOTS('',2,1,((#73500,#73501),(#73502,#73503),
(#73504,#73505)),.UNSPECIFIED.,.F.,.F.,.F.,(3,3),(2,2),(0.,1.),(0.,0.0172800000000002),
 .UNSPECIFIED.);
#553=B_SPLINE_SURFACE_WITH_KNOTS('',2,1,((#73515,#73516),(#73517,#73518),
(#73519,#73520)),.UNSPECIFIED.,.F.,.F.,.F.,(3,3),(2,2),(0.,1.),(0.,0.0172800000000002),
 .UNSPECIFIED.);
#554=B_SPLINE_SURFACE_WITH_KNOTS('',2,1,((#73530,#73531),(#73532,#73533),
(#73534,#73535)),.UNSPECIFIED.,.F.,.F.,.F.,(3,3),(2,2),(0.,1.),(0.,0.0172800000000002),
 .UNSPECIFIED.);
#555=B_SPLINE_SURFACE_WITH_KNOTS('',2,1,((#73545,#73546),(#73547,#73548),
(#73549,#73550)),.UNSPECIFIED.,.F.,.F.,.F.,(3,3),(2,2),(0.,1.),(0.,0.0172800000000002),
 .UNSPECIFIED.);
#556=B_SPLINE_SURFACE_WITH_KNOTS('',2,1,((#73560,#73561),(#73562,#73563),
(#73564,#73565)),.UNSPECIFIED.,.F.,.F.,.F.,(3,3),(2,2),(0.,1.),(0.,0.0172800000000002),
 .UNSPECIFIED.);
#557=B_SPLINE_SURFACE_WITH_KNOTS('',2,1,((#73575,#73576),(#73577,#73578),
(#73579,#73580)),.UNSPECIFIED.,.F.,.F.,.F.,(3,3),(2,2),(0.,1.),(0.,0.0172800000000002),
 .UNSPECIFIED.);
#558=B_SPLINE_SURFACE_WITH_KNOTS('',2,1,((#73590,#73591),(#73592,#73593),
(#73594,#73595)),.UNSPECIFIED.,.F.,.F.,.F.,(3,3),(2,2),(0.,1.),(0.,0.0172800000000002),
 .UNSPECIFIED.);
#559=B_SPLINE_SURFACE_WITH_KNOTS('',2,1,((#73605,#73606),(#73607,#73608),
(#73609,#73610)),.UNSPECIFIED.,.F.,.F.,.F.,(3,3),(2,2),(0.,1.),(0.,0.0172800000000002),
 .UNSPECIFIED.);
#560=B_SPLINE_SURFACE_WITH_KNOTS('',2,1,((#73620,#73621),(#73622,#73623),
(#73624,#73625)),.UNSPECIFIED.,.F.,.F.,.F.,(3,3),(2,2),(0.,1.),(0.,0.0172800000000002),
 .UNSPECIFIED.);
#561=B_SPLINE_SURFACE_WITH_KNOTS('',2,1,((#73635,#73636),(#73637,#73638),
(#73639,#73640)),.UNSPECIFIED.,.F.,.F.,.F.,(3,3),(2,2),(0.,1.),(0.,0.0172800000000002),
 .UNSPECIFIED.);
#562=B_SPLINE_SURFACE_WITH_KNOTS('',2,1,((#73648,#73649),(#73650,#73651),
(#73652,#73653)),.UNSPECIFIED.,.F.,.F.,.F.,(3,3),(2,2),(0.,1.),(0.,0.0172800000000002),
 .UNSPECIFIED.);
#563=B_SPLINE_SURFACE_WITH_KNOTS('',2,1,((#73666,#73667),(#73668,#73669),
(#73670,#73671)),.UNSPECIFIED.,.F.,.F.,.F.,(3,3),(2,2),(0.,1.),(0.,0.0172800000000002),
 .UNSPECIFIED.);
#564=B_SPLINE_SURFACE_WITH_KNOTS('',2,1,((#73681,#73682),(#73683,#73684),
(#73685,#73686)),.UNSPECIFIED.,.F.,.F.,.F.,(3,3),(2,2),(0.,1.),(0.,0.0172800000000002),
 .UNSPECIFIED.);
#565=B_SPLINE_SURFACE_WITH_KNOTS('',2,1,((#73696,#73697),(#73698,#73699),
(#73700,#73701)),.UNSPECIFIED.,.F.,.F.,.F.,(3,3),(2,2),(0.,1.),(0.,0.0172800000000002),
 .UNSPECIFIED.);
#566=B_SPLINE_SURFACE_WITH_KNOTS('',2,1,((#73711,#73712),(#73713,#73714),
(#73715,#73716)),.UNSPECIFIED.,.F.,.F.,.F.,(3,3),(2,2),(0.,1.),(0.,0.0172800000000002),
 .UNSPECIFIED.);
#567=B_SPLINE_SURFACE_WITH_KNOTS('',2,1,((#73726,#73727),(#73728,#73729),
(#73730,#73731)),.UNSPECIFIED.,.F.,.F.,.F.,(3,3),(2,2),(0.,1.),(0.,0.0172800000000002),
 .UNSPECIFIED.);
#568=B_SPLINE_SURFACE_WITH_KNOTS('',2,1,((#73741,#73742),(#73743,#73744),
(#73745,#73746)),.UNSPECIFIED.,.F.,.F.,.F.,(3,3),(2,2),(0.,1.),(0.,0.0172800000000002),
 .UNSPECIFIED.);
#569=B_SPLINE_SURFACE_WITH_KNOTS('',2,1,((#73756,#73757),(#73758,#73759),
(#73760,#73761)),.UNSPECIFIED.,.F.,.F.,.F.,(3,3),(2,2),(0.,1.),(0.,0.0172800000000002),
 .UNSPECIFIED.);
#570=B_SPLINE_SURFACE_WITH_KNOTS('',2,1,((#73771,#73772),(#73773,#73774),
(#73775,#73776)),.UNSPECIFIED.,.F.,.F.,.F.,(3,3),(2,2),(0.,1.),(0.,0.0172800000000002),
 .UNSPECIFIED.);
#571=B_SPLINE_SURFACE_WITH_KNOTS('',2,1,((#73786,#73787),(#73788,#73789),
(#73790,#73791)),.UNSPECIFIED.,.F.,.F.,.F.,(3,3),(2,2),(0.,1.),(0.,0.0172800000000002),
 .UNSPECIFIED.);
#572=B_SPLINE_SURFACE_WITH_KNOTS('',2,1,((#73801,#73802),(#73803,#73804),
(#73805,#73806)),.UNSPECIFIED.,.F.,.F.,.F.,(3,3),(2,2),(0.,1.),(0.,0.0172800000000002),
 .UNSPECIFIED.);
#573=B_SPLINE_SURFACE_WITH_KNOTS('',2,1,((#73816,#73817),(#73818,#73819),
(#73820,#73821)),.UNSPECIFIED.,.F.,.F.,.F.,(3,3),(2,2),(0.,1.),(0.,0.0172800000000002),
 .UNSPECIFIED.);
#574=B_SPLINE_SURFACE_WITH_KNOTS('',2,1,((#73837,#73838),(#73839,#73840),
(#73841,#73842)),.UNSPECIFIED.,.F.,.F.,.F.,(3,3),(2,2),(0.,1.),(0.,0.0172800000000002),
 .UNSPECIFIED.);
#575=B_SPLINE_SURFACE_WITH_KNOTS('',2,1,((#73852,#73853),(#73854,#73855),
(#73856,#73857)),.UNSPECIFIED.,.F.,.F.,.F.,(3,3),(2,2),(0.,1.),(0.,0.0172800000000002),
 .UNSPECIFIED.);
#576=B_SPLINE_SURFACE_WITH_KNOTS('',2,1,((#73867,#73868),(#73869,#73870),
(#73871,#73872)),.UNSPECIFIED.,.F.,.F.,.F.,(3,3),(2,2),(0.,1.),(0.,0.0172800000000002),
 .UNSPECIFIED.);
#577=B_SPLINE_SURFACE_WITH_KNOTS('',2,1,((#73882,#73883),(#73884,#73885),
(#73886,#73887)),.UNSPECIFIED.,.F.,.F.,.F.,(3,3),(2,2),(0.,1.),(0.,0.0172800000000002),
 .UNSPECIFIED.);
#578=B_SPLINE_SURFACE_WITH_KNOTS('',2,1,((#73897,#73898),(#73899,#73900),
(#73901,#73902)),.UNSPECIFIED.,.F.,.F.,.F.,(3,3),(2,2),(0.,1.),(0.,0.0172800000000002),
 .UNSPECIFIED.);
#579=B_SPLINE_SURFACE_WITH_KNOTS('',2,1,((#73912,#73913),(#73914,#73915),
(#73916,#73917)),.UNSPECIFIED.,.F.,.F.,.F.,(3,3),(2,2),(0.,1.),(0.,0.0172800000000002),
 .UNSPECIFIED.);
#580=B_SPLINE_SURFACE_WITH_KNOTS('',2,1,((#73927,#73928),(#73929,#73930),
(#73931,#73932)),.UNSPECIFIED.,.F.,.F.,.F.,(3,3),(2,2),(0.,1.),(0.,0.0172800000000002),
 .UNSPECIFIED.);
#581=B_SPLINE_SURFACE_WITH_KNOTS('',2,1,((#73948,#73949),(#73950,#73951),
(#73952,#73953)),.UNSPECIFIED.,.F.,.F.,.F.,(3,3),(2,2),(0.,1.),(0.,0.0172800000000002),
 .UNSPECIFIED.);
#582=B_SPLINE_SURFACE_WITH_KNOTS('',2,1,((#73963,#73964),(#73965,#73966),
(#73967,#73968)),.UNSPECIFIED.,.F.,.F.,.F.,(3,3),(2,2),(0.,1.),(0.,0.0172800000000002),
 .UNSPECIFIED.);
#583=B_SPLINE_SURFACE_WITH_KNOTS('',2,1,((#73978,#73979),(#73980,#73981),
(#73982,#73983)),.UNSPECIFIED.,.F.,.F.,.F.,(3,3),(2,2),(0.,1.),(0.,0.0172800000000002),
 .UNSPECIFIED.);
#584=B_SPLINE_SURFACE_WITH_KNOTS('',2,1,((#73993,#73994),(#73995,#73996),
(#73997,#73998)),.UNSPECIFIED.,.F.,.F.,.F.,(3,3),(2,2),(0.,1.),(0.,0.0172800000000002),
 .UNSPECIFIED.);
#585=B_SPLINE_SURFACE_WITH_KNOTS('',2,1,((#74008,#74009),(#74010,#74011),
(#74012,#74013)),.UNSPECIFIED.,.F.,.F.,.F.,(3,3),(2,2),(0.,1.),(0.,0.0172800000000002),
 .UNSPECIFIED.);
#586=B_SPLINE_SURFACE_WITH_KNOTS('',2,1,((#74023,#74024),(#74025,#74026),
(#74027,#74028)),.UNSPECIFIED.,.F.,.F.,.F.,(3,3),(2,2),(0.,1.),(0.,0.0172800000000002),
 .UNSPECIFIED.);
#587=B_SPLINE_SURFACE_WITH_KNOTS('',2,1,((#74038,#74039),(#74040,#74041),
(#74042,#74043)),.UNSPECIFIED.,.F.,.F.,.F.,(3,3),(2,2),(0.,1.),(0.,0.0172800000000002),
 .UNSPECIFIED.);
#588=B_SPLINE_SURFACE_WITH_KNOTS('',2,1,((#74059,#74060),(#74061,#74062),
(#74063,#74064)),.UNSPECIFIED.,.F.,.F.,.F.,(3,3),(2,2),(0.,1.),(0.,0.0172800000000002),
 .UNSPECIFIED.);
#589=B_SPLINE_SURFACE_WITH_KNOTS('',2,1,((#74073,#74074),(#74075,#74076),
(#74077,#74078)),.UNSPECIFIED.,.F.,.F.,.F.,(3,3),(2,2),(0.,1.),(0.,0.0172800000000002),
 .UNSPECIFIED.);
#590=B_SPLINE_SURFACE_WITH_KNOTS('',2,1,((#74091,#74092),(#74093,#74094),
(#74095,#74096)),.UNSPECIFIED.,.F.,.F.,.F.,(3,3),(2,2),(0.,1.),(0.,0.0172800000000002),
 .UNSPECIFIED.);
#591=B_SPLINE_SURFACE_WITH_KNOTS('',2,1,((#74106,#74107),(#74108,#74109),
(#74110,#74111)),.UNSPECIFIED.,.F.,.F.,.F.,(3,3),(2,2),(0.,1.),(0.,0.0172800000000002),
 .UNSPECIFIED.);
#592=B_SPLINE_SURFACE_WITH_KNOTS('',2,1,((#74121,#74122),(#74123,#74124),
(#74125,#74126)),.UNSPECIFIED.,.F.,.F.,.F.,(3,3),(2,2),(0.,1.),(0.,0.0172800000000002),
 .UNSPECIFIED.);
#593=B_SPLINE_SURFACE_WITH_KNOTS('',2,1,((#74136,#74137),(#74138,#74139),
(#74140,#74141)),.UNSPECIFIED.,.F.,.F.,.F.,(3,3),(2,2),(0.,1.),(0.,0.0172800000000002),
 .UNSPECIFIED.);
#594=B_SPLINE_SURFACE_WITH_KNOTS('',2,1,((#74151,#74152),(#74153,#74154),
(#74155,#74156)),.UNSPECIFIED.,.F.,.F.,.F.,(3,3),(2,2),(0.,1.),(0.,0.0172800000000002),
 .UNSPECIFIED.);
#595=B_SPLINE_SURFACE_WITH_KNOTS('',2,1,((#74166,#74167),(#74168,#74169),
(#74170,#74171)),.UNSPECIFIED.,.F.,.F.,.F.,(3,3),(2,2),(0.,1.),(0.,0.0172800000000002),
 .UNSPECIFIED.);
#596=B_SPLINE_SURFACE_WITH_KNOTS('',2,1,((#74181,#74182),(#74183,#74184),
(#74185,#74186)),.UNSPECIFIED.,.F.,.F.,.F.,(3,3),(2,2),(0.,1.),(0.,0.0172800000000002),
 .UNSPECIFIED.);
#597=B_SPLINE_SURFACE_WITH_KNOTS('',2,1,((#74193,#74194),(#74195,#74196),
(#74197,#74198)),.UNSPECIFIED.,.F.,.F.,.F.,(3,3),(2,2),(0.,1.),(0.,0.0172800000000002),
 .UNSPECIFIED.);
#598=B_SPLINE_SURFACE_WITH_KNOTS('',2,1,((#74211,#74212),(#74213,#74214),
(#74215,#74216)),.UNSPECIFIED.,.F.,.F.,.F.,(3,3),(2,2),(0.,1.),(0.,0.0172800000000002),
 .UNSPECIFIED.);
#599=B_SPLINE_SURFACE_WITH_KNOTS('',2,1,((#74226,#74227),(#74228,#74229),
(#74230,#74231)),.UNSPECIFIED.,.F.,.F.,.F.,(3,3),(2,2),(0.,1.),(0.,0.0172800000000002),
 .UNSPECIFIED.);
#600=B_SPLINE_SURFACE_WITH_KNOTS('',2,1,((#74241,#74242),(#74243,#74244),
(#74245,#74246)),.UNSPECIFIED.,.F.,.F.,.F.,(3,3),(2,2),(0.,1.),(0.,0.0172800000000002),
 .UNSPECIFIED.);
#601=B_SPLINE_SURFACE_WITH_KNOTS('',2,1,((#74256,#74257),(#74258,#74259),
(#74260,#74261)),.UNSPECIFIED.,.F.,.F.,.F.,(3,3),(2,2),(0.,1.),(0.,0.0172800000000002),
 .UNSPECIFIED.);
#602=B_SPLINE_SURFACE_WITH_KNOTS('',2,1,((#74271,#74272),(#74273,#74274),
(#74275,#74276)),.UNSPECIFIED.,.F.,.F.,.F.,(3,3),(2,2),(0.,1.),(0.,0.0172800000000002),
 .UNSPECIFIED.);
#603=B_SPLINE_SURFACE_WITH_KNOTS('',2,1,((#74286,#74287),(#74288,#74289),
(#74290,#74291)),.UNSPECIFIED.,.F.,.F.,.F.,(3,3),(2,2),(0.,1.),(0.,0.0172800000000002),
 .UNSPECIFIED.);
#604=B_SPLINE_SURFACE_WITH_KNOTS('',2,1,((#74301,#74302),(#74303,#74304),
(#74305,#74306)),.UNSPECIFIED.,.F.,.F.,.F.,(3,3),(2,2),(0.,1.),(0.,0.0172800000000002),
 .UNSPECIFIED.);
#605=B_SPLINE_SURFACE_WITH_KNOTS('',2,1,((#74316,#74317),(#74318,#74319),
(#74320,#74321)),.UNSPECIFIED.,.F.,.F.,.F.,(3,3),(2,2),(0.,1.),(0.,0.0172800000000002),
 .UNSPECIFIED.);
#606=B_SPLINE_SURFACE_WITH_KNOTS('',2,1,((#74331,#74332),(#74333,#74334),
(#74335,#74336)),.UNSPECIFIED.,.F.,.F.,.F.,(3,3),(2,2),(0.,1.),(0.,0.0172800000000002),
 .UNSPECIFIED.);
#607=B_SPLINE_SURFACE_WITH_KNOTS('',2,1,((#74346,#74347),(#74348,#74349),
(#74350,#74351)),.UNSPECIFIED.,.F.,.F.,.F.,(3,3),(2,2),(0.,1.),(0.,0.0172800000000002),
 .UNSPECIFIED.);
#608=B_SPLINE_SURFACE_WITH_KNOTS('',2,1,((#74361,#74362),(#74363,#74364),
(#74365,#74366)),.UNSPECIFIED.,.F.,.F.,.F.,(3,3),(2,2),(0.,1.),(0.,0.0172800000000002),
 .UNSPECIFIED.);
#609=B_SPLINE_SURFACE_WITH_KNOTS('',3,3,((#83357,#83358,#83359,#83360,#83361,
#83362,#83363,#83364,#83365,#83366,#83367,#83368,#83369,#83370,#83371,#83372,
#83373,#83374,#83375,#83376,#83377,#83378,#83379,#83380,#83381,#83382,#83383,
#83384,#83385,#83386,#83387,#83388,#83389,#83390,#83391,#83392,#83393,#83394,
#83395,#83396,#83397,#83398,#83399,#83400,#83401,#83402,#83403,#83404,#83405,
#83406,#83407,#83408,#83409,#83410,#83411,#83412,#83413,#83414,#83415),
(#83416,#83417,#83418,#83419,#83420,#83421,#83422,#83423,#83424,#83425,
#83426,#83427,#83428,#83429,#83430,#83431,#83432,#83433,#83434,#83435,#83436,
#83437,#83438,#83439,#83440,#83441,#83442,#83443,#83444,#83445,#83446,#83447,
#83448,#83449,#83450,#83451,#83452,#83453,#83454,#83455,#83456,#83457,#83458,
#83459,#83460,#83461,#83462,#83463,#83464,#83465,#83466,#83467,#83468,#83469,
#83470,#83471,#83472,#83473,#83474),(#83475,#83476,#83477,#83478,#83479,
#83480,#83481,#83482,#83483,#83484,#83485,#83486,#83487,#83488,#83489,#83490,
#83491,#83492,#83493,#83494,#83495,#83496,#83497,#83498,#83499,#83500,#83501,
#83502,#83503,#83504,#83505,#83506,#83507,#83508,#83509,#83510,#83511,#83512,
#83513,#83514,#83515,#83516,#83517,#83518,#83519,#83520,#83521,#83522,#83523,
#83524,#83525,#83526,#83527,#83528,#83529,#83530,#83531,#83532,#83533),
(#83534,#83535,#83536,#83537,#83538,#83539,#83540,#83541,#83542,#83543,
#83544,#83545,#83546,#83547,#83548,#83549,#83550,#83551,#83552,#83553,#83554,
#83555,#83556,#83557,#83558,#83559,#83560,#83561,#83562,#83563,#83564,#83565,
#83566,#83567,#83568,#83569,#83570,#83571,#83572,#83573,#83574,#83575,#83576,
#83577,#83578,#83579,#83580,#83581,#83582,#83583,#83584,#83585,#83586,#83587,
#83588,#83589,#83590,#83591,#83592)),.UNSPECIFIED.,.F.,.F.,.F.,(4,4),(4,
1,1,1,1,1,1,1,1,1,1,1,1,1,1,1,1,1,1,1,1,1,1,1,1,1,1,1,1,1,1,1,1,1,1,1,1,
1,1,1,1,1,1,1,1,1,1,1,1,1,1,1,1,1,1,1,4),(-0.000249795523849274,0.0332892348118687),
(8.30174248738077,9.29791605267402,10.2937959510397,11.2896758494053,12.285555747771,
13.2814356461366,14.2773155445023,15.2731954428679,16.2690753412336,17.2649552395992,
18.2608351379649,19.2567150363305,20.2525949346962,21.2484748330618,22.2443547314275,
23.2402346297932,24.2361145281588,25.2319944265245,26.2278743248901,27.2237542232558,
28.2196341216214,29.2155140199871,30.2113939183527,31.2072738167184,32.203153715084,
33.1990336134497,34.1949135118153,35.190793410181,36.1866733085466,37.1825532069123,
38.1784331052779,39.1743130036436,40.1701929020092,41.1660728003749,42.1619526987405,
43.1578325971062,44.1537124954719,45.1495923938375,46.1454722922032,47.1413521905688,
48.1372320889345,49.1331119873001,50.1289918856658,51.1248717840314,52.1207516823971,
53.1166315807627,54.1125114791284,55.108391377494,56.1042712758597,57.1001511742253,
58.096031072591,59.0919109709566,60.0877908693223,61.0836707676879,62.0795506660536,
63.0754305644193,64.0715602583087),.UNSPECIFIED.);
#610=B_SPLINE_SURFACE_WITH_KNOTS('',3,3,((#83776,#83777,#83778,#83779,#83780,
#83781,#83782,#83783,#83784,#83785,#83786,#83787,#83788,#83789,#83790,#83791,
#83792,#83793,#83794,#83795,#83796,#83797,#83798,#83799,#83800,#83801,#83802,
#83803,#83804,#83805,#83806,#83807,#83808,#83809,#83810,#83811,#83812,#83813,
#83814,#83815,#83816,#83817,#83818,#83819,#83820,#83821,#83822,#83823,#83824,
#83825,#83826,#83827,#83828,#83829,#83830,#83831,#83832,#83833,#83834),
(#83835,#83836,#83837,#83838,#83839,#83840,#83841,#83842,#83843,#83844,
#83845,#83846,#83847,#83848,#83849,#83850,#83851,#83852,#83853,#83854,#83855,
#83856,#83857,#83858,#83859,#83860,#83861,#83862,#83863,#83864,#83865,#83866,
#83867,#83868,#83869,#83870,#83871,#83872,#83873,#83874,#83875,#83876,#83877,
#83878,#83879,#83880,#83881,#83882,#83883,#83884,#83885,#83886,#83887,#83888,
#83889,#83890,#83891,#83892,#83893),(#83894,#83895,#83896,#83897,#83898,
#83899,#83900,#83901,#83902,#83903,#83904,#83905,#83906,#83907,#83908,#83909,
#83910,#83911,#83912,#83913,#83914,#83915,#83916,#83917,#83918,#83919,#83920,
#83921,#83922,#83923,#83924,#83925,#83926,#83927,#83928,#83929,#83930,#83931,
#83932,#83933,#83934,#83935,#83936,#83937,#83938,#83939,#83940,#83941,#83942,
#83943,#83944,#83945,#83946,#83947,#83948,#83949,#83950,#83951,#83952),
(#83953,#83954,#83955,#83956,#83957,#83958,#83959,#83960,#83961,#83962,
#83963,#83964,#83965,#83966,#83967,#83968,#83969,#83970,#83971,#83972,#83973,
#83974,#83975,#83976,#83977,#83978,#83979,#83980,#83981,#83982,#83983,#83984,
#83985,#83986,#83987,#83988,#83989,#83990,#83991,#83992,#83993,#83994,#83995,
#83996,#83997,#83998,#83999,#84000,#84001,#84002,#84003,#84004,#84005,#84006,
#84007,#84008,#84009,#84010,#84011)),.UNSPECIFIED.,.F.,.F.,.F.,(4,4),(4,
1,1,1,1,1,1,1,1,1,1,1,1,1,1,1,1,1,1,1,1,1,1,1,1,1,1,1,1,1,1,1,1,1,1,1,1,
1,1,1,1,1,1,1,1,1,1,1,1,1,1,1,1,1,1,1,4),(-0.00050668484467729,0.0332453436260118),
(11.6156899717586,12.6118196458661,13.6076995442317,14.6035794425974,15.599459340963,
16.5953392393287,17.5912191376943,18.58709903606,19.5829789344256,20.5788588327913,
21.5747387311569,22.5706186295226,23.5664985278882,24.5623784262539,25.5582583246196,
26.5541382229852,27.5500181213509,28.5458980197165,29.5417779180822,30.5376578164478,
31.5335377148135,32.5294176131791,33.5252975115448,34.5211774099104,35.5170573082761,
36.5129372066417,37.5088171050074,38.504697003373,39.5005769017387,40.4964568001043,
41.49233669847,42.4882165968357,43.4840964952013,44.479976393567,45.4758562919326,
46.4717361902983,47.4676160886639,48.4634959870296,49.4593758853952,50.4552557837609,
51.4511356821265,52.4470155804922,53.4428954788578,54.4387753772235,55.4346552755891,
56.4305351739548,57.4264150723205,58.4222949706861,59.4181748690518,60.4140547674174,
61.4099346657831,62.4058145641487,63.4016944625144,64.39757436088,65.3934542592457,
66.3893341576113,67.3855077216014),.UNSPECIFIED.);
#611=B_SPLINE_SURFACE_WITH_KNOTS('',3,3,((#105337,#105338,#105339,#105340,
#105341,#105342,#105343,#105344,#105345,#105346,#105347,#105348,#105349,
#105350,#105351,#105352,#105353,#105354,#105355,#105356,#105357,#105358,
#105359,#105360,#105361,#105362,#105363,#105364,#105365,#105366,#105367,
#105368,#105369,#105370,#105371,#105372,#105373,#105374,#105375,#105376,
#105377,#105378,#105379,#105380,#105381,#105382,#105383,#105384,#105385,
#105386,#105387,#105388,#105389,#105390,#105391,#105392,#105393,#105394,
#105395,#105396,#105397,#105398,#105399,#105400,#105401,#105402,#105403,
#105404,#105405,#105406,#105407,#105408,#105409,#105410,#105411,#105412,
#105413,#105414,#105415,#105416,#105417,#105418,#105419,#105420,#105421,
#105422,#105423,#105424,#105425,#105426,#105427,#105428,#105429,#105430,
#105431,#105432,#105433,#105434,#105435,#105436,#105437,#105438,#105439,
#105440,#105441,#105442,#105443,#105444,#105445,#105446,#105447,#105448,
#105449,#105450,#105451,#105452,#105453,#105454,#105455,#105456,#105457,
#105458,#105459,#105460,#105461,#105462,#105463,#105464,#105465,#105466,
#105467,#105468,#105469,#105470,#105471,#105472,#105473,#105474,#105475,
#105476,#105477,#105478,#105479,#105480,#105481,#105482,#105483,#105484,
#105485,#105486,#105487),(#105488,#105489,#105490,#105491,#105492,#105493,
#105494,#105495,#105496,#105497,#105498,#105499,#105500,#105501,#105502,
#105503,#105504,#105505,#105506,#105507,#105508,#105509,#105510,#105511,
#105512,#105513,#105514,#105515,#105516,#105517,#105518,#105519,#105520,
#105521,#105522,#105523,#105524,#105525,#105526,#105527,#105528,#105529,
#105530,#105531,#105532,#105533,#105534,#105535,#105536,#105537,#105538,
#105539,#105540,#105541,#105542,#105543,#105544,#105545,#105546,#105547,
#105548,#105549,#105550,#105551,#105552,#105553,#105554,#105555,#105556,
#105557,#105558,#105559,#105560,#105561,#105562,#105563,#105564,#105565,
#105566,#105567,#105568,#105569,#105570,#105571,#105572,#105573,#105574,
#105575,#105576,#105577,#105578,#105579,#105580,#105581,#105582,#105583,
#105584,#105585,#105586,#105587,#105588,#105589,#105590,#105591,#105592,
#105593,#105594,#105595,#105596,#105597,#105598,#105599,#105600,#105601,
#105602,#105603,#105604,#105605,#105606,#105607,#105608,#105609,#105610,
#105611,#105612,#105613,#105614,#105615,#105616,#105617,#105618,#105619,
#105620,#105621,#105622,#105623,#105624,#105625,#105626,#105627,#105628,
#105629,#105630,#105631,#105632,#105633,#105634,#105635,#105636,#105637,
#105638),(#105639,#105640,#105641,#105642,#105643,#105644,#105645,#105646,
#105647,#105648,#105649,#105650,#105651,#105652,#105653,#105654,#105655,
#105656,#105657,#105658,#105659,#105660,#105661,#105662,#105663,#105664,
#105665,#105666,#105667,#105668,#105669,#105670,#105671,#105672,#105673,
#105674,#105675,#105676,#105677,#105678,#105679,#105680,#105681,#105682,
#105683,#105684,#105685,#105686,#105687,#105688,#105689,#105690,#105691,
#105692,#105693,#105694,#105695,#105696,#105697,#105698,#105699,#105700,
#105701,#105702,#105703,#105704,#105705,#105706,#105707,#105708,#105709,
#105710,#105711,#105712,#105713,#105714,#105715,#105716,#105717,#105718,
#105719,#105720,#105721,#105722,#105723,#105724,#105725,#105726,#105727,
#105728,#105729,#105730,#105731,#105732,#105733,#105734,#105735,#105736,
#105737,#105738,#105739,#105740,#105741,#105742,#105743,#105744,#105745,
#105746,#105747,#105748,#105749,#105750,#105751,#105752,#105753,#105754,
#105755,#105756,#105757,#105758,#105759,#105760,#105761,#105762,#105763,
#105764,#105765,#105766,#105767,#105768,#105769,#105770,#105771,#105772,
#105773,#105774,#105775,#105776,#105777,#105778,#105779,#105780,#105781,
#105782,#105783,#105784,#105785,#105786,#105787,#105788,#105789),(#105790,
#105791,#105792,#105793,#105794,#105795,#105796,#105797,#105798,#105799,
#105800,#105801,#105802,#105803,#105804,#105805,#105806,#105807,#105808,
#105809,#105810,#105811,#105812,#105813,#105814,#105815,#105816,#105817,
#105818,#105819,#105820,#105821,#105822,#105823,#105824,#105825,#105826,
#105827,#105828,#105829,#105830,#105831,#105832,#105833,#105834,#105835,
#105836,#105837,#105838,#105839,#105840,#105841,#105842,#105843,#105844,
#105845,#105846,#105847,#105848,#105849,#105850,#105851,#105852,#105853,
#105854,#105855,#105856,#105857,#105858,#105859,#105860,#105861,#105862,
#105863,#105864,#105865,#105866,#105867,#105868,#105869,#105870,#105871,
#105872,#105873,#105874,#105875,#105876,#105877,#105878,#105879,#105880,
#105881,#105882,#105883,#105884,#105885,#105886,#105887,#105888,#105889,
#105890,#105891,#105892,#105893,#105894,#105895,#105896,#105897,#105898,
#105899,#105900,#105901,#105902,#105903,#105904,#105905,#105906,#105907,
#105908,#105909,#105910,#105911,#105912,#105913,#105914,#105915,#105916,
#105917,#105918,#105919,#105920,#105921,#105922,#105923,#105924,#105925,
#105926,#105927,#105928,#105929,#105930,#105931,#105932,#105933,#105934,
#105935,#105936,#105937,#105938,#105939,#105940)),.UNSPECIFIED.,.F.,.F.,
 .F.,(4,4),(4,1,1,1,1,1,1,1,1,1,1,1,1,1,1,1,1,1,1,1,1,1,1,1,1,1,1,1,1,1,
1,1,1,1,1,1,1,1,1,1,1,1,1,1,1,1,1,1,1,1,1,1,1,1,1,1,1,1,1,1,1,1,1,1,1,1,
1,1,1,1,1,1,1,1,1,1,1,1,1,1,1,1,1,1,1,1,1,1,1,1,1,1,1,1,1,1,1,1,1,1,1,1,
1,1,1,1,1,1,1,1,1,1,1,1,1,1,1,1,1,1,1,1,1,1,1,1,1,1,1,1,1,1,1,1,1,1,1,1,
1,1,1,1,1,1,1,1,1,1,4),(-0.000239926289433817,0.0336233065451596),(8.30175083273572,
9.2967304331541,10.2914247119998,11.2861189908456,12.2808132696913,13.275507548537,
14.2702018273828,15.2648961062285,16.2595903850742,17.2542846639199,18.2489789427657,
19.2436732216114,20.2383675004571,21.2330617793029,22.2277560581486,23.2224503369943,
24.2171446158401,25.2118388946858,26.2065331735315,27.2012274523773,28.195921731223,
29.1906160100687,30.1853102889144,31.1800045677602,32.1746988466059,33.1693931254516,
34.1640874042974,35.1587816831431,36.1534759619888,37.1481702408346,38.1428645196803,
39.137558798526,40.1322530773718,41.1269473562175,42.1216416350632,43.1163359139089,
44.1110301927547,45.1057244716004,46.1004187504461,47.0951130292919,48.0898073081376,
49.0845015869833,50.0791958658291,51.0738901446748,52.0685844235205,53.0632787023663,
54.057972981212,55.0526672600577,56.0473615389035,57.0420558177492,58.0367500965949,
59.0314443754406,60.0261386542864,61.0208329331321,62.0155272119778,63.0102214908236,
64.0049157696693,64.999610048515,65.9943043273608,66.9889986062065,67.9836928850522,
68.978387163898,69.9730814427437,70.9677757215894,71.9624700004351,72.9571642792809,
73.9518585581266,74.9465528369723,75.9412471158181,76.9359413946638,77.9306356735095,
78.9253299523553,79.920024231201,80.9147185100467,81.9094127888925,82.9041070677382,
83.8988013465839,84.8934956254297,85.8881899042754,86.8828841831211,87.8775784619668,
88.8722727408126,89.8669670196583,90.861661298504,91.8563555773498,92.8510498561955,
93.8457441350412,94.840438413887,95.8351326927327,96.8298269715784,97.8245212504242,
98.8192155292699,99.8139098081156,100.808604086961,101.803298365807,102.797992644653,
103.792686923499,104.787381202344,105.78207548119,106.776769760036,107.771464038881,
108.766158317727,109.760852596573,110.755546875419,111.750241154264,112.74493543311,
113.739629711956,114.734323990802,115.729018269647,116.723712548493,117.718406827339,
118.713101106184,119.70779538503,120.702489663876,121.697183942722,122.691878221567,
123.686572500413,124.681266779259,125.675961058105,126.67065533695,127.665349615796,
128.660043894642,129.654738173488,130.649432452333,131.644126731179,132.638821010025,
133.63351528887,134.628209567716,135.622903846562,136.617598125408,137.612292404253,
138.606986683099,139.601680961945,140.596375240791,141.591069519636,142.585763798482,
143.580458077328,144.575152356173,145.569846635019,146.564540913865,147.559235192711,
148.553929471556,149.548623750402,150.543318029248,151.538012308094,152.532706586939,
153.527400865785,154.522095144631,155.517029349766),.UNSPECIFIED.);
#612=B_SPLINE_SURFACE_WITH_KNOTS('',3,3,((#106045,#106046,#106047,#106048,
#106049,#106050,#106051,#106052,#106053,#106054,#106055,#106056,#106057,
#106058,#106059,#106060,#106061,#106062,#106063,#106064,#106065,#106066,
#106067,#106068,#106069,#106070,#106071,#106072,#106073,#106074,#106075,
#106076,#106077,#106078,#106079,#106080,#106081,#106082,#106083,#106084,
#106085,#106086,#106087,#106088,#106089,#106090,#106091,#106092,#106093,
#106094,#106095,#106096,#106097,#106098,#106099,#106100,#106101,#106102,
#106103,#106104,#106105,#106106,#106107,#106108,#106109,#106110,#106111,
#106112,#106113,#106114,#106115,#106116,#106117,#106118,#106119,#106120,
#106121,#106122,#106123,#106124,#106125,#106126,#106127,#106128,#106129,
#106130,#106131,#106132,#106133,#106134,#106135,#106136,#106137,#106138,
#106139,#106140,#106141,#106142,#106143,#106144,#106145,#106146,#106147,
#106148,#106149,#106150,#106151,#106152,#106153,#106154,#106155,#106156,
#106157,#106158,#106159,#106160,#106161,#106162,#106163,#106164,#106165,
#106166,#106167,#106168,#106169,#106170,#106171,#106172,#106173,#106174,
#106175,#106176,#106177,#106178,#106179,#106180,#106181,#106182,#106183,
#106184,#106185,#106186,#106187,#106188,#106189,#106190,#106191,#106192,
#106193,#106194,#106195),(#106196,#106197,#106198,#106199,#106200,#106201,
#106202,#106203,#106204,#106205,#106206,#106207,#106208,#106209,#106210,
#106211,#106212,#106213,#106214,#106215,#106216,#106217,#106218,#106219,
#106220,#106221,#106222,#106223,#106224,#106225,#106226,#106227,#106228,
#106229,#106230,#106231,#106232,#106233,#106234,#106235,#106236,#106237,
#106238,#106239,#106240,#106241,#106242,#106243,#106244,#106245,#106246,
#106247,#106248,#106249,#106250,#106251,#106252,#106253,#106254,#106255,
#106256,#106257,#106258,#106259,#106260,#106261,#106262,#106263,#106264,
#106265,#106266,#106267,#106268,#106269,#106270,#106271,#106272,#106273,
#106274,#106275,#106276,#106277,#106278,#106279,#106280,#106281,#106282,
#106283,#106284,#106285,#106286,#106287,#106288,#106289,#106290,#106291,
#106292,#106293,#106294,#106295,#106296,#106297,#106298,#106299,#106300,
#106301,#106302,#106303,#106304,#106305,#106306,#106307,#106308,#106309,
#106310,#106311,#106312,#106313,#106314,#106315,#106316,#106317,#106318,
#106319,#106320,#106321,#106322,#106323,#106324,#106325,#106326,#106327,
#106328,#106329,#106330,#106331,#106332,#106333,#106334,#106335,#106336,
#106337,#106338,#106339,#106340,#106341,#106342,#106343,#106344,#106345,
#106346),(#106347,#106348,#106349,#106350,#106351,#106352,#106353,#106354,
#106355,#106356,#106357,#106358,#106359,#106360,#106361,#106362,#106363,
#106364,#106365,#106366,#106367,#106368,#106369,#106370,#106371,#106372,
#106373,#106374,#106375,#106376,#106377,#106378,#106379,#106380,#106381,
#106382,#106383,#106384,#106385,#106386,#106387,#106388,#106389,#106390,
#106391,#106392,#106393,#106394,#106395,#106396,#106397,#106398,#106399,
#106400,#106401,#106402,#106403,#106404,#106405,#106406,#106407,#106408,
#106409,#106410,#106411,#106412,#106413,#106414,#106415,#106416,#106417,
#106418,#106419,#106420,#106421,#106422,#106423,#106424,#106425,#106426,
#106427,#106428,#106429,#106430,#106431,#106432,#106433,#106434,#106435,
#106436,#106437,#106438,#106439,#106440,#106441,#106442,#106443,#106444,
#106445,#106446,#106447,#106448,#106449,#106450,#106451,#106452,#106453,
#106454,#106455,#106456,#106457,#106458,#106459,#106460,#106461,#106462,
#106463,#106464,#106465,#106466,#106467,#106468,#106469,#106470,#106471,
#106472,#106473,#106474,#106475,#106476,#106477,#106478,#106479,#106480,
#106481,#106482,#106483,#106484,#106485,#106486,#106487,#106488,#106489,
#106490,#106491,#106492,#106493,#106494,#106495,#106496,#106497),(#106498,
#106499,#106500,#106501,#106502,#106503,#106504,#106505,#106506,#106507,
#106508,#106509,#106510,#106511,#106512,#106513,#106514,#106515,#106516,
#106517,#106518,#106519,#106520,#106521,#106522,#106523,#106524,#106525,
#106526,#106527,#106528,#106529,#106530,#106531,#106532,#106533,#106534,
#106535,#106536,#106537,#106538,#106539,#106540,#106541,#106542,#106543,
#106544,#106545,#106546,#106547,#106548,#106549,#106550,#106551,#106552,
#106553,#106554,#106555,#106556,#106557,#106558,#106559,#106560,#106561,
#106562,#106563,#106564,#106565,#106566,#106567,#106568,#106569,#106570,
#106571,#106572,#106573,#106574,#106575,#106576,#106577,#106578,#106579,
#106580,#106581,#106582,#106583,#106584,#106585,#106586,#106587,#106588,
#106589,#106590,#106591,#106592,#106593,#106594,#106595,#106596,#106597,
#106598,#106599,#106600,#106601,#106602,#106603,#106604,#106605,#106606,
#106607,#106608,#106609,#106610,#106611,#106612,#106613,#106614,#106615,
#106616,#106617,#106618,#106619,#106620,#106621,#106622,#106623,#106624,
#106625,#106626,#106627,#106628,#106629,#106630,#106631,#106632,#106633,
#106634,#106635,#106636,#106637,#106638,#106639,#106640,#106641,#106642,
#106643,#106644,#106645,#106646,#106647,#106648)),.UNSPECIFIED.,.F.,.F.,
 .F.,(4,4),(4,1,1,1,1,1,1,1,1,1,1,1,1,1,1,1,1,1,1,1,1,1,1,1,1,1,1,1,1,1,
1,1,1,1,1,1,1,1,1,1,1,1,1,1,1,1,1,1,1,1,1,1,1,1,1,1,1,1,1,1,1,1,1,1,1,1,
1,1,1,1,1,1,1,1,1,1,1,1,1,1,1,1,1,1,1,1,1,1,1,1,1,1,1,1,1,1,1,1,1,1,1,1,
1,1,1,1,1,1,1,1,1,1,1,1,1,1,1,1,1,1,1,1,1,1,1,1,1,1,1,1,1,1,1,1,1,1,1,1,
1,1,1,1,1,1,1,1,1,1,4),(-0.000616092092482018,0.0332354813107788),(11.6156998340738,
12.6106340263461,13.6053283051919,14.6000225840376,15.5947168628833,16.589411141729,
17.5841054205748,18.5787996994205,19.5734939782662,20.568188257112,21.5628825359577,
22.5575768148034,23.5522710936492,24.5469653724949,25.5416596513406,26.5363539301864,
27.5310482090321,28.5257424878778,29.5204367667235,30.5151310455693,31.509825324415,
32.5045196032607,33.4992138821065,34.4939081609522,35.4886024397979,36.4832967186437,
37.4779909974894,38.4726852763351,39.4673795551809,40.4620738340266,41.4567681128723,
42.4514623917181,43.4461566705638,44.4408509494095,45.4355452282552,46.430239507101,
47.4249337859467,48.4196280647924,49.4143223436382,50.4090166224839,51.4037109013296,
52.3984051801754,53.3930994590211,54.3877937378668,55.3824880167126,56.3771822955583,
57.371876574404,58.3665708532497,59.3612651320955,60.3559594109412,61.3506536897869,
62.3453479686327,63.3400422474784,64.3347365263241,65.3294308051699,66.3241250840156,
67.3188193628613,68.3135136417071,69.3082079205528,70.3029021993985,71.2975964782443,
72.29229075709,73.2869850359357,74.2816793147815,75.2763735936272,76.2710678724729,
77.2657621513186,78.2604564301644,79.2551507090101,80.2498449878558,81.2445392667016,
82.2392335455473,83.233927824393,84.2286221032388,85.2233163820845,86.2180106609302,
87.2127049397759,88.2073992186217,89.2020934974674,90.1967877763131,91.1914820551589,
92.1861763340046,93.1808706128503,94.1755648916961,95.1702591705418,96.1649534493875,
97.1596477282333,98.154342007079,99.1490362859247,100.14373056477,101.138424843616,
102.133119122462,103.127813401308,104.122507680153,105.117201958999,106.111896237845,
107.106590516691,108.101284795536,109.095979074382,110.090673353228,111.085367632073,
112.080061910919,113.074756189765,114.069450468611,115.064144747456,116.058839026302,
117.053533305148,118.048227583994,119.042921862839,120.037616141685,121.032310420531,
122.027004699377,123.021698978222,124.016393257068,125.011087535914,126.005781814759,
127.000476093605,127.995170372451,128.989864651297,129.984558930142,130.979253208988,
131.973947487834,132.96864176668,133.963336045525,134.958030324371,135.952724603217,
136.947418882062,137.942113160908,138.936807439754,139.9315017186,140.926195997445,
141.920890276291,142.915584555137,143.910278833983,144.904973112828,145.899667391674,
146.89436167052,147.889055949366,148.883750228211,149.878444507057,150.873138785903,
151.867833064748,152.862527343594,153.85722162244,154.851915901286,155.846610180131,
156.841304458977,157.835998737823,158.831090341195),.UNSPECIFIED.);
#613=B_SPLINE_SURFACE_WITH_KNOTS('',3,3,((#124738,#124739,#124740,#124741,
#124742,#124743,#124744,#124745,#124746,#124747,#124748,#124749,#124750,
#124751,#124752,#124753,#124754,#124755,#124756,#124757,#124758,#124759,
#124760,#124761,#124762,#124763,#124764,#124765,#124766,#124767,#124768,
#124769,#124770,#124771,#124772,#124773,#124774,#124775,#124776,#124777,
#124778,#124779,#124780,#124781,#124782,#124783,#124784,#124785,#124786,
#124787,#124788,#124789,#124790,#124791,#124792,#124793,#124794,#124795,
#124796,#124797,#124798,#124799,#124800,#124801,#124802,#124803,#124804,
#124805,#124806,#124807,#124808,#124809,#124810,#124811,#124812,#124813,
#124814,#124815,#124816,#124817,#124818,#124819,#124820,#124821,#124822,
#124823,#124824,#124825,#124826,#124827,#124828,#124829,#124830,#124831,
#124832,#124833,#124834,#124835,#124836,#124837,#124838,#124839,#124840,
#124841,#124842,#124843,#124844,#124845,#124846,#124847,#124848,#124849,
#124850,#124851,#124852,#124853,#124854,#124855,#124856,#124857,#124858,
#124859,#124860,#124861,#124862,#124863),(#124864,#124865,#124866,#124867,
#124868,#124869,#124870,#124871,#124872,#124873,#124874,#124875,#124876,
#124877,#124878,#124879,#124880,#124881,#124882,#124883,#124884,#124885,
#124886,#124887,#124888,#124889,#124890,#124891,#124892,#124893,#124894,
#124895,#124896,#124897,#124898,#124899,#124900,#124901,#124902,#124903,
#124904,#124905,#124906,#124907,#124908,#124909,#124910,#124911,#124912,
#124913,#124914,#124915,#124916,#124917,#124918,#124919,#124920,#124921,
#124922,#124923,#124924,#124925,#124926,#124927,#124928,#124929,#124930,
#124931,#124932,#124933,#124934,#124935,#124936,#124937,#124938,#124939,
#124940,#124941,#124942,#124943,#124944,#124945,#124946,#124947,#124948,
#124949,#124950,#124951,#124952,#124953,#124954,#124955,#124956,#124957,
#124958,#124959,#124960,#124961,#124962,#124963,#124964,#124965,#124966,
#124967,#124968,#124969,#124970,#124971,#124972,#124973,#124974,#124975,
#124976,#124977,#124978,#124979,#124980,#124981,#124982,#124983,#124984,
#124985,#124986,#124987,#124988,#124989),(#124990,#124991,#124992,#124993,
#124994,#124995,#124996,#124997,#124998,#124999,#125000,#125001,#125002,
#125003,#125004,#125005,#125006,#125007,#125008,#125009,#125010,#125011,
#125012,#125013,#125014,#125015,#125016,#125017,#125018,#125019,#125020,
#125021,#125022,#125023,#125024,#125025,#125026,#125027,#125028,#125029,
#125030,#125031,#125032,#125033,#125034,#125035,#125036,#125037,#125038,
#125039,#125040,#125041,#125042,#125043,#125044,#125045,#125046,#125047,
#125048,#125049,#125050,#125051,#125052,#125053,#125054,#125055,#125056,
#125057,#125058,#125059,#125060,#125061,#125062,#125063,#125064,#125065,
#125066,#125067,#125068,#125069,#125070,#125071,#125072,#125073,#125074,
#125075,#125076,#125077,#125078,#125079,#125080,#125081,#125082,#125083,
#125084,#125085,#125086,#125087,#125088,#125089,#125090,#125091,#125092,
#125093,#125094,#125095,#125096,#125097,#125098,#125099,#125100,#125101,
#125102,#125103,#125104,#125105,#125106,#125107,#125108,#125109,#125110,
#125111,#125112,#125113,#125114,#125115),(#125116,#125117,#125118,#125119,
#125120,#125121,#125122,#125123,#125124,#125125,#125126,#125127,#125128,
#125129,#125130,#125131,#125132,#125133,#125134,#125135,#125136,#125137,
#125138,#125139,#125140,#125141,#125142,#125143,#125144,#125145,#125146,
#125147,#125148,#125149,#125150,#125151,#125152,#125153,#125154,#125155,
#125156,#125157,#125158,#125159,#125160,#125161,#125162,#125163,#125164,
#125165,#125166,#125167,#125168,#125169,#125170,#125171,#125172,#125173,
#125174,#125175,#125176,#125177,#125178,#125179,#125180,#125181,#125182,
#125183,#125184,#125185,#125186,#125187,#125188,#125189,#125190,#125191,
#125192,#125193,#125194,#125195,#125196,#125197,#125198,#125199,#125200,
#125201,#125202,#125203,#125204,#125205,#125206,#125207,#125208,#125209,
#125210,#125211,#125212,#125213,#125214,#125215,#125216,#125217,#125218,
#125219,#125220,#125221,#125222,#125223,#125224,#125225,#125226,#125227,
#125228,#125229,#125230,#125231,#125232,#125233,#125234,#125235,#125236,
#125237,#125238,#125239,#125240,#125241)),.UNSPECIFIED.,.F.,.F.,.F.,(4,
4),(4,1,1,1,1,1,1,1,1,1,1,1,1,1,1,1,1,1,1,1,1,1,1,1,1,1,1,1,1,1,1,1,1,1,
1,1,1,1,1,1,1,1,1,1,1,1,1,1,1,1,1,1,1,1,1,1,1,1,1,1,1,1,1,1,1,1,1,1,1,1,
1,1,1,1,1,1,1,1,1,1,1,1,1,1,1,1,1,1,1,1,1,1,1,1,1,1,1,1,1,1,1,1,1,1,1,1,
1,1,1,1,1,1,1,1,1,1,1,1,1,1,1,1,1,4),(-0.000237865095396134,0.0336171964829504),
(8.30175323816384,9.29457283756397,10.2871095208197,11.2796462040753,12.272182887331,
13.2647195705867,14.2572562538424,15.2497929370981,16.2423296203538,17.2348663036095,
18.2274029868652,19.2199396701209,20.2124763533766,21.2050130366322,22.1975497198879,
23.1900864031436,24.1826230863993,25.175159769655,26.1676964529107,27.1602331361664,
28.1527698194221,29.1453065026778,30.1378431859334,31.1303798691891,32.1229165524448,
33.1154532357005,34.1079899189562,35.1005266022119,36.0930632854676,37.0855999687233,
38.078136651979,39.0706733352347,40.0632100184903,41.055746701746,42.0482833850017,
43.0408200682574,44.0333567515131,45.0258934347688,46.0184301180245,47.0109668012802,
48.0035034845359,48.9960401677916,49.9885768510472,50.9811135343029,51.9736502175586,
52.9661869008143,53.95872358407,54.9512602673257,55.9437969505814,56.9363336338371,
57.9288703170928,58.9214070003484,59.9139436836041,60.9064803668598,61.8990170501155,
62.8915537333712,63.8840904166269,64.8766270998826,65.8691637831383,66.861700466394,
67.8542371496497,68.8467738329053,69.839310516161,70.8318471994167,71.8243838826724,
72.8169205659281,73.8094572491838,74.8019939324395,75.7945306156952,76.7870672989509,
77.7796039822065,78.7721406654622,79.7646773487179,80.7572140319736,81.7497507152293,
82.742287398485,83.7348240817407,84.7273607649964,85.7198974482521,86.7124341315078,
87.7049708147634,88.6975074980191,89.6900441812748,90.6825808645305,91.6751175477862,
92.6676542310419,93.6601909142976,94.6527275975533,95.645264280809,96.6378009640647,
97.6303376473203,98.622874330576,99.6154110138317,100.607947697087,101.600484380343,
102.593021063599,103.585557746854,104.57809443011,105.570631113366,106.563167796622,
107.555704479877,108.548241163133,109.540777846389,110.533314529644,111.5258512129,
112.518387896156,113.510924579411,114.503461262667,115.495997945923,116.488534629178,
117.481071312434,118.47360799569,119.466144678946,120.458681362201,121.451218045457,
122.443754728713,123.436291411968,124.428828095224,125.42136477848,126.413901461735,
127.406438144991,128.398974828247,129.391511511502,130.384286059853),
 .UNSPECIFIED.);
#614=B_SPLINE_SURFACE_WITH_KNOTS('',3,3,((#125425,#125426,#125427,#125428,
#125429,#125430,#125431,#125432,#125433,#125434,#125435,#125436,#125437,
#125438,#125439,#125440,#125441,#125442,#125443,#125444,#125445,#125446,
#125447,#125448,#125449,#125450,#125451,#125452,#125453,#125454,#125455,
#125456,#125457,#125458,#125459,#125460,#125461,#125462,#125463,#125464,
#125465,#125466,#125467,#125468,#125469,#125470,#125471,#125472,#125473,
#125474,#125475,#125476,#125477,#125478,#125479,#125480,#125481,#125482,
#125483,#125484,#125485,#125486,#125487,#125488,#125489,#125490,#125491,
#125492,#125493,#125494,#125495,#125496,#125497,#125498,#125499,#125500,
#125501,#125502,#125503,#125504,#125505,#125506,#125507,#125508,#125509,
#125510,#125511,#125512,#125513,#125514,#125515,#125516,#125517,#125518,
#125519,#125520,#125521,#125522,#125523,#125524,#125525,#125526,#125527,
#125528,#125529,#125530,#125531,#125532,#125533,#125534,#125535,#125536,
#125537,#125538,#125539,#125540,#125541,#125542,#125543,#125544,#125545,
#125546,#125547,#125548,#125549,#125550),(#125551,#125552,#125553,#125554,
#125555,#125556,#125557,#125558,#125559,#125560,#125561,#125562,#125563,
#125564,#125565,#125566,#125567,#125568,#125569,#125570,#125571,#125572,
#125573,#125574,#125575,#125576,#125577,#125578,#125579,#125580,#125581,
#125582,#125583,#125584,#125585,#125586,#125587,#125588,#125589,#125590,
#125591,#125592,#125593,#125594,#125595,#125596,#125597,#125598,#125599,
#125600,#125601,#125602,#125603,#125604,#125605,#125606,#125607,#125608,
#125609,#125610,#125611,#125612,#125613,#125614,#125615,#125616,#125617,
#125618,#125619,#125620,#125621,#125622,#125623,#125624,#125625,#125626,
#125627,#125628,#125629,#125630,#125631,#125632,#125633,#125634,#125635,
#125636,#125637,#125638,#125639,#125640,#125641,#125642,#125643,#125644,
#125645,#125646,#125647,#125648,#125649,#125650,#125651,#125652,#125653,
#125654,#125655,#125656,#125657,#125658,#125659,#125660,#125661,#125662,
#125663,#125664,#125665,#125666,#125667,#125668,#125669,#125670,#125671,
#125672,#125673,#125674,#125675,#125676),(#125677,#125678,#125679,#125680,
#125681,#125682,#125683,#125684,#125685,#125686,#125687,#125688,#125689,
#125690,#125691,#125692,#125693,#125694,#125695,#125696,#125697,#125698,
#125699,#125700,#125701,#125702,#125703,#125704,#125705,#125706,#125707,
#125708,#125709,#125710,#125711,#125712,#125713,#125714,#125715,#125716,
#125717,#125718,#125719,#125720,#125721,#125722,#125723,#125724,#125725,
#125726,#125727,#125728,#125729,#125730,#125731,#125732,#125733,#125734,
#125735,#125736,#125737,#125738,#125739,#125740,#125741,#125742,#125743,
#125744,#125745,#125746,#125747,#125748,#125749,#125750,#125751,#125752,
#125753,#125754,#125755,#125756,#125757,#125758,#125759,#125760,#125761,
#125762,#125763,#125764,#125765,#125766,#125767,#125768,#125769,#125770,
#125771,#125772,#125773,#125774,#125775,#125776,#125777,#125778,#125779,
#125780,#125781,#125782,#125783,#125784,#125785,#125786,#125787,#125788,
#125789,#125790,#125791,#125792,#125793,#125794,#125795,#125796,#125797,
#125798,#125799,#125800,#125801,#125802),(#125803,#125804,#125805,#125806,
#125807,#125808,#125809,#125810,#125811,#125812,#125813,#125814,#125815,
#125816,#125817,#125818,#125819,#125820,#125821,#125822,#125823,#125824,
#125825,#125826,#125827,#125828,#125829,#125830,#125831,#125832,#125833,
#125834,#125835,#125836,#125837,#125838,#125839,#125840,#125841,#125842,
#125843,#125844,#125845,#125846,#125847,#125848,#125849,#125850,#125851,
#125852,#125853,#125854,#125855,#125856,#125857,#125858,#125859,#125860,
#125861,#125862,#125863,#125864,#125865,#125866,#125867,#125868,#125869,
#125870,#125871,#125872,#125873,#125874,#125875,#125876,#125877,#125878,
#125879,#125880,#125881,#125882,#125883,#125884,#125885,#125886,#125887,
#125888,#125889,#125890,#125891,#125892,#125893,#125894,#125895,#125896,
#125897,#125898,#125899,#125900,#125901,#125902,#125903,#125904,#125905,
#125906,#125907,#125908,#125909,#125910,#125911,#125912,#125913,#125914,
#125915,#125916,#125917,#125918,#125919,#125920,#125921,#125922,#125923,
#125924,#125925,#125926,#125927,#125928)),.UNSPECIFIED.,.F.,.F.,.F.,(4,
4),(4,1,1,1,1,1,1,1,1,1,1,1,1,1,1,1,1,1,1,1,1,1,1,1,1,1,1,1,1,1,1,1,1,1,
1,1,1,1,1,1,1,1,1,1,1,1,1,1,1,1,1,1,1,1,1,1,1,1,1,1,1,1,1,1,1,1,1,1,1,1,
1,1,1,1,1,1,1,1,1,1,1,1,1,1,1,1,1,1,1,1,1,1,1,1,1,1,1,1,1,1,1,1,1,1,1,1,
1,1,1,1,1,1,1,1,1,1,1,1,1,1,1,1,1,4),(-0.000612126754026731,0.033233417622924),
(11.6157018977616,12.608476430756,13.6010131140117,14.5935497972674,15.5860864805231,
16.5786231637787,17.5711598470344,18.5636965302901,19.5562332135458,20.5487698968015,
21.5413065800572,22.5338432633129,23.5263799465686,24.5189166298243,25.51145331308,
26.5039899963356,27.4965266795913,28.489063362847,29.4816000461027,30.4741367293584,
31.4666734126141,32.4592100958698,33.4517467791255,34.4442834623812,35.4368201456369,
36.4293568288925,37.4218935121482,38.4144301954039,39.4069668786596,40.3995035619153,
41.392040245171,42.3845769284267,43.3771136116824,44.3696502949381,45.3621869781938,
46.3547236614494,47.3472603447051,48.3397970279608,49.3323337112165,50.3248703944722,
51.3174070777279,52.3099437609836,53.3024804442393,54.295017127495,55.2875538107507,
56.2800904940063,57.272627177262,58.2651638605177,59.2577005437734,60.2502372270291,
61.2427739102848,62.2353105935405,63.2278472767962,64.2203839600519,65.2129206433076,
66.2054573265632,67.1979940098189,68.1905306930746,69.1830673763303,70.175604059586,
71.1681407428417,72.1606774260974,73.1532141093531,74.1457507926088,75.1382874758644,
76.1308241591201,77.1233608423758,78.1158975256315,79.1084342088872,80.1009708921429,
81.0935075753986,82.0860442586543,83.07858094191,84.0711176251657,85.0636543084213,
86.056190991677,87.0487276749327,88.0412643581884,89.0338010414441,90.0263377246998,
91.0188744079555,92.0114110912112,93.0039477744669,93.9964844577226,94.9890211409783,
95.9815578242339,96.9740945074896,97.9666311907453,98.959167874001,99.9517045572567,
100.944241240512,101.936777923768,102.929314607024,103.921851290279,104.914387973535,
105.906924656791,106.899461340047,107.891998023302,108.884534706558,109.877071389814,
110.869608073069,111.862144756325,112.854681439581,113.847218122836,114.839754806092,
115.832291489348,116.824828172603,117.817364855859,118.809901539115,119.80243822237,
120.794974905626,121.787511588882,122.780048272138,123.772584955393,124.765121638649,
125.757658321905,126.75019500516,127.742731688416,128.735268371672,129.727805054927,
130.720341738183,131.712878421439,132.705415104694,133.698346948047),
 .UNSPECIFIED.);
#615=B_SPLINE_SURFACE_WITH_KNOTS('',3,3,((#134384,#134385,#134386,#134387,
#134388,#134389,#134390,#134391,#134392,#134393,#134394,#134395,#134396,
#134397,#134398,#134399,#134400,#134401,#134402,#134403,#134404,#134405,
#134406,#134407,#134408,#134409,#134410,#134411,#134412,#134413,#134414,
#134415,#134416,#134417,#134418,#134419,#134420,#134421,#134422,#134423,
#134424,#134425,#134426,#134427,#134428,#134429,#134430,#134431,#134432,
#134433,#134434,#134435,#134436,#134437,#134438,#134439,#134440,#134441,
#134442,#134443,#134444,#134445,#134446,#134447,#134448,#134449,#134450,
#134451,#134452,#134453,#134454,#134455),(#134456,#134457,#134458,#134459,
#134460,#134461,#134462,#134463,#134464,#134465,#134466,#134467,#134468,
#134469,#134470,#134471,#134472,#134473,#134474,#134475,#134476,#134477,
#134478,#134479,#134480,#134481,#134482,#134483,#134484,#134485,#134486,
#134487,#134488,#134489,#134490,#134491,#134492,#134493,#134494,#134495,
#134496,#134497,#134498,#134499,#134500,#134501,#134502,#134503,#134504,
#134505,#134506,#134507,#134508,#134509,#134510,#134511,#134512,#134513,
#134514,#134515,#134516,#134517,#134518,#134519,#134520,#134521,#134522,
#134523,#134524,#134525,#134526,#134527),(#134528,#134529,#134530,#134531,
#134532,#134533,#134534,#134535,#134536,#134537,#134538,#134539,#134540,
#134541,#134542,#134543,#134544,#134545,#134546,#134547,#134548,#134549,
#134550,#134551,#134552,#134553,#134554,#134555,#134556,#134557,#134558,
#134559,#134560,#134561,#134562,#134563,#134564,#134565,#134566,#134567,
#134568,#134569,#134570,#134571,#134572,#134573,#134574,#134575,#134576,
#134577,#134578,#134579,#134580,#134581,#134582,#134583,#134584,#134585,
#134586,#134587,#134588,#134589,#134590,#134591,#134592,#134593,#134594,
#134595,#134596,#134597,#134598,#134599),(#134600,#134601,#134602,#134603,
#134604,#134605,#134606,#134607,#134608,#134609,#134610,#134611,#134612,
#134613,#134614,#134615,#134616,#134617,#134618,#134619,#134620,#134621,
#134622,#134623,#134624,#134625,#134626,#134627,#134628,#134629,#134630,
#134631,#134632,#134633,#134634,#134635,#134636,#134637,#134638,#134639,
#134640,#134641,#134642,#134643,#134644,#134645,#134646,#134647,#134648,
#134649,#134650,#134651,#134652,#134653,#134654,#134655,#134656,#134657,
#134658,#134659,#134660,#134661,#134662,#134663,#134664,#134665,#134666,
#134667,#134668,#134669,#134670,#134671)),.UNSPECIFIED.,.F.,.F.,.F.,(4,
4),(4,1,1,1,1,1,1,1,1,1,1,1,1,1,1,1,1,1,1,1,1,1,1,1,1,1,1,1,1,1,1,1,1,1,
1,1,1,1,1,1,1,1,1,1,1,1,1,1,1,1,1,1,1,1,1,1,1,1,1,1,1,1,1,1,1,1,1,1,1,4),
(-0.000148463654747345,0.0266708891660514),(8.30910520973557,9.29917567257901,
10.2890599933927,11.2789443142064,12.2688286350201,13.2587129558338,14.2485972766475,
15.2384815974612,16.2283659182749,17.2182502390886,18.2081345599023,19.198018880716,
20.1879032015297,21.1777875223434,22.1676718431571,23.1575561639708,24.1474404847846,
25.1373248055983,26.127209126412,27.1170934472257,28.1069777680394,29.0968620888531,
30.0867464096668,31.0766307304805,32.0665150512942,33.0563993721079,34.0462836929216,
35.0361680137353,36.026052334549,37.0159366553627,38.0058209761764,38.9957052969901,
39.9855896178038,40.9754739386175,41.9653582594312,42.9552425802449,43.9451269010586,
44.9350112218723,45.924895542686,46.9147798634997,47.9046641843134,48.8945485051271,
49.8844328259408,50.8743171467545,51.8642014675682,52.8540857883819,53.8439701091956,
54.8338544300093,55.823738750823,56.8136230716368,57.8035073924505,58.7933917132642,
59.7832760340779,60.7731603548916,61.7630446757053,62.752928996519,63.7428133173327,
64.7326976381464,65.7225819589601,66.7124662797738,67.7023506005875,68.6922349214012,
69.6821192422149,70.6720035630286,71.6618878838423,72.651772204656,73.6416565254697,
74.6315408462834,75.6214251670971,76.6114579515656),.UNSPECIFIED.);
#616=B_SPLINE_SURFACE_WITH_KNOTS('',3,3,((#134879,#134880,#134881,#134882,
#134883,#134884,#134885,#134886,#134887,#134888,#134889,#134890,#134891,
#134892,#134893,#134894,#134895,#134896,#134897,#134898,#134899,#134900,
#134901,#134902,#134903,#134904,#134905,#134906,#134907,#134908,#134909,
#134910,#134911,#134912,#134913,#134914,#134915,#134916,#134917,#134918,
#134919,#134920,#134921,#134922,#134923,#134924,#134925,#134926,#134927,
#134928,#134929,#134930,#134931,#134932,#134933,#134934,#134935,#134936,
#134937,#134938,#134939,#134940,#134941,#134942,#134943,#134944,#134945,
#134946,#134947,#134948),(#134949,#134950,#134951,#134952,#134953,#134954,
#134955,#134956,#134957,#134958,#134959,#134960,#134961,#134962,#134963,
#134964,#134965,#134966,#134967,#134968,#134969,#134970,#134971,#134972,
#134973,#134974,#134975,#134976,#134977,#134978,#134979,#134980,#134981,
#134982,#134983,#134984,#134985,#134986,#134987,#134988,#134989,#134990,
#134991,#134992,#134993,#134994,#134995,#134996,#134997,#134998,#134999,
#135000,#135001,#135002,#135003,#135004,#135005,#135006,#135007,#135008,
#135009,#135010,#135011,#135012,#135013,#135014,#135015,#135016,#135017,
#135018),(#135019,#135020,#135021,#135022,#135023,#135024,#135025,#135026,
#135027,#135028,#135029,#135030,#135031,#135032,#135033,#135034,#135035,
#135036,#135037,#135038,#135039,#135040,#135041,#135042,#135043,#135044,
#135045,#135046,#135047,#135048,#135049,#135050,#135051,#135052,#135053,
#135054,#135055,#135056,#135057,#135058,#135059,#135060,#135061,#135062,
#135063,#135064,#135065,#135066,#135067,#135068,#135069,#135070,#135071,
#135072,#135073,#135074,#135075,#135076,#135077,#135078,#135079,#135080,
#135081,#135082,#135083,#135084,#135085,#135086,#135087,#135088),(#135089,
#135090,#135091,#135092,#135093,#135094,#135095,#135096,#135097,#135098,
#135099,#135100,#135101,#135102,#135103,#135104,#135105,#135106,#135107,
#135108,#135109,#135110,#135111,#135112,#135113,#135114,#135115,#135116,
#135117,#135118,#135119,#135120,#135121,#135122,#135123,#135124,#135125,
#135126,#135127,#135128,#135129,#135130,#135131,#135132,#135133,#135134,
#135135,#135136,#135137,#135138,#135139,#135140,#135141,#135142,#135143,
#135144,#135145,#135146,#135147,#135148,#135149,#135150,#135151,#135152,
#135153,#135154,#135155,#135156,#135157,#135158)),.UNSPECIFIED.,.F.,.F.,
 .F.,(4,4),(4,1,1,1,1,1,1,1,1,1,1,1,1,1,1,1,1,1,1,1,1,1,1,1,1,1,1,1,1,1,
1,1,1,1,1,1,1,1,1,1,1,1,1,1,1,1,1,1,1,1,1,1,1,1,1,1,1,1,1,1,1,1,1,1,1,1,
1,4),(-0.000394127981503626,0.0264020341717739),(13.6815980460861,14.6704625085889,
15.6590677938146,16.6476730790403,17.6362783642661,18.6248836494918,19.6134889347175,
20.6020942199433,21.590699505169,22.5793047903947,23.5679100756204,24.5565153608462,
25.5451206460719,26.5337259312976,27.5223312165234,28.5109365017491,29.4995417869748,
30.4881470722005,31.4767523574263,32.465357642652,33.4539629278777,34.4425682131035,
35.4311734983292,36.4197787835549,37.4083840687806,38.3969893540064,39.3855946392321,
40.3741999244578,41.3628052096836,42.3514104949093,43.340015780135,44.3286210653607,
45.3172263505865,46.3058316358122,47.2944369210379,48.2830422062637,49.2716474914894,
50.2602527767151,51.2488580619408,52.2374633471666,53.2260686323923,54.214673917618,
55.2032792028438,56.1918844880695,57.1804897732952,58.1690950585209,59.1577003437467,
60.1463056289724,61.1349109141981,62.1235161994239,63.1121214846496,64.1007267698753,
65.089332055101,66.0779373403268,67.0665426255525,68.0551479107782,69.0437531960039,
70.0323584812297,71.0209637664554,72.0095690516811,72.9981743369069,73.9867796221326,
74.9753849073583,75.963990192584,76.9525954778098,77.9412007630355,78.9298060482612,
79.9185965318092),.UNSPECIFIED.);
#617=B_SPLINE_CURVE_WITH_KNOTS('',3,(#41522,#41523,#41524,#41525,#41526,
#41527,#41528,#41529,#41530,#41531,#41532,#41533,#41534,#41535,#41536,#41537,
#41538,#41539,#41540,#41541,#41542,#41543),.UNSPECIFIED.,.F.,.F.,(4,2,2,
2,2,2,2,2,2,2,4),(3.73107638342163E-6,0.0506459089674672,0.103371892378906,
0.203995846997698,0.297723322628345,0.347133425087129,0.435556350263891,
0.482653331242677,0.583240346238036,0.640653178327547,0.694267771013001),
 .UNSPECIFIED.);
#618=B_SPLINE_CURVE_WITH_KNOTS('',3,(#41545,#41546,#41547,#41548,#41549,
#41550,#41551,#41552,#41553,#41554,#41555,#41556,#41557,#41558,#41559,#41560,
#41561,#41562,#41563,#41564,#41565,#41566,#41567,#41568,#41569,#41570,#41571,
#41572,#41573,#41574,#41575,#41576,#41577,#41578,#41579,#41580,#41581,#41582,
#41583,#41584,#41585,#41586,#41587,#41588,#41589,#41590,#41591,#41592,#41593,
#41594,#41595,#41596,#41597,#41598,#41599,#41600,#41601,#41602,#41603,#41604,
#41605,#41606,#41607,#41608,#41609,#41610,#41611,#41612,#41613,#41614,#41615,
#41616,#41617,#41618,#41619,#41620,#41621,#41622,#41623,#41624,#41625,#41626,
#41627,#41628,#41629,#41630,#41631,#41632,#41633,#41634,#41635,#41636,#41637,
#41638,#41639,#41640,#41641,#41642,#41643,#41644,#41645,#41646,#41647,#41648,
#41649,#41650,#41651,#41652,#41653,#41654,#41655,#41656,#41657,#41658,#41659,
#41660,#41661,#41662,#41663,#41664,#41665,#41666,#41667,#41668,#41669,#41670,
#41671,#41672,#41673,#41674,#41675,#41676,#41677,#41678,#41679,#41680,#41681,
#41682,#41683,#41684,#41685,#41686,#41687,#41688,#41689,#41690,#41691,#41692,
#41693,#41694,#41695,#41696,#41697,#41698,#41699,#41700,#41701,#41702,#41703,
#41704,#41705,#41706,#41707,#41708,#41709,#41710,#41711,#41712,#41713,#41714,
#41715,#41716,#41717,#41718,#41719,#41720,#41721,#41722,#41723,#41724,#41725,
#41726,#41727,#41728,#41729,#41730,#41731,#41732,#41733,#41734,#41735,#41736,
#41737),.UNSPECIFIED.,.F.,.F.,(4,3,3,3,3,3,3,3,3,3,3,3,3,3,3,3,3,3,3,3,
3,3,3,3,3,3,3,3,3,3,3,3,3,3,3,3,3,3,3,3,3,3,3,3,3,3,3,3,3,3,3,3,3,3,3,3,
3,3,3,3,3,3,3,3,4),(0.00234954353479144,0.00310318921645473,0.0088582021338961,
0.00930481001264915,0.0216886296499449,0.0485537357742967,0.0600476559819482,
0.060077834493807,0.0708153993107394,0.0973229488478452,0.124174207582929,
0.150994548134737,0.168411939510706,0.173195847105295,0.173221725606229,
0.199629661690922,0.226438379404894,0.25331614970675,0.266220462053855,
0.286347834381452,0.286367093094366,0.312947470961036,0.339878442731592,
0.36419063552826,0.389390727847281,0.391018387762494,0.39951577415484,0.399520049495332,
0.426183119512092,0.453091259603804,0.46236150068436,0.489208228107559,
0.51267181785655,0.51268691960903,0.539532286181883,0.560782471473938,0.569211298980254,
0.569234438523911,0.595920151049213,0.621412765585973,0.622860168004852,
0.625813142893821,0.625848336448634,0.651175201287267,0.652699670111354,
0.659399028042767,0.686003429405952,0.712970949013868,0.738935139746066,
0.738982748431222,0.758164277735553,0.784631050256268,0.795443012593489,
0.795492931537947,0.819715584311038,0.823762057603835,0.823813147482631,
0.837908125570947,0.837958543617086,0.852030564169489,0.852083643327173,
0.85713132501906,0.880252976771596,0.883475761569799,0.894414923079292),
 .UNSPECIFIED.);
#619=B_SPLINE_CURVE_WITH_KNOTS('',3,(#41741,#41742,#41743,#41744,#41745,
#41746,#41747,#41748,#41749,#41750,#41751,#41752),.UNSPECIFIED.,.F.,.F.,
(4,2,2,2,2,4),(4.14401685134791,4.23919981484122,4.3234021788811,4.42503338177172,
4.48178100258938,4.53126296388924),.UNSPECIFIED.);
#620=B_SPLINE_CURVE_WITH_KNOTS('',3,(#41754,#41755,#41756,#41757,#41758,
#41759,#41760,#41761,#41762,#41763,#41764,#41765,#41766,#41767,#41768,#41769,
#41770,#41771,#41772,#41773,#41774,#41775,#41776,#41777,#41778,#41779,#41780,
#41781,#41782,#41783,#41784,#41785,#41786,#41787,#41788,#41789,#41790,#41791,
#41792,#41793,#41794,#41795,#41796,#41797,#41798,#41799,#41800,#41801,#41802,
#41803,#41804,#41805),.UNSPECIFIED.,.F.,.F.,(4,3,3,3,3,3,3,3,3,3,3,3,3,
3,3,3,3,4),(0.,0.0262870680174327,0.0526250957989455,0.0784797815042996,
0.10063173188014,0.101346503493714,0.123864269870963,0.146327018657836,
0.168872293830273,0.19141756900271,0.210943942314893,0.216050596552535,
0.240087946409699,0.253454166228182,0.27404349701453,0.294365188295977,
0.314525566744571,0.330523895440752),.UNSPECIFIED.);
#621=B_SPLINE_CURVE_WITH_KNOTS('',3,(#41808,#41809,#41810,#41811,#41812,
#41813,#41814,#41815,#41816,#41817,#41818,#41819,#41820,#41821,#41822,#41823,
#41824,#41825,#41826,#41827,#41828,#41829,#41830,#41831),.UNSPECIFIED.,
 .F.,.F.,(4,2,2,2,2,2,2,2,2,2,2,4),(2.73904782886837E-12,0.0817234061279085,
0.161552425644965,0.261638330253269,0.309328561956691,0.356314225569715,
0.402118903800116,0.477843813243927,0.569451511760358,0.604233221463172,
0.659917854360184,0.712631531767947),.UNSPECIFIED.);
#622=B_SPLINE_CURVE_WITH_KNOTS('',3,(#41836,#41837,#41838,#41839,#41840,
#41841,#41842,#41843,#41844,#41845,#41846,#41847,#41848,#41849,#41850,#41851,
#41852,#41853,#41854,#41855,#41856,#41857,#41858,#41859,#41860,#41861,#41862,
#41863,#41864,#41865,#41866,#41867,#41868,#41869,#41870,#41871,#41872,#41873,
#41874,#41875,#41876,#41877,#41878,#41879),.UNSPECIFIED.,.F.,.F.,(4,2,2,
2,2,2,2,2,2,2,2,2,2,2,2,2,2,2,2,2,2,4),(2.54700836416053,2.55527047039645,
2.6186560390472,2.6731150077874,2.76356237393918,2.86595286652909,2.96144125756534,
3.00742527171164,3.09922332533053,3.18621856024237,3.28775374837671,3.37402791853298,
3.47553035070879,3.51982920681099,3.56755802727897,3.66929833501538,3.76265070549564,
3.8643160955509,3.95044192085268,4.05174321628903,4.13710175052906,4.14401685134791),
 .UNSPECIFIED.);
#623=B_SPLINE_CURVE_WITH_KNOTS('',3,(#41881,#41882,#41883,#41884,#41885,
#41886,#41887,#41888,#41889,#41890,#41891,#41892,#41893,#41894,#41895,#41896,
#41897,#41898,#41899,#41900,#41901,#41902),.UNSPECIFIED.,.F.,.F.,(4,2,2,
2,2,2,2,2,2,2,4),(1.78915403369814E-6,0.0868924796927673,0.160732517221174,
0.248846661449348,0.346410911703831,0.431051162846719,0.524867255149695,
0.613111647621759,0.713356525426838,0.790010811238862,0.862101243151681),
 .UNSPECIFIED.);
#624=B_SPLINE_CURVE_WITH_KNOTS('',3,(#41903,#41904,#41905,#41906,#41907,
#41908,#41909,#41910,#41911,#41912,#41913,#41914,#41915,#41916,#41917,#41918,
#41919,#41920,#41921,#41922,#41923,#41924,#41925,#41926,#41927,#41928,#41929,
#41930,#41931,#41932,#41933,#41934,#41935,#41936,#41937,#41938,#41939,#41940,
#41941,#41942,#41943,#41944,#41945,#41946,#41947,#41948,#41949,#41950,#41951,
#41952,#41953,#41954,#41955,#41956,#41957,#41958,#41959,#41960,#41961,#41962,
#41963,#41964,#41965,#41966,#41967,#41968,#41969,#41970,#41971,#41972,#41973,
#41974,#41975,#41976,#41977,#41978,#41979,#41980,#41981,#41982,#41983,#41984,
#41985,#41986,#41987,#41988,#41989,#41990,#41991,#41992,#41993,#41994,#41995,
#41996,#41997,#41998,#41999,#42000,#42001,#42002,#42003,#42004,#42005,#42006,
#42007,#42008,#42009,#42010,#42011,#42012,#42013,#42014,#42015,#42016,#42017,
#42018,#42019,#42020,#42021,#42022,#42023,#42024,#42025,#42026,#42027,#42028,
#42029),.UNSPECIFIED.,.F.,.F.,(4,3,3,3,3,3,3,3,3,3,3,3,3,3,3,3,3,3,3,3,
3,3,3,3,3,3,3,3,3,3,3,3,3,3,3,3,3,3,3,3,3,3,4),(6.97767400438006E-5,0.0235124483256361,
0.0270464789573299,0.0540916358144278,0.0540924383659419,0.0808761116857087,
0.10182755879334,0.128477878765437,0.155397360247213,0.182107640682707,
0.203530646983436,0.207332017371417,0.207335173218032,0.233537240917649,
0.260215569308816,0.287100578155007,0.305135316889012,0.331037947464665,
0.332835591432724,0.358148063171977,0.360534126946588,0.360535865976435,
0.387324342918355,0.406659063564906,0.433301001733156,0.460207152642024,
0.486907643567796,0.508111183143103,0.513642026520772,0.513644119980954,
0.539917002725518,0.566646088148737,0.593538460524371,0.609500681295586,
0.636287771621458,0.661202837393452,0.663188937792746,0.66676046432175,
0.666767529697564,0.691789652308819,0.69357815457004,0.710837254295307,
0.727868008326198),.UNSPECIFIED.);
#625=B_SPLINE_CURVE_WITH_KNOTS('',3,(#42034,#42035,#42036,#42037,#42038,
#42039,#42040,#42041,#42042,#42043,#42044,#42045,#42046,#42047,#42048,#42049,
#42050,#42051,#42052,#42053,#42054,#42055,#42056,#42057,#42058,#42059,#42060,
#42061,#42062,#42063,#42064,#42065,#42066,#42067,#42068,#42069,#42070,#42071,
#42072,#42073,#42074,#42075,#42076,#42077,#42078,#42079,#42080,#42081,#42082,
#42083),.UNSPECIFIED.,.F.,.F.,(4,2,2,2,2,2,2,2,2,2,2,2,2,2,2,2,2,2,2,2,
2,2,2,2,4),(0.948102451772265,0.963248283802765,1.04166019732699,1.13852638559126,
1.24111112615258,1.28817418963009,1.38173677806716,1.48119583120305,1.52865407567559,
1.62580315113657,1.67715559130836,1.77123509905442,1.86940551833799,1.92006452837572,
1.96928463441235,2.07106552400663,2.11953556464442,2.1696635783818,2.2628314825113,
2.31268183523941,2.40975454513444,2.46028307555686,2.50010956658168,2.52690669878563,
2.54700836416053),.UNSPECIFIED.);
#626=B_SPLINE_CURVE_WITH_KNOTS('',3,(#42084,#42085,#42086,#42087,#42088,
#42089,#42090,#42091,#42092,#42093,#42094,#42095,#42096,#42097,#42098,#42099,
#42100,#42101,#42102,#42103,#42104,#42105,#42106,#42107,#42108,#42109,#42110,
#42111,#42112,#42113,#42114,#42115,#42116,#42117,#42118,#42119,#42120,#42121,
#42122,#42123,#42124,#42125,#42126,#42127,#42128,#42129),.UNSPECIFIED.,
 .F.,.F.,(4,2,2,2,2,2,2,2,2,2,2,2,2,2,2,2,2,2,2,2,2,2,4),(3.61415565987237E-6,
0.077382941848095,0.160320021301451,0.209315495312916,0.306998962340119,
0.403428249018374,0.453483402618285,0.502488421932669,0.552021971453635,
0.651021708478505,0.734535687626094,0.835245242957744,0.929270713532786,
0.97642189347609,1.0772912867649,1.17001200448534,1.22066776172236,1.26903355645575,
1.31675674395734,1.41727824130363,1.46576352901781,1.51581597882557,1.58755892759308),
 .UNSPECIFIED.);
#627=B_SPLINE_CURVE_WITH_KNOTS('',3,(#42135,#42136,#42137,#42138,#42139,
#42140,#42141,#42142,#42143,#42144,#42145,#42146,#42147,#42148,#42149,#42150,
#42151,#42152),.UNSPECIFIED.,.F.,.F.,(4,2,2,2,2,2,2,2,4),(1.58647040136232,
1.64954740781937,1.74368498223918,1.79306983672385,1.88170654786799,1.98253725725693,
2.07467976983039,2.1593136884966,2.23194989940745),.UNSPECIFIED.);
#628=B_SPLINE_CURVE_WITH_KNOTS('',3,(#42153,#42154,#42155,#42156,#42157,
#42158,#42159,#42160,#42161,#42162,#42163,#42164,#42165,#42166,#42167,#42168,
#42169,#42170,#42171,#42172,#42173,#42174,#42175,#42176,#42177,#42178),
 .UNSPECIFIED.,.F.,.F.,(4,2,2,2,2,2,2,2,2,2,2,2,4),(0.,0.0676700015567033,
0.122566337419964,0.205326521836919,0.282812301557027,0.378757335369595,
0.472380426030512,0.559981068984037,0.646990361523079,0.723350516868986,
0.799938201588545,0.867845104473521,0.948102451772265),.UNSPECIFIED.);
#629=B_SPLINE_CURVE_WITH_KNOTS('',3,(#42180,#42181,#42182,#42183,#42184,
#42185,#42186,#42187,#42188,#42189,#42190,#42191,#42192,#42193,#42194,#42195,
#42196,#42197,#42198,#42199,#42200,#42201,#42202,#42203,#42204,#42205,#42206,
#42207),.UNSPECIFIED.,.F.,.F.,(4,2,2,2,2,2,2,2,2,2,2,2,2,4),(1.58755892759308,
1.61118768308576,1.7120370068482,1.79401697393938,1.83561413499285,1.93632851510131,
2.01723367290632,2.05971469843759,2.16030698468104,2.24037081829283,2.33947585278893,
2.42806601707448,2.48424726450739,2.53786893574039),.UNSPECIFIED.);
#630=B_SPLINE_CURVE_WITH_KNOTS('',3,(#42208,#42209,#42210,#42211,#42212,
#42213,#42214,#42215,#42216,#42217,#42218,#42219,#42220,#42221,#42222,#42223,
#42224,#42225,#42226,#42227,#42228,#42229,#42230,#42231,#42232,#42233,#42234,
#42235,#42236,#42237,#42238,#42239,#42240,#42241,#42242,#42243,#42244,#42245,
#42246,#42247,#42248,#42249,#42250,#42251,#42252,#42253,#42254,#42255,#42256,
#42257,#42258,#42259,#42260,#42261,#42262,#42263,#42264,#42265,#42266,#42267,
#42268,#42269,#42270,#42271,#42272,#42273,#42274,#42275,#42276,#42277,#42278,
#42279,#42280,#42281,#42282,#42283,#42284,#42285,#42286,#42287,#42288,#42289,
#42290,#42291,#42292,#42293,#42294,#42295),.UNSPECIFIED.,.F.,.F.,(4,3,3,
3,3,3,3,3,3,3,3,3,3,3,3,3,3,3,3,3,3,3,3,3,3,3,3,3,3,4),(0.,0.0260937840727114,
0.0525749650683046,0.0790662183953249,0.10174715965396,0.128409551897913,
0.143179660817706,0.169333208229716,0.195892486876489,0.203377364754321,
0.229839532229633,0.256528353772948,0.282952141779042,0.304921331842682,
0.310762738631824,0.336812421877813,0.363315467390979,0.390012597263233,
0.406390796679477,0.433075871178777,0.459775676011333,0.478564893937639,
0.505168461021389,0.507799856305071,0.534148262403094,0.560816838480447,
0.587385623839857,0.604451917299051,0.60916481417943,0.63998402750676),
 .UNSPECIFIED.);
#631=B_SPLINE_CURVE_WITH_KNOTS('',3,(#42301,#42302,#42303,#42304),
 .UNSPECIFIED.,.F.,.F.,(4,4),(1.03705581745603,1.03710062472995),
 .UNSPECIFIED.);
#632=B_SPLINE_CURVE_WITH_KNOTS('',3,(#42305,#42306,#42307,#42308,#42309,
#42310,#42311,#42312,#42313,#42314,#42315,#42316,#42317,#42318,#42319,#42320,
#42321,#42322,#42323,#42324,#42325,#42326,#42327,#42328,#42329,#42330,#42331,
#42332,#42333,#42334,#42335,#42336,#42337,#42338,#42339,#42340,#42341,#42342,
#42343,#42344,#42345,#42346,#42347,#42348,#42349,#42350,#42351,#42352),
 .UNSPECIFIED.,.F.,.F.,(4,2,2,2,2,2,2,2,2,2,2,2,2,2,2,2,2,2,2,2,2,2,2,4),
(1.0000000652683E-6,0.0659798375703458,0.131960432135887,0.227947110507754,
0.278170740594184,0.32755046055882,0.377278851322222,0.426154139782107,
0.527372108276288,0.575321757958173,0.67648372491335,0.724474618070015,
0.825273934637277,0.87406352498187,0.975310913425844,1.06590783546145,1.11596419449799,
1.1622724896011,1.21029538172571,1.31150498364856,1.405531155535,1.50086798044765,
1.54850345928088,1.58647040136232),.UNSPECIFIED.);
#633=B_SPLINE_CURVE_WITH_KNOTS('',3,(#42353,#42354,#42355,#42356,#42357,
#42358,#42359,#42360,#42361,#42362,#42363,#42364,#42365,#42366,#42367,#42368,
#42369,#42370,#42371,#42372,#42373,#42374,#42375,#42376,#42377,#42378,#42379,
#42380,#42381,#42382,#42383,#42384,#42385,#42386,#42387,#42388,#42389,#42390,
#42391,#42392,#42393,#42394,#42395,#42396,#42397,#42398,#42399,#42400,#42401,
#42402),.UNSPECIFIED.,.F.,.F.,(4,2,2,2,2,2,2,2,2,2,2,2,2,2,2,2,2,2,2,2,
2,2,2,2,4),(0.000199761406301567,0.0690250162272561,0.120468154968914,0.221585345736489,
0.318571823185642,0.412447787590937,0.460525423192448,0.510348161937974,
0.559844210864398,0.660838829435275,0.709557966219876,0.757765007399357,
0.85247110551944,0.903280765958044,0.995810811626083,1.09264246022628,1.14040894397419,
1.24104431859928,1.29015750425647,1.35517589475524,1.398387594317,1.43868557502763,
1.48058004729817,1.57600852077177,1.59042890355212),.UNSPECIFIED.);
#634=B_SPLINE_CURVE_WITH_KNOTS('',3,(#42408,#42409,#42410,#42411,#42412,
#42413,#42414,#42415,#42416,#42417,#42418,#42419,#42420,#42421,#42422,#42423,
#42424,#42425),.UNSPECIFIED.,.F.,.F.,(4,2,2,2,2,2,2,2,4),(1.33398049474525E-6,
0.0691723805623115,0.134134919596717,0.179786156624329,0.276551377826846,
0.326554301751731,0.420325831437485,0.489305280783672,0.553050350028315),
 .UNSPECIFIED.);
#635=B_SPLINE_CURVE_WITH_KNOTS('',3,(#42426,#42427,#42428,#42429,#42430,
#42431,#42432,#42433,#42434,#42435,#42436,#42437,#42438,#42439,#42440,#42441,
#42442,#42443,#42444,#42445,#42446,#42447,#42448,#42449,#42450,#42451),
 .UNSPECIFIED.,.F.,.F.,(4,2,2,2,2,2,2,2,2,2,2,2,4),(3.15205015175211E-5,
0.0633644897124623,0.130089056650009,0.228142859899691,0.326403155931319,
0.422157763664604,0.518583456450466,0.619958904732367,0.719007867076939,
0.817973781907731,0.868478058477331,0.95165878657454,1.03705581745603),
 .UNSPECIFIED.);
#636=B_SPLINE_CURVE_WITH_KNOTS('',3,(#42452,#42453,#42454,#42455,#42456,
#42457,#42458,#42459,#42460,#42461,#42462,#42463,#42464,#42465,#42466,#42467,
#42468,#42469,#42470,#42471,#42472,#42473,#42474,#42475,#42476,#42477,#42478,
#42479,#42480,#42481,#42482,#42483,#42484,#42485,#42486,#42487,#42488,#42489,
#42490,#42491,#42492,#42493,#42494,#42495,#42496,#42497),.UNSPECIFIED.,
 .F.,.F.,(4,2,2,2,2,2,2,2,2,2,2,2,2,2,2,2,2,2,2,2,2,2,4),(1.59042890355212,
1.61509734716197,1.64572427898667,1.68535868251392,1.72156708258987,1.78007921656754,
1.84960897097247,1.93624638519471,2.02924170442665,2.12247140474378,2.22212513699261,
2.3077268420635,2.35571077411299,2.45666738417593,2.55076418648938,2.60085804292609,
2.69372336912999,2.74018787352896,2.8346144003695,2.92270245416146,3.02438495680549,
3.11184323544286,3.17817324820249),.UNSPECIFIED.);
#637=B_SPLINE_CURVE_WITH_KNOTS('',3,(#42503,#42504,#42505,#42506,#42507,
#42508,#42509,#42510,#42511,#42512,#42513,#42514),.UNSPECIFIED.,.F.,.F.,
(4,2,2,2,2,4),(1.58610784508116,1.65359225971699,1.70251946683584,1.79015455082039,
1.88930640561349,1.97403018723799),.UNSPECIFIED.);
#638=B_SPLINE_CURVE_WITH_KNOTS('',3,(#42515,#42516,#42517,#42518,#42519,
#42520,#42521,#42522,#42523,#42524,#42525,#42526,#42527,#42528,#42529,#42530,
#42531,#42532,#42533,#42534,#42535,#42536,#42537,#42538,#42539,#42540,#42541,
#42542,#42543,#42544,#42545,#42546,#42547,#42548,#42549,#42550,#42551,#42552,
#42553,#42554,#42555,#42556,#42557,#42558,#42559,#42560,#42561,#42562,#42563,
#42564,#42565,#42566,#42567,#42568,#42569,#42570,#42571,#42572,#42573,#42574,
#42575,#42576,#42577,#42578,#42579,#42580,#42581,#42582,#42583,#42584,#42585,
#42586,#42587,#42588,#42589,#42590,#42591,#42592,#42593,#42594,#42595,#42596,
#42597,#42598,#42599,#42600,#42601,#42602,#42603,#42604,#42605,#42606,#42607,
#42608,#42609,#42610,#42611,#42612,#42613,#42614,#42615,#42616,#42617,#42618,
#42619,#42620,#42621,#42622,#42623,#42624,#42625,#42626,#42627,#42628,#42629,
#42630,#42631,#42632,#42633,#42634,#42635,#42636,#42637,#42638,#42639,#42640,
#42641,#42642,#42643,#42644,#42645,#42646,#42647,#42648,#42649,#42650,#42651,
#42652,#42653,#42654,#42655,#42656,#42657,#42658,#42659,#42660,#42661,#42662,
#42663,#42664,#42665,#42666,#42667,#42668,#42669,#42670,#42671,#42672,#42673,
#42674,#42675,#42676,#42677,#42678,#42679,#42680,#42681,#42682,#42683,#42684,
#42685,#42686,#42687,#42688,#42689,#42690,#42691,#42692,#42693,#42694,#42695,
#42696,#42697,#42698,#42699,#42700,#42701,#42702,#42703,#42704,#42705,#42706,
#42707,#42708,#42709,#42710,#42711,#42712,#42713,#42714,#42715,#42716,#42717,
#42718,#42719,#42720,#42721,#42722,#42723,#42724,#42725,#42726,#42727,#42728,
#42729,#42730,#42731,#42732,#42733,#42734,#42735,#42736,#42737,#42738,#42739,
#42740,#42741,#42742,#42743),.UNSPECIFIED.,.F.,.F.,(4,3,3,3,3,3,3,3,3,3,
3,3,3,3,3,3,3,3,3,3,3,3,3,3,3,3,3,3,3,3,3,3,3,3,3,3,3,3,3,3,3,3,3,3,3,3,
3,3,3,3,3,3,3,3,3,3,3,3,3,3,3,3,3,3,3,3,3,3,3,3,3,3,3,3,3,3,4),(1.97046892380326E-7,
0.0165119087567328,0.0269521658292449,0.0514461508287838,0.053986697928493,
0.061957278941543,0.0619660940702222,0.0868551258564478,0.088772735096238,
0.10212602798035,0.129068676009789,0.156011324039229,0.156013890995603,
0.182913548427808,0.203854870580913,0.230701706835421,0.250045675689164,
0.250051837794113,0.27563745285687,0.277653721785625,0.305261767882086,
0.331953297927535,0.358937695991391,0.375451509787054,0.375458910130687,
0.400443220256602,0.402335123360528,0.406329654807662,0.432917759153746,
0.459832615589691,0.486691726360605,0.500788281582239,0.500791362256077,
0.507021309259397,0.533457855496874,0.560290345237192,0.587164758587564,
0.60737646809822,0.626070235128599,0.626079280624986,0.651201536368465,
0.652547853164669,0.680012430295542,0.707477007426416,0.734272256537736,
0.758887457771652,0.761271581217608,0.767098043492731,0.767106729118364,
0.791557876361479,0.793988196663842,0.807311994887596,0.833990067833167,
0.860961066123945,0.887784201963004,0.906820884562021,0.908051502841903,
0.908056675451242,0.934357362767099,0.961121352560656,0.988069529586017,
1.00602353353002,1.03072380463237,1.03297061250337,1.04901367065168,1.04902053837709,
1.07372752541493,1.07700485902145,1.10321909090914,1.10499604739123,1.1317485186321,
1.15875797074834,1.1836094806426,1.18562638883337,1.19002244111504,1.19003005836486,
1.20016986403664),.UNSPECIFIED.);
#639=B_SPLINE_CURVE_WITH_KNOTS('',3,(#42745,#42746,#42747,#42748,#42749,
#42750,#42751,#42752,#42753,#42754,#42755,#42756,#42757,#42758,#42759,#42760,
#42761,#42762),.UNSPECIFIED.,.F.,.F.,(4,2,2,2,2,2,2,2,4),(3.17817324820249,
3.21334005896499,3.30095732570528,3.40212874114706,3.48932390867776,3.59034661861351,
3.67575648182955,3.77639745946347,3.87258558614326),.UNSPECIFIED.);
#640=B_SPLINE_CURVE_WITH_KNOTS('',3,(#42763,#42764,#42765,#42766,#42767,
#42768,#42769,#42770,#42771,#42772,#42773,#42774,#42775,#42776,#42777,#42778,
#42779,#42780,#42781,#42782,#42783,#42784,#42785,#42786,#42787,#42788,#42789,
#42790,#42791,#42792,#42793,#42794,#42795,#42796,#42797,#42798,#42799,#42800,
#42801,#42802,#42803,#42804,#42805,#42806,#42807,#42808,#42809,#42810,#42811,
#42812,#42813,#42814,#42815,#42816,#42817,#42818,#42819,#42820,#42821,#42822,
#42823,#42824,#42825,#42826,#42827,#42828,#42829,#42830,#42831,#42832,#42833,
#42834,#42835,#42836,#42837,#42838,#42839,#42840,#42841,#42842,#42843,#42844,
#42845,#42846,#42847,#42848,#42849,#42850,#42851,#42852,#42853,#42854,#42855,
#42856,#42857,#42858,#42859,#42860,#42861,#42862,#42863,#42864,#42865,#42866,
#42867,#42868,#42869,#42870,#42871,#42872,#42873,#42874,#42875,#42876,#42877,
#42878,#42879,#42880,#42881,#42882,#42883,#42884,#42885,#42886,#42887,#42888,
#42889,#42890,#42891,#42892,#42893,#42894,#42895,#42896,#42897,#42898,#42899,
#42900,#42901,#42902,#42903,#42904,#42905,#42906,#42907,#42908,#42909,#42910,
#42911,#42912,#42913,#42914,#42915,#42916,#42917,#42918,#42919,#42920,#42921,
#42922,#42923,#42924,#42925,#42926,#42927,#42928),.UNSPECIFIED.,.F.,.F.,
(4,3,3,3,3,3,3,3,3,3,3,3,3,3,3,3,3,3,3,3,3,3,3,3,3,3,3,3,3,3,3,3,3,3,3,
3,3,3,3,3,3,3,3,3,3,3,3,3,3,3,3,3,3,3,3,4),(0.00195662276257164,0.0057265082120884,
0.00778343510459544,0.0262434362367702,0.0277363971949173,0.0324316244813748,
0.0591912596596283,0.0860114790298136,0.109672947671685,0.109673851626103,
0.12794618277961,0.154104266777492,0.180854266012755,0.193566709158549,
0.193570035685709,0.220316211357797,0.223705859480335,0.250575073070551,
0.275935977789185,0.277441778425786,0.277444286660766,0.302811945533245,
0.304181269015732,0.319745719238003,0.346298818737683,0.373152022009375,
0.399880935631714,0.416128760511614,0.440487000619039,0.443011467604648,
0.445160535678054,0.44516262425229,0.470169452132286,0.471533399549815,
0.49837210907613,0.512757329921647,0.539487448178301,0.566398841468605,
0.592995666409934,0.60958270433084,0.612904438499428,0.612904942401022,
0.639055399317768,0.665682621424802,0.692541721428282,0.706686554608931,
0.733464686518852,0.758577078163878,0.76027290818244,0.780655324452018,
0.7806575379144,0.804084831935261,0.830443692926505,0.857216066700044,0.884077928685615,
0.896610673280827),.UNSPECIFIED.);
#641=B_SPLINE_CURVE_WITH_KNOTS('',3,(#42933,#42934,#42935,#42936,#42937,
#42938,#42939,#42940,#42941,#42942,#42943,#42944,#42945,#42946,#42947,#42948,
#42949,#42950,#42951,#42952,#42953,#42954,#42955,#42956,#42957,#42958,#42959,
#42960,#42961,#42962,#42963,#42964,#42965,#42966,#42967,#42968,#42969,#42970,
#42971,#42972,#42973,#42974),.UNSPECIFIED.,.F.,.F.,(4,2,2,2,2,2,2,2,2,2,
2,2,2,2,2,2,2,2,2,2,4),(5.61108670082191E-6,0.0521038174851644,0.0935393401420401,
0.163487238226365,0.245209849008126,0.340133440268412,0.408755389589607,
0.509893079867885,0.608823499223934,0.699926438388842,0.797522199540615,
0.89858838991344,0.986966947055123,1.03605369324,1.12548372504641,1.22653559591547,
1.32179905784751,1.37055336956388,1.45918131120364,1.5599602720752,1.58610784508116),
 .UNSPECIFIED.);
#642=B_SPLINE_CURVE_WITH_KNOTS('',3,(#42976,#42977,#42978,#42979),
 .UNSPECIFIED.,.F.,.F.,(4,4),(0.896610673280827,0.896791920131866),
 .UNSPECIFIED.);
#643=B_SPLINE_CURVE_WITH_KNOTS('',3,(#42980,#42981,#42982,#42983,#42984,
#42985,#42986,#42987,#42988,#42989,#42990,#42991,#42992,#42993,#42994,#42995,
#42996,#42997,#42998,#42999,#43000,#43001,#43002,#43003,#43004,#43005,#43006,
#43007,#43008,#43009,#43010,#43011,#43012,#43013,#43014,#43015,#43016,#43017,
#43018,#43019),.UNSPECIFIED.,.F.,.F.,(4,2,2,2,2,2,2,2,2,2,2,2,2,2,2,2,2,
2,2,4),(5.2177231840437E-6,0.0530311686959936,0.114759217257224,0.211495904314178,
0.312968826970064,0.361760349371721,0.455764780613197,0.555669062486527,
0.605170600274074,0.70403338905179,0.804954817122082,0.906215196147122,
0.955080727331366,1.05100054971597,1.15212735488212,1.19901836385656,1.30009856105027,
1.39113241409266,1.49270447321307,1.58736511801968),.UNSPECIFIED.);
#644=B_SPLINE_CURVE_WITH_KNOTS('',3,(#43022,#43023,#43024,#43025,#43026,
#43027,#43028,#43029,#43030,#43031,#43032,#43033,#43034,#43035,#43036,#43037,
#43038,#43039,#43040,#43041,#43042,#43043,#43044,#43045),.UNSPECIFIED.,
 .F.,.F.,(4,2,2,2,2,2,2,2,2,2,2,4),(1.58736511801968,1.59210150155741,1.68173808769121,
1.72911766226968,1.82832409000194,1.92646536051439,2.01577372818829,2.06358998938427,
2.16172397625675,2.25737672526083,2.33277369713274,2.39803079505187),
 .UNSPECIFIED.);
#645=B_SPLINE_CURVE_WITH_KNOTS('',3,(#43047,#43048,#43049,#43050,#43051,
#43052,#43053,#43054,#43055,#43056,#43057,#43058,#43059,#43060,#43061,#43062,
#43063,#43064,#43065,#43066),.UNSPECIFIED.,.F.,.F.,(4,2,2,2,2,2,2,2,2,4),
(3.30476667653425E-5,0.0730119917909342,0.155321911197543,0.246835800980314,
0.348560854775418,0.439795908011992,0.541409392577865,0.6324553637244,0.681210482541812,
0.775512523779579),.UNSPECIFIED.);
#646=B_SPLINE_CURVE_WITH_KNOTS('',3,(#43070,#43071,#43072,#43073,#43074,
#43075,#43076,#43077,#43078,#43079),.UNSPECIFIED.,.F.,.F.,(4,2,2,2,4),(3.172018184782,
3.2383509868975,3.33901616963149,3.39429588367164,3.44364720042429),
 .UNSPECIFIED.);
#647=B_SPLINE_CURVE_WITH_KNOTS('',3,(#43080,#43081,#43082,#43083,#43084,
#43085,#43086,#43087,#43088,#43089,#43090,#43091,#43092,#43093,#43094,#43095,
#43096,#43097,#43098,#43099,#43100,#43101,#43102,#43103,#43104,#43105,#43106,
#43107,#43108,#43109,#43110,#43111,#43112,#43113,#43114,#43115),
 .UNSPECIFIED.,.F.,.F.,(4,2,2,2,2,2,2,2,2,2,2,2,2,2,2,2,2,4),(7.85099826035063E-5,
0.0835230548401281,0.176109879532006,0.268759385921064,0.370729149112131,
0.41970804661686,0.517513704143356,0.610332470955531,0.659293399050333,
0.706602751260405,0.807760001799314,0.856191841693314,0.95014160834287,
1.0514708942237,1.09993161210594,1.20132087842412,1.25267680689251,1.31839655317403),
 .UNSPECIFIED.);
#648=B_SPLINE_CURVE_WITH_KNOTS('',3,(#43120,#43121,#43122,#43123,#43124,
#43125,#43126,#43127,#43128,#43129,#43130,#43131,#43132,#43133,#43134,#43135,
#43136,#43137,#43138,#43139,#43140,#43141,#43142,#43143,#43144,#43145,#43146,
#43147,#43148,#43149,#43150,#43151,#43152,#43153,#43154,#43155,#43156,#43157,
#43158,#43159,#43160,#43161,#43162,#43163),.UNSPECIFIED.,.F.,.F.,(4,2,2,
2,2,2,2,2,2,2,2,2,2,2,2,2,2,2,2,2,2,4),(1.58714917405264,1.62487059328602,
1.67310993772542,1.72192229587615,1.81681073323228,1.86584217015149,1.96083596104287,
2.05613974965739,2.1040867325538,2.20532404072983,2.29897571506993,2.39974218606846,
2.48518687077461,2.5858894241594,2.66994998309819,2.77075629546814,2.86902915491451,
2.91827951445788,3.01205343509936,3.10410692331575,3.15229172786727,3.172018184782),
 .UNSPECIFIED.);
#649=B_SPLINE_CURVE_WITH_KNOTS('',3,(#43165,#43166,#43167,#43168,#43169,
#43170,#43171,#43172,#43173,#43174,#43175,#43176,#43177,#43178,#43179,#43180,
#43181,#43182,#43183,#43184,#43185,#43186,#43187,#43188,#43189,#43190,#43191,
#43192,#43193,#43194,#43195,#43196),.UNSPECIFIED.,.F.,.F.,(4,2,2,2,2,2,
2,2,2,2,2,2,2,2,2,4),(0.775512523779579,0.777139842577585,0.827904318957342,
0.876647272001025,0.977538689119265,1.07725466162777,1.12517655585581,1.22408411710603,
1.27204087343801,1.3204700519371,1.42213731037915,1.47124250018406,1.57003316977662,
1.61591228478928,1.68722356316175,1.75326419407806),.UNSPECIFIED.);
#650=B_SPLINE_CURVE_WITH_KNOTS('',3,(#43198,#43199,#43200,#43201,#43202,
#43203,#43204,#43205,#43206,#43207,#43208,#43209,#43210,#43211,#43212,#43213,
#43214,#43215,#43216,#43217,#43218,#43219,#43220,#43221,#43222,#43223,#43224,
#43225,#43226,#43227,#43228,#43229,#43230,#43231,#43232,#43233,#43234,#43235,
#43236,#43237,#43238,#43239,#43240,#43241,#43242,#43243,#43244,#43245,#43246,
#43247,#43248,#43249,#43250,#43251,#43252,#43253,#43254,#43255,#43256,#43257,
#43258,#43259,#43260,#43261,#43262,#43263,#43264,#43265,#43266,#43267,#43268,
#43269,#43270,#43271,#43272,#43273,#43274,#43275,#43276,#43277,#43278,#43279,
#43280,#43281,#43282,#43283,#43284,#43285,#43286,#43287,#43288,#43289,#43290,
#43291,#43292,#43293,#43294,#43295,#43296,#43297,#43298,#43299,#43300,#43301,
#43302,#43303),.UNSPECIFIED.,.F.,.F.,(4,3,3,3,3,3,3,3,3,3,3,3,3,3,3,3,3,
3,3,3,3,3,3,3,3,3,3,3,3,3,3,3,3,3,3,4),(0.,0.0223542576374909,0.0267832089461343,
0.0537106663391406,0.0806381237321469,0.0806454974621168,0.101827263080174,
0.128174021766349,0.1549636261091,0.181852320077753,0.203530354517993,0.228884303326543,
0.230456690199924,0.248570803195244,0.248582233437807,0.275068797818176,
0.301942959046185,0.305135333726472,0.331789806526895,0.358710123188655,
0.385428062240576,0.406659177973182,0.416447614847817,0.416448913630405,
0.442731090245464,0.46946613570733,0.496338911638681,0.508111106730458,
0.534947029113335,0.559945964594669,0.561774837982785,0.584338701001998,
0.584339726650227,0.608125666318232,0.609500547121593,0.611296099258107),
 .UNSPECIFIED.);
#651=B_SPLINE_CURVE_WITH_KNOTS('',3,(#43304,#43305,#43306,#43307),
 .UNSPECIFIED.,.F.,.F.,(4,4),(5.08580690585039E-5,0.000161519520353054),
 .UNSPECIFIED.);
#652=B_SPLINE_CURVE_WITH_KNOTS('',3,(#43313,#43314,#43315,#43316),
 .UNSPECIFIED.,.F.,.F.,(4,4),(1.06238567890844,1.06246996364553),
 .UNSPECIFIED.);
#653=B_SPLINE_CURVE_WITH_KNOTS('',3,(#43317,#43318,#43319,#43320,#43321,
#43322,#43323,#43324,#43325,#43326,#43327,#43328,#43329,#43330,#43331,#43332,
#43333,#43334,#43335,#43336,#43337,#43338,#43339,#43340,#43341,#43342,#43343,
#43344,#43345,#43346,#43347,#43348,#43349,#43350,#43351,#43352,#43353,#43354,
#43355,#43356,#43357,#43358,#43359,#43360,#43361,#43362,#43363,#43364),
 .UNSPECIFIED.,.F.,.F.,(4,2,2,2,2,2,2,2,2,2,2,2,2,2,2,2,2,2,2,2,2,2,2,4),
(1.00000016286752E-6,0.0862068928556652,0.185952757554959,0.253237461541151,
0.355299607682124,0.401863096771156,0.499562116678737,0.547297339803957,
0.597392338041793,0.646548704907709,0.747322930923275,0.795434512205605,
0.844803214979016,0.938204332302665,0.989388740266747,1.03857369442406,
1.08668491424657,1.18649323610714,1.23607437025058,1.33703207912544,1.43013146949498,
1.47866234274992,1.57414919062349,1.58714917405264),.UNSPECIFIED.);
#654=B_SPLINE_CURVE_WITH_KNOTS('',3,(#43365,#43366,#43367,#43368,#43369,
#43370,#43371,#43372,#43373,#43374,#43375,#43376,#43377,#43378,#43379,#43380,
#43381,#43382,#43383,#43384,#43385,#43386,#43387,#43388,#43389,#43390,#43391,
#43392,#43393,#43394,#43395,#43396,#43397,#43398,#43399,#43400,#43401,#43402,
#43403,#43404,#43405,#43406),.UNSPECIFIED.,.F.,.F.,(4,2,2,2,2,2,2,2,2,2,
2,2,2,2,2,2,2,2,2,2,4),(0.000161519520353054,0.0575337694029372,0.103369793689619,
0.181155008716227,0.278801444853426,0.378970141096557,0.450655431577042,
0.55217277736237,0.652186775252743,0.699348984508397,0.79445576961415,0.896119705397044,
0.993989743294838,1.09193882160934,1.19250903312403,1.27385529020416,1.31754056768087,
1.4189329957357,1.50211835110858,1.54743432722965,1.58876261697574),
 .UNSPECIFIED.);
#655=B_SPLINE_CURVE_WITH_KNOTS('',3,(#43412,#43413,#43414,#43415,#43416,
#43417,#43418,#43419,#43420,#43421,#43422,#43423,#43424,#43425,#43426,#43427),
 .UNSPECIFIED.,.F.,.F.,(4,2,2,2,2,2,2,4),(1.58640007399783,1.64139361802863,
1.73124878129425,1.77890017001795,1.87864360161113,1.97454422453998,2.04996787109459,
2.11556527080477),.UNSPECIFIED.);
#656=B_SPLINE_CURVE_WITH_KNOTS('',3,(#43428,#43429,#43430,#43431,#43432,
#43433,#43434,#43435,#43436,#43437,#43438,#43439,#43440,#43441,#43442,#43443,
#43444,#43445,#43446,#43447,#43448,#43449,#43450,#43451,#43452,#43453,#43454,
#43455),.UNSPECIFIED.,.F.,.F.,(4,2,2,2,2,2,2,2,2,2,2,2,2,4),(6.24427194408881E-5,
0.07322487298628,0.159468398207204,0.247468541542693,0.342187470127241,
0.39026831901386,0.481724140650963,0.531314422375744,0.632816993761995,
0.731666562356075,0.833221392964525,0.934705130830227,0.992889032154437,
1.06238567890844),.UNSPECIFIED.);
#657=B_SPLINE_CURVE_WITH_KNOTS('',3,(#43457,#43458,#43459,#43460),
 .UNSPECIFIED.,.F.,.F.,(4,4),(1.58876261697574,1.58885620615735),
 .UNSPECIFIED.);
#658=B_SPLINE_CURVE_WITH_KNOTS('',3,(#43462,#43463,#43464,#43465,#43466,
#43467,#43468,#43469,#43470,#43471,#43472,#43473,#43474,#43475,#43476,#43477,
#43478,#43479,#43480,#43481,#43482,#43483,#43484,#43485,#43486,#43487,#43488,
#43489,#43490,#43491),.UNSPECIFIED.,.F.,.F.,(4,2,2,2,2,2,2,2,2,2,2,2,2,
2,4),(1.00000006509386E-6,0.0682125041812062,0.143755754402067,0.235144527123705,
0.285235038132226,0.385699790431721,0.433437205858489,0.533041599863107,
0.633814101828482,0.723255246139578,0.823934860858259,0.918280079420942,
0.959774675011753,1.01516523885657,1.06608140280668),.UNSPECIFIED.);
#659=B_SPLINE_CURVE_WITH_KNOTS('',3,(#43492,#43493,#43494,#43495,#43496,
#43497,#43498,#43499,#43500,#43501,#43502,#43503,#43504,#43505,#43506,#43507,
#43508,#43509,#43510,#43511,#43512,#43513,#43514,#43515,#43516,#43517,#43518,
#43519,#43520,#43521,#43522,#43523,#43524,#43525,#43526,#43527,#43528,#43529,
#43530,#43531,#43532,#43533,#43534,#43535,#43536,#43537,#43538,#43539,#43540,
#43541,#43542,#43543,#43544,#43545,#43546,#43547,#43548,#43549,#43550,#43551,
#43552,#43553,#43554,#43555,#43556,#43557,#43558,#43559,#43560,#43561,#43562,
#43563,#43564,#43565,#43566,#43567,#43568,#43569,#43570,#43571,#43572,#43573,
#43574,#43575,#43576,#43577,#43578,#43579,#43580,#43581,#43582),
 .UNSPECIFIED.,.F.,.F.,(4,3,3,3,3,3,3,3,3,3,3,3,3,3,3,3,3,3,3,3,3,3,3,3,
3,3,3,3,3,3,4),(4.29564213299729E-5,0.0223677416501253,0.0260479680645344,
0.0525003704776632,0.0789988343680503,0.101747215251029,0.128400865748245,
0.141656975489527,0.141658872579743,0.167838207053778,0.194409625139364,
0.203377866560224,0.229878293290454,0.256578496059846,0.282984477837726,
0.304921755801306,0.309301818525669,0.309302371754537,0.33528185162595,
0.361716897293269,0.388345503430247,0.393231851464744,0.393232990413532,
0.406390647464245,0.432857974016374,0.459538001164057,0.477156228609294,
0.477156985334002,0.50380408957998,0.507799457538043,0.523223944008924),
 .UNSPECIFIED.);
#660=B_SPLINE_CURVE_WITH_KNOTS('',3,(#43588,#43589,#43590,#43591),
 .UNSPECIFIED.,.F.,.F.,(4,4),(1.1543754051628,1.15472425279361),
 .UNSPECIFIED.);
#661=B_SPLINE_CURVE_WITH_KNOTS('',3,(#43592,#43593,#43594,#43595,#43596,
#43597,#43598,#43599,#43600,#43601,#43602,#43603,#43604,#43605,#43606,#43607,
#43608,#43609,#43610,#43611,#43612,#43613,#43614,#43615,#43616,#43617,#43618,
#43619,#43620,#43621,#43622,#43623,#43624,#43625,#43626,#43627,#43628,#43629,
#43630,#43631,#43632,#43633),.UNSPECIFIED.,.F.,.F.,(4,2,2,2,2,2,2,2,2,2,
2,2,2,2,2,2,2,2,2,2,4),(1.00000007275659E-6,0.0559430608918217,0.118052148831411,
0.219093370540287,0.31153943656164,0.39946568280495,0.493720317281655,0.565610392093586,
0.666574137732805,0.764328770373596,0.863333475800359,0.911061255280105,
1.01027931209133,1.05782504393973,1.10453551958502,1.20560998841793,1.30342902587861,
1.35176877208222,1.44239422836734,1.54378429828248,1.58640007399783),
 .UNSPECIFIED.);
#662=B_SPLINE_CURVE_WITH_KNOTS('',3,(#43634,#43635,#43636,#43637,#43638,
#43639,#43640,#43641,#43642,#43643,#43644,#43645,#43646,#43647,#43648,#43649,
#43650,#43651,#43652,#43653,#43654,#43655,#43656,#43657,#43658,#43659,#43660,
#43661,#43662,#43663,#43664,#43665,#43666,#43667,#43668,#43669,#43670,#43671,
#43672,#43673,#43674,#43675,#43676,#43677),.UNSPECIFIED.,.F.,.F.,(4,2,2,
2,2,2,2,2,2,2,2,2,2,2,2,2,2,2,2,2,2,4),(1.69660442820801E-5,0.0621727637931074,
0.130603354249022,0.177156779445226,0.274547260879537,0.322784074818011,
0.424774095589815,0.522858893257094,0.614218395466428,0.710184977845561,
0.760102124203472,0.809561950944269,0.909508918270125,0.957396684954257,
1.05866387333694,1.15989818588819,1.20802386750222,1.30924683729453,1.41072994296973,
1.45924151970641,1.56039389518965,1.59029600936748),.UNSPECIFIED.);
#663=B_SPLINE_CURVE_WITH_KNOTS('',3,(#43681,#43682,#43683,#43684,#43685,
#43686,#43687,#43688,#43689,#43690,#43691,#43692,#43693,#43694),
 .UNSPECIFIED.,.F.,.F.,(4,2,2,2,2,2,4),(1.00000008239902E-6,0.0861469959055848,
0.16752892050755,0.218403038515653,0.313556177494288,0.377493724390283,
0.436724401093653),.UNSPECIFIED.);
#664=B_SPLINE_CURVE_WITH_KNOTS('',3,(#43695,#43696,#43697,#43698,#43699,
#43700,#43701,#43702,#43703,#43704,#43705,#43706,#43707,#43708,#43709,#43710,
#43711,#43712,#43713,#43714,#43715,#43716,#43717,#43718,#43719,#43720,#43721,
#43722,#43723,#43724),.UNSPECIFIED.,.F.,.F.,(4,2,2,2,2,2,2,2,2,2,2,2,2,
2,4),(9.80168944251376E-5,0.0680801262020133,0.14586143617603,0.240637522592241,
0.342636008430395,0.429957466029602,0.479549005869444,0.57745774353028,
0.679413618393056,0.780274067553753,0.82957824766732,0.922751478636959,
1.02443351086548,1.0866638759187,1.1543754051628),.UNSPECIFIED.);
#665=B_SPLINE_CURVE_WITH_KNOTS('',3,(#43726,#43727,#43728,#43729,#43730,
#43731,#43732,#43733,#43734,#43735,#43736,#43737,#43738,#43739,#43740,#43741,
#43742,#43743,#43744,#43745,#43746,#43747,#43748,#43749,#43750,#43751,#43752,
#43753,#43754,#43755,#43756,#43757,#43758,#43759,#43760,#43761,#43762,#43763,
#43764,#43765,#43766,#43767,#43768,#43769),.UNSPECIFIED.,.F.,.F.,(4,2,2,
2,2,2,2,2,2,2,2,2,2,2,2,2,2,2,2,2,2,4),(1.59029600936748,1.66099639496899,
1.70972552920993,1.75826113830702,1.8555767844832,1.90658130165602,1.99380312867189,
2.0415571279748,2.12874854987234,2.23031052191635,2.32543416384813,2.37432218963118,
2.46222816392711,2.56316053006413,2.65050249863099,2.75143612038196,2.83483132107615,
2.93564925455118,3.01983818334638,3.12056610545761,3.1647596713537,3.17771221179641),
 .UNSPECIFIED.);
#666=B_SPLINE_CURVE_WITH_KNOTS('',3,(#43776,#43777,#43778,#43779,#43780,
#43781,#43782,#43783,#43784,#43785),.UNSPECIFIED.,.F.,.F.,(4,2,2,2,4),(3.0201138090629,
3.05453144613298,3.14992585636195,3.22599329218501,3.2916937650692),
 .UNSPECIFIED.);
#667=B_SPLINE_CURVE_WITH_KNOTS('',3,(#43786,#43787,#43788,#43789,#43790,
#43791,#43792,#43793,#43794,#43795,#43796,#43797,#43798,#43799,#43800,#43801,
#43802,#43803,#43804,#43805,#43806,#43807,#43808,#43809,#43810,#43811,#43812,
#43813,#43814,#43815,#43816,#43817,#43818,#43819,#43820,#43821),
 .UNSPECIFIED.,.F.,.F.,(4,2,2,2,2,2,2,2,2,2,2,2,2,2,2,2,2,4),(1.0958252776401E-5,
0.092418778574395,0.192596706540116,0.293780595397689,0.378232209619974,
0.479502465400529,0.578999118141845,0.6577822457542,0.7066707546433,0.753368584600514,
0.854537225797866,0.903434258597658,1.00440369535868,1.05343457647593,1.10352028314666,
1.19797564688056,1.25878976507826,1.31553845584881),.UNSPECIFIED.);
#668=B_SPLINE_CURVE_WITH_KNOTS('',3,(#43823,#43824,#43825,#43826,#43827,
#43828,#43829,#43830,#43831,#43832,#43833,#43834,#43835,#43836,#43837,#43838,
#43839,#43840,#43841,#43842,#43843,#43844),.UNSPECIFIED.,.F.,.F.,(4,2,2,
2,2,2,2,2,2,2,4),(3.17771221179641,3.26518167660643,3.35089729791118,3.44993600095358,
3.49741136148196,3.57932065032728,3.68014994637309,3.76186490783962,3.80876819856172,
3.90286034910187,3.98725875054216),.UNSPECIFIED.);
#669=B_SPLINE_CURVE_WITH_KNOTS('',3,(#43845,#43846,#43847,#43848,#43849,
#43850,#43851,#43852,#43853,#43854,#43855,#43856,#43857,#43858,#43859,#43860,
#43861,#43862,#43863,#43864),.UNSPECIFIED.,.F.,.F.,(4,2,2,2,2,2,2,2,2,4),
(0.000416008717854399,0.0789160364521911,0.16820016970267,0.263721702794877,
0.364559327860852,0.41321857398184,0.511236725439311,0.601083545522871,
0.702713773320289,0.779618357029204),.UNSPECIFIED.);
#670=B_SPLINE_CURVE_WITH_KNOTS('',3,(#43869,#43870,#43871,#43872,#43873,
#43874,#43875,#43876,#43877,#43878,#43879,#43880,#43881,#43882,#43883,#43884,
#43885,#43886,#43887,#43888,#43889,#43890,#43891,#43892,#43893,#43894,#43895,
#43896,#43897,#43898,#43899,#43900,#43901,#43902,#43903,#43904,#43905,#43906,
#43907,#43908,#43909,#43910),.UNSPECIFIED.,.F.,.F.,(4,2,2,2,2,2,2,2,2,2,
2,2,2,2,2,2,2,2,2,2,4),(1.43368549808538,1.4979818748124,1.59722154075269,
1.64585489812321,1.74723097068974,1.79558854641402,1.89662306941936,1.94406137704963,
2.04514199145719,2.143137685293,2.19150536074381,2.28211255975149,2.38304812520079,
2.48116627820141,2.57177924368629,2.61913455000118,2.7202429392984,2.81788847408514,
2.90768888907198,2.95549757298729,3.0201138090629),.UNSPECIFIED.);
#671=B_SPLINE_CURVE_WITH_KNOTS('',3,(#43911,#43912,#43913,#43914,#43915,
#43916,#43917,#43918,#43919,#43920,#43921,#43922,#43923,#43924,#43925,#43926,
#43927,#43928,#43929,#43930,#43931,#43932,#43933,#43934,#43935,#43936,#43937,
#43938,#43939,#43940,#43941,#43942,#43943,#43944,#43945,#43946,#43947,#43948,
#43949,#43950),.UNSPECIFIED.,.F.,.F.,(4,2,2,2,2,2,2,2,2,2,2,2,2,2,2,2,2,
2,2,4),(0.779618357029204,0.802803112888372,0.883979095536384,0.982406118287473,
1.08387046468192,1.18507915430368,1.27523848509429,1.37664382134265,1.45559685079245,
1.49947953640491,1.60087007831783,1.6482837684803,1.74839371188088,1.84038573945747,
1.92318528656684,2.02304617346582,2.1129309070806,2.21416610470643,2.28802740994192,
2.370068662874),.UNSPECIFIED.);
#672=B_SPLINE_CURVE_WITH_KNOTS('',3,(#43956,#43957,#43958,#43959,#43960,
#43961),.UNSPECIFIED.,.F.,.F.,(4,2,4),(3.17236617648777,3.24318852578899,
3.32825735645484),.UNSPECIFIED.);
#673=B_SPLINE_CURVE_WITH_KNOTS('',3,(#43962,#43963,#43964,#43965,#43966,
#43967,#43968,#43969,#43970,#43971,#43972,#43973,#43974,#43975,#43976,#43977,
#43978,#43979,#43980,#43981,#43982,#43983,#43984,#43985,#43986,#43987,#43988,
#43989,#43990,#43991,#43992,#43993,#43994,#43995,#43996,#43997,#43998,#43999),
 .UNSPECIFIED.,.F.,.F.,(4,2,2,2,2,2,2,2,2,2,2,2,2,2,2,2,2,2,4),(4.69863450241475E-6,
0.0732561627926064,0.15152434590406,0.200526515945472,0.294383845688464,
0.389747970553781,0.486785957457453,0.536554022637231,0.585543930501015,
0.673421563000948,0.770749466128403,0.846941804556702,0.948162354569468,
1.04068442063129,1.13302357768077,1.22937273149936,1.30336321367283,1.40435174774173,
1.43368549808538),.UNSPECIFIED.);
#674=B_SPLINE_CURVE_WITH_KNOTS('',3,(#44001,#44002,#44003,#44004,#44005,
#44006,#44007,#44008,#44009,#44010,#44011,#44012,#44013,#44014,#44015,#44016,
#44017,#44018,#44019,#44020,#44021,#44022,#44023,#44024,#44025,#44026),
 .UNSPECIFIED.,.F.,.F.,(4,2,2,2,2,2,2,2,2,2,2,2,4),(2.78339753933959E-5,
0.081948818254421,0.171142740482219,0.263745465431853,0.314368120177807,
0.415241291507573,0.463391677990754,0.551622304139495,0.59977844847948,
0.694775022006912,0.742068116649189,0.841854494119041,0.9268893973431),
 .UNSPECIFIED.);
#675=B_SPLINE_CURVE_WITH_KNOTS('',3,(#44027,#44028,#44029,#44030,#44031,
#44032,#44033,#44034,#44035,#44036,#44037,#44038,#44039,#44040,#44041,#44042,
#44043,#44044,#44045,#44046,#44047,#44048,#44049,#44050,#44051,#44052,#44053,
#44054,#44055,#44056,#44057,#44058,#44059,#44060,#44061,#44062,#44063,#44064,
#44065,#44066,#44067,#44068,#44069,#44070,#44071,#44072,#44073,#44074,#44075,
#44076,#44077,#44078,#44079,#44080,#44081,#44082,#44083,#44084,#44085,#44086,
#44087,#44088,#44089,#44090,#44091,#44092,#44093,#44094,#44095,#44096,#44097,
#44098,#44099,#44100,#44101,#44102,#44103,#44104,#44105,#44106,#44107,#44108,
#44109,#44110,#44111,#44112,#44113,#44114,#44115,#44116,#44117,#44118,#44119,
#44120,#44121,#44122,#44123,#44124,#44125,#44126,#44127,#44128,#44129,#44130,
#44131,#44132,#44133,#44134,#44135,#44136,#44137,#44138,#44139,#44140,#44141,
#44142,#44143,#44144,#44145,#44146,#44147,#44148,#44149,#44150,#44151,#44152,
#44153,#44154,#44155,#44156),.UNSPECIFIED.,.F.,.F.,(4,3,3,3,3,3,3,3,3,3,
3,3,3,3,3,3,3,3,3,3,3,3,3,3,3,3,3,3,3,3,3,3,3,3,3,3,3,3,3,3,3,3,3,4),(5.40439274532324E-8,
0.0176084116492507,0.0269444774751041,0.0512050753871218,0.0539556220322877,
0.0630337718589102,0.0630394189146231,0.087122863216934,0.0898661186384374,
0.102147910187398,0.128657264222907,0.155580733384103,0.18254235728964,
0.203860958424688,0.227729591399546,0.230883610031478,0.251120014207219,
0.251131374633248,0.274693170456122,0.278168215719489,0.302781642299717,
0.305216417231759,0.331840197301536,0.358832442830213,0.385767896852117,
0.406270766662611,0.429577811886119,0.433319718368037,0.439138755580813,
0.439145684566976,0.46302409972116,0.465591224746269,0.490728914473221,
0.492579509125595,0.506987157359231,0.53377820352076,0.560836181114381,
0.587691673133311,0.607343110066019,0.627140086067375,0.627173899054037,
0.651460955435538,0.6536906004346,0.659723809344152),.UNSPECIFIED.);
#676=B_SPLINE_CURVE_WITH_KNOTS('',3,(#44161,#44162,#44163,#44164,#44165,
#44166,#44167,#44168,#44169,#44170,#44171,#44172,#44173,#44174,#44175,#44176,
#44177,#44178,#44179,#44180,#44181,#44182,#44183,#44184,#44185,#44186,#44187,
#44188,#44189,#44190,#44191,#44192,#44193,#44194,#44195,#44196,#44197,#44198,
#44199,#44200,#44201,#44202),.UNSPECIFIED.,.F.,.F.,(4,2,2,2,2,2,2,2,2,2,
2,2,2,2,2,2,2,2,2,2,4),(1.58754199438591,1.66428756220311,1.75505140709888,
1.85247262654257,1.94559879742955,1.99141264552402,2.09224806187651,2.17687381898934,
2.27760558432556,2.36115785782877,2.46273884078532,2.506970278523,2.6072783781268,
2.69242749120669,2.7910892863526,2.83848659087682,2.92081415544938,3.02162491455608,
3.10269311798798,3.15009710686931,3.17236617648777),.UNSPECIFIED.);
#677=B_SPLINE_CURVE_WITH_KNOTS('',3,(#44204,#44205,#44206,#44207,#44208,
#44209,#44210,#44211,#44212,#44213,#44214,#44215,#44216,#44217,#44218,#44219,
#44220,#44221,#44222,#44223,#44224,#44225,#44226,#44227,#44228,#44229,#44230,
#44231,#44232,#44233),.UNSPECIFIED.,.F.,.F.,(4,2,2,2,2,2,2,2,2,2,2,2,2,
2,4),(7.98383028724678E-6,0.0594068121132572,0.117173822001359,0.157563544309192,
0.25282538752385,0.353748066677795,0.452720576279622,0.547246751719325,
0.596227171842395,0.692274403534477,0.786468812754584,0.887236199880665,
0.984305583682174,1.04109120139304,1.09448507079122),.UNSPECIFIED.);
#678=B_SPLINE_CURVE_WITH_KNOTS('',3,(#44234,#44235,#44236,#44237,#44238,
#44239,#44240,#44241,#44242,#44243,#44244,#44245,#44246,#44247,#44248,#44249,
#44250,#44251,#44252,#44253,#44254,#44255,#44256,#44257,#44258,#44259,#44260,
#44261,#44262,#44263,#44264,#44265,#44266,#44267,#44268,#44269,#44270,#44271,
#44272,#44273,#44274,#44275,#44276,#44277,#44278,#44279,#44280,#44281,#44282,
#44283,#44284,#44285,#44286,#44287,#44288,#44289,#44290,#44291,#44292,#44293,
#44294,#44295,#44296,#44297,#44298,#44299,#44300,#44301,#44302,#44303,#44304,
#44305,#44306,#44307,#44308,#44309,#44310,#44311,#44312),.UNSPECIFIED.,
 .F.,.F.,(4,3,3,3,3,3,3,3,3,3,3,3,3,3,3,3,3,3,3,3,3,3,3,3,3,3,4),(4.58842016772256E-5,
0.0231862791791696,0.0267235302321618,0.0536803738369688,0.080637102547167,
0.0806372174417757,0.10182702398916,0.12820009816435,0.155010998250621,
0.181909348449436,0.203530246760958,0.22893505393977,0.230469238508873,
0.248568363744309,0.248569988525206,0.275074209658101,0.301949036381728,
0.305135524171737,0.331796956449855,0.358718535004781,0.385415027716635,
0.406659425239883,0.416445184312435,0.416446996309603,0.442599172427887,
0.469460613188687,0.494689467284077),.UNSPECIFIED.);
#679=B_SPLINE_CURVE_WITH_KNOTS('',3,(#44317,#44318,#44319,#44320,#44321,
#44322,#44323,#44324,#44325,#44326,#44327,#44328,#44329,#44330,#44331,#44332,
#44333,#44334,#44335,#44336,#44337,#44338,#44339,#44340,#44341,#44342,#44343,
#44344,#44345,#44346,#44347,#44348,#44349,#44350,#44351,#44352,#44353,#44354,
#44355,#44356,#44357,#44358,#44359,#44360,#44361,#44362),.UNSPECIFIED.,
 .F.,.F.,(4,2,2,2,2,2,2,2,2,2,2,2,2,2,2,2,2,2,2,2,2,2,4),(7.66834827221688E-5,
0.0534536371935326,0.110991983464426,0.203800972593915,0.30051808488584,
0.401775523626737,0.50287541759609,0.550982689569767,0.599782660106522,
0.694241313514436,0.745324528568043,0.839057782678784,0.93605559701574,
0.986137663701895,1.03517902588757,1.1362195664112,1.18508550988462,1.23535743991359,
1.28496964571626,1.38380065054698,1.47551163273244,1.57716784819653,1.58754199438591),
 .UNSPECIFIED.);
#680=B_SPLINE_CURVE_WITH_KNOTS('',3,(#44363,#44364,#44365,#44366,#44367,
#44368,#44369,#44370,#44371,#44372,#44373,#44374,#44375,#44376,#44377,#44378,
#44379,#44380,#44381,#44382,#44383,#44384,#44385,#44386,#44387,#44388,#44389,
#44390,#44391,#44392,#44393,#44394,#44395,#44396,#44397,#44398,#44399,#44400,
#44401,#44402),.UNSPECIFIED.,.F.,.F.,(4,2,2,2,2,2,2,2,2,2,2,2,2,2,2,2,2,
2,2,4),(6.4154566266032E-5,0.071031520425574,0.152747669641631,0.249042814711534,
0.35068929650393,0.399104833478405,0.496987801918373,0.590472086651412,
0.692109735972922,0.768401783904028,0.869620781995952,0.966429502947187,
1.0657318064452,1.11062560595854,1.19784021313316,1.29114674735375,1.38647354043681,
1.42966321924486,1.53134219242619,1.5898434740455),.UNSPECIFIED.);
#681=B_SPLINE_CURVE_WITH_KNOTS('',3,(#44405,#44406,#44407,#44408,#44409,
#44410,#44411,#44412,#44413,#44414,#44415,#44416,#44417,#44418,#44419,#44420,
#44421,#44422,#44423,#44424,#44425,#44426,#44427,#44428,#44429,#44430,#44431,
#44432,#44433,#44434,#44435,#44436),.UNSPECIFIED.,.F.,.F.,(4,2,2,2,2,2,
2,2,2,2,2,2,2,2,2,4),(1.5898434740455,1.6271433856272,1.71712100874479,
1.76388458955179,1.86488993045687,1.96329627655657,2.05442894894533,2.10180472376313,
2.2020473014041,2.30061824506391,2.39053591761843,2.43818655549719,2.5370859795822,
2.63367841104952,2.70812820243631,2.77288713491997),.UNSPECIFIED.);
#682=B_SPLINE_CURVE_WITH_KNOTS('',3,(#44438,#44439,#44440,#44441,#44442,
#44443,#44444,#44445,#44446,#44447,#44448,#44449,#44450,#44451),
 .UNSPECIFIED.,.F.,.F.,(4,2,2,2,2,2,4),(4.24690342800971E-5,0.0511137139916916,
0.106332852431889,0.202821163335648,0.298258915813529,0.34872538483187,
0.405519954193255),.UNSPECIFIED.);
#683=B_SPLINE_CURVE_WITH_KNOTS('',3,(#44455,#44456,#44457,#44458,#44459,
#44460,#44461,#44462,#44463,#44464,#44465,#44466,#44467,#44468),
 .UNSPECIFIED.,.F.,.F.,(4,2,2,2,2,2,4),(1.58698352057749,1.61948213694375,
1.66708283695248,1.76538888902147,1.86226817876712,1.93594907832504,1.99997761942734),
 .UNSPECIFIED.);
#684=B_SPLINE_CURVE_WITH_KNOTS('',3,(#44469,#44470,#44471,#44472,#44473,
#44474,#44475,#44476,#44477,#44478,#44479,#44480,#44481,#44482,#44483,#44484,
#44485,#44486,#44487,#44488,#44489,#44490,#44491,#44492,#44493,#44494,#44495,
#44496,#44497,#44498,#44499,#44500,#44501,#44502),.UNSPECIFIED.,.F.,.F.,
(4,2,2,2,2,2,2,2,2,2,2,2,2,2,2,2,4),(0.000131786380904477,0.102860341713039,
0.137101926847378,0.217735363923029,0.315916468892578,0.397129195041746,
0.493796267586976,0.592181782019098,0.694353461838846,0.742150853821977,
0.793256700217311,0.841719577877637,0.943713479381191,0.991689068265629,
1.03881655518178,1.10792105895507,1.18423727595816),.UNSPECIFIED.);
#685=B_SPLINE_CURVE_WITH_KNOTS('',3,(#44507,#44508,#44509,#44510,#44511,
#44512,#44513,#44514,#44515,#44516,#44517,#44518,#44519,#44520,#44521,#44522,
#44523,#44524,#44525,#44526,#44527,#44528,#44529,#44530,#44531,#44532,#44533,
#44534,#44535,#44536,#44537,#44538,#44539,#44540,#44541,#44542,#44543,#44544,
#44545,#44546),.UNSPECIFIED.,.F.,.F.,(4,2,2,2,2,2,2,2,2,2,2,2,2,2,2,2,2,
2,2,4),(0.000233386320108365,0.0639084378333196,0.115738834875602,0.195580708942554,
0.296872775675836,0.395308850829062,0.468647278901977,0.569260147218536,
0.659264789203345,0.706236945833907,0.80709174491497,0.907905842929024,
1.00009797247216,1.09497639692093,1.19505864006617,1.28468085990641,1.33202875244464,
1.43127168932415,1.5301694640538,1.58698352057749),.UNSPECIFIED.);
#686=B_SPLINE_CURVE_WITH_KNOTS('',3,(#44548,#44549,#44550,#44551),
 .UNSPECIFIED.,.F.,.F.,(4,4),(0.405519954193255,0.405690998123473),
 .UNSPECIFIED.);
#687=B_SPLINE_CURVE_WITH_KNOTS('',3,(#44552,#44553,#44554,#44555,#44556,
#44557,#44558,#44559,#44560,#44561,#44562,#44563,#44564,#44565,#44566,#44567,
#44568,#44569,#44570,#44571,#44572,#44573,#44574,#44575,#44576,#44577,#44578,
#44579,#44580,#44581,#44582,#44583,#44584,#44585,#44586,#44587,#44588,#44589,
#44590,#44591,#44592,#44593,#44594,#44595,#44596,#44597,#44598,#44599,#44600,
#44601,#44602,#44603,#44604,#44605),.UNSPECIFIED.,.F.,.F.,(4,2,2,2,2,2,
2,2,2,2,2,2,2,2,2,2,2,2,2,2,2,2,2,2,2,2,4),(0.000315760721890317,0.0671794601159759,
0.142466537729481,0.190297899820453,0.238768166053594,0.332946663979359,
0.430541047971958,0.526554088588678,0.557936308139163,0.569901596811977,
0.668190233380715,0.742459118264126,0.784100177232852,0.847618599139215,
0.949980342343833,1.04534048049391,1.08870174690026,1.13607572013548,1.17545912833599,
1.22708032066423,1.32273981517142,1.36325156389753,1.42070337211726,1.48376830446815,
1.52647813490246,1.5929584678999,1.59372842373243),.UNSPECIFIED.);
#688=B_SPLINE_CURVE_WITH_KNOTS('',3,(#44611,#44612,#44613,#44614,#44615,
#44616,#44617,#44618,#44619,#44620,#44621,#44622),.UNSPECIFIED.,.F.,.F.,
(4,2,2,2,2,4),(1.73689377313444E-6,0.0397074682898225,0.0816374594028487,
0.160434126623339,0.243474988518188,0.320867562725843),.UNSPECIFIED.);
#689=B_SPLINE_CURVE_WITH_KNOTS('',3,(#44624,#44625,#44626,#44627,#44628,
#44629,#44630,#44631,#44632,#44633,#44634,#44635,#44636,#44637,#44638,#44639,
#44640,#44641,#44642,#44643,#44644,#44645,#44646,#44647,#44648,#44649,#44650,
#44651,#44652,#44653,#44654,#44655,#44656,#44657,#44658,#44659,#44660,#44661,
#44662,#44663,#44664,#44665,#44666,#44667,#44668,#44669,#44670,#44671,#44672,
#44673,#44674,#44675,#44676,#44677,#44678,#44679,#44680,#44681,#44682,#44683,
#44684,#44685,#44686,#44687,#44688,#44689,#44690,#44691,#44692,#44693,#44694,
#44695,#44696,#44697,#44698,#44699,#44700,#44701,#44702,#44703,#44704,#44705,
#44706,#44707,#44708,#44709,#44710,#44711,#44712,#44713,#44714,#44715,#44716,
#44717,#44718,#44719,#44720,#44721,#44722,#44723,#44724,#44725,#44726,#44727,
#44728,#44729,#44730,#44731,#44732,#44733,#44734,#44735,#44736,#44737,#44738,
#44739,#44740,#44741,#44742,#44743,#44744,#44745,#44746,#44747,#44748,#44749,
#44750,#44751,#44752,#44753,#44754,#44755,#44756,#44757,#44758,#44759,#44760,
#44761,#44762,#44763,#44764,#44765,#44766,#44767,#44768,#44769,#44770,#44771,
#44772,#44773,#44774,#44775,#44776,#44777,#44778,#44779,#44780,#44781,#44782,
#44783,#44784,#44785,#44786,#44787,#44788,#44789,#44790,#44791,#44792,#44793,
#44794,#44795,#44796,#44797,#44798,#44799,#44800,#44801,#44802,#44803,#44804,
#44805,#44806,#44807,#44808,#44809,#44810,#44811,#44812,#44813,#44814,#44815,
#44816,#44817,#44818,#44819,#44820,#44821,#44822,#44823,#44824,#44825,#44826,
#44827,#44828,#44829,#44830,#44831,#44832,#44833,#44834,#44835,#44836,#44837,
#44838,#44839,#44840),.UNSPECIFIED.,.F.,.F.,(4,3,3,3,3,3,3,3,3,3,3,3,3,
3,3,3,3,3,3,3,3,3,3,3,3,3,3,3,3,3,3,3,3,3,3,3,3,3,3,3,3,3,3,3,3,3,3,3,3,
3,3,3,3,3,3,3,3,3,3,3,3,3,3,3,3,3,3,3,3,3,3,3,4),(5.31095027518764E-9,0.0191480404307811,
0.0268229569350739,0.0537675131188631,0.0804193339369082,0.0843763580558497,
0.0843766029239374,0.101824284415583,0.128087669003448,0.154826539242901,
0.181716882619413,0.203526770072898,0.229033516898158,0.2304418928167,0.25225492212391,
0.252260389184945,0.278990758257123,0.305132042464289,0.331749499982824,
0.358645858343833,0.385359014779447,0.406654209945588,0.42008278387528,
0.42009020951023,0.446361881136987,0.473090671353263,0.499996599516834,
0.508103946120237,0.534910171633633,0.561786915448796,0.586626585034112,
0.587962078272053,0.587964325643741,0.609493007642893,0.635865341378628,
0.662650747975075,0.689502249238686,0.710830175716059,0.735593555674911,
0.737737642485696,0.755707788969607,0.755715461128941,0.78036338986414,
0.782248582456849,0.809125623044456,0.812119352707047,0.838818701113506,
0.865764132225303,0.892456173463476,0.914207349002946,0.923466604850516,
0.923484364288651,0.948200823019635,0.949743733247729,0.976471741845332,
1.00339540898673,1.01588539484221,1.04269403687978,1.06814092402567,1.06958141316705,
1.09127739827948,1.09129934073672,1.11545127759809,1.11714505442693,1.14363806036283,
1.17047970433824,1.19722878067902,1.21807739682823,1.24123199345686,1.24517381391668,
1.25897306563341,1.25900354475818,1.27023098040024),.UNSPECIFIED.);
#690=B_SPLINE_CURVE_WITH_KNOTS('',3,(#44841,#44842,#44843,#44844),
 .UNSPECIFIED.,.F.,.F.,(4,4),(3.1560069292801E-5,0.000233386320108365),
 .UNSPECIFIED.);
#691=B_SPLINE_CURVE_WITH_KNOTS('',3,(#44846,#44847,#44848,#44849,#44850,
#44851,#44852,#44853,#44854,#44855,#44856,#44857,#44858,#44859,#44860,#44861,
#44862,#44863,#44864,#44865,#44866,#44867,#44868,#44869,#44870,#44871,#44872,
#44873,#44874,#44875,#44876,#44877,#44878,#44879,#44880,#44881,#44882,#44883,
#44884,#44885,#44886,#44887,#44888,#44889,#44890,#44891,#44892,#44893),
 .UNSPECIFIED.,.F.,.F.,(4,2,2,2,2,2,2,2,2,2,2,2,2,2,2,2,2,2,2,2,2,2,2,4),
(1.59372842373243,1.63638854674833,1.66111458565455,1.71028293204707,1.80937505144961,
1.91074393718392,1.95971059032954,2.05862989243709,2.10831236150241,2.15712578278928,
2.20499253693922,2.3068209642726,2.35606089004449,2.40548038645003,2.45275661630416,
2.55280385060893,2.59920187815348,2.68412836559863,2.76983887215137,2.87102125912343,
2.95553213085994,3.05760109679623,3.1222894965372,3.18599763231299),
 .UNSPECIFIED.);
#692=B_SPLINE_CURVE_WITH_KNOTS('',3,(#44894,#44895,#44896,#44897),
 .UNSPECIFIED.,.F.,.F.,(4,4),(1.00000009672838E-6,6.17888066936219E-5),
 .UNSPECIFIED.);
#693=B_SPLINE_CURVE_WITH_KNOTS('',3,(#44903,#44904,#44905,#44906,#44907,
#44908,#44909,#44910),.UNSPECIFIED.,.F.,.F.,(4,2,2,4),(1.58569301455726,
1.587634805142,1.6706642559489,1.74161014133595),.UNSPECIFIED.);
#694=B_SPLINE_CURVE_WITH_KNOTS('',3,(#44911,#44912,#44913,#44914,#44915,
#44916,#44917,#44918,#44919,#44920,#44921,#44922,#44923,#44924,#44925,#44926,
#44927,#44928,#44929,#44930,#44931,#44932,#44933,#44934,#44935,#44936,#44937,
#44938,#44939,#44940,#44941,#44942,#44943,#44944,#44945,#44946,#44947,#44948,
#44949,#44950,#44951,#44952,#44953,#44954,#44955,#44956,#44957,#44958,#44959,
#44960,#44961,#44962,#44963,#44964,#44965,#44966,#44967,#44968,#44969,#44970,
#44971,#44972,#44973,#44974,#44975,#44976,#44977,#44978,#44979,#44980,#44981,
#44982,#44983,#44984,#44985,#44986,#44987,#44988,#44989,#44990,#44991,#44992,
#44993,#44994,#44995,#44996,#44997,#44998,#44999,#45000,#45001,#45002,#45003,
#45004,#45005,#45006,#45007,#45008,#45009,#45010,#45011,#45012,#45013,#45014,
#45015,#45016,#45017,#45018,#45019,#45020,#45021,#45022,#45023,#45024,#45025,
#45026,#45027,#45028,#45029,#45030,#45031,#45032,#45033,#45034,#45035,#45036,
#45037,#45038,#45039,#45040,#45041,#45042,#45043,#45044,#45045,#45046,#45047,
#45048,#45049,#45050,#45051,#45052,#45053,#45054,#45055,#45056,#45057,#45058,
#45059,#45060,#45061,#45062,#45063,#45064,#45065,#45066,#45067,#45068,#45069,
#45070,#45071,#45072,#45073,#45074,#45075,#45076,#45077,#45078,#45079,#45080,
#45081,#45082,#45083,#45084,#45085,#45086,#45087,#45088,#45089,#45090,#45091,
#45092,#45093,#45094,#45095,#45096,#45097,#45098,#45099,#45100,#45101,#45102,
#45103,#45104,#45105,#45106,#45107,#45108,#45109,#45110,#45111,#45112,#45113,
#45114,#45115,#45116,#45117,#45118,#45119,#45120,#45121,#45122,#45123,#45124,
#45125,#45126,#45127,#45128,#45129,#45130,#45131,#45132,#45133,#45134,#45135,
#45136,#45137,#45138,#45139,#45140,#45141,#45142,#45143,#45144,#45145,#45146,
#45147,#45148,#45149,#45150,#45151,#45152,#45153,#45154,#45155,#45156,#45157,
#45158,#45159,#45160,#45161,#45162,#45163,#45164,#45165,#45166,#45167,#45168,
#45169,#45170,#45171,#45172,#45173,#45174,#45175,#45176,#45177,#45178,#45179,
#45180,#45181,#45182,#45183,#45184),.UNSPECIFIED.,.F.,.F.,(4,3,3,3,3,3,
3,3,3,3,3,3,3,3,3,3,3,3,3,3,3,3,3,3,3,3,3,3,3,3,3,3,3,3,3,3,3,3,3,3,3,3,
3,3,3,3,3,3,3,3,3,3,3,3,3,3,3,3,3,3,3,3,3,3,3,3,3,3,3,3,3,3,3,3,3,3,3,3,
3,3,3,3,3,3,3,3,3,3,3,3,3,4),(9.9865186199412E-8,0.0165170009540119,0.0269560963403509,
0.0516026360833156,0.0539939918893045,0.0619549903004816,0.0619569561518245,
0.0869496139842535,0.0887864088251827,0.102132027133151,0.129070531766969,
0.156009036400786,0.156009728784879,0.182902541024912,0.203851549956986,
0.230680355193655,0.250043336119814,0.250048492305348,0.275626936708897,
0.27764556096622,0.305247785812627,0.331937887925211,0.358922694967677,
0.375449181557498,0.37545383194231,0.400488263889334,0.402335048584807,
0.406320547266745,0.432920095075976,0.45984166967008,0.486692519308316,
0.500786019934413,0.500788193121711,0.507023039110945,0.53343108396808,
0.560251627646521,0.587156442098039,0.607377499256687,0.626067946696661,
0.626075385929146,0.652594867406431,0.679484622591304,0.696616153907565,
0.696623115086315,0.7074659160348,0.7339706204339,0.760896048377414,0.767095742268224,
0.767103284580723,0.794002576058669,0.807301789010731,0.833952495633197,
0.83754118627808,0.837547573059014,0.864398365331485,0.89120989339632,0.90682027159049,
0.908049260110694,0.908057170500754,0.934401369183197,0.961199033620948,
0.988154790632044,1.00602308450473,1.03060487918097,1.03298575801758,1.04901141337422,
1.04901899068072,1.07364088767949,1.07699866077235,1.10313522477293,1.10498590817048,
1.13172938424021,1.15873452930581,1.18360272650853,1.18560295888011,1.19002020304435,
1.19002635837203,1.20371732313993,1.23017716258453,1.25705058603626,1.2840098004507,
1.30214552504217,1.32624464129826,1.32907950882834,1.3309467369147,1.33095133640406,
1.35586247307618,1.35752131148749,1.38448911199129,1.40027033128569,1.42754750616507,
1.43259500515056),.UNSPECIFIED.);
#695=B_SPLINE_CURVE_WITH_KNOTS('',3,(#45186,#45187,#45188,#45189,#45190,
#45191,#45192,#45193,#45194,#45195,#45196,#45197,#45198,#45199,#45200,#45201,
#45202,#45203,#45204,#45205,#45206,#45207),.UNSPECIFIED.,.F.,.F.,(4,2,2,
2,2,2,2,2,2,2,4),(6.17888066936219E-5,0.0952321659214813,0.168572142996074,
0.269154246669155,0.361233599404335,0.462276827673878,0.552734576636099,
0.650535735082581,0.737701663102056,0.835191426558474,0.924653665098687),
 .UNSPECIFIED.);
#696=B_SPLINE_CURVE_WITH_KNOTS('',3,(#45208,#45209,#45210,#45211,#45212,
#45213,#45214,#45215,#45216,#45217,#45218,#45219,#45220,#45221,#45222,#45223,
#45224,#45225,#45226,#45227,#45228,#45229,#45230,#45231,#45232,#45233,#45234,
#45235,#45236,#45237,#45238,#45239,#45240,#45241,#45242,#45243,#45244,#45245,
#45246,#45247,#45248,#45249,#45250,#45251,#45252,#45253,#45254,#45255,#45256,
#45257,#45258,#45259,#45260,#45261,#45262,#45263,#45264,#45265,#45266,#45267,
#45268,#45269,#45270,#45271,#45272,#45273,#45274,#45275,#45276,#45277,#45278,
#45279,#45280,#45281,#45282,#45283,#45284,#45285,#45286,#45287,#45288,#45289,
#45290,#45291,#45292,#45293,#45294,#45295,#45296,#45297,#45298,#45299,#45300,
#45301,#45302,#45303,#45304,#45305,#45306,#45307,#45308,#45309,#45310,#45311,
#45312,#45313,#45314,#45315,#45316,#45317,#45318,#45319,#45320,#45321,#45322,
#45323,#45324,#45325,#45326,#45327,#45328,#45329,#45330,#45331,#45332,#45333,
#45334,#45335,#45336,#45337,#45338,#45339,#45340),.UNSPECIFIED.,.F.,.F.,
(4,3,3,3,3,3,3,3,3,3,3,3,3,3,3,3,3,3,3,3,3,3,3,3,3,3,3,3,3,3,3,3,3,3,3,
3,3,3,3,3,3,3,3,3,4),(1.66970259518317E-7,0.0195408023283141,0.0268240864561452,
0.0519109008684237,0.0519127124963912,0.0787226617260139,0.101671370691236,
0.107856553210952,0.107858116237918,0.132586573240225,0.135853998461347,
0.159529331929515,0.163849880684776,0.163855488459842,0.188513397271807,
0.190494891911395,0.203248940230886,0.229557891457817,0.256333149896959,
0.283269519729177,0.304748770645336,0.330172222241103,0.331703685429797,
0.356398100810531,0.35966945417196,0.383548279581913,0.386117015489908,
0.387635222914124,0.387651295959121,0.406179501373845,0.43224435118395,
0.458879218217511,0.485890019786178,0.507549821109392,0.534529392192245,
0.559845427216043,0.561539389676409,0.585730024157773,0.587972179090907,
0.608868993160356,0.61130729451897,0.611324084570082,0.635027594176061,
0.637557052005942,0.662236219249742),.UNSPECIFIED.);
#697=B_SPLINE_CURVE_WITH_KNOTS('',3,(#45345,#45346,#45347,#45348,#45349,
#45350,#45351,#45352,#45353,#45354,#45355,#45356,#45357,#45358,#45359,#45360,
#45361,#45362,#45363,#45364,#45365,#45366,#45367,#45368,#45369,#45370,#45371,
#45372,#45373,#45374,#45375,#45376,#45377,#45378,#45379,#45380,#45381,#45382,
#45383,#45384,#45385,#45386),.UNSPECIFIED.,.F.,.F.,(4,2,2,2,2,2,2,2,2,2,
2,2,2,2,2,2,2,2,2,2,4),(0.000200192691012083,0.0459634654450998,0.0897981263797104,
0.182563617677864,0.23043629516319,0.331499932350853,0.379339465965364,
0.480419798577262,0.572564637956923,0.622450255663974,0.723703481811166,
0.770906047985159,0.870735642587249,0.971506320484368,1.06104297895876,
1.16195264040926,1.25685403264272,1.30560365648842,1.39440414562203,1.49505415995523,
1.58569301455726),.UNSPECIFIED.);
#698=B_SPLINE_CURVE_WITH_KNOTS('',3,(#45387,#45388,#45389,#45390,#45391,
#45392,#45393,#45394,#45395,#45396,#45397,#45398,#45399,#45400,#45401,#45402,
#45403,#45404,#45405,#45406,#45407,#45408,#45409,#45410,#45411,#45412,#45413,
#45414,#45415,#45416,#45417,#45418,#45419,#45420,#45421,#45422,#45423,#45424,
#45425,#45426,#45427,#45428),.UNSPECIFIED.,.F.,.F.,(4,2,2,2,2,2,2,2,2,2,
2,2,2,2,2,2,2,2,2,2,4),(7.91614227771307E-5,0.0600035764138198,0.107716099660701,
0.18322851806419,0.284460041175081,0.377847341356911,0.465640487399806,
0.559597868052173,0.636518057225568,0.737491713471269,0.832117269395779,
0.925832800560101,0.975014451851033,1.07607976212091,1.1240775948849,1.22516313586639,
1.31513822178404,1.40585346672917,1.45293493568029,1.55386692466454,1.58754532392759),
 .UNSPECIFIED.);
#699=B_SPLINE_CURVE_WITH_KNOTS('',3,(#45434,#45435,#45436,#45437,#45438,
#45439),.UNSPECIFIED.,.F.,.F.,(4,2,4),(0.000101837034550224,0.0201470223705077,
0.0401954933212442),.UNSPECIFIED.);
#700=B_SPLINE_CURVE_WITH_KNOTS('',3,(#45441,#45442,#45443,#45444,#45445,
#45446,#45447,#45448,#45449,#45450,#45451,#45452,#45453,#45454,#45455,#45456,
#45457,#45458,#45459,#45460,#45461,#45462,#45463,#45464,#45465,#45466,#45467,
#45468,#45469,#45470,#45471,#45472,#45473,#45474,#45475,#45476,#45477,#45478,
#45479,#45480,#45481,#45482,#45483,#45484,#45485,#45486,#45487,#45488,#45489,
#45490,#45491,#45492,#45493,#45494,#45495,#45496,#45497,#45498,#45499,#45500,
#45501,#45502,#45503,#45504,#45505,#45506,#45507,#45508,#45509,#45510,#45511,
#45512,#45513,#45514,#45515,#45516,#45517,#45518,#45519,#45520,#45521,#45522,
#45523,#45524,#45525,#45526,#45527,#45528,#45529,#45530,#45531,#45532,#45533,
#45534,#45535,#45536,#45537,#45538,#45539,#45540,#45541,#45542,#45543,#45544,
#45545,#45546,#45547,#45548,#45549,#45550,#45551,#45552,#45553,#45554,#45555,
#45556,#45557,#45558,#45559,#45560,#45561,#45562,#45563,#45564,#45565,#45566,
#45567,#45568,#45569,#45570,#45571,#45572,#45573,#45574,#45575,#45576,#45577,
#45578,#45579,#45580,#45581,#45582,#45583,#45584,#45585,#45586,#45587,#45588,
#45589,#45590,#45591,#45592,#45593,#45594,#45595,#45596,#45597,#45598,#45599,
#45600,#45601,#45602,#45603,#45604,#45605,#45606,#45607,#45608,#45609,#45610,
#45611,#45612,#45613,#45614,#45615,#45616,#45617,#45618,#45619,#45620,#45621,
#45622,#45623,#45624,#45625,#45626,#45627,#45628,#45629,#45630,#45631,#45632,
#45633,#45634,#45635,#45636,#45637,#45638,#45639,#45640,#45641,#45642,#45643,
#45644,#45645,#45646,#45647,#45648,#45649,#45650,#45651,#45652,#45653,#45654,
#45655,#45656,#45657,#45658,#45659,#45660,#45661,#45662,#45663,#45664,#45665,
#45666,#45667,#45668,#45669,#45670,#45671,#45672,#45673,#45674,#45675,#45676,
#45677,#45678,#45679,#45680,#45681,#45682,#45683,#45684,#45685,#45686,#45687,
#45688,#45689,#45690,#45691,#45692,#45693,#45694,#45695,#45696,#45697,#45698,
#45699,#45700,#45701,#45702,#45703,#45704,#45705,#45706,#45707,#45708,#45709,
#45710,#45711,#45712,#45713,#45714,#45715,#45716,#45717,#45718,#45719,#45720,
#45721,#45722,#45723,#45724,#45725,#45726,#45727,#45728,#45729,#45730,#45731,
#45732,#45733,#45734,#45735,#45736,#45737,#45738,#45739,#45740,#45741,#45742,
#45743,#45744,#45745,#45746,#45747,#45748,#45749,#45750,#45751,#45752,#45753,
#45754,#45755,#45756,#45757,#45758,#45759,#45760,#45761,#45762,#45763,#45764,
#45765,#45766,#45767,#45768,#45769,#45770,#45771,#45772,#45773,#45774),
 .UNSPECIFIED.,.F.,.F.,(4,3,3,3,3,3,3,3,3,3,3,3,3,3,3,3,3,3,3,3,3,3,3,3,
3,3,3,3,3,3,3,3,3,3,3,3,3,3,3,3,3,3,3,3,3,3,3,3,3,3,3,3,3,3,3,3,3,3,3,3,
3,3,3,3,3,3,3,3,3,3,3,3,3,3,3,3,3,3,3,3,3,3,3,3,3,3,3,3,3,3,3,3,3,3,3,3,
3,3,3,3,3,3,3,3,3,3,3,3,3,3,3,4),(1.13292399530795E-7,0.0196928172933993,
0.0266956052075354,0.0503343617400793,0.0503391750759571,0.0643522297958899,
0.0643568684523188,0.0783591425935286,0.0783636026936431,0.101669107471721,
0.106302158127171,0.10630630451195,0.132795584592458,0.159597319790963,
0.162302887343916,0.162305864602742,0.189092019568487,0.203245868153258,
0.229777136283039,0.256613075626682,0.274235080436413,0.274235407135105,
0.301001096463727,0.304744104831594,0.331238225509686,0.358684698041346,
0.386131170573007,0.38613449810665,0.406172508592631,0.43259369534683,0.442014502970311,
0.442018453364401,0.470004342403802,0.49651923133194,0.497994181837294,
0.497999165742914,0.507541553513218,0.511940966359407,0.511946066546157,
0.525904535910578,0.525909869558653,0.549360849797592,0.551878270558614,
0.553893887146288,0.553898924376285,0.57841459029774,0.581377056379963,
0.604299021973496,0.608860225613638,0.609832456494235,0.633649156002123,
0.635717416259916,0.660670639785913,0.662198734481889,0.68917737665926,
0.711164765300409,0.738063711508917,0.765100247087221,0.790181412556859,
0.791720097711544,0.813130447497351,0.833487150899675,0.833496210994393,
0.856625714233385,0.859629993596308,0.88383669019327,0.887179645735812,
0.912669305169198,0.914729297875317,0.941517269106251,0.968556178625948,
0.995326318254519,1.01591627739398,1.03859646750578,1.04288287816545,1.05715560698756,
1.05717054613622,1.07968191134433,1.08347164461366,1.10689777465868,1.11035077795206,
1.11674748200187,1.14331205720645,1.17025616513136,1.19714941760193,1.21732834413762,
1.24062535644877,1.24433976862262,1.26683620881214,1.2711512358007,1.28081358130734,
1.28082854039954,1.30299671904022,1.30754584512882,1.31764387528724,1.34227944172055,
1.34399381708511,1.37082761041625,1.39786781667107,1.41761477840521,1.44291220243535,
1.44462869140057,1.46870092111847,1.47164935363387,1.49471334104812,1.49819054458882,
1.50442526885582,1.50443667340995,1.51726643247651,1.54198728460159,1.5439713432008,
1.55104955739032),.UNSPECIFIED.);
#701=B_SPLINE_CURVE_WITH_KNOTS('',3,(#45775,#45776,#45777,#45778),
 .UNSPECIFIED.,.F.,.F.,(4,4),(9.65841270823929E-5,0.000200192691012083),
 .UNSPECIFIED.);
#702=B_SPLINE_CURVE_WITH_KNOTS('',3,(#45780,#45781,#45782,#45783,#45784,
#45785,#45786,#45787,#45788,#45789,#45790,#45791,#45792,#45793,#45794,#45795,
#45796,#45797,#45798,#45799,#45800,#45801,#45802,#45803,#45804,#45805,#45806,
#45807),.UNSPECIFIED.,.F.,.F.,(4,2,2,2,2,2,2,2,2,2,2,2,2,4),(1.58754532392759,
1.65173348850276,1.69990823036454,1.79097132992545,1.89214817054913,1.99098341671071,
2.08088116422555,2.12847676160414,2.22733163510097,2.32484132890977,2.41387565781255,
2.46207264157115,2.55303228913833,2.63023061161303),.UNSPECIFIED.);
#703=B_SPLINE_CURVE_WITH_KNOTS('',3,(#45808,#45809,#45810,#45811,#45812,
#45813,#45814,#45815,#45816,#45817,#45818,#45819,#45820,#45821,#45822,#45823),
 .UNSPECIFIED.,.F.,.F.,(4,2,2,2,2,2,2,4),(0.000441888379867055,0.0712123258361295,
0.153637230093539,0.24663025572483,0.348304026319509,0.43875400981342,0.540436997579012,
0.543345573804166),.UNSPECIFIED.);
#704=B_SPLINE_CURVE_WITH_KNOTS('',3,(#45826,#45827,#45828,#45829,#45830,
#45831,#45832,#45833,#45834,#45835,#45836,#45837,#45838,#45839,#45840,#45841,
#45842,#45843,#45844,#45845,#45846,#45847,#45848,#45849,#45850,#45851,#45852,
#45853,#45854,#45855,#45856,#45857,#45858,#45859,#45860,#45861),
 .UNSPECIFIED.,.F.,.F.,(4,2,2,2,2,2,2,2,2,2,2,2,2,2,2,2,2,4),(0.543345573804166,
0.632883876225489,0.681859177676299,0.777577268298339,0.828233852261912,
0.877156775277406,0.978121049434662,1.0758107655072,1.12427682326688,1.22286953667497,
1.27082359754074,1.31918246207647,1.41998339373079,1.46885416546689,1.56843982737443,
1.61487450414648,1.68703359300301,1.75359080947889),.UNSPECIFIED.);
#705=B_SPLINE_CURVE_WITH_KNOTS('',3,(#45863,#45864,#45865,#45866,#45867,
#45868,#45869,#45870,#45871,#45872,#45873,#45874),.UNSPECIFIED.,.F.,.F.,
(4,2,2,2,2,4),(2.38764650524234E-5,0.0874762242858372,0.16161100104167,
0.263824592583728,0.351221429605352,0.377547520539708),.UNSPECIFIED.);
#706=B_SPLINE_CURVE_WITH_KNOTS('',3,(#45877,#45878,#45879,#45880,#45881,
#45882,#45883,#45884,#45885,#45886,#45887,#45888,#45889,#45890,#45891,#45892,
#45893,#45894,#45895,#45896,#45897,#45898,#45899,#45900,#45901,#45902,#45903,
#45904,#45905,#45906,#45907,#45908,#45909,#45910,#45911,#45912,#45913,#45914,
#45915,#45916),.UNSPECIFIED.,.F.,.F.,(4,2,2,2,2,2,2,2,2,2,2,2,2,2,2,2,2,
2,2,4),(2.87435079942613,2.90908627921352,2.99959019849851,3.09707993844391,
3.19714155267547,3.24484909228093,3.32636302699049,3.37071831260431,3.47159691287487,
3.56386995533199,3.65864007403778,3.75026808820601,3.84557562826543,3.9357192189986,
4.03247844544094,4.12174025181586,4.21882481577015,4.30566738965663,4.38862465799223,
4.45293375202886),.UNSPECIFIED.);
#707=B_SPLINE_CURVE_WITH_KNOTS('',3,(#45921,#45922,#45923,#45924,#45925,
#45926,#45927,#45928,#45929,#45930,#45931,#45932,#45933,#45934,#45935,#45936,
#45937,#45938,#45939,#45940,#45941,#45942,#45943,#45944,#45945,#45946,#45947,
#45948,#45949,#45950,#45951,#45952,#45953,#45954,#45955,#45956,#45957,#45958,
#45959,#45960,#45961,#45962),.UNSPECIFIED.,.F.,.F.,(4,2,2,2,2,2,2,2,2,2,
2,2,2,2,2,2,2,2,2,2,4),(1.29092315943205,1.38003890819178,1.47665828500728,
1.57754789064784,1.67848491879225,1.72634519454726,1.82718775987331,1.92805302106637,
1.97630062959479,2.07710589502321,2.17789125240703,2.22607075099038,2.32681039747117,
2.37675450699215,2.42514659011588,2.4721963487193,2.57324684507597,2.66851111481085,
2.76013041155395,2.8078211904013,2.87435079942613),.UNSPECIFIED.);
#708=B_SPLINE_CURVE_WITH_KNOTS('',3,(#45963,#45964,#45965,#45966,#45967,
#45968,#45969,#45970,#45971,#45972,#45973,#45974,#45975,#45976,#45977,#45978,
#45979,#45980,#45981,#45982,#45983,#45984,#45985,#45986,#45987,#45988,#45989,
#45990,#45991,#45992,#45993,#45994,#45995,#45996,#45997,#45998,#45999,#46000,
#46001,#46002),.UNSPECIFIED.,.F.,.F.,(4,2,2,2,2,2,2,2,2,2,2,2,2,2,2,2,2,
2,2,4),(0.377547520539708,0.452910059858426,0.497939063488615,0.581559294711028,
0.683061141383824,0.782198397513139,0.86638087248029,0.963221943764175,
1.03590139751064,1.1371715237912,1.23381855972917,1.32919735940209,1.42389091389379,
1.48878364666316,1.53500546453752,1.63207294506492,1.73242395947659,1.83142774699405,
1.92407009339033,1.9660107665537),.UNSPECIFIED.);
#709=B_SPLINE_CURVE_WITH_KNOTS('',3,(#46008,#46009,#46010,#46011,#46012,
#46013,#46014,#46015,#46016,#46017),.UNSPECIFIED.,.F.,.F.,(4,2,2,2,4),(1.58631321662086,
1.61402560378215,1.70207985040979,1.8000208134824,1.88377373488638),
 .UNSPECIFIED.);
#710=B_SPLINE_CURVE_WITH_KNOTS('',3,(#46018,#46019,#46020,#46021,#46022,
#46023,#46024,#46025,#46026,#46027,#46028,#46029,#46030,#46031,#46032,#46033,
#46034,#46035,#46036,#46037,#46038,#46039,#46040,#46041,#46042,#46043,#46044,
#46045,#46046,#46047,#46048,#46049,#46050,#46051,#46052,#46053,#46054,#46055,
#46056,#46057),.UNSPECIFIED.,.F.,.F.,(4,2,2,2,2,2,2,2,2,2,2,2,2,2,2,2,2,
2,2,4),(0.000337110448919753,0.0674382068481336,0.137790147250154,0.239065013113051,
0.325530449406533,0.422867756755189,0.512760640130854,0.605322501628678,
0.654807814067912,0.703885264670299,0.802873350225715,0.850409666676142,
0.899945799232159,0.949788722546396,1.04782193719607,1.09611534977182,1.14511541496357,
1.2384972774798,1.28809781873481,1.29092315943205),.UNSPECIFIED.);
#711=B_SPLINE_CURVE_WITH_KNOTS('',3,(#46059,#46060,#46061,#46062,#46063,
#46064,#46065,#46066,#46067,#46068,#46069,#46070,#46071,#46072,#46073,#46074,
#46075,#46076,#46077,#46078,#46079,#46080,#46081,#46082,#46083,#46084,#46085,
#46086,#46087,#46088,#46089,#46090,#46091,#46092),.UNSPECIFIED.,.F.,.F.,
(4,2,2,2,2,2,2,2,2,2,2,2,2,2,2,2,4),(1.9660107665537,2.02581281643668,2.12619938236871,
2.21649199339821,2.26384716561196,2.36159447778931,2.40948822197726,2.51058228712726,
2.60378230877955,2.69946776093669,2.74743080058653,2.8482918561081,2.94186174762132,
3.03568405796453,3.08339710005034,3.18073503357408,3.26409879879059),
 .UNSPECIFIED.);
#712=B_SPLINE_CURVE_WITH_KNOTS('',3,(#46093,#46094,#46095,#46096,#46097,
#46098,#46099,#46100,#46101,#46102),.UNSPECIFIED.,.F.,.F.,(4,2,2,2,4),(0.000401396573765282,
0.0767267724924665,0.171583258256695,0.259711836113359,0.289709300215736),
 .UNSPECIFIED.);
#713=B_SPLINE_CURVE_WITH_KNOTS('',3,(#46107,#46108,#46109,#46110,#46111,
#46112,#46113,#46114,#46115,#46116,#46117,#46118,#46119,#46120,#46121,#46122,
#46123,#46124,#46125,#46126,#46127,#46128,#46129,#46130,#46131,#46132,#46133,
#46134,#46135,#46136,#46137,#46138,#46139,#46140,#46141,#46142,#46143,#46144,
#46145,#46146,#46147,#46148),.UNSPECIFIED.,.F.,.F.,(4,2,2,2,2,2,2,2,2,2,
2,2,2,2,2,2,2,2,2,2,4),(6.19917750705267E-6,0.0779101723467662,0.163347403591141,
0.211369088637002,0.309559385368541,0.403161961538505,0.45435016612089,
0.546763115962883,0.596854200931595,0.6977571810982,0.744652526768696,0.844613323634994,
0.941898523491601,1.03126364841854,1.1324037693941,1.22675848757232,1.32139054199484,
1.36966233595816,1.47055391734561,1.56509118248676,1.58631321662086),
 .UNSPECIFIED.);
#714=B_SPLINE_CURVE_WITH_KNOTS('',3,(#46149,#46150,#46151,#46152,#46153,
#46154,#46155,#46156,#46157,#46158,#46159,#46160,#46161,#46162,#46163,#46164,
#46165,#46166,#46167,#46168,#46169,#46170,#46171,#46172,#46173,#46174,#46175,
#46176,#46177,#46178,#46179,#46180,#46181,#46182,#46183,#46184,#46185,#46186,
#46187,#46188,#46189,#46190),.UNSPECIFIED.,.F.,.F.,(4,2,2,2,2,2,2,2,2,2,
2,2,2,2,2,2,2,2,2,2,4),(0.289709300215736,0.354159359873933,0.450430540051697,
0.545790968368503,0.638492687552296,0.740854867193477,0.788324960692327,
0.879895408610432,0.976079549455883,1.07768471355924,1.17678702801279,1.22541491119139,
1.32694131959504,1.42604352921976,1.51879959847725,1.61507782511401,1.66515194848187,
1.71454858187282,1.8160243538418,1.86442895008864,1.88361728507473),
 .UNSPECIFIED.);
#715=B_SPLINE_CURVE_WITH_KNOTS('',3,(#46196,#46197,#46198,#46199,#46200,
#46201,#46202,#46203,#46204,#46205),.UNSPECIFIED.,.F.,.F.,(4,2,2,2,4),(1.19987423408312E-5,
0.0502654517634361,0.102318195477417,0.154980355752334,0.204643884264344),
 .UNSPECIFIED.);
#716=B_SPLINE_CURVE_WITH_KNOTS('',3,(#46206,#46207,#46208,#46209,#46210,
#46211,#46212,#46213,#46214,#46215,#46216,#46217,#46218,#46219,#46220,#46221,
#46222,#46223,#46224,#46225,#46226,#46227,#46228,#46229,#46230,#46231,#46232,
#46233,#46234,#46235,#46236,#46237,#46238,#46239,#46240,#46241,#46242,#46243,
#46244,#46245,#46246,#46247,#46248,#46249,#46250,#46251,#46252,#46253,#46254,
#46255,#46256,#46257,#46258,#46259,#46260,#46261,#46262,#46263,#46264,#46265,
#46266,#46267,#46268,#46269,#46270,#46271,#46272,#46273,#46274,#46275,#46276,
#46277,#46278,#46279,#46280,#46281,#46282,#46283,#46284,#46285,#46286,#46287,
#46288,#46289,#46290,#46291,#46292,#46293,#46294,#46295,#46296,#46297,#46298,
#46299,#46300,#46301,#46302,#46303,#46304,#46305,#46306,#46307,#46308,#46309,
#46310,#46311,#46312,#46313,#46314,#46315,#46316,#46317,#46318,#46319,#46320,
#46321,#46322,#46323,#46324,#46325,#46326,#46327,#46328,#46329,#46330,#46331,
#46332,#46333,#46334,#46335,#46336,#46337,#46338,#46339,#46340,#46341,#46342,
#46343,#46344,#46345,#46346,#46347,#46348,#46349,#46350,#46351,#46352,#46353,
#46354,#46355,#46356,#46357,#46358,#46359,#46360,#46361,#46362,#46363,#46364,
#46365,#46366,#46367,#46368,#46369,#46370,#46371,#46372,#46373,#46374,#46375,
#46376,#46377,#46378,#46379,#46380,#46381,#46382,#46383,#46384,#46385,#46386,
#46387,#46388,#46389,#46390,#46391,#46392,#46393,#46394,#46395,#46396,#46397,
#46398,#46399,#46400,#46401,#46402,#46403,#46404,#46405,#46406,#46407,#46408,
#46409,#46410,#46411,#46412,#46413,#46414,#46415,#46416,#46417,#46418,#46419,
#46420,#46421,#46422,#46423,#46424,#46425,#46426,#46427,#46428,#46429,#46430,
#46431,#46432,#46433,#46434,#46435,#46436,#46437,#46438,#46439,#46440,#46441,
#46442,#46443,#46444,#46445,#46446,#46447,#46448,#46449,#46450,#46451,#46452,
#46453,#46454,#46455,#46456,#46457,#46458,#46459,#46460,#46461,#46462,#46463,
#46464),.UNSPECIFIED.,.F.,.F.,(4,3,3,3,3,3,3,3,3,3,3,3,3,3,3,3,3,3,3,3,
3,3,3,3,3,3,3,3,3,3,3,3,3,3,3,3,3,3,3,3,3,3,3,3,3,3,3,3,3,3,3,3,3,3,3,3,
3,3,3,3,3,3,3,3,3,3,3,3,3,3,3,3,3,3,3,3,3,3,3,3,3,3,3,3,3,3,4),(1.33217227012311E-6,
0.0194681700743097,0.0267673112323403,0.0538008962348333,0.080584107915861,
0.101824443115546,0.126382254351437,0.128808154219708,0.140308379837731,
0.140331736201363,0.166497871296857,0.19194180857669,0.19335702062781,0.20352684729289,
0.23008128254457,0.257031409529791,0.28393764637694,0.305131966797111,0.329862153890025,
0.332137147300207,0.356221787991884,0.358969880802285,0.364186795008282,
0.364202261631717,0.388450168684,0.390849182797679,0.406654235569055,0.433023159921676,
0.459871705874179,0.486876245718093,0.508104082639558,0.533473857623085,
0.535121215478853,0.559667655210642,0.561941015242435,0.585613447401546,
0.587965212525989,0.587976323639518,0.609493077799452,0.63563971386527,
0.66232974601657,0.689346315814045,0.710830182576537,0.737822771061955,
0.762959610043142,0.764824563091553,0.788879951220074,0.791243080925086,
0.811643835672881,0.811657693323187,0.812119505296254,0.835513511256599,
0.837989836435306,0.862562815089907,0.864474914866434,0.891489423335006,
0.914208690295899,0.941141317294609,0.968210960766913,0.992952266363267,
0.994832587480743,1.0158936331595,1.03529802723853,1.03531295234316,1.05822446086301,
1.06140155475125,1.08529525625318,1.08927899950726,1.11434050369983,1.11715644426327,
1.14393065344995,1.17098540440778,1.19783521736686,1.21808204851952,1.24119892021897,
1.24512763049342,1.25897417085869,1.25898740261327,1.28275052598487,1.28544903653438,
1.31039702842331,1.31226081213009,1.31876428899761,1.34534096825719,1.3708141566497,
1.37082202499578,1.38667239091504),.UNSPECIFIED.);
#717=B_SPLINE_CURVE_WITH_KNOTS('',3,(#46465,#46466,#46467,#46468,#46469,
#46470,#46471,#46472,#46473,#46474,#46475,#46476,#46477,#46478,#46479,#46480,
#46481,#46482,#46483,#46484,#46485,#46486,#46487,#46488,#46489,#46490,#46491,
#46492,#46493,#46494,#46495,#46496,#46497,#46498,#46499,#46500,#46501,#46502,
#46503,#46504,#46505,#46506,#46507,#46508,#46509,#46510),.UNSPECIFIED.,
 .F.,.F.,(4,2,2,2,2,2,2,2,2,2,2,2,2,2,2,2,2,2,2,2,2,2,4),(1.88361728507473,
1.96613901790761,2.06744611316973,2.11575785090515,2.16536468174169,2.25859006675776,
2.30797163714038,2.35584195444279,2.45707357200554,2.50600802601238,2.55571013211468,
2.65209506654081,2.70006204432426,2.74877786583655,2.84768301560138,2.94883097916437,
2.99685457059701,3.09818140715212,3.19599431591786,3.27979391370675,3.36312376157902,
3.46429786859654,3.4738015741047),.UNSPECIFIED.);
#718=B_SPLINE_CURVE_WITH_KNOTS('',3,(#46513,#46514,#46515,#46516,#46517,
#46518,#46519,#46520,#46521,#46522,#46523,#46524,#46525,#46526,#46527,#46528,
#46529,#46530,#46531,#46532,#46533,#46534,#46535,#46536,#46537,#46538,#46539,
#46540),.UNSPECIFIED.,.F.,.F.,(4,2,2,2,2,2,2,2,2,2,2,2,2,4),(3.4738015741047,
3.55646460394477,3.65827175861552,3.74262585524875,3.84347823410159,3.92685548572533,
4.02844773414359,4.07274100135846,4.17305612403082,4.25792737984997,4.35287051687195,
4.40062979162429,4.4637145399754,4.51766419841934),.UNSPECIFIED.);
#719=B_SPLINE_CURVE_WITH_KNOTS('',3,(#46542,#46543,#46544,#46545,#46546,
#46547,#46548,#46549,#46550,#46551,#46552,#46553,#46554,#46555,#46556,#46557,
#46558,#46559,#46560,#46561,#46562,#46563,#46564,#46565,#46566,#46567,#46568,
#46569,#46570,#46571,#46572,#46573,#46574,#46575,#46576,#46577,#46578,#46579,
#46580,#46581,#46582,#46583,#46584,#46585,#46586,#46587,#46588,#46589,#46590,
#46591,#46592,#46593,#46594,#46595,#46596,#46597,#46598,#46599,#46600,#46601,
#46602,#46603,#46604,#46605,#46606,#46607,#46608,#46609,#46610,#46611,#46612,
#46613,#46614,#46615,#46616,#46617,#46618,#46619,#46620,#46621,#46622,#46623,
#46624,#46625,#46626,#46627,#46628,#46629,#46630,#46631,#46632,#46633,#46634,
#46635,#46636,#46637,#46638,#46639,#46640,#46641,#46642,#46643,#46644,#46645,
#46646,#46647),.UNSPECIFIED.,.F.,.F.,(4,3,3,3,3,3,3,3,3,3,3,3,3,3,3,3,3,
3,3,3,3,3,3,3,3,3,3,3,3,3,3,3,3,3,3,4),(0.,0.0265152916366039,0.0534408681373308,
0.0803732537892289,0.101671318199502,0.126768973351817,0.128669605927973,
0.153163172340859,0.155509697825392,0.16384911211717,0.163849430554983,
0.188424042846322,0.190512347195134,0.203249027869299,0.229570935958494,
0.256365848711328,0.283325187479159,0.304748913597632,0.330304499545278,
0.331728476013042,0.356523027277944,0.359681624709295,0.383638294470675,
0.386147280159222,0.387634773405548,0.387654846931905,0.406179509230895,
0.432211307600104,0.45880941260941,0.485718384707018,0.49948489014596,0.499498019517492,
0.507549805242806,0.527395571189254,0.52740934651372,0.545642469618713),
 .UNSPECIFIED.);
#720=B_SPLINE_CURVE_WITH_KNOTS('',3,(#46651,#46652,#46653,#46654),
 .UNSPECIFIED.,.F.,.F.,(4,4),(3.17692141158165,3.21705724092707),
 .UNSPECIFIED.);
#721=B_SPLINE_CURVE_WITH_KNOTS('',3,(#46655,#46656,#46657,#46658,#46659,
#46660,#46661,#46662,#46663,#46664,#46665,#46666,#46667,#46668,#46669,#46670,
#46671,#46672,#46673,#46674,#46675,#46676,#46677,#46678,#46679,#46680,#46681,
#46682,#46683,#46684,#46685,#46686,#46687,#46688,#46689,#46690,#46691,#46692,
#46693,#46694,#46695,#46696,#46697,#46698),.UNSPECIFIED.,.F.,.F.,(4,2,2,
2,2,2,2,2,2,2,2,2,2,2,2,2,2,2,2,2,2,4),(1.62006151030285E-6,0.0630919360385355,
0.141371266622184,0.240503139713508,0.287761650735986,0.384166379031894,
0.434674488379614,0.48430971532037,0.533052731490774,0.628943150682843,
0.678967965576476,0.773597067333852,0.823829482794688,0.919205173967643,
0.968856828764193,1.06534548410256,1.11441704174039,1.21144390918971,1.30591932981216,
1.40676744527164,1.47566588590981,1.54713662236737),.UNSPECIFIED.);
#722=B_SPLINE_CURVE_WITH_KNOTS('',3,(#46703,#46704,#46705,#46706,#46707,
#46708,#46709,#46710,#46711,#46712,#46713,#46714,#46715,#46716,#46717,#46718,
#46719,#46720,#46721,#46722,#46723,#46724,#46725,#46726,#46727,#46728,#46729,
#46730,#46731,#46732,#46733,#46734,#46735,#46736,#46737,#46738,#46739,#46740,
#46741,#46742,#46743,#46744,#46745,#46746),.UNSPECIFIED.,.F.,.F.,(4,2,2,
2,2,2,2,2,2,2,2,2,2,2,2,2,2,2,2,2,2,4),(1.59120053347567,1.60853341934407,
1.65661584810623,1.75505616994776,1.8462295408035,1.94706985801477,1.99655604703536,
2.04585088558141,2.09530509317676,2.19142149509141,2.29246978719122,2.38516127502823,
2.48243927585401,2.53024851712262,2.63125669011797,2.72417158686598,2.81887978492759,
2.86666299693515,2.96738709204182,3.05919840492306,3.14435325618814,3.17692141158165),
 .UNSPECIFIED.);
#723=B_SPLINE_CURVE_WITH_KNOTS('',3,(#46748,#46749,#46750,#46751,#46752,
#46753,#46754,#46755,#46756,#46757,#46758,#46759,#46760,#46761,#46762,#46763,
#46764,#46765,#46766,#46767,#46768,#46769,#46770,#46771,#46772,#46773,#46774,
#46775,#46776,#46777,#46778,#46779,#46780,#46781,#46782,#46783,#46784,#46785,
#46786,#46787,#46788,#46789),.UNSPECIFIED.,.F.,.F.,(4,2,2,2,2,2,2,2,2,2,
2,2,2,2,2,2,2,2,2,2,4),(0.000142530208232202,0.084807243665273,0.12049355472412,
0.219724371123383,0.292967991970656,0.39430418199766,0.490547781547131,
0.572968847782376,0.667961187809243,0.746000093988248,0.793791696819115,
0.875555352557861,0.973542726584909,1.07467540733736,1.12475371232168,1.21762151178067,
1.26566606434273,1.31580783326067,1.40843364165663,1.50260630133708,1.58743977472934),
 .UNSPECIFIED.);
#724=B_SPLINE_CURVE_WITH_KNOTS('',3,(#46790,#46791,#46792,#46793),
 .UNSPECIFIED.,.F.,.F.,(4,4),(1.00000007008057E-6,4.51866339753897E-5),
 .UNSPECIFIED.);
#725=B_SPLINE_CURVE_WITH_KNOTS('',3,(#46798,#46799,#46800,#46801,#46802,
#46803,#46804,#46805,#46806,#46807,#46808,#46809,#46810,#46811,#46812,#46813,
#46814,#46815,#46816,#46817,#46818,#46819,#46820,#46821,#46822,#46823,#46824,
#46825,#46826,#46827,#46828,#46829,#46830,#46831,#46832,#46833,#46834,#46835,
#46836,#46837),.UNSPECIFIED.,.F.,.F.,(4,2,2,2,2,2,2,2,2,2,2,2,2,2,2,2,2,
2,2,4),(0.000225597449676421,0.0742785979883565,0.172984943813638,0.21867109199009,
0.263583573029605,0.338100351692891,0.439755678406654,0.530561182861844,
0.630701087176066,0.680230522755222,0.766303621894736,0.867669669041908,
0.96729347126901,1.06300073179688,1.11181328265079,1.21259237443786,1.31385724331297,
1.41584938221636,1.51607755707357,1.59120053347567),.UNSPECIFIED.);
#726=B_SPLINE_CURVE_WITH_KNOTS('',3,(#46839,#46840,#46841,#46842,#46843,
#46844,#46845,#46846,#46847,#46848,#46849,#46850,#46851,#46852,#46853,#46854,
#46855,#46856,#46857,#46858,#46859,#46860,#46861,#46862,#46863,#46864,#46865,
#46866,#46867,#46868),.UNSPECIFIED.,.F.,.F.,(4,2,2,2,2,2,2,2,2,2,2,2,2,
2,4),(4.51866339753897E-5,0.0723418406247212,0.134392893639461,0.235357150136565,
0.327769542964459,0.37808460863748,0.478641278283578,0.579619814342238,
0.674620396174953,0.723420037361222,0.812330301317198,0.912981269215007,
1.00567215431713,1.08860054890301,1.15920864160196),.UNSPECIFIED.);
#727=B_SPLINE_CURVE_WITH_KNOTS('',3,(#46869,#46870,#46871,#46872,#46873,
#46874,#46875,#46876,#46877,#46878,#46879,#46880),.UNSPECIFIED.,.F.,.F.,
(4,2,2,2,2,4),(3.15245941783976E-5,0.0712582376283404,0.153901430321048,
0.246035781455943,0.347779076529136,0.426610112684851),.UNSPECIFIED.);
#728=B_SPLINE_CURVE_WITH_KNOTS('',3,(#46886,#46887,#46888,#46889,#46890,
#46891,#46892,#46893,#46894,#46895,#46896,#46897,#46898,#46899,#46900,#46901,
#46902,#46903,#46904,#46905,#46906,#46907,#46908,#46909,#46910,#46911,#46912,
#46913,#46914,#46915,#46916,#46917,#46918,#46919,#46920,#46921),
 .UNSPECIFIED.,.F.,.F.,(4,2,2,2,2,2,2,2,2,2,2,2,2,2,2,2,2,4),(1.58722454481072,
1.59524297044126,1.69317612751528,1.79281806368903,1.87978394745879,1.96899265118635,
2.06989725355135,2.16758224385157,2.25534165295551,2.34593089546819,2.44477013813802,
2.53454582142298,2.63253651296269,2.72236054424066,2.81965528443521,2.90701496351563,
3.00540629266297,3.09463589604302),.UNSPECIFIED.);
#729=B_SPLINE_CURVE_WITH_KNOTS('',3,(#46923,#46924,#46925,#46926,#46927,
#46928,#46929,#46930,#46931,#46932,#46933,#46934,#46935),.UNSPECIFIED.,
 .F.,.F.,(4,3,3,3,4),(0.0018605619201363,0.0062236786619737,0.0308774375217015,
0.0556573833848329,0.0777721094897591),.UNSPECIFIED.);
#730=B_SPLINE_CURVE_WITH_KNOTS('',3,(#46936,#46937,#46938,#46939),
 .UNSPECIFIED.,.F.,.F.,(4,4),(9.70452423452837E-6,0.000225597449676421),
 .UNSPECIFIED.);
#731=B_SPLINE_CURVE_WITH_KNOTS('',3,(#46941,#46942,#46943,#46944,#46945,
#46946,#46947,#46948,#46949,#46950,#46951,#46952,#46953,#46954,#46955,#46956,
#46957,#46958,#46959,#46960,#46961,#46962,#46963,#46964,#46965,#46966,#46967,
#46968,#46969,#46970,#46971,#46972,#46973,#46974,#46975,#46976,#46977,#46978,
#46979,#46980),.UNSPECIFIED.,.F.,.F.,(4,2,2,2,2,2,2,2,2,2,2,2,2,2,2,2,2,
2,2,4),(0.426610112684851,0.439472155416163,0.541098529643712,0.632374845173586,
0.681041387412177,0.777089284904803,0.827790203151545,0.876690951902663,
0.977656571294406,1.07524977633825,1.12372668491373,1.22223503711215,1.27018254242946,
1.31851261808215,1.41931586170264,1.46815778609337,1.56783530997388,1.6142737679206,
1.68646984809641,1.75330694074283),.UNSPECIFIED.);
#732=B_SPLINE_CURVE_WITH_KNOTS('',3,(#46981,#46982,#46983,#46984,#46985,
#46986,#46987,#46988,#46989,#46990),.UNSPECIFIED.,.F.,.F.,(4,2,2,2,4),(0.000434210888476285,
0.0630060612538896,0.136757874181064,0.232772050379,0.261585962310352),
 .UNSPECIFIED.);
#733=B_SPLINE_CURVE_WITH_KNOTS('',3,(#46996,#46997,#46998,#46999),
 .UNSPECIFIED.,.F.,.F.,(4,4),(1.41445606292759,1.4144793844605),
 .UNSPECIFIED.);
#734=B_SPLINE_CURVE_WITH_KNOTS('',3,(#47000,#47001,#47002,#47003,#47004,
#47005,#47006,#47007,#47008,#47009,#47010,#47011,#47012,#47013,#47014,#47015,
#47016,#47017,#47018,#47019,#47020,#47021,#47022,#47023,#47024,#47025,#47026,
#47027,#47028,#47029,#47030,#47031,#47032,#47033,#47034,#47035,#47036,#47037,
#47038,#47039,#47040,#47041),.UNSPECIFIED.,.F.,.F.,(4,2,2,2,2,2,2,2,2,2,
2,2,2,2,2,2,2,2,2,2,4),(1.00000013738019E-6,0.0796922243486748,0.164914931020009,
0.265180305781826,0.359335347902182,0.45669214052704,0.507219253269266,
0.555952281106953,0.65708827855891,0.751766673237182,0.801524920395762,
0.902500497171451,0.951104807532313,1.00077823719909,1.07925129178133,1.18069608155444,
1.25613712406717,1.3574635166215,1.44767761290287,1.54753048731727,1.58722454481072),
 .UNSPECIFIED.);
#735=B_SPLINE_CURVE_WITH_KNOTS('',3,(#47042,#47043,#47044,#47045,#47046,
#47047,#47048,#47049,#47050,#47051,#47052,#47053,#47054,#47055,#47056,#47057,
#47058,#47059,#47060,#47061,#47062,#47063,#47064,#47065,#47066,#47067,#47068,
#47069,#47070,#47071,#47072,#47073,#47074,#47075,#47076,#47077,#47078,#47079,
#47080,#47081,#47082,#47083),.UNSPECIFIED.,.F.,.F.,(4,2,2,2,2,2,2,2,2,2,
2,2,2,2,2,2,2,2,2,2,4),(0.261585962310352,0.330550507228154,0.422527548682331,
0.47237274394023,0.564999077065041,0.667050806886986,0.711465681558209,
0.800391700047598,0.902392081894043,1.00262065482135,1.08506201189223,1.18643635531154,
1.23566840489802,1.33738116675383,1.43802933084244,1.48690438160809,1.53618071386031,
1.63734686166833,1.68140483291318,1.78262408644938,1.85540224175298),
 .UNSPECIFIED.);
#736=B_SPLINE_CURVE_WITH_KNOTS('',3,(#47089,#47090,#47091,#47092,#47093,
#47094,#47095,#47096),.UNSPECIFIED.,.F.,.F.,(4,2,2,4),(1.58568783641564,
1.60107665321778,1.69047010281316,1.76702536599967),.UNSPECIFIED.);
#737=B_SPLINE_CURVE_WITH_KNOTS('',3,(#47097,#47098,#47099,#47100,#47101,
#47102,#47103,#47104,#47105,#47106,#47107,#47108,#47109,#47110,#47111,#47112,
#47113,#47114,#47115,#47116,#47117,#47118,#47119,#47120,#47121,#47122,#47123,
#47124,#47125,#47126,#47127,#47128,#47129,#47130,#47131,#47132,#47133,#47134,
#47135,#47136,#47137,#47138),.UNSPECIFIED.,.F.,.F.,(4,2,2,2,2,2,2,2,2,2,
2,2,2,2,2,2,2,2,2,2,4),(1.91775425791884E-5,0.0612944133050306,0.127958262779682,
0.228551343497341,0.277929273973939,0.369183603105148,0.465110204022711,
0.560983178942996,0.609100835872562,0.659754517209396,0.707271467351877,
0.80909755487051,0.896035614412291,0.996569978326781,1.04361179933817,1.09207570162642,
1.19392102568165,1.24233423984167,1.32720234730169,1.36928301115767,1.41445606292759),
 .UNSPECIFIED.);
#738=B_SPLINE_CURVE_WITH_KNOTS('',3,(#47140,#47141,#47142,#47143,#47144,
#47145,#47146,#47147,#47148,#47149,#47150,#47151,#47152,#47153,#47154,#47155,
#47156,#47157,#47158,#47159,#47160,#47161,#47162,#47163,#47164,#47165,#47166,
#47167,#47168,#47169,#47170,#47171,#47172,#47173,#47174,#47175,#47176,#47177),
 .UNSPECIFIED.,.F.,.F.,(4,2,2,2,2,2,2,2,2,2,2,2,2,2,2,2,2,2,4),(1.85540224175298,
1.8619285315257,1.96200419757285,2.01118534688469,2.10343957811208,2.20207178110793,
2.24977633671792,2.35130727897218,2.44561194476143,2.54209792847507,2.58987156038197,
2.69119674822331,2.78594737859994,2.83531674316662,2.9242056709114,3.02532340493309,
3.11793130320266,3.20245562576603,3.27462710206336),.UNSPECIFIED.);
#739=B_SPLINE_CURVE_WITH_KNOTS('',3,(#47178,#47179,#47180,#47181,#47182,
#47183),.UNSPECIFIED.,.F.,.F.,(4,2,4),(2.18613549776391E-5,0.086154780125611,
0.172243535902318),.UNSPECIFIED.);
#740=B_SPLINE_CURVE_WITH_KNOTS('',3,(#47186,#47187,#47188,#47189,#47190,
#47191,#47192,#47193,#47194,#47195,#47196,#47197,#47198,#47199,#47200,#47201,
#47202,#47203,#47204,#47205,#47206,#47207,#47208,#47209,#47210,#47211,#47212,
#47213,#47214,#47215,#47216,#47217,#47218,#47219,#47220,#47221,#47222,#47223),
 .UNSPECIFIED.,.F.,.F.,(4,2,2,2,2,2,2,2,2,2,2,2,2,2,2,2,2,2,4),(9.99999998785787E-7,
0.0872888446587809,0.181612821610965,0.277455319811984,0.372137063139133,
0.465554874798131,0.567846232837133,0.65372194201713,0.702757026771262,
0.798859431343223,0.900937352389522,0.989203218137305,1.08572229776357,
1.18152722648351,1.2828802925819,1.38294569604287,1.43164726657578,1.53286996181633,
1.5925198531225),.UNSPECIFIED.);
#741=B_SPLINE_CURVE_WITH_KNOTS('',3,(#47226,#47227,#47228,#47229,#47230,
#47231,#47232,#47233,#47234,#47235,#47236,#47237,#47238,#47239,#47240,#47241,
#47242,#47243,#47244,#47245,#47246,#47247,#47248,#47249,#47250,#47251,#47252,
#47253,#47254,#47255,#47256,#47257,#47258,#47259,#47260,#47261,#47262,#47263,
#47264,#47265,#47266,#47267,#47268,#47269),.UNSPECIFIED.,.F.,.F.,(4,2,2,
2,2,2,2,2,2,2,2,2,2,2,2,2,2,2,2,2,2,4),(3.63649524114627E-6,0.0506749674295985,
0.0987723951799838,0.199129291380623,0.247004760404853,0.345097478709695,
0.442075215447975,0.492724066396971,0.587904001990667,0.689009154908131,
0.735835483147296,0.836592304221807,0.883525845707275,0.930710618615424,
1.03064389394975,1.13038725002875,1.21973722341929,1.26726563753008,1.36559794931312,
1.46417011421529,1.55307633926682,1.58568783641564),.UNSPECIFIED.);
#742=B_SPLINE_CURVE_WITH_KNOTS('',3,(#47275,#47276,#47277,#47278),
 .UNSPECIFIED.,.F.,.F.,(4,4),(1.58766981265925,1.58767330633224),
 .UNSPECIFIED.);
#743=B_SPLINE_CURVE_WITH_KNOTS('',3,(#47280,#47281,#47282,#47283,#47284,
#47285,#47286),.UNSPECIFIED.,.F.,.F.,(4,3,4),(1.62164761664365E-5,0.0442981693467548,
0.0886134884474553),.UNSPECIFIED.);
#744=B_SPLINE_CURVE_WITH_KNOTS('',3,(#47287,#47288,#47289,#47290,#47291,
#47292,#47293,#47294,#47295,#47296,#47297,#47298,#47299,#47300,#47301,#47302,
#47303,#47304,#47305,#47306,#47307,#47308,#47309,#47310,#47311,#47312,#47313,
#47314,#47315,#47316,#47317,#47318,#47319,#47320,#47321,#47322,#47323,#47324,
#47325,#47326,#47327,#47328,#47329,#47330,#47331,#47332,#47333,#47334,#47335,
#47336,#47337,#47338,#47339,#47340,#47341,#47342,#47343,#47344,#47345,#47346,
#47347,#47348,#47349,#47350,#47351,#47352,#47353,#47354,#47355,#47356,#47357,
#47358,#47359,#47360,#47361,#47362,#47363,#47364,#47365,#47366,#47367,#47368,
#47369,#47370,#47371,#47372,#47373,#47374,#47375,#47376,#47377,#47378,#47379,
#47380,#47381,#47382,#47383,#47384,#47385,#47386,#47387,#47388,#47389,#47390,
#47391,#47392,#47393,#47394,#47395,#47396,#47397,#47398,#47399,#47400,#47401,
#47402,#47403,#47404,#47405,#47406,#47407,#47408,#47409,#47410,#47411,#47412,
#47413,#47414,#47415,#47416,#47417,#47418,#47419,#47420,#47421,#47422,#47423,
#47424,#47425,#47426,#47427,#47428,#47429,#47430,#47431,#47432,#47433,#47434,
#47435,#47436,#47437,#47438,#47439,#47440,#47441,#47442,#47443,#47444,#47445,
#47446,#47447,#47448,#47449,#47450,#47451,#47452,#47453,#47454,#47455,#47456,
#47457,#47458,#47459,#47460,#47461,#47462,#47463,#47464,#47465,#47466,#47467,
#47468,#47469,#47470,#47471,#47472,#47473,#47474,#47475,#47476,#47477,#47478,
#47479,#47480,#47481,#47482,#47483,#47484,#47485,#47486,#47487,#47488,#47489,
#47490,#47491,#47492,#47493,#47494,#47495,#47496,#47497,#47498,#47499,#47500,
#47501,#47502,#47503,#47504,#47505,#47506,#47507,#47508,#47509,#47510,#47511,
#47512,#47513,#47514,#47515,#47516,#47517,#47518,#47519,#47520,#47521,#47522,
#47523,#47524,#47525,#47526,#47527,#47528,#47529,#47530,#47531,#47532,#47533,
#47534,#47535,#47536,#47537,#47538,#47539,#47540,#47541,#47542,#47543,#47544,
#47545,#47546,#47547,#47548,#47549,#47550,#47551,#47552,#47553,#47554,#47555,
#47556,#47557,#47558,#47559,#47560,#47561,#47562,#47563,#47564,#47565,#47566,
#47567,#47568,#47569),.UNSPECIFIED.,.F.,.F.,(4,3,3,3,3,3,3,3,3,3,3,3,3,
3,3,3,3,3,3,3,3,3,3,3,3,3,3,3,3,3,3,3,3,3,3,3,3,3,3,3,3,3,3,3,3,3,3,3,3,
3,3,3,3,3,3,3,3,3,3,3,3,3,3,3,3,3,3,3,3,3,3,3,3,3,3,3,3,3,3,3,3,3,3,3,3,
3,3,3,3,3,3,3,3,3,4),(7.34837406725557E-8,0.019964867263137,0.0267693319277699,
0.0538018319699899,0.080579428135738,0.101824612826378,0.126388705926906,
0.128806294507739,0.140309322647435,0.140329659467777,0.165163912862995,
0.166493337341274,0.191905588690079,0.193354134040805,0.203526934231238,
0.230079241430717,0.257031002660155,0.28393706738352,0.305131955689965,
0.329790464210409,0.332136781123739,0.35614008309364,0.358965082758299,
0.364187796786279,0.364194448230442,0.388395041227389,0.390839887900307,
0.4066542974926,0.43300798160048,0.459851088836211,0.486886294610224,0.508104247050711,
0.535134837619628,0.560056375819446,0.562010330265102,0.586037386003401,
0.587966244395663,0.587967454966848,0.609493176432852,0.635682161969534,
0.662341510193711,0.689203081363828,0.699813410037673,0.699818853899349,
0.710830205766576,0.737539611782812,0.764413833638791,0.789460075551521,
0.790927600001401,0.811644907352174,0.811648797193604,0.812119671007486,
0.836086924852687,0.838125261897265,0.863339061094821,0.864709035325677,
0.891748760773525,0.914207077880491,0.941187256266604,0.968267314316379,
0.993011640482214,0.994880480564172,1.01590037275537,1.03529922270649,1.03531663017424,
1.05811313070032,1.06139837796637,1.0853081020415,1.08928336257022,1.11460462293563,
1.11716834717406,1.14394638546685,1.17098306230525,1.19773441829998,1.21808842694735,
1.24035953250997,1.2450783291986,1.2589753624395,1.25900871113918,1.2814308744521,
1.28528504821362,1.3084818360773,1.31218376228509,1.31876297219116,1.3453387934928,
1.37231702471802,1.39932418579149,1.41915612304848,1.44343126687223,1.44617731733548,
1.46954588616007,1.47307953308824,1.48265110768315,1.48265668956468,1.5030722252932),
 .UNSPECIFIED.);
#745=B_SPLINE_CURVE_WITH_KNOTS('',3,(#47570,#47571,#47572,#47573,#47574,
#47575,#47576,#47577,#47578,#47579,#47580,#47581,#47582,#47583,#47584,#47585,
#47586,#47587,#47588,#47589,#47590,#47591,#47592,#47593,#47594,#47595,#47596,
#47597,#47598,#47599,#47600,#47601,#47602,#47603,#47604,#47605,#47606,#47607,
#47608,#47609,#47610,#47611,#47612,#47613),.UNSPECIFIED.,.F.,.F.,(4,2,2,
2,2,2,2,2,2,2,2,2,2,2,2,2,2,2,2,2,2,4),(1.5925198531225,1.63115089761907,
1.68028338306566,1.7288487743576,1.82517709840843,1.87523647554672,1.97031689459656,
2.06752405104401,2.16861133619847,2.26968250121187,2.31826217170868,2.41824499459598,
2.51925552873196,2.56745564354346,2.66818108321483,2.71776519283693,2.7662031033493,
2.81370651120408,2.91461532539117,3.01101723620208,3.11201162580048,3.18046637425616),
 .UNSPECIFIED.);
#746=B_SPLINE_CURVE_WITH_KNOTS('',3,(#47618,#47619,#47620,#47621,#47622,
#47623,#47624,#47625,#47626,#47627,#47628,#47629,#47630,#47631,#47632,#47633,
#47634,#47635,#47636,#47637,#47638,#47639,#47640,#47641,#47642,#47643,#47644,
#47645,#47646,#47647,#47648,#47649,#47650,#47651,#47652,#47653,#47654,#47655,
#47656,#47657,#47658,#47659),.UNSPECIFIED.,.F.,.F.,(4,2,2,2,2,2,2,2,2,2,
2,2,2,2,2,2,2,2,2,2,4),(0.000332700259628768,0.0951610873337013,0.178264167133354,
0.273039667383402,0.371193805519262,0.467050098219079,0.547915762639124,
0.597950953485952,0.692817036535044,0.793845190917708,0.842969683744045,
0.892599286248275,0.988332887846854,1.03714150596388,1.13271901979353,1.18153079169454,
1.27832189716448,1.37232427040614,1.47310054254796,1.52908620914187,1.58766981265925),
 .UNSPECIFIED.);
#747=B_SPLINE_CURVE_WITH_KNOTS('',3,(#47661,#47662,#47663,#47664,#47665,
#47666,#47667,#47668,#47669,#47670,#47671,#47672,#47673,#47674,#47675,#47676,
#47677,#47678,#47679,#47680,#47681,#47682,#47683,#47684,#47685,#47686,#47687,
#47688),.UNSPECIFIED.,.F.,.F.,(4,2,2,2,2,2,2,2,2,2,2,2,2,4),(3.18046637425616,
3.19763502745909,3.29857986209492,3.39195214731422,3.48952696515865,3.58521097258035,
3.68156815331091,3.76906564255767,3.86983781821281,3.95777506098375,4.05877788923688,
4.14461580757828,4.24493867900757,4.33903702193303),.UNSPECIFIED.);
#748=B_SPLINE_CURVE_WITH_KNOTS('',3,(#47689,#47690,#47691,#47692,#47693,
#47694,#47695,#47696,#47697,#47698,#47699,#47700,#47701,#47702),
 .UNSPECIFIED.,.F.,.F.,(4,2,2,2,2,2,4),(7.39074714640052E-6,0.0560225944124789,
0.112993048660793,0.157595030319142,0.255703338428967,0.352232387034829,
0.428604909966747),.UNSPECIFIED.);
#749=B_SPLINE_CURVE_WITH_KNOTS('',3,(#47708,#47709,#47710,#47711,#47712,
#47713,#47714,#47715,#47716,#47717,#47718,#47719,#47720,#47721,#47722,#47723,
#47724,#47725,#47726,#47727,#47728,#47729,#47730,#47731,#47732,#47733,#47734,
#47735,#47736,#47737,#47738,#47739,#47740,#47741,#47742,#47743,#47744,#47745,
#47746,#47747),.UNSPECIFIED.,.F.,.F.,(4,2,2,2,2,2,2,2,2,2,2,2,2,2,2,2,2,
2,2,4),(1.58989822515966,1.59915917085918,1.69919078916423,1.74658988147312,
1.84785528875568,1.94360942344156,1.99292121519929,2.08243829086462,2.1835780720849,
2.27906545500479,2.3281489862221,2.41747307583334,2.51844181690281,2.61293340903648,
2.66193834680959,2.75064087305788,2.85136608761713,2.94359228351708,3.02794550059186,
3.09960259124824),.UNSPECIFIED.);
#750=B_SPLINE_CURVE_WITH_KNOTS('',3,(#47749,#47750,#47751,#47752,#47753,
#47754,#47755,#47756,#47757,#47758,#47759,#47760,#47761,#47762,#47763,#47764,
#47765,#47766,#47767,#47768,#47769,#47770,#47771,#47772,#47773,#47774,#47775,
#47776),.UNSPECIFIED.,.F.,.F.,(4,3,3,3,3,3,3,3,3,4),(0.00257022351332799,
0.00718554272612916,0.00853032056992718,0.0209145361963684,0.0449312967344481,
0.04781715587265,0.0642592511561034,0.0642736300230747,0.0700433819734726,
0.0784535026574735),.UNSPECIFIED.);
#751=B_SPLINE_CURVE_WITH_KNOTS('',3,(#47777,#47778,#47779,#47780),
 .UNSPECIFIED.,.F.,.F.,(4,4),(1.97025552236534E-5,0.000332700259628768),
 .UNSPECIFIED.);
#752=B_SPLINE_CURVE_WITH_KNOTS('',3,(#47781,#47782,#47783,#47784,#47785,
#47786,#47787,#47788,#47789,#47790,#47791,#47792,#47793,#47794,#47795,#47796,
#47797,#47798,#47799,#47800,#47801,#47802,#47803,#47804,#47805,#47806,#47807,
#47808,#47809,#47810,#47811,#47812,#47813,#47814,#47815,#47816,#47817,#47818,
#47819,#47820,#47821,#47822),.UNSPECIFIED.,.F.,.F.,(4,2,2,2,2,2,2,2,2,2,
2,2,2,2,2,2,2,2,2,2,4),(0.428604909966747,0.445529583287182,0.547065009487481,
0.624452539467869,0.725617321863814,0.819296188596134,0.914887254159531,
1.01199255838545,1.09096737493364,1.19247445741117,1.28625834692512,1.33639550374713,
1.43719821430216,1.50412082096437,1.55130356074699,1.64616163870914,1.74581251906439,
1.8369972558916,1.9185225652106,1.96301176268206,2.01706548363289),
 .UNSPECIFIED.);
#753=B_SPLINE_CURVE_WITH_KNOTS('',3,(#47827,#47828,#47829,#47830,#47831,
#47832,#47833,#47834,#47835,#47836,#47837,#47838,#47839,#47840,#47841,#47842,
#47843,#47844,#47845,#47846,#47847,#47848,#47849,#47850,#47851,#47852,#47853,
#47854,#47855,#47856,#47857,#47858,#47859,#47860,#47861,#47862,#47863,#47864,
#47865,#47866,#47867,#47868,#47869,#47870),.UNSPECIFIED.,.F.,.F.,(4,2,2,
2,2,2,2,2,2,2,2,2,2,2,2,2,2,2,2,2,2,4),(0.000341705276625282,0.0560928328092873,
0.102790668391616,0.184374451969009,0.286732434312196,0.331732934943196,
0.417676823545026,0.466062468242685,0.515746518663139,0.564570875086013,
0.643435069330897,0.744805452143349,0.841979042757459,0.925117184647647,
1.02054525775881,1.10245593081841,1.20364640868695,1.30106169525946,1.35051533162512,
1.45017308381718,1.55030069541036,1.58989822515966),.UNSPECIFIED.);
#754=B_SPLINE_CURVE_WITH_KNOTS('',3,(#47872,#47873,#47874,#47875,#47876,
#47877,#47878,#47879,#47880,#47881,#47882,#47883,#47884,#47885,#47886,#47887,
#47888,#47889,#47890,#47891,#47892,#47893,#47894,#47895,#47896,#47897,#47898,
#47899,#47900,#47901,#47902,#47903,#47904,#47905),.UNSPECIFIED.,.F.,.F.,
(4,2,2,2,2,2,2,2,2,2,2,2,2,2,2,2,4),(2.01706548363289,2.06402058510678,
2.11258685382852,2.21344856852205,2.31199447340875,2.36028586383664,2.45063151831325,
2.5514528244517,2.64909661933046,2.73923168408122,2.78684519594595,2.88733463019532,
2.98400799147551,3.0735739102523,3.12210765377232,3.21406068429801,3.29229578180851),
 .UNSPECIFIED.);
#755=B_SPLINE_CURVE_WITH_KNOTS('',3,(#47906,#47907,#47908,#47909,#47910,
#47911,#47912,#47913,#47914,#47915),.UNSPECIFIED.,.F.,.F.,(4,2,2,2,4),(0.000546235713184444,
0.0692821643427151,0.15084981789586,0.24746567567304,0.3106638555438),
 .UNSPECIFIED.);
#756=B_SPLINE_CURVE_WITH_KNOTS('',3,(#47921,#47922,#47923,#47924),
 .UNSPECIFIED.,.F.,.F.,(4,4),(1.58665344971703,1.58674871126382),
 .UNSPECIFIED.);
#757=B_SPLINE_CURVE_WITH_KNOTS('',3,(#47926,#47927,#47928,#47929,#47930,
#47931,#47932,#47933,#47934,#47935,#47936,#47937,#47938,#47939,#47940,#47941,
#47942,#47943,#47944,#47945,#47946,#47947,#47948,#47949,#47950,#47951,#47952,
#47953,#47954,#47955,#47956,#47957,#47958,#47959),.UNSPECIFIED.,.F.,.F.,
(4,2,2,2,2,2,2,2,2,2,2,2,2,2,2,2,4),(1.00000009372207E-6,0.0914529989276999,
0.191958650169849,0.276092173518159,0.376470995555748,0.459934127269538,
0.560923245043053,0.64585410666141,0.695543265710111,0.777019748534897,
0.822880712206414,0.923353130505685,1.0117585768333,1.11236877445855,1.19804423061871,
1.29811833254116,1.39109815874005),.UNSPECIFIED.);
#758=B_SPLINE_CURVE_WITH_KNOTS('',3,(#47961,#47962,#47963,#47964,#47965,
#47966,#47967,#47968,#47969,#47970,#47971,#47972,#47973,#47974,#47975,#47976,
#47977,#47978,#47979,#47980,#47981,#47982,#47983,#47984,#47985,#47986,#47987,
#47988,#47989,#47990,#47991),.UNSPECIFIED.,.F.,.F.,(4,3,3,3,3,3,3,3,3,3,
4),(0.00155980632875505,0.00467670428344775,0.0108997205793838,0.0233044349028981,
0.0483422336533325,0.0735317838257157,0.0983723994983146,0.118769142279212,
0.152602909073467,0.163507164534158,0.194306062421083),.UNSPECIFIED.);
#759=B_SPLINE_CURVE_WITH_KNOTS('',3,(#47992,#47993,#47994,#47995),
 .UNSPECIFIED.,.F.,.F.,(4,4),(0.00013539478902181,0.000341705276625282),
 .UNSPECIFIED.);
#760=B_SPLINE_CURVE_WITH_KNOTS('',3,(#47997,#47998,#47999,#48000,#48001,
#48002,#48003,#48004,#48005,#48006,#48007,#48008,#48009,#48010,#48011,#48012,
#48013,#48014,#48015,#48016,#48017,#48018,#48019,#48020,#48021,#48022,#48023,
#48024,#48025,#48026,#48027,#48028,#48029,#48030,#48031,#48032,#48033,#48034,
#48035,#48036,#48037,#48038),.UNSPECIFIED.,.F.,.F.,(4,2,2,2,2,2,2,2,2,2,
2,2,2,2,2,2,2,2,2,2,4),(0.3106638555438,0.345520813405148,0.438855187371024,
0.540468398856733,0.632954100967386,0.682167393955402,0.777701028875872,
0.828190357719904,0.877246102039471,0.978219152787592,1.07601538620938,
1.12452184255947,1.22317843275787,1.27114226129121,1.31952796216626,1.42033510923658,
1.4692222924981,1.56875812994508,1.61522154097716,1.68738346703665,1.75387240600549),
 .UNSPECIFIED.);
#761=B_SPLINE_CURVE_WITH_KNOTS('',3,(#48040,#48041,#48042,#48043,#48044,
#48045),.UNSPECIFIED.,.F.,.F.,(4,2,4),(1.70615880496912E-5,0.0719633053329676,
0.14405946356654),.UNSPECIFIED.);
#762=B_SPLINE_CURVE_WITH_KNOTS('',3,(#48046,#48047,#48048,#48049),
 .UNSPECIFIED.,.F.,.F.,(4,4),(4.2050335126144E-6,0.000109190503574576),
 .UNSPECIFIED.);
#763=B_SPLINE_CURVE_WITH_KNOTS('',3,(#48055,#48056,#48057,#48058),
 .UNSPECIFIED.,.F.,.F.,(4,4),(1.52690522644045,1.5269547118134),
 .UNSPECIFIED.);
#764=B_SPLINE_CURVE_WITH_KNOTS('',3,(#48059,#48060,#48061,#48062,#48063,
#48064,#48065,#48066,#48067,#48068,#48069,#48070,#48071,#48072,#48073,#48074,
#48075,#48076,#48077,#48078,#48079,#48080,#48081,#48082,#48083,#48084,#48085,
#48086,#48087,#48088,#48089,#48090,#48091,#48092,#48093,#48094,#48095,#48096,
#48097,#48098,#48099,#48100,#48101,#48102,#48103,#48104),.UNSPECIFIED.,
 .F.,.F.,(4,2,2,2,2,2,2,2,2,2,2,2,2,2,2,2,2,2,2,2,2,2,4),(8.20148954344905E-6,
0.0733429545867836,0.150301022577521,0.198847604410379,0.300002773164144,
0.399490303765739,0.448556694297784,0.496902763145731,0.592825595248763,
0.643551222672669,0.692340666989221,0.793378991921083,0.842199664407604,
0.892120800865433,0.986899677250673,1.08211067812445,1.12831172383911,1.22931229191877,
1.32305075053588,1.37144823302362,1.46280899557072,1.52902673345602,1.58665344971703),
 .UNSPECIFIED.);
#765=B_SPLINE_CURVE_WITH_KNOTS('',3,(#48105,#48106,#48107,#48108,#48109,
#48110,#48111,#48112,#48113,#48114,#48115,#48116,#48117,#48118,#48119,#48120,
#48121,#48122,#48123,#48124,#48125,#48126,#48127,#48128,#48129,#48130,#48131,
#48132,#48133,#48134,#48135,#48136,#48137,#48138,#48139,#48140,#48141,#48142,
#48143,#48144),.UNSPECIFIED.,.F.,.F.,(4,2,2,2,2,2,2,2,2,2,2,2,2,2,2,2,2,
2,2,4),(0.000109190503574576,0.0931915287847442,0.193793529234649,0.242818234568438,
0.340825947034013,0.430115799896213,0.531798734395658,0.632497388800296,
0.714755117226066,0.81324805833013,0.884777328630934,0.986517570464202,
1.03040325379661,1.10745127824861,1.20895044502336,1.30717346411687,1.39380073308839,
1.4943510402189,1.563518198958,1.59273035347225),.UNSPECIFIED.);
#766=B_SPLINE_CURVE_WITH_KNOTS('',3,(#48150,#48151,#48152,#48153,#48154,
#48155),.UNSPECIFIED.,.F.,.F.,(4,2,4),(3.17452747086746,3.17498472826448,
3.23986154436098),.UNSPECIFIED.);
#767=B_SPLINE_CURVE_WITH_KNOTS('',3,(#48156,#48157,#48158,#48159,#48160,
#48161,#48162,#48163,#48164,#48165,#48166,#48167,#48168,#48169,#48170,#48171,
#48172,#48173,#48174,#48175,#48176,#48177,#48178,#48179,#48180,#48181,#48182,
#48183,#48184,#48185,#48186,#48187,#48188,#48189,#48190,#48191,#48192,#48193,
#48194,#48195,#48196,#48197,#48198,#48199),.UNSPECIFIED.,.F.,.F.,(4,2,2,
2,2,2,2,2,2,2,2,2,2,2,2,2,2,2,2,2,2,4),(0.,0.0680186494305738,0.147676699355569,
0.235953182143958,0.285547214660472,0.376247643903819,0.470614224147492,
0.570259024729443,0.668194135923833,0.716238677096708,0.763441689184039,
0.860628057911294,0.910841062199871,0.956846564037905,1.05884988772573,
1.15320390167318,1.24910472962057,1.29541955762797,1.39740642862325,1.45930066606842,
1.49100971138413,1.52690522644045),.UNSPECIFIED.);
#768=B_SPLINE_CURVE_WITH_KNOTS('',3,(#48201,#48202,#48203,#48204,#48205,
#48206,#48207,#48208,#48209,#48210,#48211,#48212,#48213,#48214,#48215,#48216,
#48217,#48218,#48219,#48220,#48221,#48222,#48223,#48224,#48225,#48226,#48227,
#48228,#48229,#48230,#48231,#48232,#48233,#48234,#48235,#48236,#48237,#48238,
#48239,#48240),.UNSPECIFIED.,.F.,.F.,(4,2,2,2,2,2,2,2,2,2,2,2,2,2,2,2,2,
2,2,4),(1.59273035347225,1.66505000446301,1.74724033904894,1.79141405934091,
1.89276848186806,1.94106112316785,2.04236543169102,2.13992244944502,2.18875968529191,
2.27856804179947,2.37984834121376,2.47624614257626,2.52491305274713,2.61452913633043,
2.71554383228709,2.81108550047719,2.8596507303388,2.94828748249565,3.04448466377449,
3.12687551391254),.UNSPECIFIED.);
#769=B_SPLINE_CURVE_WITH_KNOTS('',3,(#48241,#48242,#48243,#48244),
 .UNSPECIFIED.,.F.,.F.,(4,4),(0.000550918055278865,0.0552481405980463),
 .UNSPECIFIED.);
#770=B_SPLINE_CURVE_WITH_KNOTS('',3,(#48249,#48250,#48251,#48252,#48253,
#48254,#48255,#48256,#48257,#48258,#48259,#48260,#48261,#48262,#48263,#48264,
#48265,#48266,#48267,#48268,#48269,#48270,#48271,#48272,#48273,#48274,#48275,
#48276,#48277,#48278,#48279,#48280,#48281,#48282,#48283,#48284,#48285,#48286,
#48287,#48288),.UNSPECIFIED.,.F.,.F.,(4,2,2,2,2,2,2,2,2,2,2,2,2,2,2,2,2,
2,2,4),(1.58954882556145,1.61994694155016,1.72111687689724,1.76953629068976,
1.86004171494891,1.96135645219197,2.05437746056574,2.10311900473412,2.19774598905527,
2.2986696589194,2.36402330234716,2.45765034270909,2.55918959039695,2.65837551289255,
2.74927194990235,2.83713438799803,2.90572543240668,3.00347539627398,3.10350357217783,
3.17452747086746),.UNSPECIFIED.);
#771=B_SPLINE_CURVE_WITH_KNOTS('',3,(#48289,#48290,#48291,#48292,#48293,
#48294,#48295,#48296,#48297,#48298,#48299,#48300,#48301,#48302,#48303,#48304,
#48305,#48306,#48307,#48308,#48309,#48310,#48311,#48312,#48313,#48314,#48315,
#48316,#48317,#48318,#48319,#48320,#48321,#48322,#48323,#48324,#48325,#48326,
#48327,#48328,#48329,#48330),.UNSPECIFIED.,.F.,.F.,(4,2,2,2,2,2,2,2,2,2,
2,2,2,2,2,2,2,2,2,2,4),(0.0552481405980463,0.0553431489108911,0.115543456159899,
0.210045383711121,0.306300846524538,0.398105513813643,0.487896698019488,
0.538071256306237,0.629719711437245,0.724376190949434,0.825197212458761,
0.924936205324376,0.973410366125791,1.07331868508949,1.17233739929906,1.22105376960377,
1.32230277165209,1.4202679363978,1.51436814529117,1.60994983209693,1.64703455004425),
 .UNSPECIFIED.);
#772=B_SPLINE_CURVE_WITH_KNOTS('',3,(#48336,#48337,#48338,#48339),
 .UNSPECIFIED.,.F.,.F.,(4,4),(0.0272291530888202,0.0273067833034242),
 .UNSPECIFIED.);
#773=B_SPLINE_CURVE_WITH_KNOTS('',3,(#48340,#48341,#48342,#48343,#48344,
#48345,#48346,#48347,#48348,#48349,#48350,#48351,#48352,#48353,#48354,#48355,
#48356,#48357,#48358,#48359,#48360,#48361,#48362,#48363,#48364,#48365,#48366,
#48367,#48368,#48369,#48370,#48371,#48372,#48373,#48374,#48375,#48376,#48377,
#48378,#48379,#48380,#48381,#48382,#48383),.UNSPECIFIED.,.F.,.F.,(4,2,2,
2,2,2,2,2,2,2,2,2,2,2,2,2,2,2,2,2,2,4),(1.00000018631629E-6,0.0905679837143679,
0.179742205585551,0.276160654514949,0.32512840106993,0.417516088904147,
0.466418315869915,0.566670317298738,0.654236472477998,0.75567445571018,
0.846198850084504,0.928573188796696,1.02712838427427,1.07634585028451,1.1748235354661,
1.22376269978151,1.31992682439122,1.37015346607007,1.4200367796879,1.52107771731938,
1.56988937965821,1.58954882556145),.UNSPECIFIED.);
#774=B_SPLINE_CURVE_WITH_KNOTS('',3,(#48384,#48385,#48386,#48387,#48388,
#48389,#48390,#48391,#48392,#48393,#48394,#48395,#48396,#48397,#48398,#48399,
#48400,#48401,#48402,#48403,#48404,#48405,#48406,#48407,#48408,#48409,#48410,
#48411,#48412,#48413,#48414,#48415,#48416,#48417,#48418,#48419,#48420,#48421,
#48422,#48423,#48424,#48425,#48426,#48427,#48428,#48429),.UNSPECIFIED.,
 .F.,.F.,(4,2,2,2,2,2,2,2,2,2,2,2,2,2,2,2,2,2,2,2,2,2,4),(1.64703455004425,
1.66024315979441,1.70914644311717,1.81028344660311,1.85831612652545,1.95937444897362,
2.06062861635938,2.10919013003134,2.15862064062204,2.25104129654871,2.30077954150846,
2.34822840849651,2.44910652315638,2.49603004296635,2.58332529821825,2.67779176069456,
2.72684247326199,2.81434388849864,2.91589263902365,3.01005996359688,3.09956324210311,
3.19323112914222,3.2335044050079),.UNSPECIFIED.);
#775=B_SPLINE_CURVE_WITH_KNOTS('',3,(#48436,#48437,#48438,#48439,#48440,
#48441,#48442,#48443,#48444,#48445,#48446,#48447,#48448,#48449,#48450,#48451,
#48452,#48453,#48454,#48455,#48456,#48457,#48458,#48459,#48460,#48461,#48462,
#48463,#48464,#48465,#48466,#48467,#48468,#48469,#48470,#48471,#48472,#48473,
#48474,#48475,#48476,#48477,#48478,#48479,#48480,#48481),.UNSPECIFIED.,
 .F.,.F.,(4,2,2,2,2,2,2,2,2,2,2,2,2,2,2,2,2,2,2,2,2,2,4),(-2.1855659803523,
-2.1060005592318,-2.01694296594534,-1.96901256052504,-1.86973206877917,
-1.77661798959221,-1.7274257082086,-1.67776494030543,-1.58450065227025,
-1.53434330399221,-1.43682863158872,-1.38746760106178,-1.28974491299529,
-1.23998499123436,-1.19135175996526,-1.14184453125496,-1.09301970067391,
-1.0431147266302,-0.994114591646302,-0.944106478309579,-0.895086657006542,
-0.844989929727302,-0.793898774335287),.UNSPECIFIED.);
#776=B_SPLINE_CURVE_WITH_KNOTS('',3,(#48483,#48484,#48485,#48486,#48487,
#48488,#48489,#48490,#48491,#48492,#48493,#48494,#48495,#48496,#48497,#48498,
#48499,#48500,#48501,#48502,#48503,#48504,#48505,#48506,#48507,#48508,#48509,
#48510,#48511,#48512,#48513,#48514,#48515,#48516,#48517,#48518,#48519,#48520,
#48521,#48522,#48523,#48524,#48525,#48526,#48527,#48528,#48529,#48530,#48531),
 .UNSPECIFIED.,.F.,.F.,(4,3,3,3,3,3,3,3,3,3,3,3,3,3,3,3,4),(0.00230840540264672,
0.00310329427917845,0.0166018506520161,0.0301004070248538,0.0544449092607173,
0.0571114353405323,0.0643911154884955,0.0644105816672325,0.0889679651173259,
0.0912098467045946,0.100490355331003,0.126749317454847,0.153598562219919,
0.158399345765457,0.15843447591468,0.185342050715828,0.194940455552248),
 .UNSPECIFIED.);
#777=B_SPLINE_CURVE_WITH_KNOTS('',3,(#48535,#48536,#48537,#48538,#48539,
#48540,#48541,#48542,#48543,#48544,#48545,#48546,#48547,#48548,#48549,#48550,
#48551,#48552,#48553,#48554,#48555,#48556),.UNSPECIFIED.,.F.,.F.,(4,2,2,
2,2,2,2,2,2,2,4),(0.000119906415017354,0.0675877728219243,0.149050275973358,
0.247839430914635,0.296210880517655,0.397796827580989,0.477892848335411,
0.573960419844177,0.621161322113836,0.702422731226525,0.795597339453887),
 .UNSPECIFIED.);
#778=B_SPLINE_CURVE_WITH_KNOTS('',3,(#48559,#48560,#48561,#48562,#48563,
#48564,#48565,#48566,#48567,#48568,#48569,#48570,#48571,#48572,#48573,#48574,
#48575,#48576,#48577,#48578,#48579,#48580),.UNSPECIFIED.,.F.,.F.,(4,2,2,
2,2,2,2,2,2,2,4),(-0.793898774335287,-0.746514719997815,-0.648277050769764,
-0.599653567815491,-0.499874425645475,-0.399738910701365,-0.305164360470678,
-0.207651154701469,-0.109238030629384,-0.0578922718396024,0.),
 .UNSPECIFIED.);
#779=B_SPLINE_CURVE_WITH_KNOTS('',3,(#48583,#48584,#48585,#48586,#48587,
#48588,#48589,#48590,#48591,#48592,#48593,#48594,#48595,#48596,#48597,#48598,
#48599,#48600,#48601,#48602,#48603,#48604,#48605,#48606,#48607,#48608,#48609,
#48610,#48611,#48612,#48613,#48614,#48615,#48616,#48617,#48618,#48619,#48620,
#48621,#48622,#48623,#48624),.UNSPECIFIED.,.F.,.F.,(4,2,2,2,2,2,2,2,2,2,
2,2,2,2,2,2,2,2,2,2,4),(4.04744268479612E-5,0.0723888050419246,0.150253876730198,
0.244248023045839,0.343763946381597,0.435081640514679,0.484290834942794,
0.584376734907669,0.681113147042144,0.72998400442407,0.779993622576139,
0.880540287813974,0.980078111135639,1.08102675755066,1.12973105890516,1.23061503227431,
1.27986097964202,1.37809314185868,1.42365730090318,1.49407955944685,1.55994181257962),
 .UNSPECIFIED.);
#780=B_SPLINE_CURVE_WITH_KNOTS('',3,(#48625,#48626,#48627,#48628,#48629,
#48630),.UNSPECIFIED.,.F.,.F.,(4,2,4),(2.4381224475444E-5,0.0136379782908506,
0.0272291530888202),.UNSPECIFIED.);
#781=B_SPLINE_CURVE_WITH_KNOTS('',3,(#48632,#48633,#48634,#48635,#48636,
#48637,#48638,#48639,#48640,#48641,#48642,#48643,#48644,#48645,#48646,#48647,
#48648,#48649,#48650,#48651,#48652,#48653,#48654,#48655,#48656,#48657,#48658,
#48659,#48660,#48661,#48662,#48663,#48664,#48665),.UNSPECIFIED.,.F.,.F.,
(4,2,2,2,2,2,2,2,2,2,2,2,2,2,2,2,4),(3.2335044050079,3.27389245423008,3.35865616251168,
3.45939263362858,3.54385578027792,3.64452294805333,3.72764425789838,3.82907930277935,
3.87317025517201,3.97294041952549,4.05858009238465,4.15598332557383,4.20351932199527,
4.2848801328365,4.38519455201069,4.44868477138579,4.50206007644754),
 .UNSPECIFIED.);
#782=B_SPLINE_CURVE_WITH_KNOTS('',3,(#48667,#48668,#48669,#48670),
 .UNSPECIFIED.,.F.,.F.,(4,4),(-5.68774429195932E-5,0.),.UNSPECIFIED.);
#783=B_SPLINE_CURVE_WITH_KNOTS('',3,(#48672,#48673,#48674,#48675,#48676,
#48677,#48678,#48679,#48680,#48681),.UNSPECIFIED.,.F.,.F.,(4,2,2,2,4),(0.000110635194286315,
0.0642159947776442,0.156548519658155,0.23536697325852,0.312794483273568),
 .UNSPECIFIED.);
#784=B_SPLINE_CURVE_WITH_KNOTS('',3,(#48682,#48683,#48684,#48685),
 .UNSPECIFIED.,.F.,.F.,(4,4),(1.00000011060521E-6,0.000119906415017354),
 .UNSPECIFIED.);
#785=B_SPLINE_CURVE_WITH_KNOTS('',3,(#48845,#48846,#48847,#48848,#48849,
#48850,#48851,#48852,#48853,#48854,#48855,#48856,#48857,#48858,#48859,#48860,
#48861,#48862,#48863,#48864,#48865,#48866,#48867,#48868,#48869,#48870,#48871,
#48872,#48873,#48874,#48875,#48876,#48877,#48878,#48879,#48880,#48881,#48882,
#48883,#48884,#48885,#48886,#48887,#48888,#48889,#48890,#48891,#48892,#48893,
#48894,#48895,#48896,#48897,#48898,#48899,#48900,#48901,#48902,#48903,#48904,
#48905,#48906,#48907,#48908,#48909,#48910,#48911,#48912,#48913,#48914,#48915,
#48916,#48917,#48918,#48919,#48920,#48921,#48922,#48923,#48924,#48925,#48926,
#48927,#48928,#48929,#48930,#48931,#48932,#48933,#48934,#48935,#48936,#48937,
#48938,#48939,#48940,#48941,#48942,#48943,#48944,#48945,#48946,#48947,#48948,
#48949,#48950,#48951,#48952,#48953,#48954,#48955,#48956,#48957,#48958,#48959,
#48960,#48961,#48962,#48963,#48964,#48965,#48966,#48967,#48968,#48969,#48970,
#48971,#48972,#48973,#48974,#48975,#48976,#48977,#48978,#48979,#48980,#48981,
#48982,#48983,#48984,#48985,#48986,#48987,#48988,#48989,#48990,#48991,#48992),
 .UNSPECIFIED.,.F.,.F.,(4,3,3,3,3,3,3,3,3,3,3,3,3,3,3,3,3,3,3,3,3,3,3,3,
3,3,3,3,3,3,3,3,3,3,3,3,3,3,3,3,3,3,3,3,3,3,3,3,3,4),(0.981527464250843,
0.982092490001789,0.982250570201131,0.982821922329735,0.983393387693289,
0.983942796582145,0.984165788573041,0.984222792790674,0.984769994125036,
0.985346304630392,0.985920888527997,0.986193875236633,0.986773936837428,
0.986804823810868,0.987331227961664,0.987856154503689,0.988163327839545,
0.988693044486107,0.989148450490744,0.989443859048694,0.989642599247085,
0.989889591278668,0.990013023081767,0.990074724548194,0.990136417005633,
0.990790401665348,0.991461921896627,0.992082894286521,0.992108550310556,
0.992714880848456,0.993325842358457,0.993927728447798,0.994080943138248,
0.994672953070892,0.994721929524347,0.995187789529314,0.995562865020324,
0.996032292855299,0.996503865055638,0.996971618828127,0.99703909746875,
0.997360964762174,0.997938692768488,0.998485881127698,0.998519885957476,
0.998680482381087,0.999045493804115,0.999413210914547,0.999780332009316,
1.),.UNSPECIFIED.);
#786=B_SPLINE_CURVE_WITH_KNOTS('',3,(#48993,#48994,#48995,#48996,#48997,
#48998,#48999,#49000,#49001,#49002,#49003,#49004,#49005,#49006,#49007,#49008,
#49009,#49010,#49011,#49012,#49013,#49014,#49015,#49016,#49017,#49018,#49019,
#49020,#49021,#49022,#49023,#49024,#49025,#49026,#49027,#49028,#49029,#49030,
#49031,#49032,#49033,#49034,#49035,#49036,#49037,#49038,#49039,#49040,#49041,
#49042,#49043,#49044,#49045,#49046,#49047,#49048,#49049,#49050,#49051,#49052,
#49053,#49054,#49055,#49056,#49057,#49058,#49059,#49060,#49061,#49062,#49063,
#49064,#49065,#49066,#49067,#49068,#49069,#49070,#49071,#49072,#49073,#49074,
#49075,#49076,#49077,#49078,#49079,#49080,#49081,#49082,#49083,#49084,#49085,
#49086,#49087,#49088,#49089,#49090,#49091,#49092,#49093,#49094,#49095,#49096,
#49097,#49098,#49099,#49100,#49101,#49102,#49103,#49104,#49105,#49106,#49107,
#49108,#49109,#49110,#49111,#49112,#49113,#49114,#49115,#49116,#49117,#49118,
#49119,#49120,#49121,#49122,#49123,#49124,#49125,#49126,#49127,#49128,#49129,
#49130,#49131,#49132,#49133,#49134,#49135,#49136,#49137,#49138,#49139,#49140,
#49141,#49142,#49143,#49144,#49145,#49146,#49147,#49148,#49149,#49150,#49151,
#49152,#49153,#49154,#49155,#49156,#49157,#49158,#49159,#49160,#49161,#49162,
#49163,#49164,#49165,#49166,#49167,#49168,#49169,#49170,#49171,#49172,#49173,
#49174,#49175,#49176,#49177,#49178,#49179,#49180,#49181,#49182,#49183,#49184,
#49185,#49186,#49187,#49188,#49189,#49190,#49191,#49192,#49193,#49194,#49195,
#49196,#49197,#49198,#49199,#49200,#49201,#49202,#49203,#49204,#49205,#49206,
#49207,#49208,#49209,#49210,#49211,#49212,#49213,#49214,#49215,#49216,#49217,
#49218,#49219,#49220,#49221,#49222,#49223,#49224,#49225,#49226,#49227,#49228,
#49229,#49230,#49231,#49232,#49233,#49234,#49235,#49236,#49237,#49238,#49239,
#49240,#49241,#49242,#49243,#49244,#49245,#49246,#49247,#49248,#49249,#49250,
#49251,#49252,#49253,#49254,#49255,#49256,#49257,#49258,#49259,#49260,#49261,
#49262,#49263,#49264,#49265,#49266,#49267,#49268,#49269,#49270,#49271,#49272,
#49273,#49274,#49275,#49276,#49277,#49278,#49279,#49280,#49281,#49282,#49283,
#49284,#49285,#49286,#49287,#49288,#49289,#49290,#49291,#49292,#49293,#49294,
#49295,#49296,#49297,#49298,#49299),.UNSPECIFIED.,.F.,.F.,(4,3,3,3,3,3,
3,3,3,3,3,3,3,3,3,3,3,3,3,3,3,3,3,3,3,3,3,3,3,3,3,3,3,3,3,3,3,3,3,3,3,3,
3,3,3,3,3,3,3,3,3,3,3,3,3,3,3,3,3,3,3,3,3,3,3,3,3,3,3,3,3,3,3,3,3,3,3,3,
3,3,3,3,3,3,3,3,3,3,3,3,3,3,3,3,3,3,3,3,3,3,3,3,4),(0.958582012693979,0.959057373153544,
0.959531895240945,0.959882163298524,0.960061197080218,0.960594634397,0.960883867419892,
0.961413301456373,0.961540412003173,0.961887365736604,0.962422945132031,
0.962888489257781,0.963423565588256,0.96388924157441,0.964441816459992,
0.964498841849082,0.964994923825078,0.96551746413172,0.966040004438362,
0.966547126147729,0.966895435246582,0.967423872663115,0.967457271694992,
0.968189830473271,0.968984752914132,0.969906680046786,0.970415701540902,
0.970600603406271,0.970785505271641,0.971155309002379,0.971587448549721,
0.971894916463857,0.972353492511569,0.972816476880084,0.972918959336232,
0.973374131386812,0.973985274440157,0.974113738848289,0.97456746908772,
0.974798134679613,0.974939154315201,0.975447610813723,0.975928659806014,
0.976323723048143,0.976623356656524,0.97720260783381,0.977433429455508,
0.977844575774526,0.978394852988506,0.978937302512818,0.979241928683297,
0.979436661700231,0.980111702826308,0.980442642818478,0.980783654976453,
0.981457437902959,0.981947209563255,0.982241057646065,0.98241526310154,
0.983131880691015,0.983452142949751,0.984204488767931,0.984365727673976,
0.98495683458611,0.985555059044411,0.986008035827076,0.986177825090869,
0.986358085398057,0.986461012609742,0.987286338640029,0.987965464622891,
0.988263610898574,0.988834391871281,0.989222790004238,0.989468539305708,
0.989863717687797,0.990058804384792,0.990138567180301,0.99059027119165,
0.990971780718536,0.991424690022283,0.991881017331188,0.99211085374424,
0.992704130080236,0.993282699864252,0.993804782958349,0.99397983369436,
0.99408314030818,0.994581798219916,0.995072076725526,0.995562355231135,
0.995988544787359,0.996408145874342,0.996820844800321,0.996993103554728,
0.99704157015409,0.997589077496104,0.998172708728611,0.998496173800892,
0.998520785077045,0.999156675232777,0.999733891928085,1.),.UNSPECIFIED.);
#787=B_SPLINE_CURVE_WITH_KNOTS('',3,(#49449,#49450,#49451,#49452,#49453,
#49454,#49455,#49456,#49457,#49458,#49459,#49460,#49461,#49462,#49463,#49464,
#49465,#49466,#49467,#49468,#49469,#49470,#49471,#49472,#49473,#49474,#49475,
#49476,#49477,#49478,#49479,#49480,#49481,#49482,#49483,#49484,#49485,#49486,
#49487,#49488,#49489,#49490,#49491,#49492,#49493,#49494,#49495,#49496,#49497,
#49498,#49499,#49500,#49501,#49502,#49503,#49504,#49505,#49506,#49507,#49508,
#49509,#49510,#49511,#49512,#49513,#49514,#49515,#49516,#49517,#49518,#49519,
#49520,#49521,#49522,#49523,#49524,#49525,#49526,#49527,#49528,#49529,#49530,
#49531,#49532,#49533,#49534,#49535,#49536,#49537,#49538,#49539,#49540,#49541,
#49542,#49543,#49544,#49545,#49546,#49547,#49548,#49549,#49550,#49551,#49552,
#49553,#49554,#49555,#49556,#49557,#49558,#49559,#49560,#49561,#49562,#49563,
#49564,#49565,#49566,#49567,#49568,#49569,#49570,#49571,#49572,#49573,#49574,
#49575,#49576,#49577,#49578,#49579,#49580,#49581,#49582,#49583,#49584,#49585,
#49586,#49587,#49588,#49589,#49590,#49591,#49592,#49593,#49594,#49595,#49596,
#49597,#49598,#49599,#49600,#49601,#49602,#49603,#49604,#49605,#49606,#49607,
#49608,#49609,#49610,#49611,#49612,#49613,#49614,#49615,#49616,#49617,#49618,
#49619,#49620,#49621,#49622,#49623,#49624,#49625,#49626,#49627,#49628,#49629,
#49630,#49631,#49632,#49633,#49634,#49635,#49636,#49637,#49638,#49639,#49640,
#49641,#49642,#49643,#49644,#49645,#49646,#49647,#49648,#49649,#49650,#49651,
#49652,#49653,#49654,#49655,#49656,#49657,#49658,#49659,#49660,#49661,#49662,
#49663,#49664,#49665,#49666,#49667,#49668,#49669,#49670,#49671,#49672,#49673,
#49674,#49675,#49676,#49677),.UNSPECIFIED.,.F.,.F.,(4,3,3,3,3,3,3,3,3,3,
3,3,3,3,3,3,3,3,3,3,3,3,3,3,3,3,3,3,3,3,3,3,3,3,3,3,3,3,3,3,3,3,3,3,3,3,
3,3,3,3,3,3,3,3,3,3,3,3,3,3,3,3,3,3,3,3,3,3,3,3,3,3,3,3,3,3,4),(0.,0.000359963247642554,
0.000730782414337265,0.00109740071145868,0.00147032031294004,0.0018432399144214,
0.00205249069972499,0.00246150015657244,0.00287147315877874,0.00327897649381078,
0.00368647982884281,0.00409556414483304,0.00466610669130213,0.00523323942328513,
0.00552971974326421,0.0059521096061035,0.00614735487448577,0.00656909827483017,
0.00698845597869335,0.00737295965768562,0.0079845207093368,0.00819395765445556,
0.00827915432352533,0.0083643463698637,0.00853472530094449,0.00887552345905345,
0.0094701356547484,0.00955776993844597,0.00983061287691415,0.0104636984438137,
0.0109235719412858,0.0115603343811466,0.0121819050867249,0.0122882660961427,
0.0122883630402977,0.0127442522716054,0.0132022542537409,0.013517092705757,
0.0136535057723781,0.0140302785058248,0.0141315060105641,0.0144387126629677,
0.0147285348775666,0.0147459193153712,0.0150194560827448,0.0156407003907238,
0.01626246681243,0.0163840835398903,0.0169918228636084,0.0172035725345998,
0.0174092876371001,0.0179973749126947,0.0184340180115974,0.0190184385959836,
0.0194590321259564,0.0196612257538283,0.0199723493251172,0.0204851674142444,
0.021014578815863,0.0215667288944599,0.0220834328614806,0.0221188789730568,
0.0225373035513935,0.023173079715083,0.0238191067694135,0.0244491815377821,
0.0245765321922854,0.0245864657268039,0.0251991054859768,0.0258053588018997,
0.0263050134535735,0.0266347536340908,0.0270341854115139,0.0275500268891959,
0.0280703359425124,0.0285935267829691,0.0286806425028429),.UNSPECIFIED.);
#788=B_SPLINE_CURVE_WITH_KNOTS('',3,(#49680,#49681,#49682,#49683,#49684,
#49685,#49686,#49687,#49688,#49689,#49690,#49691,#49692,#49693,#49694,#49695,
#49696,#49697,#49698,#49699,#49700,#49701,#49702,#49703,#49704,#49705),
 .UNSPECIFIED.,.F.,.F.,(4,1,1,1,1,1,1,1,1,1,1,1,1,1,1,1,1,1,1,1,1,1,1,4),
(0.,0.00168771915268776,0.00337543830537552,0.00675087661075104,0.0101263149161266,
0.0135017532215021,0.0157520454250858,0.0180023376286695,0.0202526298322531,
0.0219403489849409,0.0236280681376287,0.0253157872903164,0.0270035064430042,
0.0292537986465879,0.0315040908501715,0.0337543830537552,0.0360046752573389,
0.0382549674609226,0.0405052596645063,0.0427555518680899,0.0450058440716736,
0.0472561362752573,0.049506428478841,0.0516089027088776),.UNSPECIFIED.);
#789=B_SPLINE_CURVE_WITH_KNOTS('',3,(#49954,#49955,#49956,#49957,#49958,
#49959,#49960,#49961,#49962,#49963,#49964,#49965,#49966,#49967,#49968,#49969,
#49970,#49971,#49972,#49973,#49974,#49975,#49976,#49977,#49978,#49979,#49980,
#49981,#49982,#49983,#49984,#49985,#49986,#49987,#49988,#49989,#49990,#49991,
#49992,#49993,#49994,#49995,#49996,#49997,#49998,#49999,#50000,#50001,#50002,
#50003,#50004,#50005,#50006,#50007,#50008,#50009,#50010,#50011,#50012,#50013,
#50014,#50015,#50016,#50017,#50018,#50019,#50020,#50021,#50022,#50023,#50024,
#50025,#50026,#50027,#50028,#50029,#50030,#50031,#50032,#50033,#50034,#50035,
#50036,#50037,#50038,#50039,#50040,#50041,#50042,#50043,#50044,#50045,#50046,
#50047,#50048,#50049,#50050,#50051,#50052,#50053,#50054,#50055,#50056,#50057,
#50058,#50059,#50060,#50061,#50062,#50063,#50064,#50065,#50066,#50067,#50068,
#50069,#50070,#50071,#50072,#50073,#50074,#50075,#50076,#50077,#50078,#50079,
#50080,#50081,#50082,#50083,#50084,#50085,#50086,#50087,#50088,#50089,#50090,
#50091,#50092,#50093,#50094,#50095,#50096,#50097,#50098,#50099,#50100,#50101,
#50102,#50103,#50104,#50105,#50106,#50107,#50108,#50109,#50110,#50111,#50112,
#50113,#50114,#50115,#50116,#50117,#50118,#50119,#50120,#50121,#50122,#50123,
#50124,#50125,#50126,#50127,#50128,#50129,#50130,#50131,#50132,#50133,#50134,
#50135,#50136,#50137,#50138,#50139,#50140,#50141,#50142,#50143,#50144,#50145,
#50146,#50147,#50148,#50149,#50150,#50151,#50152,#50153,#50154,#50155,#50156,
#50157,#50158,#50159,#50160,#50161,#50162,#50163,#50164,#50165,#50166,#50167,
#50168,#50169,#50170,#50171,#50172,#50173,#50174,#50175,#50176,#50177,#50178,
#50179,#50180,#50181,#50182,#50183,#50184,#50185,#50186,#50187,#50188,#50189,
#50190,#50191,#50192,#50193,#50194,#50195,#50196,#50197,#50198,#50199,#50200,
#50201,#50202,#50203,#50204,#50205,#50206,#50207,#50208,#50209,#50210,#50211,
#50212,#50213,#50214,#50215,#50216,#50217,#50218,#50219,#50220,#50221,#50222,
#50223,#50224,#50225,#50226,#50227,#50228,#50229,#50230,#50231,#50232,#50233,
#50234,#50235,#50236,#50237,#50238,#50239,#50240,#50241,#50242,#50243,#50244,
#50245,#50246,#50247,#50248,#50249,#50250,#50251,#50252,#50253,#50254,#50255,
#50256,#50257,#50258,#50259,#50260,#50261,#50262,#50263,#50264,#50265,#50266,
#50267,#50268,#50269,#50270,#50271,#50272,#50273,#50274,#50275,#50276,#50277,
#50278,#50279,#50280,#50281,#50282,#50283,#50284,#50285,#50286,#50287,#50288,
#50289,#50290,#50291,#50292,#50293,#50294,#50295,#50296,#50297,#50298,#50299,
#50300,#50301,#50302,#50303,#50304,#50305,#50306,#50307,#50308,#50309,#50310,
#50311,#50312,#50313,#50314,#50315,#50316,#50317,#50318,#50319,#50320,#50321,
#50322,#50323,#50324,#50325,#50326,#50327,#50328,#50329,#50330,#50331,#50332,
#50333,#50334,#50335,#50336,#50337,#50338,#50339,#50340,#50341,#50342,#50343,
#50344,#50345,#50346,#50347,#50348,#50349,#50350,#50351,#50352,#50353,#50354,
#50355,#50356,#50357,#50358,#50359,#50360,#50361,#50362,#50363,#50364,#50365,
#50366,#50367,#50368,#50369,#50370,#50371,#50372,#50373,#50374,#50375,#50376,
#50377,#50378,#50379,#50380,#50381,#50382,#50383,#50384,#50385,#50386,#50387,
#50388,#50389,#50390,#50391,#50392,#50393,#50394,#50395,#50396,#50397,#50398,
#50399,#50400,#50401,#50402,#50403,#50404,#50405,#50406,#50407,#50408,#50409,
#50410,#50411,#50412,#50413,#50414,#50415,#50416,#50417,#50418,#50419,#50420,
#50421,#50422,#50423,#50424,#50425,#50426,#50427,#50428,#50429,#50430,#50431,
#50432,#50433,#50434,#50435,#50436,#50437,#50438,#50439,#50440,#50441,#50442,
#50443,#50444,#50445,#50446,#50447,#50448,#50449,#50450,#50451,#50452,#50453,
#50454,#50455,#50456,#50457,#50458,#50459,#50460,#50461,#50462,#50463,#50464,
#50465,#50466,#50467,#50468,#50469,#50470,#50471,#50472,#50473,#50474,#50475,
#50476,#50477,#50478,#50479,#50480,#50481,#50482,#50483,#50484,#50485,#50486,
#50487,#50488,#50489,#50490,#50491,#50492,#50493,#50494,#50495,#50496,#50497,
#50498,#50499,#50500,#50501,#50502,#50503,#50504,#50505,#50506,#50507,#50508,
#50509,#50510,#50511,#50512,#50513,#50514,#50515,#50516,#50517,#50518,#50519,
#50520,#50521,#50522,#50523,#50524),.UNSPECIFIED.,.F.,.F.,(4,3,3,3,3,3,
3,3,3,3,3,3,3,3,3,3,3,3,3,3,3,3,3,3,3,3,3,3,3,3,3,3,3,3,3,3,3,3,3,3,3,3,
3,3,3,3,3,3,3,3,3,3,3,3,3,3,3,3,3,3,3,3,3,3,3,3,3,3,3,3,3,3,3,3,3,3,3,3,
3,3,3,3,3,3,3,3,3,3,3,3,3,3,3,3,3,3,3,3,3,3,3,3,3,3,3,3,3,3,3,3,3,3,3,3,
3,3,3,3,3,3,3,3,3,3,3,3,3,3,3,3,3,3,3,3,3,3,3,3,3,3,3,3,3,3,3,3,3,3,3,3,
3,3,3,3,3,3,3,3,3,3,3,3,3,3,3,3,3,3,3,3,3,3,3,3,3,3,3,3,3,3,3,3,3,3,3,3,
3,3,3,3,4),(0.116743831555477,0.117271549516828,0.11780216534719,0.11788849433131,
0.118426160808469,0.118587303856748,0.11917275494541,0.119775021091971,
0.120086717938801,0.120430777434874,0.121054310593861,0.121685110717334,
0.122274251012999,0.12228523422923,0.123031324335223,0.123826254050568,
0.124117724591124,0.124484080881706,0.12508074012303,0.125679687701571,
0.125961198169249,0.126465937736982,0.126682936526009,0.127187310823517,
0.12769297006349,0.127804671747374,0.128380611942788,0.128882267748352,
0.129462222463457,0.1296481453255,0.130246401265819,0.130844664477249,0.131081032058959,
0.131491618903625,0.132216391580684,0.132961094929179,0.13328064537096,
0.133949583674458,0.134564074867167,0.134992464280823,0.135178566059875,
0.135480920211346,0.135944234328319,0.136407548445292,0.136969195600248,
0.137540892158841,0.137679203351775,0.13827235828395,0.138865513216126,
0.13940169277199,0.139877677745977,0.140415028110087,0.140948862946838,
0.141323477986959,0.141853960541869,0.142075928851122,0.142605303520816,
0.143140587343418,0.143664932145426,0.143781442757793,0.144272847527163,
0.144905224088376,0.145547409087995,0.145737719603048,0.146239407528626,
0.14679346636521,0.147203111292158,0.147754842038307,0.14793523366648,0.148082881106752,
0.148640997946119,0.149202345746228,0.149742549988632,0.149926354684877,
0.150134740024583,0.150666497234683,0.151218162748842,0.151731359132526,
0.151769828263002,0.152255334955058,0.152738824720568,0.153068393525934,
0.153546079527893,0.153613301841127,0.154134366158647,0.154663823869616,
0.15518067074369,0.155456775419252,0.155933374262726,0.156001424139149,
0.156474008906968,0.156949475429383,0.157300248997378,0.157822080516296,
0.158342074467166,0.158850602623591,0.158934402298568,0.159143722575503,
0.159618178955598,0.160094893609646,0.160566033713449,0.160987196153628,
0.161534655156901,0.16186632610495,0.162409222101943,0.162597882746008,
0.162830669731753,0.163329952357396,0.164061883361872,0.164674143309878,
0.164794026868702,0.165224924373528,0.165639434318916,0.16605195816296,
0.16646105129726,0.166517616888004,0.166948623268704,0.167376252184625,
0.167726925135452,0.168152505538122,0.168361090466129,0.168918885736223,
0.169493042266387,0.170052921258187,0.170204564044254,0.170661873459268,
0.17111916645363,0.171583602038004,0.172048037622379,0.172128378269063,
0.172672616208526,0.172861957993751,0.173407038755241,0.1735948610192,0.173891511200504,
0.174445121479788,0.17499691825412,0.175548715028451,0.17573498477863,0.176037821849044,
0.176526392526301,0.177132526087169,0.177503099434671,0.178104359208324,
0.178192949549463,0.178698491217907,0.179210480324561,0.179457562571755,
0.179967365167328,0.180470635330094,0.180650914320297,0.181182328720393,
0.181656663721916,0.182185008959917,0.182710296611938,0.18310887909113,
0.183628901543184,0.183855228361026,0.184378510206937,0.184904700846289,
0.185423217261101,0.185566843861964,0.18605279219044,0.186521820203989,
0.186795826247381,0.187361663261442,0.187921947018491,0.188024808632798,
0.18825153231159,0.188963922315969,0.189709904046076,0.190450508127851,
0.190482773403631,0.19109726459634,0.191711755789048,0.19220148550707,0.192651271329696,
0.192940738174465,0.193247983770819,0.193555229367173,0.194102040676105,
0.194169720559882,0.194528383952344,0.19478421175259,0.194852339466579,
0.195183787620667,0.195398702945298,0.19585180183904,0.19630739318511,0.196762420619596,
0.197048670931309),.UNSPECIFIED.);
#790=B_SPLINE_CURVE_WITH_KNOTS('',3,(#50525,#50526,#50527,#50528,#50529,
#50530,#50531,#50532,#50533,#50534,#50535,#50536,#50537,#50538,#50539,#50540,
#50541,#50542,#50543,#50544,#50545,#50546,#50547,#50548,#50549,#50550,#50551,
#50552,#50553,#50554,#50555,#50556,#50557,#50558,#50559,#50560,#50561,#50562,
#50563,#50564,#50565,#50566,#50567),.UNSPECIFIED.,.F.,.F.,(4,1,1,1,1,1,
1,1,1,1,1,1,1,1,1,1,1,1,1,1,1,1,1,1,1,1,1,1,1,1,1,1,1,1,1,1,1,1,1,1,4),
(0.139688666527305,0.141888509865,0.144088353202694,0.146288196540389,0.148488039878084,
0.150687883215779,0.152887726553474,0.155087569891169,0.157287413228864,
0.160220537679124,0.163153662129384,0.164620224354514,0.166086786579644,
0.167553348804774,0.169019911029903,0.171953035480163,0.174886159930423,
0.177086003268118,0.179285846605813,0.181485689943508,0.183685533281203,
0.184235494115627,0.18478545495005,0.185885376618898,0.188085219956593,
0.190285063294288,0.192484906631983,0.194684749969677,0.196884593307372,
0.199084436645067,0.200184358313915,0.200734319148339,0.201284279982762,
0.203484123320457,0.205683966658152,0.207883809995847,0.210083653333542,
0.213016777783802,0.215949902234062,0.218883026684322,0.219978350651175),
 .UNSPECIFIED.);
#791=B_SPLINE_CURVE_WITH_KNOTS('',3,(#50844,#50845,#50846,#50847,#50848,
#50849,#50850,#50851,#50852,#50853,#50854,#50855,#50856,#50857,#50858,#50859,
#50860,#50861,#50862,#50863,#50864,#50865,#50866,#50867,#50868,#50869,#50870,
#50871,#50872,#50873,#50874,#50875,#50876,#50877,#50878,#50879,#50880,#50881,
#50882,#50883,#50884,#50885,#50886,#50887,#50888,#50889,#50890,#50891,#50892,
#50893,#50894,#50895,#50896,#50897,#50898,#50899,#50900,#50901,#50902,#50903,
#50904,#50905,#50906,#50907,#50908,#50909,#50910,#50911,#50912,#50913,#50914,
#50915,#50916,#50917,#50918,#50919,#50920,#50921,#50922,#50923,#50924,#50925,
#50926,#50927,#50928,#50929,#50930,#50931,#50932,#50933,#50934,#50935,#50936,
#50937,#50938,#50939,#50940,#50941,#50942,#50943,#50944,#50945,#50946,#50947,
#50948,#50949,#50950,#50951,#50952,#50953,#50954,#50955,#50956,#50957,#50958,
#50959,#50960,#50961,#50962,#50963,#50964,#50965,#50966,#50967,#50968,#50969,
#50970,#50971,#50972,#50973,#50974,#50975,#50976,#50977,#50978,#50979,#50980,
#50981,#50982,#50983,#50984,#50985,#50986,#50987,#50988,#50989,#50990,#50991,
#50992,#50993,#50994,#50995,#50996,#50997,#50998,#50999,#51000,#51001,#51002,
#51003,#51004,#51005,#51006,#51007,#51008,#51009,#51010,#51011,#51012,#51013,
#51014,#51015,#51016,#51017,#51018,#51019,#51020,#51021,#51022,#51023,#51024,
#51025,#51026,#51027,#51028,#51029,#51030,#51031,#51032,#51033,#51034,#51035,
#51036,#51037,#51038,#51039,#51040,#51041,#51042,#51043,#51044,#51045,#51046,
#51047,#51048,#51049,#51050,#51051,#51052,#51053,#51054,#51055,#51056,#51057,
#51058,#51059,#51060,#51061,#51062,#51063,#51064,#51065,#51066,#51067,#51068,
#51069,#51070,#51071,#51072,#51073,#51074,#51075,#51076,#51077,#51078,#51079,
#51080,#51081,#51082,#51083,#51084,#51085,#51086,#51087,#51088,#51089,#51090,
#51091,#51092,#51093,#51094,#51095,#51096,#51097,#51098,#51099,#51100,#51101,
#51102,#51103,#51104,#51105,#51106,#51107,#51108,#51109,#51110,#51111,#51112,
#51113,#51114,#51115,#51116,#51117,#51118,#51119,#51120,#51121,#51122,#51123,
#51124,#51125,#51126,#51127,#51128,#51129,#51130,#51131,#51132,#51133,#51134,
#51135,#51136,#51137,#51138,#51139,#51140,#51141,#51142,#51143,#51144,#51145,
#51146,#51147,#51148,#51149,#51150,#51151,#51152,#51153,#51154,#51155,#51156,
#51157,#51158,#51159,#51160,#51161,#51162,#51163,#51164,#51165,#51166,#51167,
#51168,#51169,#51170,#51171,#51172,#51173,#51174,#51175,#51176,#51177,#51178,
#51179,#51180,#51181,#51182,#51183,#51184,#51185,#51186,#51187,#51188,#51189,
#51190,#51191,#51192,#51193,#51194,#51195,#51196,#51197,#51198,#51199,#51200,
#51201,#51202,#51203,#51204,#51205,#51206,#51207,#51208,#51209,#51210,#51211,
#51212,#51213,#51214,#51215,#51216,#51217,#51218,#51219,#51220,#51221,#51222,
#51223,#51224,#51225,#51226,#51227,#51228,#51229,#51230,#51231,#51232,#51233,
#51234,#51235,#51236,#51237,#51238,#51239),.UNSPECIFIED.,.F.,.F.,(4,2,2,
2,2,2,2,2,2,2,2,2,2,2,2,2,2,2,2,2,2,2,2,2,2,2,2,2,2,2,2,2,2,2,2,2,2,2,2,
2,2,2,2,2,2,2,2,2,2,2,2,2,2,2,2,2,2,2,2,2,2,2,2,2,2,2,2,2,2,2,2,2,2,2,2,
2,2,2,2,2,2,2,2,2,2,2,2,2,2,2,2,2,2,2,2,2,2,2,2,2,2,2,2,2,2,2,2,2,2,2,2,
2,2,2,2,2,2,2,2,2,2,2,2,2,2,2,2,2,2,2,2,2,2,2,2,2,2,2,2,2,2,2,2,2,2,2,2,
2,2,2,2,2,2,2,2,2,2,2,2,2,2,2,2,2,2,2,2,2,2,2,2,2,2,2,2,2,2,2,2,2,2,2,2,
2,2,2,2,2,2,2,2,2,2,2,2,2,2,4),(0.285111806346874,0.285640371084623,0.286169688619292,
0.286253528781122,0.28679049202008,0.286954925748233,0.287624941988217,
0.288322782411678,0.288452680346209,0.288798399656758,0.289447319071883,
0.29011084240271,0.290641873565284,0.290652246933881,0.291414851470538,
0.291751755837375,0.292485347473809,0.292851528592237,0.293505663327753,
0.293951003885431,0.294281878521236,0.294411806864067,0.294947623823447,
0.295050766229014,0.295600713975397,0.296013174785185,0.296163107931787,
0.296266722938215,0.296813898716011,0.297250557214549,0.29781023827113,
0.298006955465365,0.29814817767842,0.298824649511877,0.299450041448425,
0.29985924310791,0.300456377556101,0.301066857549586,0.301648532377361,
0.302261918074419,0.302317208319277,0.302848546895361,0.303388381324519,
0.303846251520219,0.304388329451953,0.304775173530644,0.305337847954477,
0.305912156270017,0.306046151016494,0.306639644879253,0.307233138742011,
0.307749298247224,0.308245332269785,0.308763863101548,0.309076612650536,
0.30987698412567,0.310443547903747,0.310920086559061,0.311781227445867,
0.312588144003948,0.312642368332673,0.312763560467587,0.313303200481775,
0.31386237748905,0.314427200435492,0.314607034376112,0.315046976447381,
0.315483786381483,0.315573150254336,0.316013598145793,0.316450508284637,
0.316964560632992,0.317475657386103,0.317962930768564,0.318293982193163,
0.318501368989331,0.318904406997231,0.319215719147425,0.319637107883235,
0.320063230859427,0.320137456101688,0.320614464130452,0.320828758817385,
0.32105919305595,0.32143188567371,0.32161347578906,0.321750495771647,0.321980930010213,
0.322465194307811,0.322962701555398,0.323455598846691,0.323922283517711,
0.32428527239587,0.324363062752028,0.324816416375222,0.325266314686911,
0.325667877827264,0.326212295021501,0.326765838711299,0.327296277392487,
0.327864683041269,0.328403985140896,0.328433088690051,0.328909994031669,
0.329354825644314,0.329964329620402,0.330231406193989,0.330843324987258,
0.331198299552839,0.331699223621591,0.332242822753204,0.332432288182419,
0.332798816968857,0.333041773461365,0.333165629225368,0.333595533761498,
0.334009505508754,0.334421685174999,0.334830881689862,0.33488524736989,
0.335330563646124,0.335773794074081,0.336100769244151,0.336540569023547,
0.336728721278415,0.337189589755546,0.337567352148602,0.337650458232678,
0.338132913214294,0.33857219518694,0.338994920565243,0.339033472503465,
0.339453103438159,0.339493932141203,0.33981815411855,0.340142638771275,
0.340415669095466,0.340838079174422,0.341260533567594,0.341682693714999,
0.341963208106005,0.342259143003991,0.342947012186205,0.343638635766066,
0.343918284848948,0.344362602634211,0.345116924982843,0.345871247331475,
0.346274226969221,0.347049537036131,0.347586983698222,0.347824847103041,
0.348374001532803,0.348648513521792,0.348923042595576,0.349472333873503,
0.349623750066329,0.349773890326151,0.350021898056725,0.35065911454714,
0.35112045281866,0.351343653761936,0.351484905463245,0.351852249073299,
0.352115036902343,0.352219592683353,0.35239824950088,0.352705495152301,
0.353172017206261,0.353638044531663,0.353934477757984,0.354419567683639,
0.355097222338029,0.355783241653761,0.356392442969351,0.356619162091783,
0.357060054857063,0.357504178211808,0.357621425575035,0.357996578083137,
0.358235916877876,0.358653902590294,0.358818025956889,0.358850408180718,
0.359578759831332,0.360297492507432,0.360975177719308,0.361016225183532,
0.361308373392085,0.361859361467179,0.362420715176227,0.362979009728679,
0.363215660397334,0.363766338603452,0.364237719657693,0.364712606478098,
0.365187957031571,0.365413919238787),.UNSPECIFIED.);
#792=B_SPLINE_CURVE_WITH_KNOTS('',3,(#51240,#51241,#51242,#51243,#51244,
#51245,#51246,#51247,#51248,#51249,#51250,#51251,#51252,#51253,#51254,#51255,
#51256,#51257,#51258,#51259,#51260,#51261,#51262,#51263,#51264,#51265,#51266,
#51267,#51268,#51269,#51270,#51271,#51272,#51273,#51274,#51275,#51276,#51277,
#51278,#51279,#51280,#51281,#51282,#51283,#51284,#51285,#51286,#51287,#51288,
#51289,#51290,#51291,#51292,#51293,#51294,#51295,#51296,#51297,#51298,#51299,
#51300,#51301,#51302,#51303,#51304,#51305,#51306,#51307,#51308,#51309,#51310,
#51311,#51312,#51313,#51314,#51315,#51316,#51317,#51318,#51319,#51320,#51321,
#51322,#51323,#51324,#51325,#51326,#51327,#51328,#51329,#51330,#51331,#51332,
#51333,#51334,#51335,#51336,#51337,#51338,#51339,#51340,#51341,#51342,#51343,
#51344,#51345,#51346,#51347,#51348,#51349,#51350,#51351,#51352,#51353,#51354,
#51355,#51356,#51357,#51358,#51359,#51360,#51361,#51362,#51363,#51364,#51365,
#51366,#51367,#51368,#51369,#51370,#51371,#51372,#51373,#51374,#51375,#51376,
#51377,#51378,#51379,#51380,#51381,#51382,#51383,#51384,#51385,#51386,#51387,
#51388,#51389,#51390,#51391,#51392,#51393,#51394,#51395,#51396,#51397,#51398,
#51399,#51400,#51401,#51402,#51403,#51404,#51405,#51406,#51407,#51408,#51409,
#51410,#51411,#51412,#51413,#51414,#51415,#51416,#51417,#51418,#51419,#51420,
#51421,#51422,#51423,#51424,#51425,#51426,#51427,#51428,#51429,#51430,#51431,
#51432,#51433,#51434,#51435,#51436,#51437,#51438,#51439,#51440,#51441,#51442,
#51443,#51444,#51445,#51446,#51447,#51448,#51449,#51450,#51451,#51452,#51453,
#51454,#51455,#51456,#51457,#51458,#51459,#51460,#51461,#51462,#51463,#51464,
#51465,#51466,#51467,#51468,#51469,#51470,#51471,#51472,#51473,#51474,#51475,
#51476,#51477,#51478,#51479,#51480,#51481,#51482,#51483,#51484,#51485,#51486,
#51487,#51488,#51489,#51490,#51491,#51492,#51493,#51494,#51495,#51496,#51497,
#51498,#51499,#51500,#51501,#51502,#51503,#51504,#51505,#51506,#51507,#51508,
#51509,#51510,#51511,#51512,#51513,#51514,#51515,#51516,#51517,#51518,#51519,
#51520,#51521,#51522,#51523,#51524,#51525,#51526,#51527,#51528,#51529,#51530,
#51531,#51532,#51533,#51534,#51535,#51536,#51537,#51538,#51539,#51540,#51541,
#51542,#51543,#51544,#51545,#51546,#51547,#51548,#51549,#51550,#51551,#51552,
#51553,#51554,#51555,#51556,#51557,#51558,#51559,#51560,#51561,#51562,#51563,
#51564,#51565,#51566,#51567,#51568,#51569,#51570,#51571,#51572,#51573,#51574,
#51575,#51576,#51577,#51578,#51579,#51580,#51581,#51582,#51583,#51584,#51585,
#51586,#51587,#51588,#51589,#51590,#51591,#51592,#51593,#51594,#51595,#51596,
#51597,#51598,#51599,#51600,#51601,#51602,#51603,#51604,#51605,#51606,#51607,
#51608,#51609,#51610,#51611,#51612,#51613,#51614,#51615,#51616,#51617,#51618,
#51619,#51620,#51621,#51622,#51623,#51624,#51625,#51626,#51627,#51628,#51629,
#51630,#51631,#51632,#51633,#51634,#51635,#51636,#51637,#51638,#51639,#51640,
#51641,#51642,#51643,#51644,#51645,#51646,#51647,#51648,#51649,#51650,#51651,
#51652,#51653,#51654,#51655,#51656,#51657,#51658,#51659,#51660,#51661,#51662,
#51663,#51664,#51665,#51666,#51667,#51668,#51669,#51670,#51671,#51672,#51673,
#51674,#51675,#51676,#51677,#51678,#51679,#51680,#51681,#51682,#51683,#51684,
#51685,#51686,#51687,#51688,#51689,#51690,#51691,#51692,#51693,#51694,#51695,
#51696,#51697,#51698,#51699,#51700,#51701,#51702,#51703,#51704,#51705,#51706,
#51707,#51708,#51709,#51710,#51711,#51712,#51713,#51714,#51715,#51716,#51717,
#51718,#51719,#51720,#51721,#51722,#51723,#51724,#51725,#51726,#51727,#51728,
#51729,#51730,#51731,#51732,#51733,#51734,#51735,#51736,#51737,#51738,#51739,
#51740,#51741,#51742,#51743,#51744,#51745,#51746,#51747,#51748,#51749,#51750,
#51751,#51752,#51753,#51754,#51755,#51756,#51757,#51758,#51759,#51760,#51761,
#51762,#51763,#51764,#51765,#51766,#51767,#51768,#51769,#51770,#51771,#51772,
#51773,#51774,#51775,#51776,#51777,#51778,#51779,#51780,#51781,#51782,#51783,
#51784,#51785,#51786,#51787,#51788,#51789,#51790,#51791,#51792,#51793,#51794,
#51795,#51796,#51797,#51798,#51799,#51800,#51801,#51802,#51803,#51804,#51805,
#51806,#51807,#51808,#51809,#51810,#51811,#51812,#51813,#51814,#51815,#51816,
#51817,#51818,#51819,#51820,#51821,#51822,#51823,#51824,#51825,#51826,#51827,
#51828,#51829,#51830,#51831,#51832,#51833,#51834,#51835,#51836,#51837,#51838,
#51839,#51840,#51841,#51842,#51843,#51844,#51845,#51846,#51847,#51848,#51849,
#51850,#51851,#51852,#51853,#51854,#51855,#51856,#51857,#51858,#51859,#51860,
#51861,#51862,#51863,#51864,#51865,#51866,#51867,#51868,#51869,#51870,#51871,
#51872,#51873,#51874,#51875,#51876,#51877,#51878,#51879,#51880,#51881,#51882,
#51883,#51884,#51885,#51886,#51887,#51888,#51889,#51890,#51891,#51892,#51893,
#51894,#51895,#51896,#51897,#51898,#51899,#51900,#51901,#51902,#51903,#51904,
#51905,#51906,#51907,#51908,#51909,#51910,#51911,#51912,#51913,#51914,#51915,
#51916,#51917,#51918,#51919,#51920,#51921,#51922,#51923,#51924,#51925,#51926,
#51927,#51928,#51929,#51930,#51931,#51932,#51933,#51934,#51935,#51936,#51937,
#51938,#51939,#51940,#51941,#51942,#51943,#51944,#51945,#51946,#51947,#51948,
#51949,#51950,#51951,#51952,#51953,#51954,#51955,#51956,#51957,#51958,#51959,
#51960,#51961,#51962,#51963,#51964,#51965,#51966,#51967,#51968,#51969,#51970,
#51971,#51972,#51973,#51974,#51975,#51976,#51977,#51978,#51979,#51980,#51981,
#51982,#51983,#51984,#51985,#51986,#51987,#51988,#51989,#51990,#51991,#51992,
#51993,#51994,#51995,#51996,#51997,#51998,#51999,#52000,#52001,#52002,#52003,
#52004,#52005,#52006,#52007,#52008,#52009,#52010,#52011,#52012,#52013,#52014,
#52015,#52016,#52017,#52018,#52019,#52020,#52021,#52022,#52023,#52024,#52025,
#52026,#52027,#52028,#52029,#52030,#52031,#52032,#52033,#52034,#52035,#52036,
#52037,#52038,#52039,#52040,#52041,#52042,#52043,#52044,#52045,#52046,#52047,
#52048,#52049,#52050,#52051,#52052,#52053,#52054,#52055,#52056,#52057,#52058,
#52059,#52060,#52061,#52062,#52063,#52064,#52065,#52066,#52067,#52068,#52069,
#52070,#52071,#52072,#52073,#52074,#52075,#52076,#52077,#52078,#52079,#52080,
#52081,#52082,#52083,#52084,#52085,#52086,#52087,#52088,#52089,#52090,#52091,
#52092,#52093,#52094,#52095,#52096,#52097,#52098,#52099,#52100,#52101,#52102,
#52103,#52104,#52105,#52106,#52107,#52108,#52109,#52110,#52111,#52112,#52113),
 .UNSPECIFIED.,.F.,.F.,(4,3,3,3,3,3,3,3,3,3,3,3,3,3,3,3,3,3,3,3,3,3,3,3,
3,3,3,3,3,3,3,3,3,3,3,3,3,3,3,3,3,3,3,3,3,3,3,3,3,3,3,3,3,3,3,3,3,3,3,3,
3,3,3,3,3,3,3,3,3,3,3,3,3,3,3,3,3,3,3,3,3,3,3,3,3,3,3,3,3,3,3,3,3,3,3,3,
3,3,3,3,3,3,3,3,3,3,3,3,3,3,3,3,3,3,3,3,3,3,3,3,3,3,3,3,3,3,3,3,3,3,3,3,
3,3,3,3,3,3,3,3,3,3,3,3,3,3,3,3,3,3,3,3,3,3,3,3,3,3,3,3,3,3,3,3,3,3,3,3,
3,3,3,3,3,3,3,3,3,3,3,3,3,3,3,3,3,3,3,3,3,3,3,3,3,3,3,3,3,3,3,3,3,3,3,3,
3,3,3,3,3,3,3,3,3,3,3,3,3,3,3,3,3,3,3,3,3,3,3,3,3,3,3,3,3,3,3,3,3,3,3,3,
3,3,3,3,3,3,3,3,3,3,3,3,3,3,3,3,3,3,3,3,3,3,3,3,3,3,3,3,3,3,3,3,3,3,3,3,
3,3,3,3,3,3,3,3,3,3,3,3,3,3,3,4),(0.30805700545397,0.30842631823362,0.30867821759715,
0.30907401465744,0.309475521913904,0.30969878573946,0.310084850075262,0.310256126873765,
0.310256131102317,0.31059915974391,0.310835644928473,0.310917103883896,
0.311361464873264,0.311498503382682,0.312073982405682,0.312281423858008,
0.31242181744669,0.312456103104523,0.312780347773963,0.313361229956204,
0.314014862562268,0.314383874965016,0.314631411651958,0.314656073911279,
0.31481593937699,0.315325948261099,0.315752028210539,0.316185345841358,
0.316667243001024,0.316855974913424,0.317049160857981,0.317498738314017,
0.317815960493163,0.318192323873742,0.318421262314861,0.318738484211031,
0.318941104723126,0.3190557061072,0.319220033386332,0.319606200915324,0.319815849720664,
0.320142002166964,0.320563452996499,0.320744645139698,0.320833011079153,
0.321063450110493,0.321255347685694,0.321255392999736,0.321524402339523,
0.321754578820996,0.321984584513574,0.322349421139369,0.322513789514616,
0.322870191717163,0.32304938384856,0.323393413079713,0.323455191002369,
0.323455232867165,0.323799503315996,0.324143773764826,0.324286339644825,
0.324763826258503,0.324970686981935,0.325460304805887,0.325655034319044,
0.325655055286748,0.325668256652078,0.326023574000325,0.326252717295575,
0.326698188297976,0.326845081523442,0.3272876544818,0.327610450600534,0.327610528635596,
0.328209641918397,0.328431862720052,0.328780692444404,0.329130126327003,
0.329354547318243,0.329565866882023,0.32956593140403,0.330100378669315,
0.330685215141153,0.331103249152332,0.331375304475226,0.331521283163512,
0.331521356570397,0.331871387584888,0.332086250581248,0.332381287496353,
0.332673958597452,0.333042290801308,0.333395745129851,0.333632492368121,
0.333978279196955,0.334210361582656,0.334454407585746,0.334454426442488,
0.334754111974627,0.334886072344529,0.335403290978656,0.335930000811901,
0.336450809179484,0.336724089775649,0.337030157298995,0.337184706716219,
0.337387532007979,0.337646409194722,0.338015497358372,0.33819427196612,
0.338567449746788,0.339058128376821,0.339122122235974,0.339487702719904,
0.339795946924541,0.340023804866389,0.340320635989051,0.340320656430213,
0.340617966980718,0.340986830911199,0.341447995770135,0.341580162111079,
0.342037187299761,0.342176675861317,0.342255410107777,0.342694862902167,
0.342851202420166,0.34321968720601,0.343253725017748,0.343388466069785,
0.343437040198125,0.343620358480361,0.343987004308469,0.344353653400577,
0.344720289869125,0.34502217580816,0.345511481737521,0.345903021475991,
0.346186825413991,0.346290019253806,0.346684134854412,0.346771735966535,
0.347256414984072,0.347376120546762,0.347684959692493,0.347792901755893,
0.348182416648847,0.348397335910164,0.348801260494588,0.348983690663044,
0.349120029696914,0.349120110024139,0.349511878656296,0.349638586328738,
0.350171678805315,0.350713863430756,0.351247950412733,0.351478110296708,
0.35186663869738,0.352012882520311,0.352053119511091,0.352146286790599,
0.352427332072899,0.3527083773552,0.353202448566926,0.353337453014862,0.353896724536809,
0.353936185320789,0.354252997435823,0.354253088674553,0.354839320655598,
0.354983812875947,0.355725074809772,0.356359295716468,0.356394072507208,
0.356452840752499,0.356452895274245,0.356916177408798,0.357066671348408,
0.357622935711093,0.358047275428847,0.358237001903881,0.358624756547822,
0.358652684069174,0.358652749921928,0.358851700177434,0.359385433389968,
0.359513252456057,0.360182889920953,0.360680968940598,0.360852527385849,
0.360852705659415,0.361309720004682,0.361811647734616,0.361875865205525,
0.362464117954024,0.362872432638893,0.363015400675881,0.363052370702524,
0.363052465480579,0.363597343389616,0.363766420397923,0.364305316667945,
0.364783190914614,0.36484286397938,0.365215551503501,0.3652522140192,0.365252324151075,
0.365670733157252,0.365749468314731,0.366223171767458,0.366714758604002,
0.367141779079656,0.367206704044414,0.367452050719647,0.367452057335875,
0.367867540123123,0.367973089388087,0.368493675853447,0.368678577352071,
0.369194715739538,0.36957912160619,0.36965190065255,0.370143634964898,0.370264773959565,
0.370317917286151,0.370877630019394,0.370932260622303,0.371543209374464,
0.371851736655365,0.371851743969226,0.371956775378399,0.372563771377561,
0.372624713224631,0.373288916771482,0.373595811316661,0.374051574336618,
0.374051587285901,0.374489729711754,0.374611777628573,0.375177352642783,
0.375441071936421,0.376002562899652,0.37625141481233,0.376251430602576,
0.376615047791481,0.376801375987611,0.376801391431745,0.37714273544159,
0.377287061331257,0.377351338795321,0.377351352260914,0.377691341885409,
0.378031167005512,0.378370314928258,0.378451273919252,0.378451289411068,
0.378889799191242,0.379021732686115,0.379408904421259,0.379813728063135,
0.3802739252859,0.38082118757719,0.380973407178383,0.381322088637239,0.38138439299867,
0.381384398341485,0.381744123785997,0.381875836108492,0.382379199283566,
0.382734926594743,0.38297774345126,0.383319049897772,0.383714884070583,
0.383818286330745,0.384157088697015,0.384317522763719,0.38431753840627,
0.384663023268301,0.385080001174113,0.385156982202099,0.385645601046297,
0.386123472022762,0.386503161337802,0.386882830473844,0.386998692941381,
0.387250647185953,0.387250674077535,0.387583139088101,0.387916429900176,
0.388249309169795,0.388346186021293),.UNSPECIFIED.);
#793=B_SPLINE_CURVE_WITH_KNOTS('',3,(#52366,#52367,#52368,#52369,#52370,
#52371,#52372,#52373,#52374,#52375,#52376,#52377,#52378,#52379,#52380,#52381,
#52382,#52383,#52384,#52385,#52386,#52387,#52388,#52389,#52390,#52391,#52392,
#52393,#52394,#52395,#52396,#52397,#52398,#52399,#52400,#52401,#52402,#52403,
#52404,#52405,#52406,#52407,#52408,#52409,#52410,#52411,#52412,#52413,#52414,
#52415,#52416,#52417,#52418,#52419,#52420,#52421,#52422,#52423,#52424,#52425,
#52426,#52427,#52428,#52429,#52430,#52431,#52432,#52433,#52434,#52435,#52436,
#52437,#52438,#52439,#52440,#52441,#52442,#52443,#52444,#52445,#52446,#52447,
#52448,#52449,#52450,#52451,#52452,#52453,#52454,#52455,#52456,#52457,#52458,
#52459,#52460,#52461,#52462,#52463,#52464,#52465,#52466,#52467,#52468,#52469,
#52470,#52471,#52472,#52473,#52474,#52475,#52476,#52477,#52478,#52479,#52480,
#52481,#52482,#52483,#52484,#52485,#52486,#52487,#52488,#52489,#52490,#52491,
#52492,#52493,#52494,#52495,#52496,#52497,#52498,#52499,#52500,#52501,#52502,
#52503,#52504,#52505,#52506,#52507,#52508,#52509,#52510,#52511,#52512,#52513,
#52514,#52515,#52516,#52517,#52518,#52519,#52520,#52521,#52522,#52523,#52524,
#52525,#52526,#52527,#52528,#52529,#52530,#52531,#52532,#52533,#52534,#52535,
#52536,#52537,#52538,#52539,#52540,#52541,#52542,#52543,#52544,#52545,#52546,
#52547,#52548,#52549,#52550,#52551,#52552,#52553,#52554,#52555,#52556,#52557,
#52558,#52559,#52560,#52561,#52562,#52563,#52564,#52565,#52566,#52567,#52568,
#52569,#52570,#52571,#52572,#52573,#52574,#52575,#52576,#52577,#52578,#52579,
#52580,#52581,#52582,#52583,#52584,#52585,#52586,#52587,#52588,#52589,#52590,
#52591,#52592,#52593,#52594,#52595,#52596,#52597,#52598,#52599,#52600,#52601,
#52602,#52603,#52604,#52605,#52606,#52607,#52608,#52609,#52610,#52611,#52612,
#52613,#52614,#52615,#52616,#52617,#52618,#52619,#52620,#52621,#52622,#52623,
#52624,#52625,#52626,#52627,#52628,#52629,#52630,#52631,#52632,#52633,#52634,
#52635,#52636,#52637,#52638,#52639,#52640,#52641,#52642,#52643,#52644,#52645,
#52646,#52647,#52648,#52649,#52650,#52651,#52652,#52653,#52654,#52655,#52656,
#52657,#52658,#52659,#52660,#52661,#52662,#52663,#52664,#52665,#52666,#52667,
#52668,#52669,#52670,#52671,#52672,#52673,#52674,#52675,#52676,#52677,#52678,
#52679,#52680,#52681,#52682,#52683,#52684,#52685,#52686,#52687,#52688,#52689,
#52690,#52691,#52692,#52693,#52694,#52695,#52696,#52697,#52698,#52699,#52700,
#52701,#52702,#52703,#52704,#52705,#52706,#52707,#52708,#52709,#52710,#52711,
#52712,#52713,#52714,#52715,#52716,#52717,#52718,#52719,#52720,#52721,#52722,
#52723,#52724,#52725,#52726,#52727,#52728,#52729,#52730,#52731,#52732,#52733,
#52734,#52735,#52736,#52737,#52738,#52739,#52740,#52741,#52742,#52743,#52744,
#52745,#52746,#52747,#52748,#52749,#52750,#52751,#52752,#52753,#52754,#52755,
#52756,#52757,#52758,#52759,#52760,#52761,#52762,#52763,#52764,#52765,#52766,
#52767,#52768,#52769,#52770,#52771,#52772,#52773,#52774,#52775,#52776,#52777,
#52778,#52779,#52780,#52781,#52782,#52783,#52784,#52785,#52786,#52787,#52788,
#52789,#52790,#52791,#52792,#52793,#52794,#52795,#52796,#52797,#52798,#52799,
#52800,#52801,#52802,#52803,#52804,#52805,#52806,#52807,#52808,#52809,#52810,
#52811,#52812,#52813,#52814,#52815,#52816,#52817,#52818,#52819,#52820,#52821,
#52822,#52823,#52824,#52825,#52826,#52827,#52828,#52829,#52830,#52831,#52832,
#52833,#52834,#52835,#52836,#52837,#52838,#52839,#52840,#52841,#52842,#52843,
#52844,#52845,#52846,#52847,#52848,#52849,#52850,#52851,#52852,#52853,#52854,
#52855,#52856,#52857,#52858,#52859,#52860,#52861,#52862,#52863,#52864,#52865,
#52866,#52867,#52868,#52869,#52870,#52871,#52872,#52873,#52874,#52875,#52876,
#52877,#52878,#52879,#52880,#52881,#52882,#52883,#52884,#52885,#52886,#52887,
#52888,#52889,#52890,#52891,#52892,#52893,#52894,#52895,#52896,#52897,#52898,
#52899,#52900,#52901,#52902,#52903,#52904,#52905,#52906,#52907,#52908,#52909,
#52910,#52911,#52912,#52913,#52914,#52915,#52916,#52917,#52918,#52919,#52920,
#52921,#52922,#52923,#52924,#52925,#52926,#52927,#52928,#52929,#52930,#52931,
#52932,#52933,#52934,#52935,#52936,#52937,#52938,#52939,#52940,#52941,#52942,
#52943,#52944,#52945,#52946,#52947,#52948,#52949,#52950,#52951,#52952,#52953,
#52954,#52955,#52956,#52957,#52958,#52959,#52960,#52961,#52962,#52963,#52964,
#52965,#52966,#52967,#52968,#52969,#52970,#52971,#52972,#52973,#52974,#52975,
#52976,#52977,#52978,#52979,#52980,#52981,#52982,#52983,#52984,#52985,#52986,
#52987,#52988,#52989,#52990,#52991,#52992,#52993,#52994,#52995,#52996,#52997,
#52998,#52999,#53000,#53001,#53002,#53003,#53004,#53005,#53006,#53007,#53008,
#53009,#53010,#53011,#53012,#53013,#53014,#53015,#53016,#53017,#53018,#53019,
#53020,#53021,#53022,#53023,#53024,#53025,#53026,#53027,#53028,#53029,#53030,
#53031,#53032,#53033,#53034,#53035,#53036,#53037,#53038,#53039,#53040,#53041,
#53042,#53043,#53044,#53045,#53046,#53047,#53048,#53049,#53050,#53051,#53052,
#53053,#53054,#53055,#53056,#53057,#53058,#53059,#53060,#53061,#53062,#53063,
#53064,#53065,#53066,#53067,#53068,#53069,#53070,#53071,#53072,#53073,#53074,
#53075,#53076,#53077,#53078,#53079,#53080,#53081,#53082,#53083,#53084,#53085,
#53086,#53087,#53088,#53089,#53090,#53091,#53092,#53093,#53094,#53095,#53096,
#53097,#53098,#53099,#53100,#53101,#53102,#53103,#53104,#53105,#53106,#53107,
#53108,#53109,#53110,#53111,#53112,#53113,#53114,#53115,#53116,#53117,#53118,
#53119,#53120,#53121,#53122,#53123,#53124,#53125,#53126,#53127,#53128,#53129,
#53130,#53131,#53132,#53133,#53134,#53135,#53136,#53137,#53138,#53139,#53140,
#53141,#53142,#53143,#53144,#53145,#53146,#53147,#53148,#53149,#53150,#53151,
#53152,#53153,#53154,#53155,#53156,#53157,#53158,#53159,#53160,#53161,#53162,
#53163,#53164,#53165,#53166,#53167,#53168,#53169,#53170,#53171,#53172,#53173,
#53174,#53175,#53176,#53177,#53178,#53179,#53180,#53181,#53182,#53183,#53184,
#53185,#53186,#53187,#53188,#53189,#53190,#53191,#53192,#53193,#53194,#53195,
#53196,#53197,#53198,#53199,#53200,#53201,#53202,#53203,#53204,#53205,#53206,
#53207,#53208,#53209,#53210,#53211,#53212,#53213,#53214,#53215,#53216,#53217,
#53218,#53219,#53220,#53221,#53222,#53223,#53224,#53225,#53226,#53227,#53228,
#53229,#53230,#53231,#53232,#53233,#53234,#53235,#53236,#53237,#53238,#53239,
#53240,#53241,#53242,#53243,#53244,#53245,#53246,#53247,#53248,#53249,#53250,
#53251,#53252,#53253,#53254,#53255,#53256,#53257,#53258,#53259,#53260,#53261,
#53262,#53263,#53264,#53265,#53266,#53267,#53268,#53269,#53270,#53271,#53272,
#53273,#53274,#53275,#53276,#53277,#53278,#53279,#53280,#53281,#53282,#53283,
#53284,#53285,#53286,#53287,#53288,#53289,#53290,#53291,#53292,#53293,#53294,
#53295,#53296,#53297,#53298,#53299,#53300,#53301,#53302,#53303,#53304,#53305,
#53306,#53307,#53308,#53309,#53310,#53311,#53312,#53313,#53314,#53315,#53316,
#53317,#53318,#53319,#53320,#53321,#53322,#53323,#53324,#53325,#53326),
 .UNSPECIFIED.,.F.,.F.,(4,3,3,3,3,3,3,3,3,3,3,3,3,3,3,3,3,3,3,3,3,3,3,3,
3,3,3,3,3,3,3,3,3,3,3,3,3,3,3,3,3,3,3,3,3,3,3,3,3,3,3,3,3,3,3,3,3,3,3,3,
3,3,3,3,3,3,3,3,3,3,3,3,3,3,3,3,3,3,3,3,3,3,3,3,3,3,3,3,3,3,3,3,3,3,3,3,
3,3,3,3,3,3,3,3,3,3,3,3,3,3,3,3,3,3,3,3,3,3,3,3,3,3,3,3,3,3,3,3,3,3,3,3,
3,3,3,3,3,3,3,3,3,3,3,3,3,3,3,3,3,3,3,3,3,3,3,3,3,3,3,3,3,3,3,3,3,3,3,3,
3,3,3,3,3,3,3,3,3,3,3,3,3,3,3,3,3,3,3,3,3,3,3,3,3,3,3,3,3,3,3,3,3,3,3,3,
3,3,3,3,3,3,3,3,3,3,3,3,3,3,3,3,3,3,3,3,3,3,3,3,3,3,3,3,3,3,3,3,3,3,3,3,
3,3,3,3,3,3,3,3,3,3,3,3,3,3,3,3,3,3,3,3,3,3,3,3,3,3,3,3,3,3,3,3,3,3,3,3,
3,3,3,3,3,3,3,3,3,3,3,3,3,3,3,3,3,3,3,3,3,3,3,3,3,3,3,3,3,3,3,3,3,3,3,3,
3,3,3,3,3,3,3,3,4),(0.45348023372167,0.453790469791108,0.453924734856489,
0.454245381133265,0.454368139113723,0.454621936522178,0.454919149780836,
0.455072257562434,0.45532256751791,0.45532260007357,0.455622708409302,0.455797353300424,
0.456277816308681,0.456622306513274,0.456746369309662,0.457104413997482,
0.457166041104501,0.457166189575094,0.457446635158765,0.457554086603849,
0.457905084192223,0.458018742216773,0.458270496828743,0.458488382055047,
0.458844074732817,0.458952016875946,0.459008977890699,0.459009514691093,
0.459398406076876,0.459620969601057,0.459903843026781,0.460186894759034,
0.460283544912754,0.460486819924068,0.460773324540919,0.460852988277684,
0.460853120225679,0.461266936093801,0.461346485692105,0.46170263458956,
0.461854442266315,0.462238635524003,0.462366824300372,0.462696461864275,
0.462696604245544,0.462988521681667,0.463133914236636,0.463417597442529,
0.463755365498805,0.463850537419796,0.464173842317907,0.46428814986503,
0.464539935450866,0.464540327636473,0.464901176448483,0.465262025260493,
0.465613771301447,0.465946005612296,0.466278618910396,0.466344666797197,
0.466383298363033,0.466383409037458,0.466774064832716,0.466944209080824,
0.467337869911513,0.467501868151571,0.467811578920541,0.468226528326458,
0.468226882624049,0.468655674825323,0.468895378482076,0.469561741320397,
0.469934771302287,0.470012543462751,0.470500435874145,0.470684163544798,
0.470684847406171,0.471074772144608,0.47133474243947,0.471768693167588,
0.472214358331939,0.472764783968333,0.473142136752783,0.473240103260704,
0.473627511153589,0.473685335200338,0.474077597308726,0.474239098296372,
0.47441546230957,0.474750579062031,0.47497023105009,0.475331404887055,0.475521202319557,
0.47560036886865,0.475600776970414,0.475974272746165,0.476153675504332,
0.476473395039719,0.476615557370942,0.476999620058135,0.477169933569646,
0.477604839358826,0.47772129540641,0.478058380682379,0.478058741752536,
0.478554525741549,0.478603057217752,0.47881504225536,0.479259883139497,
0.479358511396559,0.479799823928292,0.479937608965608,0.480339809101745,
0.480476191729039,0.480516706534658,0.480516914981747,0.480858990635641,
0.481011723036403,0.481531322336638,0.481680088986041,0.482211231263052,
0.482360252095033,0.482826342205504,0.48297467131678,0.482974972844709,
0.483208180585816,0.483758094960384,0.483888449525093,0.484433466733313,
0.484572381520078,0.484818144903371,0.484818299872858,0.485221553888479,
0.485405226580635,0.485864202115283,0.486033422535298,0.486453511711716,
0.486661518258747,0.486661618489962,0.48706078821189,0.487188699971035,
0.487604313151055,0.488050168328899,0.488132704130397,0.488504828204312,
0.488505092076554,0.488980465449272,0.489112591207691,0.489646229297193,
0.489715244453029,0.489804221670911,0.490268682788055,0.490348340750487,
0.490348565663145,0.490859220333916,0.491027563260648,0.491271745610459,
0.491455071126767,0.491638390913829,0.492005057114982,0.492191896303053,
0.492192039249736,0.492738480426435,0.49336841108412,0.493427599001982,
0.493960279715027,0.494035385631583,0.494035512836328,0.49420528989616,
0.494900188530942,0.495605736321105,0.495670996327693,0.495878986422919,
0.495879043022329,0.496403845981915,0.497004333193076,0.497136418879869,
0.497319550607677,0.497502688303911,0.497722513479523,0.497869017202689,
0.498183421184899,0.498238753332429,0.498601686955044,0.498644196802806,
0.498644307940159,0.499105065199454,0.499565756669991,0.499565933596102,
0.500043574105038,0.500520944462694,0.500989782434813,0.501409407182693,
0.501409460797714,0.501533833466022,0.501974247889604,0.502010259570668,
0.502485617123122,0.502955772406981,0.503252748847819,0.503252880769284,
0.503640708900326,0.503726654127854,0.504196924619551,0.504464444297072,
0.50493723358145,0.505096354355876,0.505096372603651,0.505583039999626,
0.506074503568958,0.506553654026795,0.506939827942467,0.507327666055506,
0.507397317486871,0.507400696339115,0.507400745932985,0.507807282713654,
0.50821458149422,0.508621067184384,0.508783203899882,0.508783301529058,
0.509176966489728,0.509218498324237,0.509653960252979,0.510088821396247,
0.510329322034527,0.510626775115649,0.511348787261653,0.512110048863779,
0.512283442870139,0.512470237026294,0.512470248702241,0.512946059522407,
0.513041330770913,0.513639081561961,0.514134415348567,0.514204547981925,
0.51423683235301,0.514671061881375,0.514803582855506,0.514928213484362,
0.514928218967118,0.515334525052906,0.515454273862953,0.515988239961532,
0.516193434372497,0.516724661608416,0.517119848376792,0.517250490128293,
0.517386178266484,0.517386203705458,0.517793168800916,0.517910498018892,
0.518326825457484,0.518393745780107,0.518856558800808,0.518915054636807,
0.519324323912781,0.519433138548259,0.519795436072675,0.519844143048606,
0.519844149609364,0.520250525584912,0.520360005731246,0.520592238370696,
0.521050486855063,0.521111593796236,0.521543438514737,0.521632517341446,
0.522032817715619,0.522146085214015,0.522302107830728,0.522302123690607,
0.522667271225169,0.522791471835816,0.523271974962783,0.523374754316014,
0.52391494096234,0.523965718788713,0.524427475731704,0.524552209759413,
0.524760040597086,0.52476007261285,0.524988288844166,0.525632082109919,
0.526276088239782,0.526848232541706,0.526886097506026,0.527185208253064,
0.527218037394971,0.527218055331716,0.52769028709017,0.527882394720423,
0.528427395915005,0.528568702738237,0.529128361973499,0.529247631186266,
0.52938358734141,0.529642816166946,0.529675973102647,0.529676002177093,
0.530155413416485,0.530290493372624,0.53029054627694,0.530740029860379,
0.530904984568154,0.530905035074824,0.531241074620977,0.531519451599375,
0.531519475763684,0.531582823133813,0.531896566102861,0.531959892648512,
0.532133966959215,0.532134064211177,0.532511118973597,0.532687508961153,
0.533124008239765,0.533251893760347,0.533664164121437,0.533781533154975),
 .UNSPECIFIED.);
#794=B_SPLINE_CURVE_WITH_KNOTS('',3,(#53327,#53328,#53329,#53330,#53331,
#53332,#53333,#53334,#53335,#53336,#53337,#53338,#53339,#53340,#53341,#53342,
#53343,#53344,#53345,#53346,#53347,#53348,#53349,#53350,#53351,#53352,#53353,
#53354,#53355,#53356,#53357,#53358,#53359,#53360,#53361,#53362,#53363,#53364,
#53365,#53366,#53367),.UNSPECIFIED.,.F.,.F.,(4,1,1,1,1,1,1,1,1,1,1,1,1,
1,1,1,1,1,1,1,1,1,1,1,1,1,1,1,1,1,1,1,1,1,1,1,1,1,4),(0.476423916058673,
0.478623759221241,0.480823602383808,0.483023445546375,0.485223288708942,
0.487423131871509,0.489622975034076,0.491822818196643,0.49402266135921,
0.495978077503714,0.497933493648219,0.499888909792723,0.502822034009479,
0.505755158226235,0.508688282442991,0.511621406659747,0.514554530876503,
0.51748765509326,0.518220936147449,0.518954217201638,0.519687498255827,
0.520420779310016,0.522620622472583,0.52482046563515,0.527020308797717,
0.529220151960284,0.531419995122852,0.533619838285419,0.535819681447986,
0.538019524610553,0.54021936777312,0.542419210935687,0.544619054098254,
0.546818897260821,0.549018740423388,0.551218583585956,0.554151707802712,
0.55561826991109,0.556713614780248),.UNSPECIFIED.);
#795=B_SPLINE_CURVE_WITH_KNOTS('',3,(#53596,#53597,#53598,#53599,#53600,
#53601,#53602,#53603,#53604,#53605,#53606,#53607,#53608,#53609,#53610,#53611,
#53612,#53613,#53614,#53615,#53616,#53617,#53618,#53619,#53620,#53621,#53622,
#53623,#53624,#53625,#53626,#53627,#53628,#53629,#53630,#53631,#53632,#53633,
#53634,#53635,#53636,#53637,#53638,#53639,#53640,#53641,#53642,#53643,#53644,
#53645,#53646,#53647,#53648,#53649,#53650,#53651,#53652,#53653,#53654,#53655,
#53656,#53657,#53658,#53659,#53660,#53661,#53662,#53663,#53664,#53665,#53666,
#53667,#53668,#53669,#53670,#53671,#53672,#53673,#53674,#53675,#53676,#53677,
#53678,#53679,#53680,#53681,#53682,#53683,#53684,#53685,#53686,#53687,#53688,
#53689,#53690,#53691,#53692,#53693,#53694,#53695,#53696,#53697,#53698,#53699,
#53700,#53701,#53702,#53703,#53704,#53705,#53706,#53707,#53708,#53709,#53710,
#53711,#53712,#53713,#53714,#53715,#53716,#53717,#53718,#53719,#53720,#53721,
#53722,#53723,#53724,#53725,#53726,#53727,#53728,#53729,#53730,#53731,#53732,
#53733,#53734,#53735,#53736,#53737,#53738,#53739,#53740,#53741,#53742,#53743,
#53744,#53745,#53746,#53747,#53748,#53749,#53750,#53751,#53752,#53753,#53754,
#53755,#53756,#53757,#53758,#53759,#53760,#53761,#53762,#53763,#53764,#53765,
#53766,#53767,#53768,#53769,#53770,#53771,#53772,#53773,#53774,#53775,#53776,
#53777,#53778,#53779,#53780,#53781,#53782,#53783,#53784,#53785,#53786,#53787,
#53788,#53789,#53790,#53791,#53792,#53793,#53794,#53795,#53796,#53797,#53798,
#53799,#53800,#53801,#53802,#53803,#53804,#53805,#53806,#53807,#53808,#53809,
#53810,#53811,#53812,#53813,#53814,#53815,#53816,#53817,#53818,#53819,#53820,
#53821,#53822,#53823,#53824,#53825,#53826,#53827,#53828,#53829,#53830,#53831,
#53832,#53833,#53834,#53835,#53836,#53837,#53838,#53839,#53840,#53841,#53842,
#53843,#53844,#53845,#53846,#53847,#53848,#53849,#53850,#53851,#53852,#53853,
#53854,#53855,#53856,#53857,#53858,#53859,#53860,#53861,#53862,#53863,#53864,
#53865,#53866,#53867,#53868,#53869,#53870,#53871,#53872,#53873,#53874,#53875,
#53876,#53877,#53878,#53879,#53880,#53881,#53882,#53883,#53884,#53885,#53886,
#53887,#53888,#53889,#53890,#53891,#53892,#53893,#53894,#53895,#53896,#53897,
#53898,#53899,#53900,#53901,#53902,#53903,#53904,#53905,#53906,#53907,#53908,
#53909,#53910,#53911,#53912,#53913,#53914,#53915,#53916,#53917,#53918,#53919,
#53920,#53921,#53922,#53923,#53924,#53925,#53926,#53927,#53928,#53929,#53930,
#53931,#53932,#53933,#53934,#53935,#53936,#53937,#53938,#53939,#53940,#53941,
#53942,#53943,#53944,#53945,#53946,#53947,#53948,#53949,#53950,#53951,#53952,
#53953,#53954,#53955,#53956,#53957,#53958,#53959,#53960,#53961,#53962,#53963,
#53964,#53965,#53966,#53967,#53968,#53969,#53970,#53971,#53972,#53973,#53974,
#53975,#53976,#53977,#53978,#53979,#53980,#53981,#53982,#53983,#53984,#53985,
#53986,#53987,#53988,#53989,#53990,#53991,#53992,#53993,#53994,#53995,#53996,
#53997,#53998,#53999,#54000,#54001,#54002,#54003,#54004,#54005,#54006,#54007,
#54008,#54009,#54010,#54011,#54012,#54013,#54014,#54015,#54016,#54017,#54018,
#54019,#54020,#54021,#54022,#54023,#54024,#54025,#54026,#54027,#54028,#54029,
#54030,#54031,#54032,#54033,#54034,#54035,#54036,#54037,#54038,#54039,#54040,
#54041,#54042,#54043,#54044,#54045,#54046,#54047,#54048,#54049,#54050,#54051,
#54052,#54053,#54054,#54055,#54056,#54057,#54058,#54059,#54060,#54061,#54062,
#54063,#54064,#54065,#54066,#54067,#54068,#54069,#54070,#54071,#54072,#54073,
#54074,#54075,#54076,#54077,#54078,#54079,#54080,#54081,#54082,#54083,#54084,
#54085,#54086,#54087,#54088,#54089,#54090,#54091,#54092,#54093,#54094,#54095,
#54096,#54097,#54098,#54099,#54100,#54101,#54102,#54103,#54104,#54105,#54106,
#54107,#54108,#54109,#54110,#54111,#54112,#54113,#54114,#54115,#54116,#54117,
#54118,#54119,#54120,#54121,#54122,#54123,#54124,#54125,#54126,#54127,#54128,
#54129,#54130,#54131,#54132,#54133,#54134,#54135,#54136,#54137,#54138,#54139,
#54140,#54141,#54142,#54143,#54144,#54145,#54146,#54147,#54148,#54149,#54150,
#54151,#54152,#54153,#54154,#54155,#54156,#54157,#54158,#54159,#54160,#54161,
#54162,#54163,#54164,#54165,#54166,#54167,#54168,#54169,#54170,#54171,#54172,
#54173,#54174,#54175,#54176,#54177,#54178,#54179,#54180,#54181,#54182,#54183,
#54184,#54185,#54186,#54187,#54188,#54189,#54190,#54191,#54192,#54193,#54194,
#54195,#54196,#54197,#54198,#54199,#54200,#54201,#54202,#54203,#54204,#54205,
#54206,#54207,#54208,#54209,#54210,#54211,#54212,#54213,#54214,#54215,#54216,
#54217,#54218,#54219,#54220,#54221,#54222,#54223,#54224,#54225,#54226,#54227,
#54228,#54229,#54230,#54231,#54232,#54233,#54234,#54235,#54236,#54237,#54238,
#54239,#54240,#54241,#54242,#54243,#54244,#54245,#54246,#54247,#54248,#54249,
#54250,#54251,#54252,#54253,#54254,#54255,#54256,#54257,#54258,#54259,#54260,
#54261,#54262,#54263,#54264,#54265,#54266,#54267,#54268,#54269,#54270,#54271,
#54272,#54273,#54274,#54275,#54276,#54277,#54278,#54279,#54280,#54281,#54282,
#54283,#54284,#54285,#54286,#54287,#54288,#54289,#54290,#54291,#54292,#54293,
#54294,#54295,#54296,#54297,#54298,#54299,#54300,#54301,#54302,#54303,#54304,
#54305,#54306,#54307,#54308,#54309,#54310,#54311,#54312,#54313,#54314,#54315,
#54316,#54317,#54318,#54319,#54320,#54321,#54322,#54323,#54324,#54325,#54326,
#54327,#54328,#54329,#54330,#54331,#54332,#54333,#54334,#54335,#54336,#54337,
#54338,#54339,#54340,#54341,#54342,#54343,#54344,#54345,#54346,#54347,#54348,
#54349,#54350,#54351,#54352,#54353,#54354,#54355,#54356,#54357,#54358,#54359,
#54360,#54361,#54362,#54363,#54364,#54365,#54366,#54367,#54368,#54369,#54370,
#54371,#54372,#54373,#54374,#54375,#54376,#54377,#54378,#54379,#54380,#54381,
#54382,#54383,#54384,#54385,#54386,#54387,#54388,#54389,#54390,#54391,#54392,
#54393,#54394,#54395,#54396,#54397,#54398,#54399,#54400,#54401,#54402,#54403,
#54404,#54405,#54406,#54407,#54408,#54409,#54410,#54411,#54412,#54413,#54414,
#54415,#54416,#54417,#54418,#54419,#54420,#54421,#54422,#54423,#54424,#54425,
#54426,#54427,#54428,#54429,#54430,#54431,#54432,#54433,#54434,#54435,#54436,
#54437,#54438,#54439,#54440,#54441,#54442,#54443,#54444,#54445,#54446,#54447,
#54448,#54449,#54450,#54451,#54452,#54453,#54454,#54455,#54456,#54457,#54458,
#54459,#54460,#54461,#54462,#54463,#54464,#54465,#54466,#54467,#54468,#54469,
#54470,#54471,#54472,#54473,#54474,#54475,#54476,#54477,#54478,#54479,#54480,
#54481,#54482,#54483,#54484,#54485,#54486,#54487,#54488,#54489,#54490,#54491,
#54492,#54493,#54494,#54495,#54496,#54497,#54498,#54499,#54500,#54501,#54502,
#54503,#54504,#54505,#54506,#54507,#54508,#54509,#54510,#54511,#54512,#54513,
#54514,#54515,#54516,#54517,#54518,#54519,#54520),.UNSPECIFIED.,.F.,.F.,
(4,3,3,3,3,3,3,3,3,3,3,3,3,3,3,3,3,3,3,3,3,3,3,3,3,3,3,3,3,3,3,3,3,3,3,
3,3,3,3,3,3,3,3,3,3,3,3,3,3,3,3,3,3,3,3,3,3,3,3,3,3,3,3,3,3,3,3,3,3,3,3,
3,3,3,3,3,3,3,3,3,3,3,3,3,3,3,3,3,3,3,3,3,3,3,3,3,3,3,3,3,3,3,3,3,3,3,3,
3,3,3,3,3,3,3,3,3,3,3,3,3,3,3,3,3,3,3,3,3,3,3,3,3,3,3,3,3,3,3,3,3,3,3,3,
3,3,3,3,3,3,3,3,3,3,3,3,3,3,3,3,3,3,3,3,3,3,3,3,3,3,3,3,3,3,3,3,3,3,3,3,
3,3,3,3,3,3,3,3,3,3,3,3,3,3,3,3,3,3,3,3,3,3,3,3,3,3,3,3,3,3,3,3,3,3,3,3,
3,3,3,3,3,3,3,3,3,3,3,3,3,3,3,3,3,3,3,3,3,3,3,3,3,3,3,3,3,3,3,3,3,3,3,3,
3,3,3,3,3,3,3,3,3,3,3,3,3,3,3,3,3,3,3,3,3,3,3,3,3,3,3,3,3,3,3,3,3,3,3,3,
3,3,3,3,3,3,3,3,3,3,3,3,3,3,3,3,3,3,3,3,3,4),(0.621846856583102,0.621892368004092,
0.622217754402355,0.622512398940775,0.622842115954442,0.622991576945145,
0.623260935267364,0.62352959867094,0.623614317432359,0.623690005388955,
0.623690199736931,0.624239382984407,0.624823524763165,0.625380980181381,
0.625533666494912,0.625533673395834,0.62581659080554,0.625922630075138,
0.62632966176229,0.626661915347805,0.627058444237377,0.627377147054738,
0.627377166815579,0.627388799295699,0.627853878881753,0.628137038123222,
0.628947485830711,0.629220598439111,0.629220620713642,0.629519077136893,
0.629586450804523,0.629979828156307,0.630244781179595,0.630673671783401,
0.630874607656459,0.631063927555557,0.631064094372546,0.631404070692801,
0.631577505275728,0.631785531280198,0.632111327850892,0.632298280612031,
0.632616998065837,0.632720056214535,0.632879518135696,0.6329072533034,0.63297441474824,
0.633398286175892,0.633523264465984,0.633810420114705,0.633985383022046,
0.63435647066126,0.634535019501422,0.634750641816437,0.635171345412579,
0.635612887009179,0.636118305501101,0.636353650182501,0.63652852424096,
0.636594267207711,0.636656907174331,0.636947027746356,0.637161234610997,
0.637490113291513,0.637652203413422,0.637992574863838,0.638162278120342,
0.638523409865301,0.63867876879381,0.639029560275845,0.639051974756686,
0.639052480227795,0.639411066819603,0.639513905773405,0.639772948973219,
0.639979341092053,0.640326035026194,0.640437249538887,0.640580189492334,
0.640893742032511,0.641045334456777,0.641350157683134,0.641510445106334,
0.641510520468996,0.641855447338863,0.642145741044356,0.642504786958309,
0.642781036982378,0.643143260455569,0.643429755604233,0.643787947840224,
0.643968337255306,0.643968409984872,0.644311970313094,0.644519894040162,
0.64487515938326,0.644979314629088,0.645364126006925,0.645532913269996,
0.645898207943654,0.646077762835349,0.646426104551011,0.646426374863411,
0.646903296177914,0.646968824192859,0.647178376789036,0.647616325850096,
0.647718937150597,0.648155393765759,0.648266193553022,0.648668146628746,
0.64880222161661,0.648884320276792,0.648884339741949,0.649226800377354,
0.64937595891545,0.64989765197277,0.650030480626183,0.650564348293318,0.650690367012657,
0.651160839486392,0.651342199845661,0.651342304620487,0.651574257682463,
0.652178608548435,0.652307398772069,0.652804778862935,0.653185506970598,
0.653433745519239,0.653733088132842,0.653976851830688,0.654311059815641,
0.654683356014655,0.65495462603492,0.655028760084688,0.655125927070742,
0.655552992353464,0.655591184342934,0.655921086710341,0.65597513120871,
0.656435130214724,0.656535762886226,0.656974326652741,0.657099447125672,
0.657333334797077,0.657333594011925,0.657849778299409,0.65788352032917,
0.658174361190189,0.658716199256103,0.658716231150652,0.659235096782956,
0.659367077841226,0.659639218198966,0.660216832023549,0.660282720594914,
0.660372165593032,0.660535409556554,0.66055973216036,0.6606773284617,0.661105887847589,
0.661827729130058,0.661967148644685,0.66240314657391,0.662403243536604,
0.662570692333655,0.663031924300911,0.663324880441152,0.663324883403362,
0.663780122147482,0.664035884325968,0.664768810217626,0.665452699119168,
0.665501736109285,0.665977218153675,0.666089925560195,0.666090093891718,
0.666405252042465,0.666715525057786,0.666969145781492,0.667392274044864,
0.667451356666056,0.667933323118611,0.667933567550621,0.668399012595211,
0.668850026105056,0.66931353365729,0.669753436268086,0.669777041209525,
0.669777063757701,0.66990175999802,0.670336541074922,0.670363468260186,
0.670823820213632,0.671279676695711,0.671620351658753,0.671620514868429,
0.672012982164485,0.672096242248359,0.672568466796311,0.672832807138605,
0.673307273781809,0.673463988527333,0.673463993254202,0.673949266280578,
0.674436321409013,0.674846535338015,0.674846593771511,0.67516463195361,
0.675307462186237,0.675307473834191,0.675765484218751,0.676238176537912,
0.676713164461141,0.677072734813525,0.677150860525229,0.677150935845141,
0.677541464645956,0.677593947489397,0.678037275633189,0.678479948931442,
0.678696094435218,0.678994409504044,0.678994424995288,0.679636251815923,
0.680304809352545,0.680650824154123,0.680837873863623,0.680837883162948,
0.681313451598143,0.681396506836904,0.681963063308275,0.682464379490378,
0.682518500564243,0.682604390363344,0.68303635841607,0.68316020954716,0.683295848041487,
0.683295854986793,0.683697951637246,0.683821949446226,0.684356147216294,
0.684561096692745,0.685028766729934,0.685092464044742,0.685475155241169,
0.685618632271069,0.685753812920025,0.685753835579768,0.686138943891943,
0.686281011537786,0.686761323597106,0.687245578329172,0.687285493897112,
0.687751354770776,0.687806434760149,0.688169131423624,0.688211777798563,
0.688571197333438,0.688730739103929,0.689113056311331,0.689481928590921,
0.68992985984292,0.690005858927733,0.690403744007667,0.690522537141612,
0.690669742677102,0.690669765081458,0.691010156824626,0.691158411304279,
0.691656278311949,0.691725835072625,0.692243766277744,0.692300043756321,
0.69275115179365,0.692864587804725,0.69312770755564,0.693355096033911,0.694008810835572,
0.694146584170164,0.694831159081235,0.694926491298771,0.695496197861561,
0.695553192932812,0.695585672434178,0.695585728026548,0.696093025979352,
0.696164280447754,0.696749200143603,0.697319347282953,0.697751415553726,
0.698043637312717,0.698043809025599,0.698443081416774,0.698575319251526,
0.699021391544107,0.699114416684524,0.699596756504331,0.69965572425361,
0.699952328223295,0.70026812359144,0.700501602191255,0.700501819333784,
0.700977661104677,0.701462623953163,0.701730584630524,0.701730673094993,
0.702107832683567,0.702150215830222),.UNSPECIFIED.);
#796=B_SPLINE_CURVE_WITH_KNOTS('',3,(#54521,#54522,#54523,#54524,#54525,
#54526,#54527,#54528,#54529,#54530,#54531,#54532,#54533,#54534,#54535,#54536,
#54537,#54538,#54539,#54540,#54541,#54542,#54543,#54544,#54545,#54546,#54547,
#54548,#54549,#54550,#54551,#54552,#54553,#54554,#54555,#54556,#54557,#54558,
#54559,#54560,#54561,#54562,#54563,#54564,#54565,#54566,#54567,#54568,#54569,
#54570,#54571,#54572,#54573,#54574,#54575,#54576,#54577,#54578,#54579,#54580,
#54581,#54582,#54583,#54584,#54585,#54586,#54587,#54588,#54589,#54590,#54591,
#54592,#54593,#54594,#54595,#54596,#54597,#54598,#54599,#54600,#54601,#54602,
#54603,#54604,#54605,#54606,#54607,#54608,#54609,#54610,#54611,#54612,#54613,
#54614,#54615,#54616,#54617,#54618,#54619,#54620,#54621,#54622,#54623,#54624,
#54625,#54626,#54627,#54628,#54629,#54630,#54631,#54632,#54633,#54634,#54635,
#54636,#54637,#54638,#54639,#54640,#54641,#54642,#54643,#54644,#54645,#54646,
#54647,#54648,#54649,#54650,#54651,#54652,#54653,#54654,#54655,#54656,#54657,
#54658,#54659,#54660,#54661,#54662,#54663,#54664,#54665,#54666,#54667,#54668,
#54669,#54670,#54671,#54672,#54673,#54674,#54675,#54676,#54677,#54678,#54679,
#54680,#54681,#54682,#54683,#54684,#54685,#54686,#54687,#54688,#54689,#54690,
#54691,#54692,#54693,#54694,#54695,#54696,#54697,#54698,#54699,#54700,#54701,
#54702,#54703,#54704,#54705,#54706,#54707,#54708,#54709,#54710,#54711,#54712,
#54713,#54714,#54715,#54716,#54717,#54718,#54719,#54720,#54721,#54722,#54723,
#54724,#54725,#54726,#54727,#54728,#54729,#54730,#54731,#54732,#54733,#54734,
#54735,#54736,#54737,#54738,#54739,#54740,#54741,#54742,#54743,#54744,#54745,
#54746,#54747,#54748,#54749,#54750,#54751,#54752,#54753,#54754,#54755,#54756,
#54757,#54758,#54759,#54760,#54761,#54762,#54763,#54764,#54765,#54766,#54767,
#54768,#54769,#54770,#54771,#54772,#54773,#54774,#54775,#54776,#54777,#54778,
#54779,#54780,#54781,#54782,#54783,#54784,#54785,#54786,#54787,#54788,#54789,
#54790,#54791,#54792,#54793,#54794,#54795,#54796,#54797,#54798,#54799,#54800,
#54801,#54802,#54803,#54804,#54805,#54806,#54807,#54808,#54809,#54810,#54811,
#54812,#54813,#54814,#54815,#54816,#54817,#54818,#54819,#54820,#54821,#54822,
#54823,#54824,#54825,#54826,#54827,#54828,#54829,#54830,#54831,#54832,#54833,
#54834,#54835,#54836,#54837,#54838,#54839,#54840,#54841,#54842,#54843,#54844,
#54845,#54846,#54847,#54848,#54849,#54850,#54851,#54852,#54853,#54854,#54855,
#54856,#54857,#54858,#54859,#54860,#54861,#54862,#54863,#54864,#54865,#54866,
#54867,#54868,#54869,#54870,#54871,#54872,#54873,#54874,#54875,#54876,#54877,
#54878,#54879,#54880,#54881,#54882,#54883,#54884,#54885,#54886,#54887,#54888,
#54889,#54890,#54891,#54892,#54893,#54894,#54895,#54896,#54897,#54898,#54899,
#54900,#54901,#54902,#54903,#54904,#54905,#54906,#54907,#54908,#54909,#54910,
#54911,#54912,#54913,#54914,#54915,#54916,#54917,#54918,#54919,#54920,#54921,
#54922,#54923,#54924,#54925,#54926,#54927,#54928,#54929,#54930,#54931,#54932,
#54933,#54934,#54935,#54936,#54937,#54938,#54939,#54940,#54941,#54942,#54943,
#54944,#54945,#54946,#54947,#54948,#54949,#54950,#54951,#54952,#54953,#54954,
#54955,#54956,#54957,#54958,#54959,#54960,#54961,#54962,#54963,#54964,#54965,
#54966,#54967,#54968,#54969,#54970,#54971,#54972,#54973,#54974,#54975,#54976,
#54977,#54978,#54979,#54980,#54981,#54982,#54983,#54984,#54985,#54986,#54987,
#54988,#54989,#54990,#54991,#54992,#54993,#54994,#54995,#54996,#54997,#54998,
#54999,#55000,#55001,#55002,#55003,#55004,#55005,#55006,#55007,#55008,#55009,
#55010,#55011,#55012,#55013,#55014,#55015,#55016,#55017,#55018,#55019,#55020,
#55021,#55022,#55023,#55024,#55025,#55026,#55027,#55028,#55029,#55030,#55031,
#55032,#55033,#55034,#55035,#55036,#55037,#55038,#55039,#55040,#55041,#55042,
#55043,#55044,#55045,#55046,#55047,#55048,#55049,#55050,#55051,#55052,#55053,
#55054,#55055,#55056,#55057,#55058,#55059,#55060,#55061,#55062,#55063,#55064,
#55065,#55066,#55067,#55068,#55069,#55070,#55071,#55072,#55073,#55074,#55075,
#55076,#55077,#55078,#55079,#55080,#55081,#55082,#55083,#55084,#55085,#55086,
#55087,#55088,#55089,#55090,#55091,#55092,#55093,#55094,#55095,#55096,#55097,
#55098,#55099,#55100,#55101,#55102,#55103,#55104,#55105,#55106,#55107,#55108,
#55109,#55110,#55111,#55112,#55113,#55114,#55115,#55116,#55117,#55118,#55119,
#55120,#55121,#55122,#55123,#55124,#55125,#55126,#55127,#55128,#55129,#55130,
#55131,#55132,#55133,#55134,#55135,#55136,#55137,#55138,#55139,#55140,#55141,
#55142,#55143,#55144,#55145,#55146,#55147,#55148,#55149,#55150,#55151,#55152,
#55153,#55154,#55155,#55156,#55157,#55158,#55159,#55160,#55161,#55162,#55163,
#55164,#55165,#55166,#55167,#55168,#55169,#55170,#55171,#55172,#55173,#55174,
#55175,#55176,#55177,#55178,#55179,#55180,#55181,#55182,#55183,#55184,#55185,
#55186,#55187,#55188,#55189,#55190,#55191,#55192,#55193,#55194,#55195,#55196,
#55197,#55198,#55199,#55200,#55201,#55202,#55203,#55204,#55205,#55206,#55207,
#55208,#55209,#55210,#55211,#55212,#55213,#55214,#55215,#55216,#55217,#55218,
#55219,#55220,#55221,#55222,#55223,#55224,#55225,#55226,#55227,#55228,#55229,
#55230,#55231,#55232,#55233,#55234,#55235,#55236,#55237,#55238,#55239,#55240,
#55241,#55242,#55243,#55244,#55245,#55246,#55247,#55248,#55249,#55250,#55251,
#55252,#55253,#55254,#55255,#55256,#55257,#55258,#55259,#55260,#55261,#55262,
#55263,#55264,#55265,#55266,#55267,#55268,#55269,#55270,#55271,#55272,#55273,
#55274,#55275,#55276,#55277,#55278,#55279,#55280,#55281,#55282,#55283,#55284,
#55285,#55286,#55287,#55288,#55289,#55290,#55291,#55292,#55293,#55294,#55295,
#55296,#55297,#55298,#55299,#55300,#55301,#55302,#55303,#55304,#55305,#55306,
#55307,#55308,#55309,#55310,#55311,#55312,#55313,#55314,#55315,#55316,#55317,
#55318,#55319,#55320,#55321,#55322,#55323,#55324,#55325,#55326,#55327,#55328,
#55329,#55330,#55331,#55332,#55333,#55334,#55335,#55336,#55337,#55338,#55339,
#55340,#55341,#55342,#55343,#55344,#55345,#55346,#55347,#55348,#55349,#55350,
#55351,#55352,#55353,#55354,#55355,#55356,#55357,#55358,#55359,#55360,#55361,
#55362,#55363,#55364,#55365,#55366,#55367,#55368,#55369,#55370,#55371,#55372,
#55373,#55374,#55375,#55376,#55377,#55378,#55379,#55380,#55381,#55382,#55383,
#55384,#55385,#55386,#55387,#55388,#55389,#55390,#55391,#55392,#55393,#55394,
#55395,#55396,#55397,#55398,#55399,#55400,#55401,#55402,#55403,#55404,#55405,
#55406,#55407,#55408,#55409,#55410,#55411,#55412,#55413,#55414,#55415,#55416,
#55417,#55418),.UNSPECIFIED.,.F.,.F.,(4,3,3,3,3,3,3,3,3,3,3,3,3,3,3,3,3,
3,3,3,3,3,3,3,3,3,3,3,3,3,3,3,3,3,3,3,3,3,3,3,3,3,3,3,3,3,3,3,3,3,3,3,3,
3,3,3,3,3,3,3,3,3,3,3,3,3,3,3,3,3,3,3,3,3,3,3,3,3,3,3,3,3,3,3,3,3,3,3,3,
3,3,3,3,3,3,3,3,3,3,3,3,3,3,3,3,3,3,3,3,3,3,3,3,3,3,3,3,3,3,3,3,3,3,3,3,
3,3,3,3,3,3,3,3,3,3,3,3,3,3,3,3,3,3,3,3,3,3,3,3,3,3,3,3,3,3,3,3,3,3,3,3,
3,3,3,3,3,3,3,3,3,3,3,3,3,3,3,3,3,3,3,3,3,3,3,3,3,3,3,3,3,3,3,3,3,3,3,3,
3,3,3,3,3,3,3,3,3,3,3,3,3,3,3,3,3,3,3,3,3,3,3,3,3,3,3,3,3,3,3,3,3,3,3,3,
3,3,3,3,3,3,3,3,3,3,3,3,3,3,3,3,3,3,3,3,3,3,3,3,3,3,3,3,3,3,3,3,3,3,3,3,
3,3,3,3,3,3,3,3,3,3,3,3,3,3,3,3,3,3,3,3,3,3,3,3,3,3,3,3,3,3,4),(0.644791544335362,
0.645153526214939,0.645310959618977,0.645676474496103,0.645833977154658,
0.646251301875498,0.646353924248001,0.646424939099399,0.646751072183065,
0.646950625627699,0.64699138736001,0.646991525407673,0.64741101203503,0.647643683290812,
0.648195346727212,0.648314485471916,0.648760289982565,0.64888432497532,
0.649191230384658,0.64919137322513,0.649743701241436,0.650140118372147,
0.650719692365367,0.651214822882452,0.651343080325357,0.651391073409306,
0.651391118944592,0.651951507715739,0.652100355662719,0.652712754250196,
0.652802674436081,0.653186195416618,0.65350741365838,0.653590916433954,
0.653590949962743,0.653951215231746,0.654105156926794,0.654482857907031,
0.654630094944148,0.655028794384741,0.655315168920487,0.655559771981192,
0.655790759458603,0.655790903513987,0.656185724410983,0.65638239282991,
0.656821086322865,0.65697575108274,0.657332254560426,0.657734962677141,
0.657924154301468,0.657990683752338,0.658460186042501,0.658709155264617,
0.658929817760636,0.6593803011134,0.659694947721945,0.660021259979664,0.66019060041926,
0.660511836060965,0.660952534313357,0.661343081661848,0.661695233509873,
0.66204282942369,0.662216627380598,0.662328533219871,0.662390425337507,
0.66240491166612,0.662761745796994,0.662955596401597,0.663264831817701,
0.663328505469564,0.663704741137132,0.663892542138641,0.664235780750512,
0.664467522099156,0.664785121524789,0.665033275081114,0.665323412565411,
0.665323504224367,0.665592315581149,0.665778427922754,0.666074241307012,
0.666091977245835,0.666470976691864,0.666543952896891,0.666789974581843,
0.666789995247387,0.667330927477148,0.667393714335977,0.667933178703534,
0.668256536598275,0.668256544848671,0.668605057755227,0.66877470553658,
0.669134150256417,0.66930821010701,0.669677339906848,0.669774720705461,
0.670125227874921,0.670310269821686,0.670651527670531,0.670830859015959,
0.67118966063114,0.671189662891252,0.671538735284599,0.671618030118071,
0.67208399631781,0.672135733711233,0.672661552360578,0.673044160487637,
0.673179325034197,0.673525613633103,0.673848078572894,0.674076140309273,
0.674122729337065,0.67420257814757,0.674559244662587,0.67486862550672,0.675257295657817,
0.675637894901448,0.675983426972843,0.676427553621864,0.676741731944786,
0.676911294803007,0.677025830947751,0.677055910267708,0.677151777331771,
0.677655659551064,0.677713913776227,0.67816429033793,0.678292630192222,
0.678763137657689,0.678874664674428,0.678993708944106,0.679352446613448,
0.679572038930489,0.67989743364412,0.679989025127146,0.679989032729732,
0.680417499639778,0.680529121847719,0.680837199560911,0.681190702812042,
0.681376485586431,0.681832054604986,0.681918146094485,0.682188840285563,
0.68218887575438,0.682592647713095,0.682741217853742,0.683080469862056,
0.683293559953105,0.68363245094592,0.683841139366067,0.684230019465082,
0.684388688142652,0.684388718779029,0.68477543417128,0.684901445944761,
0.685237165836678,0.685419525169911,0.685752152648389,0.686135017102178,
0.686270873035483,0.686588561803677,0.686588563961573,0.68701213394025,
0.687208852037015,0.687645656957109,0.687832869652567,0.688210448282073,
0.688603622060726,0.688788404828325,0.688788445304447,0.689234599453257,
0.689460878957657,0.690014332354325,0.690145416254356,0.690621741553209,
0.690667884777815,0.690988247852973,0.690988419520626,0.691578457316744,
0.691668549527717,0.692360626115915,0.69293700643562,0.693026399397215,
0.693126468529246,0.693188090877621,0.693188210019722,0.693927397679595,
0.693979095312235,0.694775852319244,0.695387933902269,0.695388047386415,
0.695584235585489,0.696108116218357,0.696229480688965,0.696870106729419,
0.697364125699618,0.697498050280852,0.697587776926917,0.697587885484661,
0.698042602111492,0.698519485036437,0.698556272656978,0.699069574081016,
0.699500643103421,0.699574567853642,0.699787589992094,0.699787619951565,
0.700415085712946,0.700499821760193,0.701126162407082,0.701603988320641,
0.701728364262427,0.701987439035147,0.701987462976214,0.702537414953183,
0.7028430229729,0.703057651041027,0.703388907902351,0.703603444135822,0.70418727088409,
0.704361221807698,0.704789009876726,0.705188575134246,0.705488249077386,
0.705913030342945,0.706150150624875,0.706292385171816,0.706382421329585,
0.706387270906805,0.706710299363978,0.706972180134217,0.707375869617682,
0.707647452157423,0.707957694005688,0.70829012570918,0.708586938068078,
0.708659205690346,0.708990910364272,0.709365643469127,0.709644137700458,
0.709921252561858,0.710299578784898,0.710332334411613,0.710688552901087,
0.710786835074806,0.710787432953519,0.711123697531024,0.711299298463576,
0.711656326506015,0.711714602623934,0.71202822819272,0.712174659651686,
0.712694888330029,0.712986678099454,0.712986879391121,0.713441669408398,
0.71366310711077,0.714017902447798,0.714694833321608,0.715092726948194,
0.715186521124103,0.715186555121356,0.715694340947741,0.71586053451435,
0.716367122125722,0.716876743137236,0.717285120793596,0.717386364148751,
0.71738638419871,0.71770367156283,0.718370718748376,0.718997757402535,0.719548123644611,
0.719586207173399,0.719586275934013,0.71998749286588,0.720388799951697,
0.720788181016139,0.721052769189831,0.721052822585763,0.721391810704347,
0.721928057393333,0.722030765857978,0.722621495484741,0.72268180044997,
0.723118129548938,0.7232370927966,0.723599034779558,0.723879022187679,0.723985893222695,
0.723985955035569,0.724315949004016,0.724646856840013,0.724978232920593,
0.725079475029497),.UNSPECIFIED.);
#797=B_SPLINE_CURVE_WITH_KNOTS('',3,(#55651,#55652,#55653,#55654,#55655,
#55656,#55657,#55658,#55659,#55660,#55661,#55662,#55663,#55664,#55665,#55666,
#55667,#55668,#55669,#55670,#55671,#55672,#55673,#55674,#55675,#55676,#55677,
#55678,#55679,#55680,#55681,#55682,#55683,#55684,#55685,#55686,#55687,#55688,
#55689,#55690,#55691,#55692,#55693,#55694,#55695,#55696,#55697,#55698,#55699,
#55700,#55701,#55702,#55703,#55704,#55705,#55706,#55707,#55708,#55709,#55710,
#55711,#55712,#55713,#55714,#55715,#55716,#55717,#55718,#55719,#55720,#55721,
#55722,#55723,#55724,#55725,#55726,#55727,#55728,#55729,#55730,#55731,#55732,
#55733,#55734,#55735,#55736,#55737,#55738,#55739,#55740,#55741,#55742,#55743,
#55744,#55745,#55746,#55747,#55748,#55749,#55750,#55751,#55752,#55753,#55754,
#55755,#55756,#55757,#55758,#55759,#55760,#55761,#55762,#55763,#55764,#55765,
#55766,#55767,#55768,#55769,#55770,#55771,#55772,#55773,#55774,#55775,#55776,
#55777,#55778,#55779,#55780,#55781,#55782,#55783,#55784,#55785,#55786,#55787,
#55788,#55789,#55790,#55791,#55792,#55793,#55794,#55795,#55796,#55797,#55798,
#55799,#55800,#55801,#55802,#55803,#55804,#55805,#55806,#55807,#55808,#55809,
#55810,#55811,#55812,#55813,#55814,#55815,#55816,#55817,#55818,#55819,#55820,
#55821,#55822,#55823,#55824,#55825,#55826,#55827,#55828,#55829,#55830,#55831,
#55832,#55833,#55834,#55835,#55836,#55837,#55838,#55839,#55840,#55841,#55842,
#55843,#55844,#55845,#55846,#55847,#55848,#55849,#55850,#55851,#55852,#55853,
#55854,#55855,#55856,#55857,#55858,#55859,#55860,#55861,#55862,#55863,#55864,
#55865,#55866,#55867,#55868,#55869,#55870,#55871,#55872,#55873,#55874,#55875,
#55876,#55877,#55878,#55879,#55880,#55881,#55882,#55883,#55884,#55885,#55886,
#55887,#55888,#55889,#55890,#55891,#55892,#55893,#55894,#55895,#55896,#55897,
#55898,#55899,#55900,#55901,#55902,#55903,#55904,#55905,#55906,#55907,#55908,
#55909,#55910,#55911,#55912,#55913,#55914,#55915,#55916,#55917,#55918,#55919,
#55920,#55921,#55922,#55923,#55924,#55925,#55926,#55927,#55928,#55929,#55930,
#55931,#55932,#55933,#55934,#55935,#55936,#55937,#55938,#55939,#55940,#55941,
#55942,#55943,#55944,#55945,#55946,#55947,#55948,#55949,#55950,#55951,#55952,
#55953,#55954,#55955,#55956,#55957,#55958,#55959,#55960,#55961,#55962,#55963,
#55964,#55965,#55966,#55967,#55968,#55969,#55970,#55971,#55972,#55973,#55974,
#55975,#55976,#55977,#55978,#55979,#55980,#55981,#55982,#55983,#55984,#55985,
#55986,#55987,#55988,#55989,#55990,#55991,#55992,#55993,#55994,#55995,#55996,
#55997,#55998,#55999,#56000,#56001,#56002,#56003,#56004,#56005,#56006,#56007,
#56008,#56009,#56010,#56011,#56012,#56013,#56014,#56015,#56016,#56017,#56018,
#56019,#56020,#56021,#56022,#56023,#56024,#56025,#56026,#56027,#56028,#56029,
#56030,#56031,#56032,#56033,#56034,#56035,#56036,#56037,#56038,#56039,#56040,
#56041,#56042,#56043,#56044,#56045,#56046,#56047,#56048,#56049,#56050,#56051,
#56052,#56053,#56054,#56055,#56056,#56057,#56058,#56059,#56060,#56061,#56062,
#56063,#56064,#56065,#56066,#56067,#56068,#56069,#56070,#56071,#56072,#56073,
#56074,#56075,#56076,#56077,#56078,#56079,#56080,#56081,#56082,#56083,#56084,
#56085,#56086,#56087,#56088,#56089,#56090,#56091,#56092,#56093,#56094,#56095,
#56096,#56097,#56098,#56099,#56100,#56101,#56102,#56103,#56104,#56105,#56106,
#56107,#56108,#56109,#56110,#56111,#56112,#56113,#56114,#56115,#56116,#56117,
#56118,#56119,#56120,#56121,#56122,#56123,#56124,#56125,#56126,#56127,#56128,
#56129,#56130,#56131,#56132,#56133,#56134,#56135,#56136,#56137,#56138,#56139,
#56140,#56141,#56142,#56143,#56144,#56145,#56146,#56147,#56148,#56149,#56150,
#56151,#56152,#56153,#56154,#56155,#56156,#56157,#56158,#56159,#56160,#56161,
#56162,#56163,#56164,#56165,#56166,#56167,#56168,#56169,#56170,#56171,#56172,
#56173,#56174,#56175,#56176,#56177,#56178,#56179,#56180,#56181,#56182,#56183,
#56184,#56185,#56186,#56187,#56188,#56189,#56190,#56191,#56192,#56193,#56194,
#56195,#56196,#56197,#56198,#56199,#56200,#56201,#56202,#56203,#56204,#56205,
#56206,#56207,#56208,#56209,#56210,#56211,#56212,#56213,#56214,#56215,#56216,
#56217,#56218,#56219,#56220,#56221,#56222,#56223,#56224,#56225,#56226,#56227,
#56228,#56229,#56230,#56231,#56232,#56233),.UNSPECIFIED.,.F.,.F.,(4,3,3,
3,3,3,3,3,3,3,3,3,3,3,3,3,3,3,3,3,3,3,3,3,3,3,3,3,3,3,3,3,3,3,3,3,3,3,3,
3,3,3,3,3,3,3,3,3,3,3,3,3,3,3,3,3,3,3,3,3,3,3,3,3,3,3,3,3,3,3,3,3,3,3,3,
3,3,3,3,3,3,3,3,3,3,3,3,3,3,3,3,3,3,3,3,3,3,3,3,3,3,3,3,3,3,3,3,3,3,3,3,
3,3,3,3,3,3,3,3,3,3,3,3,3,3,3,3,3,3,3,3,3,3,3,3,3,3,3,3,3,3,3,3,3,3,3,3,
3,3,3,3,3,3,3,3,3,3,3,3,3,3,3,3,3,3,3,3,3,3,3,3,3,3,3,3,3,3,3,3,3,3,3,3,
3,3,3,3,3,3,3,3,3,3,3,4),(0.915748838693565,0.916067586719041,0.916618732140758,
0.917169877562474,0.917721481216459,0.918241275309113,0.918273084870444,
0.918757739489292,0.919246857269427,0.919746927616459,0.920247700587533,
0.920483825124084,0.920990364456346,0.921484789544461,0.9217667121008,0.922249664809996,
0.922698785915839,0.92318275926108,0.923671046736705,0.924149740011753,
0.924356372081894,0.924775684712307,0.925307267240614,0.925860796180226,
0.926019879675272,0.926576660565611,0.927130916852163,0.927678914489343,
0.927784657323815,0.928394696744112,0.929031497175013,0.929338792057307,
0.92979063906482,0.930168046555878,0.930997525017763,0.931796620805825,
0.931827442761244,0.932381920865375,0.932656371732784,0.933070393415616,
0.933484504567997,0.93380260254683,0.934313586850845,0.934917026397449,
0.935142074968692,0.935307088852584,0.93555558405891,0.935968790006292,
0.936418900111347,0.936811575158338,0.937527538981205,0.93827342969671,
0.938995279415561,0.939284250243221,0.939820547769846,0.940071295487471,
0.940322043205097,0.940823538640348,0.940948912499161,0.941074286357974,
0.9413250340756,0.941575781793225,0.941701155652038,0.941826529510851,0.942249264940764,
0.942495190091186,0.942603578551054,0.943095900896275,0.943580323596278,
0.943832511251856,0.944166841542024,0.944501171832191,0.944938638928722,
0.945169832412526,0.945538045761981,0.945838492992861,0.945921380498607,
0.946297882566809,0.946507153573196,0.946950286941434,0.94739738083765,
0.947844474733866,0.948324751514134,0.948804857448725,0.949234065154626,
0.949712200936782,0.949850456474872,0.950647440566719,0.951441288481875,
0.951856438215877,0.952410060135101,0.952962335487208,0.953508063872448,
0.953650084172403,0.953862419956882,0.954510225961816,0.955186614305362,
0.955863002648908,0.955868401697887,0.956564283223973,0.957261946421114,
0.957522607015327,0.957874383438892,0.958471899894767,0.959072403401592,
0.959183774960762,0.959781949211659,0.959880365179897,0.960281925199207,
0.960682630542461,0.960845791924747,0.9608833560504,0.961311031019981,0.961737255803494,
0.961886346920902,0.962308282220108,0.962507322521059,0.962889337791405,
0.963271501480925,0.963651777930102,0.963892328661908,0.96416714743821,
0.964728584203379,0.965299528905214,0.965822212371328,0.966383697312681,
0.966901301273415,0.967445154901957,0.967481492533015,0.968027964557667,
0.968308874491794,0.968722367006821,0.969136310989922,0.969677231781982,
0.969910273884923,0.970342754897255,0.970786543600009,0.971235578300656,
0.971682710908604,0.972126784752767,0.972454518470128,0.972919246496431,
0.973450678525925,0.974001282847571,0.974116846453059,0.974667737072339,
0.975220565268069,0.975773393463799,0.975928219107938,0.976507314070495,
0.977104755059656,0.977432705413692,0.977935838204517,0.978257070471356,
0.978765012877377,0.978937191719446,0.97959434532721,0.980205160388321,
0.9804416780252,0.980740989458624,0.98143807725267,0.981946164330954,0.982434467230622,
0.982922769293201,0.98322518755684,0.983450650636708,0.983992206813968,
0.984468374379881,0.984955136942461,0.98547473936798,0.985712352984715,
0.986234938879445,0.986459623248215,0.986990260954347,0.987532112492594,
0.987964109553969,0.988202177576321,0.9886837301815,0.989175358682956,0.989468595859723,
0.989973288090569,0.990473310403973,0.990693251075575,0.990973082165477,
0.991469851085119,0.991986421692916,0.992500190747837,0.992994577671546,
0.993177675872154,0.993680925517914,0.993982054776985,0.994478920023504,
0.99498840685027,0.99550066833255,0.995667097027233),.UNSPECIFIED.);
#798=B_SPLINE_CURVE_WITH_KNOTS('',3,(#56595,#56596,#56597,#56598,#56599,
#56600,#56601,#56602,#56603,#56604,#56605,#56606,#56607,#56608,#56609,#56610,
#56611,#56612,#56613,#56614,#56615,#56616,#56617,#56618,#56619,#56620,#56621,
#56622,#56623,#56624,#56625,#56626,#56627,#56628,#56629,#56630,#56631,#56632,
#56633,#56634,#56635,#56636,#56637,#56638,#56639,#56640,#56641,#56642,#56643,
#56644,#56645,#56646,#56647,#56648,#56649,#56650,#56651,#56652,#56653,#56654,
#56655,#56656,#56657,#56658,#56659,#56660,#56661,#56662,#56663,#56664,#56665,
#56666,#56667,#56668,#56669,#56670,#56671,#56672,#56673,#56674,#56675,#56676,
#56677,#56678,#56679,#56680,#56681,#56682,#56683,#56684,#56685,#56686,#56687,
#56688,#56689,#56690,#56691,#56692,#56693,#56694,#56695,#56696,#56697,#56698,
#56699,#56700,#56701,#56702,#56703,#56704,#56705,#56706,#56707,#56708,#56709,
#56710,#56711,#56712,#56713,#56714,#56715,#56716,#56717,#56718,#56719,#56720,
#56721,#56722,#56723,#56724,#56725,#56726,#56727,#56728,#56729,#56730,#56731,
#56732,#56733,#56734,#56735,#56736,#56737,#56738,#56739,#56740,#56741,#56742,
#56743,#56744,#56745,#56746,#56747,#56748,#56749,#56750,#56751,#56752,#56753,
#56754,#56755,#56756,#56757,#56758,#56759,#56760,#56761,#56762,#56763,#56764,
#56765,#56766,#56767,#56768,#56769,#56770,#56771,#56772,#56773,#56774,#56775,
#56776,#56777,#56778,#56779,#56780,#56781,#56782,#56783,#56784,#56785,#56786,
#56787,#56788,#56789,#56790,#56791,#56792,#56793,#56794,#56795,#56796,#56797,
#56798,#56799,#56800,#56801,#56802,#56803,#56804,#56805,#56806,#56807,#56808,
#56809,#56810,#56811,#56812,#56813,#56814,#56815,#56816,#56817,#56818,#56819,
#56820,#56821,#56822,#56823,#56824,#56825,#56826,#56827,#56828,#56829,#56830,
#56831,#56832,#56833,#56834,#56835,#56836,#56837,#56838,#56839,#56840,#56841,
#56842,#56843,#56844,#56845,#56846,#56847,#56848,#56849,#56850,#56851,#56852,
#56853,#56854,#56855,#56856,#56857,#56858,#56859,#56860,#56861,#56862,#56863,
#56864,#56865,#56866,#56867,#56868,#56869,#56870,#56871,#56872,#56873,#56874,
#56875,#56876,#56877,#56878,#56879,#56880,#56881,#56882,#56883,#56884,#56885,
#56886,#56887,#56888,#56889,#56890,#56891,#56892,#56893,#56894,#56895,#56896,
#56897,#56898,#56899,#56900,#56901,#56902,#56903,#56904,#56905,#56906,#56907,
#56908,#56909,#56910,#56911,#56912,#56913,#56914,#56915,#56916,#56917,#56918,
#56919,#56920,#56921,#56922,#56923,#56924,#56925,#56926,#56927,#56928,#56929,
#56930,#56931,#56932,#56933,#56934,#56935,#56936,#56937,#56938,#56939,#56940,
#56941,#56942,#56943,#56944,#56945,#56946,#56947,#56948,#56949,#56950,#56951,
#56952,#56953,#56954,#56955,#56956,#56957,#56958,#56959,#56960,#56961,#56962,
#56963,#56964,#56965,#56966,#56967,#56968,#56969,#56970,#56971,#56972,#56973,
#56974,#56975,#56976,#56977,#56978,#56979,#56980,#56981,#56982,#56983,#56984,
#56985,#56986,#56987,#56988,#56989,#56990,#56991,#56992,#56993,#56994,#56995,
#56996,#56997,#56998,#56999,#57000,#57001,#57002,#57003,#57004,#57005,#57006,
#57007,#57008,#57009,#57010,#57011,#57012,#57013,#57014,#57015,#57016,#57017,
#57018,#57019,#57020,#57021,#57022,#57023,#57024,#57025,#57026,#57027,#57028,
#57029,#57030,#57031,#57032,#57033,#57034,#57035,#57036,#57037,#57038,#57039,
#57040,#57041,#57042,#57043,#57044,#57045,#57046,#57047,#57048,#57049,#57050,
#57051,#57052,#57053,#57054,#57055,#57056,#57057,#57058,#57059,#57060,#57061,
#57062,#57063,#57064,#57065,#57066,#57067,#57068,#57069,#57070,#57071,#57072,
#57073,#57074,#57075,#57076,#57077,#57078,#57079,#57080,#57081,#57082,#57083,
#57084,#57085,#57086,#57087,#57088,#57089,#57090,#57091,#57092,#57093,#57094,
#57095,#57096,#57097,#57098,#57099,#57100,#57101,#57102,#57103,#57104,#57105,
#57106,#57107,#57108,#57109,#57110,#57111,#57112,#57113,#57114,#57115,#57116,
#57117,#57118,#57119,#57120,#57121,#57122,#57123,#57124,#57125,#57126,#57127,
#57128,#57129,#57130,#57131,#57132,#57133,#57134,#57135,#57136,#57137,#57138,
#57139,#57140,#57141,#57142,#57143,#57144),.UNSPECIFIED.,.F.,.F.,(4,3,3,
3,3,3,3,3,3,3,3,3,3,3,3,3,3,3,3,3,3,3,3,3,3,3,3,3,3,3,3,3,3,3,3,3,3,3,3,
3,3,3,3,3,3,3,3,3,3,3,3,3,3,3,3,3,3,3,3,3,3,3,3,3,3,3,3,3,3,3,3,3,3,3,3,
3,3,3,3,3,3,3,3,3,3,3,3,3,3,3,3,3,3,3,3,3,3,3,3,3,3,3,3,3,3,3,3,3,3,3,3,
3,3,3,3,3,3,3,3,3,3,3,3,3,3,3,3,3,3,3,3,3,3,3,3,3,3,3,3,3,3,3,3,3,3,3,3,
3,3,3,3,3,3,3,3,3,3,3,3,3,3,3,3,3,3,3,3,3,3,3,3,3,3,3,3,3,3,3,3,3,3,3,3,
4),(0.0739106570180644,0.0742505665322785,0.0749231593883048,0.0755866481880669,
0.0759087958897528,0.076109515853017,0.0766704676188221,0.0772427974835055,
0.0775672823813314,0.0781410133149838,0.0783083908329088,0.0789200737186309,
0.0792265158692337,0.0798668908410172,0.0804745670761699,0.0805072658128007,
0.0808859595499181,0.0814877117812548,0.0820930282493823,0.0825447199390884,
0.0827061407926925,0.0833087258292241,0.0839238796533188,0.0842038066950157,
0.0848203409180411,0.0849050157725843,0.0854899487551179,0.0858631843941102,
0.0864523004693559,0.087032068073914,0.0871038907524762,0.0875229639776386,
0.0882679936403748,0.0890439628033391,0.0891822488886336,0.089302765732368,
0.0898310045056427,0.0903636653995039,0.0908393319980337,0.0913718057085553,
0.0915016407122598,0.0920835465321469,0.0924996977112301,0.0930930176814939,
0.0936813910903183,0.0941575341655823,0.0944334740187823,0.0951651912138979,
0.0958167134838409,0.0958993906720435,0.0966323489986741,0.0973181599504825,
0.0973653073253047,0.0974755459779731,0.0980219245564783,0.0985838235379587,
0.0991325409926556,0.0997148408122413,0.100258221552417,0.100297140631827,
0.100792995183773,0.101308629054549,0.101830716554359,0.102345774153224,
0.102450652527534,0.102965706889615,0.10322897393835,0.103738172914004,
0.104113788359032,0.104627808420626,0.105146290123506,0.10565440664557,
0.105770524262713,0.106160807244872,0.106705901621213,0.107271149233365,
0.107430308244803,0.107997658854337,0.108559372191222,0.109092640551394,
0.109640205515494,0.110205338349633,0.110773045133129,0.111291515531286,
0.111806384546412,0.111850938235435,0.112365499248319,0.112877106880496,
0.113381077069814,0.113490390511178,0.114064065326149,0.114681693127011,
0.114893126254671,0.115510243216294,0.11568926549107,0.115722281841006,
0.116393734861723,0.117070158047736,0.117380439167713,0.117888140470962,
0.118499435575117,0.119039707104872,0.119649338716235,0.120087015450854,
0.12069921012744,0.121330234043752,0.121955732108456,0.122285890430745,
0.122358373459964,0.12300483067754,0.12365625651878,0.124017367865778,0.124484765410637,
0.125098996875331,0.125677401720794,0.12628924989947,0.126683640390529,
0.127260089345903,0.127337209863532,0.127914998541037,0.128442609316833,
0.128882515370421,0.12936438870894,0.12954913842743,0.130034891721818,0.130520457661336,
0.131003051321121,0.131081390350313,0.131618115585724,0.131761670629781,
0.132314371274939,0.132867071920098,0.133280265330205,0.13375140920545,
0.133973203597052,0.134449087317234,0.134925679495375,0.135400668751173,
0.135479140310096,0.135969345652594,0.136459550995091,0.136945358596306,
0.137428217493013,0.137678015289988,0.138189487685163,0.138701835983074,
0.13894804272558,0.139460242574507,0.13987689026988,0.140333710283354,0.140792571382241,
0.141247205717867,0.141435605416639,0.141894660642086,0.142075765249772,
0.142544562020476,0.143016314713469,0.14349170384893,0.143924407321535,
0.144274640229664,0.144869070757695,0.145455531262855,0.145740556882925,
0.146224374908676,0.146412980072117,0.146898415400794,0.147206473536186,
0.147638362202818,0.147939431862817,0.148393236367263,0.14884865756534,
0.148901346511435,0.14936212130732,0.149819542963643,0.150138306842709,
0.150607829238979,0.151087910716682,0.151392024260246,0.151867636287259,
0.15234404539651,0.15280700372131,0.153070140149231,0.153474908875717,0.153879677602202),
 .UNSPECIFIED.);
#799=B_SPLINE_CURVE_WITH_KNOTS('',3,(#57421,#57422,#57423,#57424,#57425,
#57426,#57427,#57428,#57429,#57430,#57431,#57432,#57433,#57434,#57435,#57436,
#57437,#57438,#57439,#57440,#57441,#57442,#57443,#57444,#57445,#57446,#57447,
#57448,#57449,#57450,#57451,#57452,#57453,#57454,#57455,#57456,#57457,#57458,
#57459,#57460,#57461,#57462,#57463,#57464,#57465,#57466,#57467,#57468,#57469,
#57470,#57471,#57472,#57473,#57474,#57475,#57476,#57477,#57478,#57479,#57480,
#57481,#57482,#57483,#57484,#57485,#57486,#57487,#57488,#57489,#57490,#57491,
#57492,#57493,#57494,#57495,#57496,#57497,#57498,#57499,#57500,#57501,#57502,
#57503,#57504,#57505,#57506,#57507,#57508,#57509,#57510,#57511,#57512,#57513,
#57514,#57515,#57516,#57517,#57518,#57519,#57520,#57521,#57522,#57523,#57524,
#57525,#57526,#57527,#57528,#57529,#57530,#57531,#57532,#57533,#57534,#57535,
#57536,#57537,#57538,#57539,#57540,#57541,#57542,#57543,#57544,#57545,#57546,
#57547,#57548,#57549,#57550,#57551,#57552,#57553,#57554,#57555,#57556,#57557,
#57558,#57559,#57560,#57561,#57562,#57563,#57564,#57565,#57566,#57567,#57568,
#57569,#57570,#57571,#57572,#57573,#57574,#57575,#57576,#57577,#57578,#57579,
#57580,#57581,#57582,#57583,#57584,#57585,#57586,#57587,#57588,#57589,#57590,
#57591,#57592,#57593,#57594,#57595,#57596,#57597,#57598,#57599,#57600,#57601,
#57602,#57603,#57604,#57605,#57606,#57607,#57608,#57609,#57610,#57611,#57612,
#57613,#57614,#57615,#57616,#57617,#57618,#57619,#57620,#57621,#57622,#57623,
#57624,#57625,#57626,#57627,#57628,#57629,#57630,#57631,#57632,#57633,#57634,
#57635,#57636,#57637,#57638,#57639,#57640,#57641,#57642,#57643,#57644,#57645,
#57646,#57647,#57648,#57649,#57650,#57651,#57652,#57653,#57654,#57655,#57656,
#57657,#57658,#57659,#57660,#57661,#57662,#57663,#57664,#57665,#57666,#57667,
#57668,#57669,#57670,#57671,#57672,#57673,#57674,#57675,#57676,#57677,#57678,
#57679,#57680,#57681,#57682,#57683,#57684,#57685,#57686,#57687,#57688,#57689,
#57690,#57691,#57692,#57693,#57694,#57695,#57696,#57697,#57698,#57699,#57700,
#57701,#57702,#57703,#57704,#57705,#57706,#57707,#57708,#57709,#57710,#57711,
#57712,#57713,#57714,#57715,#57716,#57717,#57718,#57719,#57720,#57721,#57722,
#57723,#57724,#57725,#57726,#57727,#57728,#57729,#57730,#57731,#57732,#57733,
#57734,#57735,#57736,#57737,#57738,#57739,#57740,#57741,#57742,#57743,#57744,
#57745,#57746,#57747,#57748,#57749,#57750,#57751,#57752,#57753,#57754,#57755,
#57756,#57757,#57758,#57759,#57760,#57761,#57762,#57763,#57764,#57765,#57766,
#57767,#57768,#57769,#57770,#57771,#57772,#57773,#57774,#57775,#57776,#57777,
#57778,#57779,#57780,#57781,#57782,#57783,#57784,#57785,#57786,#57787,#57788,
#57789,#57790,#57791,#57792,#57793,#57794,#57795,#57796,#57797,#57798,#57799,
#57800,#57801,#57802,#57803,#57804,#57805,#57806,#57807,#57808,#57809,#57810,
#57811,#57812,#57813,#57814,#57815,#57816,#57817,#57818,#57819,#57820,#57821,
#57822,#57823,#57824,#57825,#57826,#57827,#57828,#57829,#57830,#57831,#57832,
#57833,#57834,#57835,#57836,#57837,#57838,#57839,#57840,#57841,#57842,#57843,
#57844,#57845,#57846,#57847,#57848,#57849,#57850,#57851,#57852,#57853,#57854,
#57855,#57856,#57857,#57858,#57859,#57860,#57861,#57862,#57863,#57864,#57865,
#57866,#57867,#57868,#57869,#57870,#57871,#57872,#57873,#57874,#57875,#57876,
#57877,#57878,#57879,#57880,#57881,#57882,#57883,#57884,#57885,#57886,#57887,
#57888,#57889,#57890,#57891,#57892,#57893,#57894,#57895,#57896,#57897,#57898,
#57899,#57900,#57901,#57902,#57903,#57904,#57905,#57906,#57907,#57908,#57909,
#57910,#57911,#57912,#57913,#57914,#57915,#57916,#57917,#57918,#57919,#57920,
#57921,#57922,#57923,#57924,#57925,#57926,#57927,#57928,#57929,#57930,#57931,
#57932,#57933,#57934,#57935,#57936,#57937,#57938,#57939,#57940,#57941,#57942,
#57943,#57944,#57945,#57946,#57947,#57948,#57949,#57950,#57951,#57952,#57953,
#57954,#57955,#57956,#57957,#57958,#57959,#57960,#57961,#57962,#57963,#57964,
#57965,#57966,#57967,#57968,#57969,#57970,#57971,#57972,#57973,#57974,#57975,
#57976),.UNSPECIFIED.,.F.,.F.,(4,3,3,3,3,3,3,3,3,3,3,3,3,3,3,3,3,3,3,3,
3,3,3,3,3,3,3,3,3,3,3,3,3,3,3,3,3,3,3,3,3,3,3,3,3,3,3,3,3,3,3,3,3,3,3,3,
3,3,3,3,3,3,3,3,3,3,3,3,3,3,3,3,3,3,3,3,3,3,3,3,3,3,3,3,3,3,3,3,3,3,3,3,
3,3,3,3,3,3,3,3,3,3,3,3,3,3,3,3,3,3,3,3,3,3,3,3,3,3,3,3,3,3,3,3,3,3,3,3,
3,3,3,3,3,3,3,3,3,3,3,3,3,3,3,3,3,3,3,3,3,3,3,3,3,3,3,3,3,3,3,3,3,3,3,3,
3,3,3,3,3,3,3,3,3,3,3,3,3,3,3,3,3,3,3,3,3,4),(0.242278780929826,0.242618092734303,
0.24333413469777,0.244041377852319,0.244276211430585,0.244477134072873,
0.245048716885547,0.245630318148922,0.245934257263667,0.24651646348893,
0.246676009090878,0.247275528750946,0.247593525392491,0.248197421968456,
0.248793107754317,0.248874884108883,0.249253083014459,0.249841372675952,
0.250430946208237,0.25091227673342,0.251073759126888,0.251694184001655,
0.252331325282905,0.252572255228947,0.253211703330374,0.253272634144893,
0.253915385740023,0.254232115752439,0.254875938471737,0.255471509162898,
0.255892371854385,0.256671581711036,0.257488034344503,0.257670384180903,
0.258104037545759,0.258647290627824,0.25919235253277,0.259720571055585,
0.259869259198908,0.260315674536895,0.260920072763573,0.261541478450576,
0.26215654026975,0.262525647993766,0.262801092556248,0.263395374712079,
0.263631320840352,0.264232047831297,0.264267009234918,0.264736085275376,
0.264999967574253,0.265520860472095,0.265732925913588,0.266363313930647,
0.26694788496221,0.267198842592258,0.26796439105204,0.268664759270928,0.269159798730286,
0.269838257667216,0.270130675949598,0.27065940760475,0.270818435077856,
0.271334239762136,0.271596592628268,0.272121943008842,0.272478740635087,
0.273006150744408,0.273535551497999,0.274049971110777,0.274528425985608,
0.27496557447442,0.275526621230416,0.275794006797749,0.276377267361676,
0.276945889259611,0.277450741186514,0.277460259342948,0.278071205706145,
0.278688949701149,0.279110613584496,0.279659134360953,0.28030602981158,
0.280770741699047,0.281406076164999,0.281858009378958,0.28243267024347,
0.283055968940653,0.283681117572295,0.284056884396963,0.28409226323821,
0.284782864424869,0.285484490530849,0.28575124579018,0.286255759414968,
0.286581040013058,0.287155883361734,0.287409792675525,0.287982238169878,
0.288238782002927,0.288454634432973,0.288986046819895,0.289068666071738,
0.289603870252683,0.290139223277884,0.290653509450978,0.291141623420863,
0.29161324931921,0.29175294695998,0.292315024123177,0.292385994793472,0.292852384468983,
0.293313484425323,0.293775351727085,0.293951821977985,0.294044613232258,
0.294457492982334,0.294869659538409,0.295051259486988,0.295531943183432,
0.295703522559497,0.296188974291973,0.296673748337722,0.297155815944093,
0.297250134504992,0.297731578182707,0.297915726534434,0.29839946085133,
0.298883836628845,0.299363939507877,0.299449009522997,0.299984447864382,
0.300127479234637,0.300680364295311,0.301219414013074,0.301647884541002,
0.302211754014893,0.302338298452502,0.302904677623029,0.302959531988322,
0.303518684943125,0.303581301750564,0.303846759559007,0.304359108159607,
0.304825946455333,0.305342469693399,0.305858608951964,0.306045634577012,
0.306534541228051,0.307021795839783,0.307314705683034,0.307799676321633,
0.308244509595017,0.308560286619933,0.309078981781974,0.309598360370356,
0.309804512206349,0.310325829198734,0.310443384613022,0.310937225600257,
0.311434800905744,0.311930980948835,0.31229262793642,0.312642259631027,
0.313177966841344,0.313722311584695,0.314253098011966,0.31477866501222,
0.315309133748266,0.315574092988367,0.316040840884101,0.31651564394236,
0.316987351420504,0.317269581931868,0.317742925877595,0.318206935144652,
0.318505926345707,0.31896678814637,0.319438255897193,0.319761756688362,
0.320227810551655,0.320695470738025,0.321150972778566,0.321437759703047,
0.321843502411458,0.322249245119868),.UNSPECIFIED.);
#800=B_SPLINE_CURVE_WITH_KNOTS('',3,(#58233,#58234,#58235,#58236,#58237,
#58238,#58239,#58240,#58241,#58242,#58243,#58244,#58245,#58246,#58247,#58248,
#58249,#58250,#58251,#58252,#58253,#58254,#58255,#58256,#58257,#58258,#58259,
#58260,#58261,#58262,#58263,#58264,#58265,#58266,#58267,#58268,#58269),
 .UNSPECIFIED.,.F.,.F.,(4,1,1,1,1,1,1,1,1,1,1,1,1,1,1,1,1,1,1,1,1,1,1,1,
1,1,1,1,1,1,1,1,1,1,4),(0.410646223392491,0.412844762664804,0.415043637537941,
0.417242512411078,0.419441387284215,0.421640262157351,0.423839137030488,
0.426038011903625,0.428236886776761,0.43019144221955,0.431168719940944,
0.434100553105126,0.437032386269308,0.439964219433491,0.442896052597673,
0.445827885761855,0.448759718926038,0.45169155209022,0.454623385254402,
0.457555218418585,0.460487051582767,0.463418884746949,0.465617759620086,
0.467816634493223,0.470015509366359,0.472214384239496,0.474413259112633,
0.47661213398577,0.478811008858906,0.481009883732043,0.48320875860518,0.485407633478317,
0.487606508351453,0.48980538322459,0.490612244996583),.UNSPECIFIED.);
#801=B_SPLINE_CURVE_WITH_KNOTS('',3,(#58522,#58523,#58524,#58525,#58526,
#58527,#58528,#58529,#58530,#58531,#58532,#58533,#58534,#58535,#58536,#58537,
#58538,#58539,#58540,#58541,#58542,#58543,#58544,#58545,#58546,#58547,#58548,
#58549,#58550,#58551,#58552,#58553,#58554,#58555,#58556,#58557,#58558,#58559,
#58560,#58561,#58562),.UNSPECIFIED.,.F.,.F.,(4,1,1,1,1,1,1,1,1,1,1,1,1,
1,1,1,1,1,1,1,1,1,1,1,1,1,1,1,1,1,1,1,1,1,1,1,1,1,4),(0.579016667860491,
0.581212386019991,0.583411260963338,0.585610135906685,0.587809010850032,
0.590007885793379,0.592206760736727,0.594405635680074,0.596604510623421,
0.599536343881217,0.602468177139013,0.605400010396809,0.605949729132646,
0.607598885340156,0.609797760283503,0.61199663522685,0.614195510170197,
0.616394385113544,0.618593260056891,0.620792135000238,0.621891572471912,
0.622991009943585,0.625922843201381,0.627388759830279,0.629587634773626,
0.631786509716973,0.633985384660321,0.636184259603668,0.637650176232566,
0.640582009490362,0.642780884433709,0.644979759377056,0.647178634320403,
0.64937750926375,0.651576384207097,0.653775259150444,0.655974134093791,
0.658173009037138,0.658979631102386),.UNSPECIFIED.);
#802=B_SPLINE_CURVE_WITH_KNOTS('',3,(#58791,#58792,#58793,#58794,#58795,
#58796,#58797,#58798,#58799,#58800,#58801,#58802,#58803,#58804,#58805,#58806,
#58807,#58808,#58809,#58810,#58811,#58812,#58813,#58814,#58815,#58816,#58817,
#58818,#58819,#58820,#58821,#58822,#58823,#58824,#58825,#58826,#58827,#58828,
#58829,#58830,#58831,#58832,#58833,#58834,#58835,#58836,#58837,#58838,#58839,
#58840,#58841,#58842,#58843,#58844,#58845,#58846,#58847,#58848,#58849,#58850,
#58851,#58852,#58853,#58854,#58855,#58856,#58857,#58858,#58859,#58860,#58861,
#58862,#58863,#58864,#58865,#58866,#58867,#58868,#58869,#58870,#58871,#58872,
#58873,#58874,#58875,#58876,#58877,#58878,#58879,#58880,#58881,#58882,#58883,
#58884,#58885,#58886,#58887,#58888,#58889,#58890,#58891,#58892,#58893,#58894,
#58895,#58896,#58897,#58898,#58899,#58900,#58901,#58902,#58903,#58904,#58905,
#58906,#58907,#58908,#58909,#58910,#58911,#58912,#58913,#58914,#58915,#58916,
#58917,#58918,#58919,#58920,#58921,#58922,#58923,#58924,#58925,#58926,#58927,
#58928,#58929,#58930,#58931,#58932,#58933,#58934,#58935,#58936,#58937,#58938,
#58939,#58940,#58941,#58942,#58943,#58944,#58945,#58946,#58947,#58948,#58949,
#58950,#58951,#58952,#58953,#58954,#58955,#58956,#58957,#58958,#58959,#58960,
#58961,#58962,#58963,#58964,#58965,#58966,#58967,#58968,#58969,#58970,#58971,
#58972,#58973,#58974,#58975,#58976,#58977,#58978,#58979,#58980,#58981,#58982,
#58983,#58984,#58985,#58986,#58987,#58988,#58989,#58990,#58991,#58992,#58993,
#58994,#58995,#58996,#58997,#58998,#58999,#59000,#59001,#59002,#59003,#59004,
#59005,#59006,#59007,#59008,#59009,#59010,#59011,#59012,#59013,#59014,#59015,
#59016,#59017,#59018,#59019,#59020,#59021,#59022,#59023,#59024,#59025,#59026,
#59027,#59028,#59029,#59030,#59031,#59032,#59033,#59034,#59035,#59036,#59037,
#59038,#59039,#59040,#59041,#59042,#59043,#59044,#59045,#59046,#59047,#59048,
#59049,#59050,#59051,#59052,#59053,#59054,#59055,#59056,#59057,#59058,#59059,
#59060,#59061,#59062,#59063,#59064,#59065,#59066,#59067,#59068,#59069,#59070,
#59071,#59072,#59073,#59074,#59075,#59076,#59077,#59078,#59079,#59080,#59081,
#59082,#59083,#59084,#59085,#59086,#59087,#59088,#59089,#59090,#59091,#59092,
#59093,#59094,#59095,#59096,#59097,#59098,#59099,#59100,#59101,#59102,#59103,
#59104,#59105,#59106,#59107,#59108,#59109,#59110,#59111,#59112,#59113,#59114,
#59115,#59116,#59117,#59118,#59119,#59120,#59121,#59122,#59123,#59124,#59125,
#59126,#59127,#59128,#59129,#59130,#59131,#59132,#59133,#59134,#59135,#59136,
#59137,#59138,#59139,#59140,#59141,#59142,#59143,#59144,#59145,#59146,#59147,
#59148,#59149,#59150,#59151,#59152,#59153,#59154,#59155,#59156,#59157,#59158,
#59159,#59160,#59161,#59162,#59163,#59164,#59165,#59166,#59167,#59168,#59169,
#59170,#59171,#59172,#59173,#59174,#59175,#59176,#59177,#59178,#59179,#59180,
#59181,#59182,#59183,#59184,#59185,#59186,#59187,#59188,#59189,#59190,#59191,
#59192,#59193,#59194,#59195,#59196,#59197,#59198,#59199,#59200,#59201,#59202,
#59203,#59204,#59205,#59206,#59207,#59208,#59209,#59210,#59211,#59212,#59213,
#59214,#59215,#59216,#59217,#59218,#59219,#59220,#59221,#59222,#59223,#59224,
#59225,#59226,#59227,#59228,#59229,#59230,#59231,#59232,#59233,#59234,#59235,
#59236,#59237,#59238,#59239,#59240,#59241,#59242,#59243,#59244,#59245,#59246,
#59247,#59248,#59249,#59250,#59251,#59252,#59253,#59254,#59255,#59256,#59257,
#59258,#59259,#59260,#59261,#59262,#59263,#59264,#59265,#59266,#59267,#59268,
#59269,#59270,#59271,#59272,#59273,#59274,#59275,#59276,#59277,#59278,#59279,
#59280,#59281,#59282,#59283,#59284,#59285,#59286,#59287,#59288,#59289,#59290,
#59291,#59292,#59293,#59294,#59295,#59296,#59297,#59298,#59299,#59300,#59301,
#59302,#59303,#59304,#59305,#59306,#59307,#59308,#59309,#59310,#59311,#59312,
#59313,#59314,#59315,#59316,#59317,#59318,#59319,#59320,#59321,#59322,#59323,
#59324,#59325,#59326,#59327,#59328,#59329,#59330,#59331,#59332,#59333,#59334,
#59335,#59336,#59337,#59338,#59339,#59340,#59341,#59342,#59343,#59344,#59345,
#59346,#59347,#59348,#59349,#59350,#59351,#59352,#59353,#59354,#59355,#59356,
#59357,#59358,#59359,#59360,#59361,#59362,#59363,#59364,#59365,#59366,#59367,
#59368,#59369,#59370,#59371,#59372,#59373,#59374,#59375,#59376,#59377,#59378,
#59379,#59380,#59381,#59382,#59383,#59384,#59385,#59386,#59387,#59388,#59389,
#59390,#59391,#59392,#59393,#59394,#59395,#59396,#59397,#59398,#59399,#59400,
#59401,#59402,#59403,#59404,#59405,#59406,#59407,#59408,#59409,#59410,#59411,
#59412,#59413,#59414,#59415,#59416,#59417,#59418,#59419,#59420,#59421,#59422,
#59423,#59424,#59425,#59426,#59427,#59428,#59429,#59430,#59431,#59432,#59433,
#59434,#59435,#59436,#59437,#59438,#59439,#59440,#59441,#59442,#59443,#59444,
#59445,#59446,#59447,#59448,#59449,#59450,#59451,#59452,#59453,#59454,#59455,
#59456,#59457,#59458,#59459,#59460,#59461,#59462,#59463,#59464,#59465,#59466,
#59467,#59468,#59469,#59470,#59471,#59472,#59473,#59474,#59475,#59476,#59477,
#59478,#59479,#59480,#59481,#59482,#59483,#59484,#59485,#59486,#59487,#59488,
#59489,#59490,#59491,#59492,#59493,#59494,#59495,#59496,#59497,#59498,#59499,
#59500,#59501,#59502,#59503,#59504,#59505,#59506,#59507,#59508,#59509,#59510,
#59511,#59512,#59513,#59514,#59515,#59516,#59517,#59518,#59519,#59520,#59521,
#59522,#59523,#59524,#59525,#59526,#59527,#59528,#59529,#59530,#59531,#59532,
#59533,#59534,#59535,#59536,#59537,#59538,#59539,#59540,#59541,#59542,#59543,
#59544,#59545,#59546,#59547,#59548,#59549,#59550,#59551,#59552,#59553,#59554,
#59555,#59556,#59557,#59558,#59559,#59560,#59561,#59562,#59563,#59564,#59565,
#59566,#59567,#59568,#59569,#59570,#59571,#59572,#59573,#59574,#59575,#59576,
#59577,#59578,#59579,#59580,#59581,#59582,#59583,#59584,#59585,#59586,#59587,
#59588,#59589,#59590,#59591,#59592,#59593,#59594,#59595,#59596,#59597,#59598,
#59599,#59600,#59601,#59602,#59603,#59604,#59605,#59606,#59607,#59608,#59609,
#59610,#59611,#59612,#59613,#59614,#59615,#59616,#59617,#59618,#59619,#59620,
#59621,#59622,#59623,#59624,#59625,#59626,#59627,#59628,#59629,#59630,#59631,
#59632,#59633,#59634,#59635,#59636,#59637,#59638,#59639,#59640,#59641,#59642,
#59643,#59644,#59645,#59646,#59647,#59648,#59649,#59650,#59651,#59652,#59653,
#59654,#59655,#59656,#59657,#59658,#59659,#59660,#59661,#59662,#59663,#59664,
#59665,#59666,#59667,#59668,#59669,#59670,#59671,#59672,#59673,#59674,#59675,
#59676,#59677,#59678,#59679,#59680,#59681,#59682,#59683,#59684,#59685,#59686,
#59687,#59688,#59689,#59690,#59691,#59692,#59693,#59694,#59695,#59696,#59697,
#59698,#59699,#59700,#59701,#59702,#59703,#59704,#59705,#59706,#59707,#59708,
#59709),.UNSPECIFIED.,.F.,.F.,(4,3,3,3,3,3,3,3,3,3,3,3,3,3,3,3,3,3,3,3,
3,3,3,3,3,3,3,3,3,3,3,3,3,3,3,3,3,3,3,3,3,3,3,3,3,3,3,3,3,3,3,3,3,3,3,3,
3,3,3,3,3,3,3,3,3,3,3,3,3,3,3,3,3,3,3,3,3,3,3,3,3,3,3,3,3,3,3,3,3,3,3,3,
3,3,3,3,3,3,3,3,3,3,3,3,3,3,3,3,3,3,3,3,3,3,3,3,3,3,3,3,3,3,3,3,3,3,3,3,
3,3,3,3,3,3,3,3,3,3,3,3,3,3,3,3,3,3,3,3,3,3,3,3,3,3,3,3,3,3,3,3,3,3,3,3,
3,3,3,3,3,3,3,3,3,3,3,3,3,3,3,3,3,3,3,3,3,3,3,3,3,3,3,3,3,3,3,3,3,3,3,3,
3,3,3,3,3,3,3,3,3,3,3,3,3,3,3,3,3,3,3,3,3,3,3,3,3,3,3,3,3,3,3,3,3,3,3,3,
3,3,3,3,3,3,3,3,3,3,3,3,3,3,3,3,3,3,3,3,3,3,3,3,3,3,3,3,3,3,3,3,3,3,3,3,
3,3,3,3,3,3,3,3,3,3,3,3,3,3,3,3,3,3,3,3,3,3,3,3,3,3,3,3,3,3,3,3,3,3,4),
(0.747382054616714,0.747723038678491,0.748202269571123,0.74844883371857,
0.749008302929647,0.74916671941293,0.749528589991814,0.749579915917099,
0.749580010757179,0.749880419804752,0.749935683138351,0.750396885757279,
0.750520960225312,0.75097500210156,0.751115880591238,0.751531129716683,
0.751697873792483,0.751778842328894,0.751778885415099,0.752087027424461,
0.752147527493318,0.752710384626379,0.753252218158787,0.753689424921576,
0.753804640846901,0.753977760073019,0.753977856839936,0.75408108747541,
0.754272811119852,0.754357333043548,0.754699169061808,0.754867244488106,
0.755166403756855,0.755388891802379,0.755692376950258,0.755909909618255,
0.756176186880368,0.756261221312009,0.756625573646643,0.756670821449427,
0.757100721728996,0.757171848282764,0.757450691416385,0.757672875116101,
0.757944696329765,0.758168389129736,0.758375313153121,0.758467352615369,
0.758844930392626,0.75910288258438,0.75938033151878,0.759819370162283,0.76010368649377,
0.760574112800631,0.76099205141762,0.761293258545597,0.76140999003461,0.761739345794588,
0.761825011746506,0.762318635961665,0.762654832237045,0.762773128011837,
0.762773258704699,0.763163612286573,0.763304930448033,0.763483618470429,
0.764019382630583,0.764311891898089,0.764764186400357,0.764840655750405,
0.764972023353423,0.764972133362619,0.765142182321038,0.765487971287168,
0.765709927374939,0.765971621054858,0.766552642238766,0.766799771284327,
0.767193837514219,0.767372463085503,0.767628716700242,0.767903900615377,
0.767903966239845,0.768353405009465,0.768650907782731,0.769033201735314,
0.769287361593117,0.769369882678459,0.769369920962504,0.769785302193162,
0.770039179151212,0.770462476011809,0.770785965982225,0.770835773634281,
0.770835799117072,0.770945912131936,0.771342306762054,0.771486999743917,
0.771901330964326,0.772044984188627,0.772475802820194,0.772602228832398,
0.772942395894644,0.773184930413349,0.773514816942057,0.773725206909473,
0.773767558086762,0.773767631994299,0.774186188963178,0.774262105726299,
0.77477864263865,0.775301458601153,0.775816670237033,0.775919541898361,
0.776309266557836,0.776546231145194,0.776698991217311,0.776775534823269,
0.777138450090972,0.777205482842393,0.77753215344153,0.777582747727868,
0.777957135771029,0.778093502396538,0.778608378739238,0.779030365986988,
0.779112889064764,0.779239979157345,0.779609566486991,0.779631140889186,
0.779631297748752,0.779956665100638,0.780169911509665,0.780531191103311,
0.780728103769669,0.780900663678196,0.781299942217719,0.781460567508864,
0.78185932742848,0.78201572572199,0.782391400280891,0.782563050622278,0.782563130625979,
0.782964008759921,0.783111640805055,0.78361561358035,0.783704798968149,
0.784208259868694,0.784305593985655,0.784761888807492,0.784762005283899,
0.785123582173051,0.785322296162653,0.78577830524352,0.785866123240921,
0.786338607216922,0.78641350159137,0.786825803734849,0.786960813347516,
0.786960879941819,0.787327998131616,0.787535326014198,0.788083399091502,
0.788138035729741,0.788681878089593,0.788742765766024,0.789159710924315,
0.789159754599739,0.789193388003017,0.789715694225066,0.789807334753473,
0.790429064212927,0.790851068948597,0.791262045509168,0.791358565392232,
0.791358629257659,0.791800808504292,0.791982707831161,0.79250987342608,
0.793019764643509,0.793133205933914,0.793557503915579,0.793557507375853,
0.794020865954325,0.794168625464213,0.794773937904032,0.794836761703345,
0.795403737480731,0.795500193464019,0.795756378573499,0.795756386599024,
0.795826979655061,0.796462092472985,0.797100232755515,0.79748544524889,
0.797914918373215,0.797955253231419,0.797955261888282,0.798421202840041,
0.79847889762451,0.798730652250557,0.79925557914175,0.799778777006595,0.800154127889339,
0.800154139653922,0.800752363184986,0.800804399518246,0.801407801642156,
0.801930308659008,0.802005444173409,0.802353002547259,0.802353022430264,
0.80246383986443,0.803061505625562,0.80366471129822,0.804123378741273,0.804538721293759,
0.804551877205179,0.804551905522224,0.805023654326599,0.805134139385097,
0.805694313921552,0.80572529726815,0.805783946796156,0.806371824062616,
0.806750751863099,0.806750779738102,0.807286825348273,0.807341143428747,
0.807444172866529,0.808032395395678,0.808066108539222,0.808646875573981,
0.808688305252117,0.808949626521019,0.808949630238794,0.809382225807286,
0.809519805753925,0.809932883978935,0.810452376293869,0.810505441540481,
0.81098571268166,0.811070464319094,0.811148395102808,0.811148501178939,
0.811176420276288,0.81160573932313,0.811739281771248,0.812301869196572,
0.812419820582741,0.81298439977347,0.813347341007746,0.813347375836859,
0.813716239417427,0.813813496249108,0.814284176332224,0.814666964667789,
0.814905184228181,0.815373273192269,0.815545897535462,0.815546250494779,
0.815978763041164,0.816250742584155,0.816924770873125,0.81696629174527,
0.817391265768666,0.817702097809648,0.817744729731671,0.817745125152699,
0.818193730523411,0.81825983321799,0.818633503933522,0.819145183541033,
0.819643237645425,0.819876160343907,0.819943925946354,0.819943999810619,
0.820417494266013,0.820767236993593,0.821122107885917,0.821700672166623,
0.82192438241048,0.822142874468539,0.822142942441421,0.822366378794246,
0.822812878269025,0.822988386454827,0.823375661000645,0.82343626103651,
0.823608790907153,0.823608958191491,0.823963851307888,0.824171091480278,
0.824582975191355,0.824746096576986,0.824858532840308,0.825273656933478,
0.825433414257374,0.825841003525415,0.825997545689005,0.826332597592095,
0.826540623784379,0.82654076757806,0.826870780522054,0.826944975091906,
0.827278644560235,0.82734781356787),.UNSPECIFIED.);
#803=B_SPLINE_CURVE_WITH_KNOTS('',3,(#59710,#59711,#59712,#59713,#59714,
#59715,#59716,#59717,#59718,#59719,#59720,#59721,#59722,#59723,#59724,#59725,
#59726,#59727,#59728,#59729,#59730,#59731,#59732,#59733,#59734,#59735,#59736,
#59737,#59738,#59739,#59740,#59741,#59742,#59743,#59744,#59745,#59746,#59747,
#59748,#59749,#59750,#59751,#59752,#59753,#59754,#59755,#59756,#59757,#59758,
#59759,#59760,#59761,#59762,#59763,#59764,#59765,#59766,#59767,#59768,#59769,
#59770,#59771,#59772,#59773,#59774,#59775,#59776,#59777,#59778,#59779,#59780,
#59781,#59782,#59783,#59784,#59785,#59786,#59787,#59788,#59789,#59790,#59791,
#59792,#59793,#59794,#59795,#59796,#59797,#59798,#59799,#59800,#59801,#59802,
#59803,#59804,#59805,#59806,#59807,#59808,#59809,#59810,#59811,#59812,#59813,
#59814,#59815,#59816,#59817,#59818,#59819,#59820,#59821,#59822,#59823,#59824,
#59825,#59826,#59827,#59828,#59829,#59830,#59831,#59832,#59833,#59834,#59835,
#59836,#59837,#59838,#59839,#59840,#59841,#59842,#59843,#59844,#59845,#59846,
#59847,#59848,#59849,#59850,#59851,#59852,#59853,#59854,#59855,#59856,#59857,
#59858,#59859,#59860,#59861,#59862,#59863,#59864,#59865,#59866,#59867,#59868,
#59869,#59870,#59871,#59872,#59873,#59874,#59875,#59876,#59877,#59878,#59879,
#59880,#59881,#59882,#59883,#59884,#59885,#59886,#59887,#59888,#59889,#59890,
#59891,#59892,#59893,#59894,#59895,#59896,#59897,#59898,#59899,#59900,#59901,
#59902,#59903,#59904,#59905,#59906,#59907,#59908,#59909,#59910,#59911,#59912,
#59913,#59914,#59915,#59916,#59917,#59918,#59919,#59920,#59921,#59922,#59923,
#59924,#59925,#59926,#59927,#59928,#59929,#59930,#59931,#59932,#59933,#59934,
#59935,#59936,#59937,#59938,#59939,#59940,#59941,#59942,#59943,#59944,#59945,
#59946,#59947,#59948,#59949,#59950,#59951,#59952,#59953,#59954,#59955,#59956,
#59957,#59958,#59959,#59960,#59961,#59962,#59963,#59964,#59965,#59966,#59967,
#59968,#59969,#59970,#59971,#59972,#59973,#59974,#59975,#59976,#59977,#59978,
#59979,#59980,#59981,#59982,#59983,#59984,#59985,#59986,#59987,#59988,#59989,
#59990,#59991,#59992,#59993,#59994,#59995,#59996,#59997,#59998,#59999,#60000,
#60001,#60002,#60003,#60004,#60005,#60006,#60007,#60008,#60009,#60010,#60011,
#60012,#60013,#60014,#60015,#60016,#60017,#60018,#60019,#60020,#60021,#60022,
#60023,#60024,#60025,#60026,#60027,#60028,#60029,#60030,#60031,#60032,#60033,
#60034,#60035,#60036,#60037,#60038,#60039,#60040,#60041,#60042,#60043,#60044,
#60045,#60046,#60047,#60048,#60049,#60050,#60051,#60052,#60053,#60054,#60055,
#60056,#60057,#60058,#60059,#60060,#60061,#60062,#60063,#60064,#60065,#60066,
#60067,#60068,#60069,#60070,#60071,#60072,#60073,#60074,#60075,#60076,#60077,
#60078,#60079,#60080,#60081,#60082,#60083,#60084,#60085,#60086,#60087,#60088,
#60089,#60090,#60091,#60092,#60093,#60094,#60095,#60096,#60097,#60098,#60099,
#60100,#60101,#60102,#60103,#60104,#60105,#60106,#60107,#60108,#60109,#60110,
#60111,#60112,#60113,#60114,#60115,#60116,#60117,#60118,#60119,#60120,#60121,
#60122,#60123,#60124,#60125,#60126,#60127,#60128,#60129,#60130,#60131,#60132,
#60133,#60134,#60135,#60136,#60137,#60138,#60139,#60140,#60141,#60142,#60143,
#60144,#60145,#60146,#60147,#60148,#60149,#60150,#60151,#60152,#60153,#60154,
#60155,#60156,#60157,#60158,#60159,#60160,#60161,#60162,#60163,#60164,#60165,
#60166,#60167,#60168,#60169,#60170,#60171,#60172,#60173,#60174,#60175,#60176,
#60177,#60178,#60179,#60180,#60181,#60182,#60183,#60184,#60185,#60186,#60187,
#60188,#60189,#60190,#60191,#60192,#60193,#60194,#60195,#60196,#60197,#60198,
#60199,#60200,#60201,#60202,#60203,#60204,#60205,#60206,#60207,#60208,#60209,
#60210,#60211,#60212,#60213,#60214,#60215,#60216,#60217,#60218,#60219,#60220,
#60221,#60222,#60223,#60224,#60225,#60226,#60227,#60228,#60229,#60230,#60231,
#60232,#60233,#60234,#60235,#60236,#60237,#60238,#60239,#60240,#60241,#60242,
#60243,#60244,#60245,#60246,#60247,#60248,#60249,#60250,#60251,#60252,#60253,
#60254,#60255,#60256,#60257,#60258,#60259,#60260,#60261,#60262,#60263,#60264,
#60265,#60266,#60267,#60268,#60269,#60270,#60271,#60272,#60273,#60274,#60275,
#60276,#60277,#60278,#60279,#60280,#60281,#60282,#60283,#60284,#60285,#60286,
#60287,#60288,#60289,#60290,#60291,#60292,#60293,#60294,#60295,#60296,#60297,
#60298,#60299,#60300,#60301,#60302,#60303,#60304,#60305,#60306,#60307,#60308,
#60309,#60310,#60311,#60312,#60313,#60314,#60315,#60316,#60317,#60318,#60319,
#60320,#60321,#60322,#60323,#60324,#60325,#60326,#60327,#60328,#60329,#60330,
#60331,#60332,#60333,#60334,#60335,#60336,#60337,#60338,#60339,#60340,#60341,
#60342,#60343,#60344,#60345,#60346,#60347,#60348,#60349,#60350,#60351,#60352,
#60353,#60354,#60355,#60356,#60357,#60358,#60359,#60360,#60361,#60362,#60363,
#60364,#60365,#60366,#60367,#60368,#60369,#60370,#60371,#60372,#60373,#60374,
#60375,#60376,#60377,#60378,#60379,#60380,#60381,#60382,#60383,#60384,#60385,
#60386,#60387,#60388,#60389,#60390,#60391,#60392,#60393,#60394,#60395,#60396,
#60397,#60398,#60399,#60400,#60401,#60402,#60403,#60404,#60405,#60406,#60407,
#60408,#60409,#60410,#60411,#60412,#60413,#60414,#60415,#60416,#60417,#60418,
#60419,#60420,#60421,#60422,#60423,#60424,#60425,#60426,#60427,#60428,#60429,
#60430,#60431,#60432,#60433,#60434,#60435,#60436,#60437,#60438,#60439,#60440,
#60441,#60442,#60443,#60444,#60445,#60446,#60447,#60448,#60449,#60450,#60451,
#60452,#60453,#60454,#60455,#60456,#60457,#60458,#60459,#60460,#60461,#60462,
#60463,#60464,#60465,#60466,#60467,#60468,#60469,#60470,#60471,#60472,#60473,
#60474,#60475,#60476,#60477,#60478,#60479,#60480,#60481,#60482,#60483,#60484,
#60485,#60486,#60487,#60488,#60489,#60490,#60491,#60492,#60493,#60494,#60495,
#60496,#60497,#60498,#60499,#60500,#60501,#60502,#60503,#60504,#60505,#60506,
#60507,#60508,#60509,#60510,#60511,#60512,#60513,#60514,#60515,#60516,#60517,
#60518,#60519,#60520,#60521,#60522,#60523,#60524,#60525,#60526,#60527,#60528,
#60529,#60530,#60531,#60532,#60533,#60534,#60535,#60536,#60537,#60538,#60539,
#60540,#60541,#60542,#60543,#60544,#60545,#60546,#60547,#60548,#60549,#60550,
#60551,#60552,#60553,#60554,#60555,#60556,#60557,#60558,#60559,#60560,#60561,
#60562,#60563,#60564,#60565,#60566,#60567,#60568,#60569,#60570,#60571,#60572,
#60573,#60574,#60575,#60576,#60577,#60578,#60579,#60580,#60581,#60582,#60583,
#60584,#60585,#60586,#60587,#60588,#60589,#60590,#60591,#60592,#60593,#60594,
#60595,#60596,#60597,#60598,#60599,#60600,#60601,#60602,#60603,#60604,#60605,
#60606,#60607,#60608,#60609,#60610,#60611,#60612,#60613,#60614,#60615,#60616,
#60617,#60618,#60619),.UNSPECIFIED.,.F.,.F.,(4,3,3,3,3,3,3,3,3,3,3,3,3,
3,3,3,3,3,3,3,3,3,3,3,3,3,3,3,3,3,3,3,3,3,3,3,3,3,3,3,3,3,3,3,3,3,3,3,3,
3,3,3,3,3,3,3,3,3,3,3,3,3,3,3,3,3,3,3,3,3,3,3,3,3,3,3,3,3,3,3,3,3,3,3,3,
3,3,3,3,3,3,3,3,3,3,3,3,3,3,3,3,3,3,3,3,3,3,3,3,3,3,3,3,3,3,3,3,3,3,3,3,
3,3,3,3,3,3,3,3,3,3,3,3,3,3,3,3,3,3,3,3,3,3,3,3,3,3,3,3,3,3,3,3,3,3,3,3,
3,3,3,3,3,3,3,3,3,3,3,3,3,3,3,3,3,3,3,3,3,3,3,3,3,3,3,3,3,3,3,3,3,3,3,3,
3,3,3,3,3,3,3,3,3,3,3,3,3,3,3,3,3,3,3,3,3,3,3,3,3,3,3,3,3,3,3,3,3,3,3,3,
3,3,3,3,3,3,3,3,3,3,3,3,3,3,3,3,3,3,3,3,3,3,3,3,3,3,3,3,3,3,3,3,3,3,3,3,
3,3,3,3,3,3,3,3,3,3,3,3,3,3,3,3,3,3,3,3,3,3,3,3,3,3,3,3,3,3,3,3,3,3,3,3,
3,3,4),(0.790214816153757,0.790569912932159,0.790786698957973,0.791139692395635,
0.791358581762188,0.791675459555256,0.791914515211802,0.792057822178675,
0.792057831484434,0.792493279308416,0.792711744571504,0.79311285344863,
0.793385243105577,0.793557244181597,0.793854927123416,0.793901305088964,
0.79390138484995,0.794490247500423,0.794524685966545,0.795060349260568,
0.795150689706796,0.795641447294025,0.795744778693493,0.795744902796468,
0.795756264150162,0.796253752507393,0.796565617446721,0.797070681716938,
0.797443362301572,0.797588252298022,0.79758829497373,0.79788503399331,0.797955223872942,
0.798366962195766,0.798548980017166,0.798940476557062,0.799145711584124,
0.799431658291204,0.799431725902551,0.799770230437916,0.800108734973281,
0.800153888614457,0.800353462704815,0.800353573020671,0.800700609162085,
0.801047645303499,0.801275072152928,0.801275199507079,0.801678092781813,
0.80186073652046,0.802207367685839,0.802352732650851,0.802679702991785,
0.802942094934437,0.803118617066971,0.803118673111608,0.803618695631444,
0.803723128122228,0.804120769610145,0.804328625876611,0.80455071990004,
0.804847805473215,0.804962076432187,0.804962146716138,0.805392011572228,
0.805581733389879,0.805988419180543,0.806211517645016,0.806626052872013,
0.806748520090158,0.80706517708908,0.807381834088002,0.807420098105313,
0.807420111522176,0.807774893845597,0.807948018092396,0.808318558284417,
0.808483891046771,0.808864968822568,0.808946153705399,0.809247906925796,
0.809484508039827,0.809774604717984,0.809877765126567,0.809878076328215,
0.810266399909876,0.810438745953138,0.81074548755304,0.811012264872445,
0.811146230491986,0.811486022599776,0.81174113581312,0.812102974217444,
0.812335704768818,0.812336041134254,0.812757787169612,0.812857948877311,
0.813194767928685,0.813345555347721,0.813669091587204,0.813869928052145,
0.814179233637975,0.814325893075373,0.814823251814232,0.815033743755928,
0.815409658391976,0.815545654013101,0.816022780873877,0.816022988343312,
0.816535817934084,0.81691305656922,0.817477046607752,0.81783420511667,0.817866343878736,
0.818061061817964,0.818890304486143,0.818992814305639,0.819544058180871,
0.819709890213367,0.81970993555237,0.819946773129324,0.820391044797367,
0.820631575017876,0.820631672354634,0.821265185675308,0.821553281414016,
0.821553409156899,0.82195500201065,0.822144691572379,0.822475145959163,
0.822475375562885,0.822958579423763,0.823396882761428,0.823397330385553,
0.823611558691224,0.824050027286603,0.824127670438347,0.824541261726617,
0.824649041718287,0.825040793236437,0.82516444291762,0.825240146990458,
0.825240356365957,0.825643669093472,0.825750536801151,0.826218237406702,
0.826260652935695,0.826538839416065,0.826978888682608,0.827049298085276,
0.827083829970486,0.827084172483868,0.827584387071297,0.82809359697854,
0.828312812373505,0.828312815339727,0.828739235283743,0.829278570140441,
0.829374073879451,0.83002507227085,0.830539632263667,0.830671852698409,
0.830770767118543,0.830770777179544,0.830936805196092,0.831604426167356,
0.832267657031647,0.832614250784073,0.832614297691869,0.833134202083226,
0.833659647271449,0.833687434251001,0.834131164567614,0.834233805815265,
0.834457531345718,0.834571947612787,0.834929967250832,0.835272505355427,
0.83555815407035,0.83587651695162,0.836300990365938,0.836417647858886,0.836814204529502,
0.837212975469315,0.837529335421427,0.837841610906211,0.838103107461859,
0.838144473241817,0.838634835439669,0.839248721546978,0.839373472293171,
0.839703219006991,0.839737659885107,0.840270122220773,0.840378982536802,
0.841020766527459,0.841530821308701,0.841650107719815,0.84183154700295,
0.841831618806718,0.841937257470971,0.842504843189513,0.842753326810742,
0.842753355608982,0.843249236999302,0.843517750503382,0.843675117075162,
0.844012011750895,0.844327955724285,0.844677187878075,0.845140805062117,
0.8452153479961,0.845518485467049,0.845518566015776,0.845885120201988,0.846287553509617,
0.846440258754865,0.846758168216791,0.847065903222691,0.847362035674858,
0.847362039620305,0.847779647091993,0.848207802813831,0.848634701462988,
0.849055960793595,0.849205430527273,0.849351336210306,0.849675297785354,
0.849999259360402,0.850443911663908,0.850825142152362,0.850893126352701,
0.851048970462266,0.851048986829363,0.851448702552374,0.851852092648127,
0.852255655565265,0.852655855305455,0.852892365677593,0.853001820079873,
0.853440069578575,0.853759624066998,0.854289093810722,0.854649662780378,
0.854735833886438,0.855090996185286,0.855449762088454,0.855809942981132,
0.856211176172309,0.856488002469863,0.856579317156367,0.856740923477002,
0.857097483084965,0.857448573969311,0.857808311033977,0.85823331905572,
0.858925246424692,0.859037302113415,0.859400435455285,0.85965177878236,
0.859651863650498,0.860188619633516,0.860266343442275,0.860266354852008,
0.860880846053518,0.861453580045515,0.861495306845753,0.861495337255027,
0.861720726503584,0.862176216652237,0.862304564574268,0.862724319658047,
0.86272439754642,0.863110086730732,0.863338810859556,0.863338850477214,
0.863795598860009,0.86392008869005,0.863953302061066,0.86395332216636,0.864523981256641,
0.864759302376409,0.865531958560339,0.866119118894912,0.866411266867105,
0.866411347434597,0.866816667763681,0.866925804754119,0.867318486347646,
0.867447810671785,0.867963858198031,0.868277772104125,0.868317527056099,
0.86861873835963,0.868835480088362,0.868869231673143,0.868869394883433,
0.869238287384484,0.869362882010857,0.869673090830737,0.869862242626579,
0.870305722055053,0.870366513820095,0.870517391042945),.UNSPECIFIED.);
#804=B_SPLINE_CURVE_WITH_KNOTS('',3,(#60952,#60953,#60954,#60955,#60956,
#60957,#60958,#60959,#60960,#60961,#60962,#60963,#60964,#60965,#60966,#60967,
#60968,#60969,#60970,#60971,#60972,#60973,#60974,#60975,#60976,#60977,#60978,
#60979,#60980,#60981,#60982,#60983,#60984,#60985,#60986,#60987,#60988,#60989,
#60990,#60991,#60992,#60993,#60994,#60995,#60996,#60997,#60998,#60999,#61000,
#61001,#61002,#61003,#61004,#61005,#61006,#61007,#61008,#61009,#61010,#61011,
#61012,#61013,#61014,#61015,#61016,#61017,#61018,#61019,#61020,#61021,#61022,
#61023,#61024,#61025,#61026,#61027,#61028,#61029,#61030,#61031,#61032,#61033,
#61034,#61035,#61036,#61037,#61038,#61039,#61040,#61041,#61042,#61043,#61044,
#61045,#61046,#61047,#61048,#61049,#61050,#61051,#61052,#61053,#61054,#61055,
#61056,#61057,#61058,#61059,#61060,#61061,#61062,#61063,#61064,#61065,#61066,
#61067,#61068,#61069,#61070,#61071,#61072,#61073,#61074,#61075,#61076,#61077,
#61078,#61079,#61080,#61081,#61082,#61083,#61084,#61085,#61086,#61087,#61088,
#61089,#61090,#61091,#61092,#61093,#61094,#61095,#61096,#61097,#61098,#61099,
#61100,#61101,#61102,#61103,#61104,#61105,#61106,#61107,#61108,#61109,#61110,
#61111,#61112,#61113,#61114,#61115,#61116,#61117,#61118,#61119,#61120,#61121,
#61122,#61123,#61124,#61125,#61126,#61127,#61128,#61129,#61130,#61131,#61132,
#61133,#61134,#61135,#61136,#61137,#61138,#61139,#61140,#61141,#61142,#61143,
#61144,#61145,#61146,#61147,#61148,#61149,#61150,#61151,#61152,#61153,#61154,
#61155,#61156,#61157,#61158,#61159,#61160,#61161,#61162,#61163,#61164,#61165,
#61166,#61167,#61168,#61169,#61170,#61171,#61172,#61173,#61174,#61175,#61176,
#61177,#61178,#61179,#61180,#61181,#61182,#61183,#61184,#61185,#61186,#61187,
#61188,#61189,#61190,#61191,#61192,#61193,#61194,#61195,#61196,#61197,#61198,
#61199,#61200,#61201,#61202,#61203,#61204,#61205,#61206,#61207,#61208,#61209,
#61210,#61211,#61212,#61213,#61214,#61215,#61216,#61217,#61218,#61219,#61220,
#61221,#61222,#61223,#61224,#61225,#61226,#61227,#61228,#61229,#61230,#61231,
#61232,#61233,#61234,#61235,#61236,#61237,#61238,#61239,#61240,#61241,#61242,
#61243,#61244,#61245,#61246,#61247,#61248,#61249,#61250,#61251,#61252,#61253,
#61254,#61255,#61256,#61257,#61258,#61259,#61260,#61261,#61262,#61263,#61264,
#61265,#61266,#61267,#61268,#61269,#61270,#61271,#61272,#61273,#61274,#61275,
#61276,#61277,#61278,#61279,#61280,#61281,#61282,#61283,#61284,#61285,#61286,
#61287,#61288,#61289,#61290,#61291,#61292,#61293,#61294,#61295,#61296,#61297,
#61298,#61299,#61300,#61301,#61302,#61303,#61304,#61305,#61306,#61307,#61308,
#61309,#61310,#61311,#61312,#61313,#61314,#61315,#61316,#61317,#61318,#61319,
#61320,#61321,#61322,#61323,#61324,#61325,#61326,#61327,#61328,#61329,#61330,
#61331,#61332,#61333,#61334,#61335,#61336,#61337,#61338,#61339,#61340,#61341,
#61342,#61343,#61344,#61345,#61346,#61347,#61348,#61349,#61350,#61351,#61352,
#61353,#61354,#61355,#61356,#61357,#61358,#61359,#61360,#61361,#61362,#61363,
#61364,#61365,#61366,#61367,#61368,#61369,#61370,#61371,#61372,#61373,#61374,
#61375,#61376,#61377,#61378,#61379,#61380,#61381,#61382,#61383,#61384,#61385,
#61386,#61387,#61388,#61389,#61390,#61391,#61392,#61393,#61394,#61395,#61396,
#61397,#61398,#61399,#61400,#61401,#61402,#61403,#61404,#61405,#61406,#61407,
#61408,#61409,#61410,#61411,#61412,#61413,#61414,#61415,#61416,#61417,#61418,
#61419,#61420,#61421,#61422,#61423,#61424,#61425,#61426,#61427,#61428,#61429,
#61430,#61431,#61432,#61433,#61434,#61435,#61436,#61437,#61438,#61439,#61440,
#61441,#61442,#61443,#61444,#61445,#61446,#61447,#61448,#61449,#61450,#61451,
#61452,#61453,#61454,#61455,#61456,#61457,#61458,#61459,#61460,#61461,#61462,
#61463,#61464,#61465,#61466,#61467,#61468,#61469,#61470,#61471,#61472,#61473,
#61474,#61475,#61476,#61477,#61478,#61479,#61480,#61481,#61482,#61483,#61484,
#61485,#61486,#61487,#61488,#61489,#61490,#61491,#61492,#61493,#61494,#61495,
#61496,#61497,#61498,#61499,#61500,#61501,#61502,#61503,#61504,#61505,#61506,
#61507,#61508,#61509,#61510,#61511,#61512,#61513,#61514,#61515,#61516,#61517,
#61518,#61519,#61520,#61521,#61522,#61523,#61524,#61525,#61526,#61527,#61528,
#61529,#61530,#61531,#61532,#61533,#61534,#61535,#61536,#61537,#61538,#61539,
#61540,#61541,#61542,#61543,#61544,#61545,#61546,#61547,#61548,#61549,#61550,
#61551,#61552,#61553,#61554,#61555,#61556,#61557,#61558,#61559,#61560,#61561,
#61562,#61563,#61564,#61565,#61566,#61567,#61568,#61569,#61570,#61571,#61572,
#61573,#61574,#61575,#61576,#61577,#61578,#61579,#61580,#61581,#61582,#61583,
#61584,#61585,#61586,#61587,#61588,#61589,#61590,#61591,#61592,#61593,#61594,
#61595,#61596,#61597,#61598,#61599,#61600,#61601,#61602,#61603,#61604,#61605,
#61606,#61607,#61608,#61609,#61610,#61611,#61612,#61613,#61614,#61615,#61616,
#61617,#61618,#61619,#61620,#61621,#61622,#61623,#61624,#61625,#61626,#61627,
#61628,#61629,#61630,#61631,#61632,#61633,#61634,#61635,#61636,#61637,#61638,
#61639,#61640,#61641,#61642,#61643,#61644,#61645,#61646,#61647,#61648,#61649,
#61650,#61651,#61652,#61653,#61654,#61655,#61656,#61657,#61658,#61659,#61660,
#61661,#61662,#61663,#61664,#61665,#61666,#61667,#61668,#61669,#61670,#61671,
#61672,#61673,#61674,#61675,#61676,#61677,#61678,#61679,#61680,#61681,#61682,
#61683,#61684,#61685,#61686,#61687,#61688,#61689,#61690,#61691,#61692,#61693,
#61694,#61695,#61696,#61697,#61698,#61699,#61700,#61701,#61702,#61703,#61704,
#61705,#61706,#61707,#61708,#61709,#61710,#61711,#61712,#61713,#61714,#61715,
#61716,#61717,#61718,#61719,#61720,#61721,#61722,#61723,#61724,#61725,#61726,
#61727,#61728,#61729,#61730,#61731,#61732,#61733,#61734,#61735,#61736,#61737,
#61738,#61739,#61740,#61741,#61742,#61743,#61744,#61745,#61746,#61747,#61748,
#61749,#61750,#61751,#61752,#61753,#61754,#61755,#61756,#61757,#61758,#61759,
#61760,#61761,#61762,#61763,#61764,#61765,#61766,#61767,#61768,#61769,#61770,
#61771,#61772,#61773,#61774,#61775,#61776,#61777,#61778,#61779,#61780,#61781,
#61782,#61783,#61784,#61785,#61786,#61787,#61788,#61789,#61790,#61791,#61792,
#61793,#61794,#61795,#61796,#61797,#61798,#61799,#61800,#61801,#61802,#61803,
#61804,#61805,#61806,#61807,#61808,#61809,#61810,#61811,#61812,#61813,#61814,
#61815,#61816,#61817,#61818,#61819,#61820,#61821,#61822,#61823,#61824,#61825,
#61826,#61827,#61828,#61829,#61830,#61831,#61832,#61833,#61834,#61835,#61836,
#61837,#61838,#61839,#61840,#61841,#61842,#61843,#61844,#61845,#61846,#61847,
#61848,#61849),.UNSPECIFIED.,.F.,.F.,(4,3,3,3,3,3,3,3,3,3,3,3,3,3,3,3,3,
3,3,3,3,3,3,3,3,3,3,3,3,3,3,3,3,3,3,3,3,3,3,3,3,3,3,3,3,3,3,3,3,3,3,3,3,
3,3,3,3,3,3,3,3,3,3,3,3,3,3,3,3,3,3,3,3,3,3,3,3,3,3,3,3,3,3,3,3,3,3,3,3,
3,3,3,3,3,3,3,3,3,3,3,3,3,3,3,3,3,3,3,3,3,3,3,3,3,3,3,3,3,3,3,3,3,3,3,3,
3,3,3,3,3,3,3,3,3,3,3,3,3,3,3,3,3,3,3,3,3,3,3,3,3,3,3,3,3,3,3,3,3,3,3,3,
3,3,3,3,3,3,3,3,3,3,3,3,3,3,3,3,3,3,3,3,3,3,3,3,3,3,3,3,3,3,3,3,3,3,3,3,
3,3,3,3,3,3,3,3,3,3,3,3,3,3,3,3,3,3,3,3,3,3,3,3,3,3,3,3,3,3,3,3,3,3,3,3,
3,3,3,3,3,3,3,3,3,3,3,3,3,3,3,3,3,3,3,3,3,3,3,3,3,3,3,3,3,3,3,3,3,3,3,3,
3,3,3,3,3,3,3,3,3,3,3,3,3,3,3,3,3,3,3,3,3,3,3,3,3,3,3,3,3,3,4),(0.0145921063417177,
0.01494498896954,0.0151414343792162,0.0155991031283622,0.0157494739476449,
0.0161489199803882,0.0163480559569645,0.0167526091727277,0.0169360751976015,
0.0170193973464053,0.0170194368213593,0.017368557965186,0.017521980587612,
0.0179163174749734,0.0179994507332042,0.0184148530732642,0.0185039806404691,
0.018857211607717,0.0190058494900324,0.0193876186564051,0.0195077183395957,
0.0195079706482738,0.0198311533711606,0.0200317596461261,0.0202503103719008,
0.020712687016784,0.020773069117367,0.0212500144542332,0.0213012015559477,
0.0216870599385147,0.0218178729007355,0.0219407406253231,0.0219963072985394,
0.0223875675982871,0.0225295413822536,0.0229607422921723,0.0230774597141039,
0.0235737137924015,0.0236252067105452,0.0240275589477095,0.0241724863409542,
0.0243476689468201,0.0244638276318662,0.0244848324667108,0.0248526753933804,
0.0250787991879157,0.0253146788360168,0.0258102135546507,0.0259168701165055,
0.0264598074834853,0.0267780626666368,0.0269730901210823,0.0272126543850709,
0.027774826839563,0.0283800367456755,0.0288868553501964,0.0291740997766178,
0.0293794134355193,0.0294613442030393,0.0298883423612777,0.0300672827309982,
0.0304989744969724,0.0306856802261637,0.0311692758229822,0.0312898616254177,
0.0315033199524961,0.0318474081826925,0.0319493233055476,0.0319495774493657,
0.0323241990368826,0.0325826602113226,0.0329349866443945,0.0332374621276672,
0.0336396831011873,0.0337542991621983,0.0340711733376522,0.0343871557854915,
0.0344375457644208,0.034437644298738,0.0348067288873789,0.035008487163829,
0.0353899966968821,0.0355880146777214,0.0359760061919466,0.036003201468871,
0.0363168331776758,0.0365865863245377,0.0366492531037856,0.0366494851815739,
0.0370321297719284,0.0372744054545636,0.0376680801317804,0.0379060310150702,
0.0382521170686287,0.0385643313210177,0.0388612363976579,0.0388613260644098,
0.0392468618100091,0.0394856493157112,0.0398823752779798,0.0401166952531944,
0.0405017407618004,0.0407874538545231,0.0410731669472457,0.041073373049391,
0.0415528364149162,0.0417234699352747,0.0422278153850288,0.0424833601809103,
0.0426585635414544,0.0427321608347829,0.0431787156631357,0.0435358814900289,
0.0439636463244554,0.0442190052732109,0.0443755165973623,0.0443914111588819,
0.0448061473436753,0.0450377385277743,0.0455100533378483,0.0457802046179519,
0.0459562287504106,0.0460503558980555,0.0464650013081703,0.0467517837969972,
0.0472406262110292,0.0475255561546537,0.0477089375385147,0.0482916049754539,
0.0483397610150859,0.0488078257374213,0.0489558236703124,0.0493674487514282,
0.0493675702578804,0.0495086767683798,0.0499464719641969,0.0503781450874696,
0.0508096397703441,0.0510264509200073,0.0510265016895091,0.0513688483338306,
0.0515522143160684,0.0517586266481565,0.0521261839347652,0.0522851145121985,
0.0526853315821342,0.0526854794191335,0.0531575822864484,0.0535147719131977,
0.0535147886692577,0.0539144371248942,0.0540086974632535,0.0543440632094634,
0.0543442122442611,0.0548980825124975,0.0552140451327165,0.0556956457278704,
0.0559524544057642,0.056002955937668,0.0561453754914953,0.0566384143871544,
0.0569984287008584,0.0573827363405339,0.0576444702300798,0.0576617948411024,
0.0578814588978127,0.058478447965699,0.0590684263941783,0.0592803287184296,
0.0593207428682015,0.0594278417913414,0.0598862183712118,0.059918983327099,
0.0603547928964372,0.0603900975280435,0.0605647804224837,0.0605650147272371,
0.0607571971489412,0.0609796303876242,0.0609797348927689,0.0613071045479967,
0.0613955167415226,0.0617853574226454,0.0618109415534416,0.0622251185198664,
0.0624322070030788,0.0625690933163434,0.0626392954862912,0.063034094394662,
0.0634288933030329,0.0637944392139662,0.063820776649469,0.0641301759876878,
0.0642973774473228,0.0642974962170227,0.064773979836535,0.0652629661483903,
0.0657532222072641,0.0658198274911648,0.0659563768791496,0.065956444076727,
0.0664746556612816,0.066998085538047,0.0675072939241088,0.0676152575412766,
0.0676153404644975,0.0680300808427615,0.0684448133482964,0.0689677513501084,
0.0692742443628509,0.0702037589037057,0.0708130175714309,0.0709331218184356,
0.0716612249019194,0.0723947655040235,0.0725750783176391,0.0725918995276573,
0.0725919649161931,0.0733628468827993,0.0741415931240865,0.0742507801897843,
0.074250855677326,0.0742633055451511,0.0748300972933925,0.0753995067141672,
0.0759096608519112,0.0759097695124051,0.0764048701624809,0.0765139566729015,
0.0770037536150007,0.0774264581899242,0.0774949581656026,0.0775685415140381,
0.0775685818723875,0.0780510140055978,0.0781653632510877,0.078681519696992,
0.0787272828532932,0.0787621849881373,0.0792274221761651,0.0792275499018148,
0.0797384782875757,0.0798711594614943,0.0804702982385853,0.080886302838292,
0.0808865897272711,0.0810111587464966,0.0814218995478847,0.0814565399643726,
0.0819050207731814,0.0823193328874672,0.082353789129362,0.0825450841594454,
0.0825451835004189,0.0829466330378264,0.0830276770380248,0.0835106162604698,
0.0839506252503161,0.0839828547202685,0.0842040641625458,0.084204455951171,
0.0843824864714303,0.0848283015634868,0.085081553804432,0.0854720404128058,
0.0857565544251839,0.0858626689985701,0.0858629448246728,0.0862409044962003,
0.0866229519670493,0.0870038229220728,0.0873761996372048,0.0875218254867997,
0.08752211742225,0.0877596849540256,0.0881665392263277,0.0882177692466477,
0.0886992376977871,0.089049265273922,0.0891534495533465,0.0891802236073339,
0.0891807061489266,0.0895954263144584,0.0900046203066122,0.0904221035588329,
0.0908395696551521,0.0908395868110536,0.0911367582134736,0.0917997669311156,
0.0918912333247692,0.0922890067306582,0.0924984225576922,0.0924984674731805,
0.0928255904719477,0.0933612307645322,0.0939025070602852,0.0941572866208839,
0.0941573481353074,0.0944913654294245,0.0945119390290117),.UNSPECIFIED.);
#805=B_SPLINE_CURVE_WITH_KNOTS('',3,(#62206,#62207,#62208,#62209,#62210,
#62211,#62212,#62213,#62214,#62215,#62216,#62217,#62218,#62219,#62220,#62221,
#62222,#62223,#62224,#62225,#62226,#62227,#62228,#62229,#62230,#62231,#62232,
#62233,#62234,#62235,#62236,#62237,#62238,#62239,#62240,#62241,#62242,#62243,
#62244,#62245,#62246,#62247,#62248,#62249,#62250,#62251,#62252,#62253,#62254,
#62255,#62256,#62257,#62258,#62259,#62260,#62261,#62262,#62263,#62264,#62265,
#62266,#62267,#62268,#62269,#62270,#62271,#62272,#62273,#62274,#62275,#62276,
#62277,#62278,#62279,#62280,#62281,#62282,#62283,#62284,#62285,#62286,#62287,
#62288,#62289,#62290,#62291,#62292,#62293,#62294,#62295,#62296,#62297,#62298,
#62299,#62300,#62301,#62302,#62303,#62304,#62305,#62306,#62307,#62308,#62309,
#62310,#62311,#62312,#62313,#62314,#62315,#62316,#62317,#62318,#62319,#62320,
#62321,#62322,#62323,#62324,#62325,#62326,#62327,#62328,#62329,#62330,#62331,
#62332,#62333,#62334,#62335,#62336,#62337,#62338,#62339,#62340,#62341,#62342,
#62343,#62344,#62345,#62346,#62347,#62348,#62349,#62350,#62351,#62352,#62353,
#62354,#62355,#62356,#62357,#62358,#62359,#62360,#62361,#62362,#62363,#62364,
#62365,#62366,#62367,#62368,#62369,#62370,#62371,#62372,#62373,#62374,#62375,
#62376,#62377,#62378,#62379,#62380,#62381,#62382,#62383,#62384,#62385,#62386,
#62387,#62388,#62389,#62390,#62391,#62392,#62393,#62394,#62395,#62396,#62397,
#62398,#62399,#62400,#62401,#62402,#62403,#62404,#62405,#62406,#62407,#62408,
#62409,#62410,#62411,#62412,#62413,#62414,#62415,#62416,#62417,#62418,#62419,
#62420,#62421,#62422,#62423,#62424,#62425,#62426,#62427,#62428,#62429,#62430,
#62431,#62432,#62433,#62434,#62435,#62436,#62437,#62438,#62439,#62440,#62441,
#62442,#62443,#62444,#62445,#62446,#62447,#62448,#62449,#62450,#62451,#62452,
#62453,#62454,#62455,#62456,#62457,#62458,#62459,#62460,#62461,#62462,#62463,
#62464,#62465,#62466,#62467,#62468,#62469,#62470,#62471,#62472,#62473,#62474,
#62475,#62476,#62477,#62478,#62479,#62480,#62481,#62482,#62483,#62484,#62485,
#62486,#62487,#62488,#62489,#62490,#62491,#62492,#62493,#62494,#62495,#62496,
#62497,#62498,#62499,#62500,#62501,#62502,#62503,#62504,#62505,#62506,#62507,
#62508,#62509,#62510,#62511,#62512,#62513,#62514,#62515,#62516,#62517,#62518,
#62519,#62520,#62521,#62522,#62523,#62524,#62525,#62526,#62527,#62528,#62529,
#62530,#62531,#62532,#62533,#62534,#62535,#62536,#62537,#62538,#62539,#62540,
#62541,#62542,#62543,#62544,#62545,#62546,#62547,#62548,#62549,#62550,#62551,
#62552,#62553,#62554,#62555,#62556,#62557,#62558,#62559,#62560,#62561,#62562,
#62563,#62564,#62565,#62566,#62567,#62568,#62569,#62570,#62571,#62572,#62573,
#62574,#62575,#62576,#62577,#62578,#62579,#62580,#62581,#62582,#62583,#62584,
#62585,#62586,#62587,#62588,#62589,#62590,#62591,#62592,#62593,#62594,#62595,
#62596,#62597,#62598,#62599,#62600,#62601,#62602,#62603,#62604,#62605,#62606,
#62607,#62608,#62609,#62610,#62611,#62612,#62613,#62614,#62615,#62616,#62617,
#62618,#62619,#62620,#62621,#62622,#62623,#62624,#62625,#62626,#62627,#62628,
#62629,#62630,#62631,#62632,#62633,#62634,#62635,#62636,#62637,#62638,#62639,
#62640,#62641,#62642,#62643,#62644,#62645,#62646,#62647,#62648,#62649,#62650,
#62651,#62652,#62653,#62654,#62655,#62656,#62657,#62658,#62659,#62660,#62661,
#62662,#62663,#62664,#62665,#62666,#62667,#62668,#62669,#62670,#62671,#62672,
#62673,#62674,#62675,#62676,#62677,#62678,#62679,#62680,#62681,#62682,#62683,
#62684,#62685,#62686,#62687,#62688,#62689,#62690,#62691,#62692,#62693,#62694,
#62695,#62696,#62697,#62698,#62699,#62700,#62701,#62702,#62703,#62704,#62705,
#62706,#62707,#62708,#62709,#62710,#62711,#62712,#62713,#62714,#62715,#62716,
#62717,#62718,#62719,#62720,#62721,#62722,#62723,#62724,#62725,#62726,#62727,
#62728,#62729,#62730,#62731,#62732,#62733,#62734,#62735,#62736,#62737,#62738,
#62739,#62740,#62741,#62742,#62743,#62744,#62745,#62746,#62747,#62748,#62749,
#62750,#62751,#62752,#62753,#62754,#62755,#62756,#62757,#62758,#62759,#62760,
#62761,#62762,#62763,#62764,#62765,#62766,#62767,#62768,#62769,#62770,#62771,
#62772,#62773,#62774,#62775,#62776,#62777,#62778,#62779,#62780,#62781,#62782,
#62783,#62784,#62785,#62786,#62787,#62788,#62789,#62790,#62791,#62792,#62793,
#62794,#62795,#62796,#62797,#62798,#62799,#62800,#62801,#62802,#62803,#62804,
#62805,#62806,#62807,#62808,#62809,#62810,#62811,#62812,#62813,#62814,#62815,
#62816,#62817,#62818,#62819,#62820,#62821,#62822,#62823,#62824,#62825,#62826,
#62827,#62828,#62829,#62830,#62831,#62832,#62833,#62834,#62835,#62836,#62837,
#62838,#62839,#62840,#62841,#62842,#62843,#62844,#62845,#62846,#62847,#62848,
#62849,#62850,#62851,#62852,#62853,#62854,#62855,#62856,#62857,#62858,#62859,
#62860,#62861,#62862,#62863,#62864,#62865,#62866,#62867,#62868,#62869,#62870,
#62871,#62872,#62873,#62874,#62875,#62876,#62877,#62878,#62879,#62880,#62881,
#62882,#62883,#62884,#62885,#62886,#62887,#62888,#62889,#62890,#62891,#62892,
#62893,#62894,#62895,#62896,#62897,#62898,#62899,#62900,#62901,#62902,#62903,
#62904,#62905,#62906,#62907,#62908,#62909,#62910,#62911,#62912,#62913,#62914,
#62915,#62916,#62917,#62918,#62919,#62920,#62921,#62922,#62923,#62924,#62925,
#62926,#62927,#62928,#62929,#62930,#62931,#62932,#62933,#62934,#62935,#62936,
#62937,#62938,#62939,#62940,#62941,#62942,#62943,#62944,#62945,#62946,#62947,
#62948,#62949,#62950,#62951,#62952,#62953,#62954,#62955,#62956,#62957,#62958,
#62959,#62960,#62961,#62962,#62963,#62964,#62965,#62966,#62967,#62968,#62969,
#62970,#62971,#62972,#62973,#62974,#62975,#62976,#62977,#62978,#62979,#62980,
#62981,#62982,#62983,#62984,#62985,#62986,#62987,#62988,#62989,#62990,#62991,
#62992,#62993,#62994,#62995,#62996,#62997,#62998,#62999,#63000,#63001,#63002,
#63003,#63004,#63005,#63006,#63007,#63008,#63009,#63010,#63011,#63012,#63013,
#63014,#63015,#63016,#63017,#63018,#63019,#63020,#63021,#63022,#63023,#63024,
#63025,#63026,#63027,#63028,#63029,#63030,#63031,#63032,#63033,#63034,#63035,
#63036,#63037,#63038,#63039,#63040,#63041,#63042,#63043,#63044,#63045,#63046,
#63047,#63048,#63049,#63050,#63051,#63052,#63053,#63054,#63055,#63056,#63057,
#63058,#63059,#63060,#63061,#63062,#63063,#63064,#63065,#63066,#63067,#63068,
#63069,#63070,#63071,#63072,#63073,#63074,#63075,#63076,#63077,#63078,#63079,
#63080,#63081,#63082,#63083,#63084,#63085,#63086,#63087,#63088,#63089,#63090,
#63091,#63092,#63093,#63094,#63095,#63096,#63097,#63098,#63099,#63100,#63101,
#63102,#63103,#63104,#63105,#63106,#63107,#63108,#63109,#63110,#63111,#63112,
#63113,#63114,#63115,#63116,#63117,#63118,#63119,#63120,#63121,#63122,#63123,
#63124,#63125,#63126,#63127,#63128,#63129,#63130,#63131,#63132,#63133,#63134,
#63135,#63136,#63137,#63138,#63139,#63140,#63141,#63142),.UNSPECIFIED.,
 .F.,.F.,(4,3,3,3,3,3,3,3,3,3,3,3,3,3,3,3,3,3,3,3,3,3,3,3,3,3,3,3,3,3,3,
3,3,3,3,3,3,3,3,3,3,3,3,3,3,3,3,3,3,3,3,3,3,3,3,3,3,3,3,3,3,3,3,3,3,3,3,
3,3,3,3,3,3,3,3,3,3,3,3,3,3,3,3,3,3,3,3,3,3,3,3,3,3,3,3,3,3,3,3,3,3,3,3,
3,3,3,3,3,3,3,3,3,3,3,3,3,3,3,3,3,3,3,3,3,3,3,3,3,3,3,3,3,3,3,3,3,3,3,3,
3,3,3,3,3,3,3,3,3,3,3,3,3,3,3,3,3,3,3,3,3,3,3,3,3,3,3,3,3,3,3,3,3,3,3,3,
3,3,3,3,3,3,3,3,3,3,3,3,3,3,3,3,3,3,3,3,3,3,3,3,3,3,3,3,3,3,3,3,3,3,3,3,
3,3,3,3,3,3,3,3,3,3,3,3,3,3,3,3,3,3,3,3,3,3,3,3,3,3,3,3,3,3,3,3,3,3,3,3,
3,3,3,3,3,3,3,3,3,3,3,3,3,3,3,3,3,3,3,3,3,3,3,3,3,3,3,3,3,3,3,3,3,3,3,3,
3,3,3,3,3,3,3,3,3,3,3,3,3,3,3,3,3,3,3,3,3,3,3,3,3,3,3,3,3,4),(0.182899145085017,
0.183263528687836,0.183473753205273,0.183684503249907,0.184233646645112,
0.18469728350229,0.184783016732281,0.185176818032187,0.185344322912941,
0.18538724782252,0.185387336016129,0.185747562346674,0.185883607088664,
0.186365622168009,0.186468694243726,0.186938533254263,0.187062418288696,
0.187554538554016,0.187640861312347,0.187803828183196,0.187875873458272,
0.188083107361859,0.188716731739939,0.189363513501688,0.189992344245774,
0.190283169440411,0.190363966683647,0.190364102474105,0.190819712278314,
0.191116111418507,0.191656164316416,0.191907597584301,0.192420613141666,
0.192484027826661,0.192793156576219,0.192852282017407,0.192852555815474,
0.193408651590982,0.193926082297544,0.194096439684286,0.194096625798643,
0.194422182597619,0.194581200875238,0.19468462481958,0.194991998383055,
0.195173242549772,0.195336831695984,0.195340844506715,0.195845155854362,
0.195982133749486,0.196359273198225,0.196434056879778,0.19658477886086,
0.196610731556704,0.19688598001007,0.197196240942322,0.197322767162915,
0.197762903007137,0.197828912684925,0.197829208096378,0.198203938783702,
0.19850964682361,0.198867073655538,0.19908576582645,0.199462431600692,0.199774653157635,
0.200140083916306,0.200185540730199,0.200317212902433,0.200317228018684,
0.200701854027722,0.200735557379781,0.201090409704972,0.201285041487425,
0.201561246657516,0.201561385685564,0.201997298267757,0.202087477562286,
0.202549150829979,0.202627626661227,0.202805543352443,0.202805554004613,
0.203136026419175,0.203308333327251,0.203484783426379,0.203844371890436,
0.203989257925437,0.204334977082562,0.204464326246553,0.204464420241616,
0.204833978453808,0.205097849331174,0.205473202780681,0.205683116128945,
0.206004866844681,0.206122912740792,0.206123297130789,0.206787047742686,
0.207389397027825,0.207468693245331,0.207781893952244,0.207782174019962,
0.207881695599617,0.208357870522842,0.20855089979797,0.209050016756459,
0.209230270269441,0.20944082211402,0.209441050909135,0.209756996578365,
0.209904380159533,0.210081414225744,0.210392327296829,0.210544641877459,
0.210838269106101,0.211013217833463,0.211100582903117,0.211565146641376,
0.2120098364277,0.212203496194613,0.212600241665112,0.212714780986435,0.212758685799301,
0.21275880468748,0.213015575233525,0.213387538030512,0.213581822153208,
0.213915939562133,0.21414409078994,0.214417681576653,0.214417912539699,
0.214725395351362,0.214873542956843,0.215246819780476,0.21524712002124,
0.215597339087354,0.215849135163016,0.21586842898292,0.215947558153467,
0.216075777605415,0.216076558465826,0.216467629524831,0.216632026988447,
0.217027887015844,0.217239456887018,0.217588561536885,0.217735435354999,
0.217735621855321,0.218071372391186,0.218236078391015,0.218586937030159,
0.218739189032184,0.218880083140786,0.219198193148187,0.219394098580177,
0.219394312244172,0.219908073787879,0.220430925972927,0.220946014987092,
0.221052933340913,0.221053189133344,0.221378486882475,0.221494608624949,
0.221811069574464,0.222146916265991,0.22226156779849,0.222585586794641,
0.222712066022517,0.223088482336287,0.223224545610072,0.223740289263314,
0.22423957732554,0.224370930705853,0.22437094291169,0.224689150297459,0.224746152019814,
0.225147743921987,0.225234858801252,0.225669314512927,0.225727231999456,
0.225920161194922,0.22603035389434,0.226742531591767,0.227135737726978,
0.227136062561739,0.227436404308476,0.227682241087317,0.228136327237122,
0.228279114908813,0.2287243324094,0.228876111457403,0.229149039882898,0.229347573579209,
0.22934769422317,0.229729127128221,0.229900532542266,0.229900575950594,
0.230319862058617,0.230453472410766,0.230453491505324,0.230616055486533,
0.230977299704976,0.23133732057681,0.231474494916104,0.231559769410146,
0.231944659340071,0.23205681445195,0.232418497812745,0.232547396014727,
0.233048212764105,0.233476881337157,0.233549029513483,0.233771167700448,
0.233771245283669,0.234237080556968,0.234725330117285,0.235213122506284,
0.235685032912032,0.2359830811359,0.235983129298908,0.236368180533942,0.236412945639474,
0.236485191592944,0.236907418779729,0.237336469114539,0.237641958025073,
0.237642030808215,0.238086117418035,0.238532563475558,0.238977264207995,
0.239300834914246,0.239300875336245,0.239415854171785,0.2399662531224,0.23999991490173,
0.24058693707282,0.240959711803418,0.240959742766705,0.241372003695055,
0.241874921163338,0.24237737025309,0.242618588692591,0.242618621288792,
0.243197964750271,0.24326742749683,0.243327117996986,0.243934756051637,
0.243969138825144,0.244277465581764,0.244277486659965,0.244304836536952,
0.24491620539582,0.245282427391075,0.245830524511867,0.245892515830428,
0.245936342470937,0.245936366376164,0.246382230731561,0.24721347027279,
0.247481706076934,0.24759521936011,0.247595273647355,0.248195322597542,
0.248795817345073,0.249254096249282,0.249254158720183,0.24968115631505,
0.250332658316406,0.250752796550357,0.250912973138455,0.250912991795234,
0.251372312400339,0.251411676272452,0.25187978233059,0.252375953614537,
0.252571840869658,0.252571850027628,0.253030524043992,0.253127602265603,
0.253688741088463,0.254079559629245,0.254230726916801,0.254230771577903,
0.254711318370289,0.25519441871275,0.255677046663041,0.255889552746644,
0.255889603805974,0.256279511385039,0.25677729203742,0.256834645518382,
0.257392271578631,0.2578412944297,0.257949164758202,0.258101395718981,0.258101439658204,
0.258479809094404,0.258980782226928,0.259040142400447,0.259604452734636,
0.260055790373525,0.260166297783907,0.260313243681732,0.260313275510435,
0.260679509571009,0.26120622208671,0.261290799359835,0.26190795536125,0.262358765504495,
0.262525048300564,0.262525111362665,0.262853849358093,0.262879005814513),
 .UNSPECIFIED.);
#806=B_SPLINE_CURVE_WITH_KNOTS('',3,(#63479,#63480,#63481,#63482,#63483,
#63484,#63485,#63486,#63487,#63488,#63489,#63490,#63491,#63492,#63493,#63494,
#63495,#63496,#63497,#63498,#63499,#63500,#63501,#63502,#63503,#63504,#63505,
#63506,#63507,#63508,#63509,#63510,#63511,#63512,#63513,#63514,#63515,#63516,
#63517,#63518,#63519,#63520,#63521,#63522,#63523,#63524,#63525,#63526,#63527,
#63528,#63529,#63530,#63531,#63532,#63533,#63534,#63535,#63536,#63537,#63538,
#63539,#63540,#63541,#63542,#63543,#63544,#63545,#63546,#63547,#63548,#63549,
#63550,#63551,#63552,#63553,#63554,#63555,#63556,#63557,#63558,#63559,#63560,
#63561,#63562,#63563,#63564,#63565,#63566,#63567,#63568,#63569,#63570,#63571,
#63572,#63573,#63574,#63575,#63576,#63577,#63578,#63579,#63580,#63581,#63582,
#63583,#63584,#63585,#63586,#63587,#63588,#63589,#63590,#63591,#63592,#63593,
#63594,#63595,#63596,#63597,#63598,#63599,#63600,#63601,#63602,#63603,#63604,
#63605,#63606,#63607,#63608,#63609,#63610,#63611,#63612,#63613,#63614,#63615,
#63616,#63617,#63618,#63619,#63620,#63621,#63622,#63623,#63624,#63625,#63626,
#63627,#63628,#63629,#63630,#63631,#63632,#63633,#63634,#63635,#63636,#63637,
#63638,#63639,#63640,#63641,#63642,#63643,#63644,#63645,#63646,#63647,#63648,
#63649,#63650,#63651,#63652,#63653,#63654,#63655,#63656,#63657,#63658,#63659,
#63660,#63661,#63662,#63663,#63664,#63665,#63666,#63667,#63668,#63669,#63670,
#63671,#63672,#63673,#63674,#63675,#63676,#63677,#63678,#63679,#63680,#63681,
#63682,#63683,#63684,#63685,#63686,#63687,#63688,#63689,#63690,#63691,#63692,
#63693,#63694,#63695,#63696,#63697,#63698,#63699,#63700,#63701,#63702,#63703,
#63704,#63705,#63706,#63707,#63708,#63709,#63710,#63711,#63712,#63713,#63714,
#63715,#63716,#63717,#63718,#63719,#63720,#63721,#63722,#63723,#63724,#63725,
#63726,#63727,#63728,#63729,#63730,#63731,#63732,#63733,#63734,#63735,#63736,
#63737,#63738,#63739,#63740,#63741,#63742,#63743,#63744,#63745,#63746,#63747,
#63748,#63749,#63750,#63751,#63752,#63753,#63754,#63755,#63756,#63757,#63758,
#63759,#63760,#63761,#63762,#63763,#63764,#63765,#63766,#63767,#63768,#63769,
#63770,#63771,#63772,#63773,#63774,#63775,#63776,#63777,#63778,#63779,#63780,
#63781,#63782,#63783,#63784,#63785,#63786,#63787,#63788,#63789,#63790,#63791,
#63792,#63793,#63794,#63795,#63796,#63797,#63798,#63799,#63800,#63801,#63802,
#63803,#63804,#63805,#63806,#63807,#63808,#63809,#63810,#63811,#63812,#63813,
#63814,#63815,#63816,#63817,#63818,#63819,#63820,#63821,#63822,#63823,#63824,
#63825,#63826,#63827,#63828,#63829,#63830,#63831,#63832,#63833,#63834,#63835,
#63836,#63837,#63838,#63839,#63840,#63841,#63842,#63843,#63844,#63845,#63846,
#63847,#63848,#63849,#63850,#63851,#63852,#63853,#63854,#63855,#63856,#63857,
#63858,#63859,#63860,#63861,#63862,#63863,#63864,#63865,#63866,#63867,#63868,
#63869,#63870,#63871,#63872,#63873,#63874,#63875,#63876,#63877,#63878,#63879,
#63880,#63881,#63882,#63883,#63884,#63885,#63886,#63887,#63888,#63889,#63890,
#63891,#63892,#63893,#63894,#63895,#63896,#63897,#63898,#63899,#63900,#63901,
#63902,#63903,#63904,#63905,#63906,#63907,#63908,#63909,#63910,#63911,#63912,
#63913,#63914,#63915,#63916,#63917,#63918,#63919,#63920,#63921,#63922,#63923,
#63924,#63925,#63926,#63927,#63928,#63929,#63930,#63931,#63932,#63933,#63934,
#63935,#63936,#63937,#63938,#63939,#63940,#63941,#63942,#63943,#63944,#63945,
#63946,#63947,#63948,#63949,#63950,#63951,#63952,#63953,#63954,#63955,#63956,
#63957,#63958,#63959,#63960,#63961,#63962,#63963,#63964,#63965,#63966,#63967,
#63968,#63969,#63970,#63971,#63972,#63973,#63974,#63975,#63976,#63977,#63978,
#63979,#63980,#63981,#63982,#63983,#63984,#63985,#63986,#63987,#63988,#63989,
#63990,#63991,#63992,#63993,#63994,#63995,#63996,#63997,#63998,#63999,#64000,
#64001,#64002,#64003,#64004,#64005,#64006,#64007,#64008,#64009,#64010,#64011,
#64012,#64013,#64014,#64015,#64016,#64017,#64018,#64019,#64020,#64021,#64022,
#64023,#64024,#64025,#64026,#64027,#64028,#64029,#64030,#64031,#64032,#64033,
#64034,#64035,#64036,#64037,#64038,#64039,#64040,#64041,#64042,#64043,#64044,
#64045,#64046,#64047,#64048,#64049,#64050,#64051,#64052,#64053,#64054,#64055),
 .UNSPECIFIED.,.F.,.F.,(4,3,3,3,3,3,3,3,3,3,3,3,3,3,3,3,3,3,3,3,3,3,3,3,
3,3,3,3,3,3,3,3,3,3,3,3,3,3,3,3,3,3,3,3,3,3,3,3,3,3,3,3,3,3,3,3,3,3,3,3,
3,3,3,3,3,3,3,3,3,3,3,3,3,3,3,3,3,3,3,3,3,3,3,3,3,3,3,3,3,3,3,3,3,3,3,3,
3,3,3,3,3,3,3,3,3,3,3,3,3,3,3,3,3,3,3,3,3,3,3,3,3,3,3,3,3,3,3,3,3,3,3,3,
3,3,3,3,3,3,3,3,3,3,3,3,3,3,3,3,3,3,3,3,3,3,3,3,3,3,3,3,3,3,3,3,3,3,3,3,
3,3,3,3,3,3,3,3,3,3,3,3,3,3,3,3,3,3,3,3,3,3,3,3,4),(0.351267156365414,0.351750391359728,
0.352053768574433,0.352534925272286,0.353021590178722,0.35349882735455,
0.353754974599999,0.35425310170779,0.354784707541866,0.355327216319465,
0.355864800511277,0.356243289735703,0.35645105803837,0.357343280142757,
0.358206061509809,0.358651247070275,0.358731604871407,0.359324925451463,
0.359931723984194,0.360527984817262,0.360850748009482,0.361219920007111,
0.361806003340944,0.362428787462243,0.363051571583543,0.363659465672652,
0.363708235142815,0.364198446345135,0.364681457285473,0.364952392710666,
0.365253537864432,0.365725044071475,0.366196550278518,0.366758624783651,
0.367333348044981,0.367454340554546,0.36803001293294,0.368601585530452,
0.368684865414222,0.36924531748377,0.369654410669678,0.369929022982074,
0.370461401312978,0.371012766981758,0.371173180549926,0.371682892872077,
0.37185357714997,0.372365561697048,0.372832057307062,0.373475163656902,
0.37405258729195,0.374490934064198,0.375138184729189,0.3757916587624,0.376149810821334,
0.376251494518407,0.376800852830691,0.377350204648083,0.37780868757847,
0.378293420562503,0.378449369799278,0.378958467067442,0.379467564335606,
0.380028116995775,0.380577279044258,0.381126441092742,0.381382977762748,
0.381946259261549,0.382501112798003,0.382785317849878,0.383390635373774,
0.383975894741936,0.384315038402458,0.384444194607014,0.385016831019777,
0.385273632985582,0.385736697642693,0.38610307136415,0.386594706101067,
0.387084931607747,0.387249534242943,0.387734703639615,0.387761948121286,
0.388282278030875,0.388811554714553,0.389330608847941,0.389420824878422,
0.389861750321648,0.390181517755373,0.390630609695465,0.391079701635558,
0.391568863820643,0.392061173207715,0.392538953584999,0.392738578392693,
0.39311567715121,0.393567869297984,0.394020621172992,0.394397455149829,
0.394848055603842,0.395296854174968,0.395737074251576,0.396048735953485,
0.396056331906965,0.396496321886107,0.396935932582208,0.397371685468723,
0.397715208664101,0.398101041883674,0.398483464171324,0.398821126502192,
0.398982064711357,0.39933496660133,0.399686788844184,0.399927044340283,
0.400380681565484,0.400836075142965,0.401289973659049,0.401737212312914,
0.401916265365166,0.402138880016464,0.402645572315188,0.403166490416785,
0.403682641320516,0.404187093648233,0.404350715692645,0.404850487385546,
0.405362632432205,0.405877181689164,0.406009592449781,0.406315536957987,
0.407119550268592,0.407668469206917,0.407781616513089,0.40828507633214,
0.408806211148097,0.409327345964053,0.40973700362179,0.409981450776902,
0.410225887810325,0.410772422439078,0.410986222721189,0.411540821737823,
0.41169281377135,0.412247864394274,0.412645099478325,0.413172611534843,
0.413648463917508,0.41417165474335,0.414303976235461,0.414797132526775,
0.415133414614029,0.41552667033309,0.415849135458713,0.415962852992597,
0.416378061007014,0.416792291371165,0.417484374377118,0.417621729749733,
0.418049547352951,0.418497188898418,0.4189463751368,0.419280606506868,0.419776608752345,
0.420248109372826,0.420741112431842,0.420939483264004,0.421367394376181,
0.421797032915755,0.422227524743399,0.422447519620171,0.42259836002114,
0.42309112946944,0.423585109863308,0.424076779760356,0.424257236778276,
0.424647136307702,0.425151048627296,0.425657100548399,0.426163649110633,
0.426469072454458,0.426846990838846,0.42737415954416,0.427904473124376,
0.428435378236698,0.428680908130639,0.429046510090048,0.429582357542127,
0.430121732722553,0.430661132028704,0.43089274380682,0.431217811560911,
0.431246327079438),.UNSPECIFIED.);
#807=B_SPLINE_CURVE_WITH_KNOTS('',3,(#64400,#64401,#64402,#64403,#64404,
#64405,#64406,#64407,#64408,#64409,#64410,#64411,#64412,#64413,#64414,#64415,
#64416,#64417,#64418,#64419,#64420,#64421,#64422,#64423,#64424,#64425,#64426,
#64427,#64428,#64429,#64430,#64431,#64432,#64433,#64434,#64435,#64436,#64437,
#64438,#64439,#64440,#64441,#64442,#64443,#64444,#64445,#64446,#64447,#64448,
#64449,#64450,#64451,#64452,#64453,#64454,#64455,#64456,#64457,#64458,#64459,
#64460,#64461,#64462,#64463,#64464,#64465,#64466,#64467,#64468,#64469,#64470,
#64471,#64472,#64473,#64474,#64475,#64476,#64477,#64478,#64479,#64480,#64481,
#64482,#64483,#64484,#64485,#64486,#64487,#64488,#64489,#64490,#64491,#64492,
#64493,#64494,#64495,#64496,#64497,#64498,#64499,#64500,#64501,#64502,#64503,
#64504,#64505,#64506,#64507,#64508,#64509,#64510,#64511,#64512,#64513,#64514,
#64515,#64516,#64517,#64518,#64519,#64520,#64521,#64522,#64523,#64524,#64525,
#64526,#64527,#64528,#64529,#64530,#64531,#64532,#64533,#64534,#64535,#64536,
#64537,#64538,#64539,#64540,#64541,#64542,#64543,#64544,#64545,#64546,#64547,
#64548,#64549,#64550,#64551,#64552,#64553,#64554,#64555,#64556,#64557,#64558,
#64559,#64560,#64561,#64562,#64563,#64564,#64565,#64566,#64567,#64568,#64569,
#64570,#64571,#64572,#64573,#64574,#64575,#64576,#64577,#64578,#64579,#64580,
#64581,#64582,#64583,#64584,#64585,#64586,#64587,#64588,#64589,#64590,#64591,
#64592,#64593,#64594,#64595,#64596,#64597,#64598,#64599,#64600,#64601,#64602,
#64603,#64604,#64605,#64606,#64607,#64608,#64609,#64610,#64611,#64612,#64613,
#64614,#64615,#64616,#64617,#64618,#64619,#64620,#64621,#64622,#64623,#64624,
#64625,#64626,#64627,#64628,#64629,#64630,#64631,#64632,#64633,#64634,#64635,
#64636,#64637,#64638,#64639,#64640,#64641,#64642,#64643,#64644,#64645,#64646,
#64647,#64648,#64649,#64650,#64651,#64652,#64653,#64654,#64655,#64656,#64657,
#64658,#64659,#64660,#64661,#64662,#64663,#64664,#64665,#64666,#64667,#64668,
#64669,#64670,#64671,#64672,#64673,#64674,#64675,#64676,#64677,#64678,#64679,
#64680,#64681,#64682,#64683,#64684,#64685,#64686,#64687,#64688,#64689,#64690,
#64691,#64692,#64693,#64694,#64695,#64696,#64697,#64698,#64699,#64700,#64701,
#64702,#64703,#64704,#64705,#64706,#64707,#64708,#64709,#64710,#64711,#64712,
#64713,#64714,#64715,#64716,#64717,#64718,#64719,#64720,#64721,#64722,#64723,
#64724,#64725,#64726,#64727,#64728,#64729,#64730,#64731,#64732,#64733,#64734,
#64735,#64736,#64737,#64738,#64739,#64740,#64741,#64742,#64743,#64744,#64745,
#64746,#64747,#64748,#64749,#64750,#64751,#64752,#64753,#64754,#64755,#64756,
#64757,#64758,#64759,#64760,#64761,#64762,#64763,#64764,#64765,#64766,#64767,
#64768,#64769,#64770,#64771,#64772,#64773,#64774,#64775,#64776,#64777,#64778,
#64779,#64780,#64781,#64782,#64783,#64784,#64785,#64786,#64787,#64788,#64789,
#64790,#64791,#64792,#64793,#64794,#64795,#64796,#64797,#64798,#64799,#64800,
#64801,#64802,#64803,#64804,#64805,#64806,#64807,#64808,#64809,#64810,#64811,
#64812,#64813,#64814,#64815,#64816,#64817,#64818,#64819,#64820,#64821,#64822,
#64823,#64824,#64825,#64826,#64827,#64828,#64829,#64830,#64831,#64832,#64833,
#64834,#64835,#64836,#64837,#64838,#64839,#64840,#64841,#64842,#64843,#64844,
#64845,#64846,#64847,#64848,#64849,#64850,#64851,#64852,#64853,#64854,#64855,
#64856,#64857,#64858,#64859,#64860,#64861,#64862,#64863,#64864,#64865,#64866,
#64867,#64868,#64869,#64870,#64871,#64872,#64873,#64874,#64875,#64876,#64877,
#64878,#64879,#64880,#64881,#64882,#64883,#64884,#64885,#64886,#64887,#64888,
#64889,#64890,#64891,#64892,#64893,#64894,#64895,#64896,#64897,#64898,#64899,
#64900,#64901,#64902,#64903,#64904,#64905,#64906,#64907,#64908,#64909,#64910,
#64911,#64912,#64913,#64914,#64915,#64916,#64917,#64918,#64919,#64920,#64921,
#64922,#64923,#64924,#64925,#64926,#64927,#64928,#64929,#64930,#64931,#64932,
#64933,#64934,#64935,#64936,#64937,#64938,#64939,#64940,#64941,#64942,#64943,
#64944,#64945,#64946,#64947,#64948,#64949,#64950,#64951,#64952,#64953,#64954,
#64955,#64956,#64957,#64958,#64959,#64960,#64961,#64962,#64963,#64964,#64965,
#64966,#64967,#64968,#64969,#64970,#64971,#64972,#64973,#64974,#64975,#64976,
#64977,#64978,#64979,#64980,#64981,#64982,#64983,#64984,#64985,#64986,#64987,
#64988,#64989,#64990,#64991,#64992,#64993,#64994,#64995,#64996,#64997,#64998,
#64999,#65000,#65001,#65002,#65003,#65004,#65005,#65006,#65007,#65008,#65009,
#65010,#65011,#65012,#65013,#65014,#65015,#65016,#65017,#65018,#65019,#65020,
#65021,#65022,#65023,#65024,#65025,#65026,#65027,#65028,#65029,#65030,#65031,
#65032,#65033,#65034,#65035,#65036,#65037,#65038,#65039,#65040,#65041,#65042,
#65043,#65044,#65045,#65046,#65047,#65048,#65049,#65050,#65051,#65052,#65053,
#65054,#65055,#65056,#65057,#65058,#65059,#65060,#65061,#65062,#65063,#65064,
#65065,#65066,#65067,#65068,#65069,#65070,#65071,#65072,#65073,#65074,#65075,
#65076,#65077,#65078,#65079,#65080,#65081,#65082,#65083,#65084,#65085,#65086,
#65087,#65088,#65089,#65090,#65091,#65092,#65093,#65094,#65095,#65096,#65097,
#65098,#65099,#65100,#65101,#65102,#65103,#65104,#65105,#65106,#65107,#65108,
#65109,#65110,#65111,#65112,#65113,#65114,#65115,#65116,#65117,#65118,#65119,
#65120,#65121,#65122,#65123,#65124,#65125,#65126,#65127,#65128,#65129,#65130,
#65131,#65132,#65133,#65134,#65135,#65136,#65137,#65138,#65139,#65140,#65141,
#65142,#65143,#65144,#65145,#65146,#65147,#65148,#65149,#65150,#65151,#65152,
#65153,#65154,#65155,#65156,#65157,#65158,#65159,#65160,#65161,#65162,#65163,
#65164,#65165,#65166,#65167,#65168,#65169,#65170,#65171,#65172,#65173,#65174,
#65175,#65176,#65177,#65178,#65179,#65180,#65181,#65182,#65183,#65184,#65185,
#65186,#65187,#65188,#65189,#65190,#65191,#65192,#65193,#65194,#65195,#65196,
#65197,#65198,#65199,#65200,#65201,#65202,#65203,#65204,#65205,#65206,#65207,
#65208,#65209,#65210,#65211,#65212,#65213,#65214,#65215,#65216,#65217,#65218,
#65219,#65220,#65221,#65222,#65223,#65224,#65225,#65226,#65227,#65228,#65229,
#65230,#65231,#65232,#65233,#65234,#65235,#65236,#65237,#65238,#65239,#65240,
#65241,#65242,#65243,#65244,#65245,#65246,#65247,#65248,#65249,#65250,#65251,
#65252,#65253,#65254,#65255,#65256,#65257,#65258,#65259,#65260,#65261,#65262,
#65263,#65264,#65265,#65266,#65267,#65268,#65269,#65270,#65271,#65272,#65273,
#65274,#65275,#65276,#65277,#65278,#65279,#65280,#65281,#65282,#65283,#65284,
#65285,#65286,#65287,#65288,#65289,#65290,#65291,#65292,#65293,#65294,#65295,
#65296,#65297,#65298,#65299,#65300,#65301,#65302,#65303,#65304,#65305,#65306,
#65307,#65308,#65309,#65310,#65311,#65312,#65313,#65314,#65315,#65316,#65317,
#65318,#65319,#65320,#65321,#65322,#65323,#65324,#65325,#65326,#65327,#65328,
#65329,#65330,#65331,#65332,#65333,#65334,#65335,#65336,#65337,#65338,#65339,
#65340,#65341,#65342,#65343,#65344,#65345,#65346,#65347,#65348,#65349,#65350,
#65351,#65352,#65353,#65354,#65355,#65356,#65357,#65358,#65359,#65360,#65361,
#65362,#65363,#65364,#65365,#65366,#65367,#65368,#65369),.UNSPECIFIED.,
 .F.,.F.,(4,3,3,3,3,3,3,3,3,3,3,3,3,3,3,3,3,3,3,3,3,3,3,3,3,3,3,3,3,3,3,
3,3,3,3,3,3,3,3,3,3,3,3,3,3,3,3,3,3,3,3,3,3,3,3,3,3,3,3,3,3,3,3,3,3,3,3,
3,3,3,3,3,3,3,3,3,3,3,3,3,3,3,3,3,3,3,3,3,3,3,3,3,3,3,3,3,3,3,3,3,3,3,3,
3,3,3,3,3,3,3,3,3,3,3,3,3,3,3,3,3,3,3,3,3,3,3,3,3,3,3,3,3,3,3,3,3,3,3,3,
3,3,3,3,3,3,3,3,3,3,3,3,3,3,3,3,3,3,3,3,3,3,3,3,3,3,3,3,3,3,3,3,3,3,3,3,
3,3,3,3,3,3,3,3,3,3,3,3,3,3,3,3,3,3,3,3,3,3,3,3,3,3,3,3,3,3,3,3,3,3,3,3,
3,3,3,3,3,3,3,3,3,3,3,3,3,3,3,3,3,3,3,3,3,3,3,3,3,3,3,3,3,3,3,3,3,3,3,3,
3,3,3,3,3,3,3,3,3,3,3,3,3,3,3,3,3,3,3,3,3,3,3,3,3,3,3,3,3,3,3,3,3,3,3,3,
3,3,3,3,3,3,3,3,3,3,3,3,3,3,3,3,3,3,3,3,3,3,3,3,3,3,3,3,3,3,3,3,3,3,3,3,
3,3,3,3,4),(0.519634288272965,0.519685328699529,0.520064748915136,0.520317377395171,
0.52041882622757,0.520862629228728,0.521055598791493,0.521608503818973,
0.521683880116917,0.521949407569178,0.522103609227474,0.522122900721666,
0.522194625439873,0.522546034517934,0.522620445475116,0.523096346355821,
0.523177630920305,0.523660881144983,0.52374147215814,0.524221681230113,
0.524281202764036,0.524482495257025,0.524611230176765,0.524716416437288,
0.524820933369932,0.52536566976277,0.525453436385481,0.526106323961512,
0.526754869685056,0.527020889720284,0.527099233743331,0.527099277203579,
0.527582135112661,0.527757221295722,0.528314043234494,0.528430114927927,
0.528993375460614,0.529086167710458,0.529219959775975,0.529543895701582,
0.52958754890012,0.529587630937454,0.529977456891594,0.530156916054297,
0.530588309840476,0.530738497933387,0.531180168104028,0.531312507498718,
0.531418964631181,0.531746460164742,0.532002956712191,0.532075864056908,
0.532076060866791,0.532440903797139,0.53262808670734,0.533011517229871,
0.533190418858229,0.533577201788498,0.533618895324374,0.533955285664405,
0.534183375759633,0.534491968780854,0.534564179213697,0.534564531741459,
0.534874225454161,0.5350741437442,0.53541539953875,0.535592193256161,0.535819310443381,
0.536169477904769,0.536339628003893,0.536678131841218,0.536853677988387,
0.537052494370486,0.537052895108299,0.537405347814862,0.537608154053057,
0.537931950012464,0.538021099168023,0.538405583141743,0.538578329449285,
0.53895141665959,0.539138229913681,0.539496520171077,0.539540809527275,
0.539540988570634,0.539861663840644,0.540059301442978,0.540221061997415,
0.540602465762505,0.540736575089981,0.541102630644287,0.541180856588068,
0.541199557458666,0.541307545250463,0.541691361588774,0.541967913239337,
0.542356014405844,0.542419354920138,0.5427453555008,0.542858064226597,0.542945322977705,
0.543503914014392,0.543607680490904,0.54412414824012,0.54425799078739,0.544516855983004,
0.544517439840852,0.54461756988546,0.545052109445124,0.545442006868756,
0.545880174090394,0.546176087079588,0.546176316612045,0.546499735836316,
0.54667364546119,0.546815758868419,0.547186662019704,0.547325476125828,
0.547680850612868,0.547835182761928,0.547835193383237,0.548247442724799,
0.548422790618243,0.548664587179423,0.548664631768834,0.549013350718906,
0.549341372305563,0.54949407015443,0.549494225068885,0.550019243808671,
0.550479626932218,0.550539415922156,0.550964046420334,0.551033927493458,
0.551152905048832,0.551152946925622,0.551217046456726,0.551638420351807,
0.551907137251258,0.551982385311219,0.55198292810655,0.55239795763465,0.552605363661335,
0.552811823696815,0.552812789177049,0.553103236083438,0.553346610897895,
0.553617111751246,0.553887612604596,0.554148146967989,0.554540173762878,
0.554684868911349,0.555070009559826,0.555208905676705,0.555584558639431,
0.55561318736948,0.555918776435394,0.5561295772392,0.556129951812526,0.556417857233963,
0.556614544343955,0.556951756087017,0.557110879990134,0.557460926408367,
0.557611236045966,0.557815627826188,0.558170539705477,0.558316410385829,
0.55866373208175,0.558812915816199,0.559195892885701,0.559290662375238,
0.559395069100249,0.559447922497438,0.559783274014755,0.560018781254633,
0.560509613861431,0.560562494403706,0.561068870852784,0.561106207552778,
0.5611064241511,0.561570163349529,0.561613622761172,0.562110304428833,0.562218088325341,
0.562720821705787,0.56276508432397,0.562765506512604,0.563096386740074,
0.56335672413056,0.563751060238607,0.563955559845074,0.564343253512623,
0.564423125352024,0.564807306948141,0.565012225582776,0.565338252441909,
0.565595137789165,0.565937492527023,0.566082837866355,0.566083305223524,
0.566290558602028,0.566497870458405,0.56662436047434,0.566912276251951,
0.566912553185446,0.567351614620598,0.567741714637548,0.56774196785478,
0.568233190525925,0.568262889249545,0.568571153023144,0.568571203661145,
0.56882537837842,0.569239105243424,0.569287877949591,0.569400580543106,
0.569553117821054,0.570186121177483,0.57068515625277,0.571021295028928,
0.571059323946559,0.571219571436256,0.571778523153722,0.572328620057531,
0.57271816815427,0.572718344951125,0.57313602810784,0.573185294676041,0.573217271654526,
0.573684047634441,0.574096811422129,0.574151787876143,0.574377198662668,
0.574377221722318,0.574851542486652,0.575326375323,0.575795357182198,0.57603603375322,
0.57603609849351,0.576146419885079,0.57656190279015,0.576978136439357,0.577392543078506,
0.577694975264703,0.577695006938886,0.578087616610859,0.578188843009782,
0.578683381655279,0.579079581222031,0.579353816732127,0.579353852035895,
0.579747707031495,0.580148705440453,0.580549216095425,0.580946733847149,
0.581012698465323,0.581012728807088,0.581450019985727,0.581513943575523,
0.581989771834821,0.582015158343958,0.582489114392038,0.582671590517892,
0.58267160557828,0.583084254741761,0.583115660889144,0.583546735106938,
0.58366588366946,0.584114024632597,0.584216076115485,0.584330458037086,
0.584330482349473,0.584995793416719,0.585316469886586,0.585799041310968,
0.585989349773787,0.585989359120665,0.586417179063202,0.586879871687596,
0.587342969056041,0.58764821966101,0.587648235891858,0.588117971918786,
0.588144008688664,0.588617152903228,0.589110011816295,0.58930711266305,
0.589769585860652,0.589872824892581,0.59044241083114,0.590817402878396,
0.590965989434243,0.590966142307199,0.591531270699443,0.591606910100047,
0.592259975940435,0.592624866205435,0.592625013025626,0.593015942520109,
0.593574386378729,0.593823107660491,0.594309857022409,0.594626170563338,
0.594836701900359,0.594836877607622,0.595213571428038,0.595722866777785,
0.595849042762403,0.596440903702074,0.596475072270493,0.596892830512108,
0.597048490362349,0.597048537595282,0.597412222783684,0.597953152400304,
0.598042720995882,0.598682854065377,0.59914438845755,0.599260172474802,
0.599260373290205,0.599543077637962,0.599608753599983),.UNSPECIFIED.);
#808=B_SPLINE_CURVE_WITH_KNOTS('',3,(#65734,#65735,#65736,#65737,#65738,
#65739,#65740,#65741,#65742,#65743,#65744,#65745,#65746,#65747,#65748,#65749,
#65750,#65751,#65752,#65753,#65754,#65755,#65756,#65757,#65758,#65759,#65760,
#65761,#65762,#65763,#65764,#65765,#65766,#65767,#65768,#65769,#65770,#65771,
#65772,#65773,#65774,#65775,#65776,#65777,#65778,#65779,#65780,#65781,#65782,
#65783,#65784,#65785,#65786),.UNSPECIFIED.,.F.,.F.,(4,1,1,1,1,1,1,1,1,1,
1,1,1,1,1,1,1,1,1,1,1,1,1,1,1,1,1,1,1,1,1,1,1,1,1,1,1,1,1,1,1,1,1,1,1,1,
1,1,1,1,4),(0.688002641823372,0.690490227769403,0.692978542756553,0.695466857743702,
0.697955172730851,0.700443487718,0.702931802705149,0.705420117692299,0.707908432679448,
0.710120268223581,0.712332103767713,0.714543939311846,0.716202815969945,
0.717861692628045,0.719520569286144,0.721179445944244,0.722838322602343,
0.724497199260443,0.726156075918542,0.727814952576642,0.729473829234741,
0.731132705892841,0.73279158255094,0.73445045920904,0.736109335867139,0.737768212525239,
0.739427089183338,0.741085965841438,0.742191883613504,0.74329780138557,
0.745509636929703,0.747721472473835,0.749933308017968,0.752145143562101,
0.753251061334167,0.7538040202202,0.754080499663217,0.754356979106233,0.757674732422432,
0.759333609080532,0.760992485738631,0.761407204903156,0.761821924067681,
0.762651362396731,0.763480800725781,0.76431023905483,0.76513967738388,0.76596911571293,
0.766798554041979,0.767627992371029,0.767981201714498),.UNSPECIFIED.);
#809=B_SPLINE_CURVE_WITH_KNOTS('',3,(#67268,#67269,#67270,#67271,#67272,
#67273,#67274,#67275,#67276,#67277,#67278,#67279,#67280,#67281,#67282,#67283,
#67284,#67285,#67286,#67287,#67288,#67289,#67290,#67291,#67292,#67293,#67294,
#67295,#67296,#67297,#67298,#67299,#67300,#67301,#67302,#67303,#67304,#67305,
#67306,#67307,#67308,#67309,#67310,#67311,#67312,#67313,#67314,#67315,#67316,
#67317,#67318,#67319,#67320,#67321,#67322,#67323,#67324,#67325),
 .UNSPECIFIED.,.F.,.F.,(4,1,1,1,1,1,1,1,1,1,1,1,1,1,1,1,1,1,1,1,1,1,1,1,
1,1,1,1,1,1,1,1,1,1,1,1,1,1,1,1,1,1,1,1,1,1,1,1,1,1,1,1,1,1,1,4),(0.813159529437338,
0.815359014876381,0.817558857709555,0.819758700542729,0.821958543375904,
0.824158386209078,0.826358229042252,0.828558071875427,0.830757914708601,
0.832224476597384,0.833691038486167,0.83515760037495,0.835890881319341,
0.836624162263733,0.837357443208124,0.839557286041298,0.841757128874473,
0.843956971707647,0.846156814540821,0.848356657373996,0.85055650020717,
0.852756343040344,0.853856264456931,0.854956185873519,0.857156028706693,
0.857889309651084,0.858622590595476,0.859355871539867,0.860089152484259,
0.86082243342865,0.861555714373042,0.862655635789629,0.863755557206216,
0.864855478622803,0.86595540003939,0.868155242872565,0.870355085705739,
0.871821647594522,0.874754771372088,0.875854692788675,0.876954614205262,
0.879154457038436,0.880254378455023,0.880804339163317,0.881079319517464,
0.881354299871611,0.883554142704785,0.885753985537959,0.887953828371133,
0.890153671204308,0.892353514037482,0.89253683427358,0.892628494391629,
0.892720154509678,0.893086794981873,0.893448166194802),.UNSPECIFIED.);
#810=B_SPLINE_CURVE_WITH_KNOTS('',3,(#67678,#67679,#67680,#67681,#67682,
#67683,#67684,#67685,#67686,#67687,#67688,#67689,#67690,#67691,#67692,#67693,
#67694,#67695,#67696,#67697,#67698,#67699,#67700,#67701,#67702,#67703,#67704,
#67705,#67706,#67707,#67708,#67709,#67710,#67711,#67712,#67713,#67714,#67715,
#67716,#67717,#67718,#67719,#67720,#67721,#67722,#67723,#67724,#67725,#67726,
#67727,#67728,#67729,#67730,#67731,#67732,#67733,#67734,#67735,#67736,#67737,
#67738,#67739,#67740,#67741,#67742,#67743,#67744,#67745,#67746,#67747,#67748,
#67749,#67750,#67751,#67752,#67753,#67754,#67755,#67756,#67757,#67758,#67759,
#67760,#67761,#67762,#67763,#67764,#67765,#67766,#67767,#67768,#67769,#67770,
#67771,#67772,#67773,#67774,#67775,#67776,#67777,#67778,#67779,#67780,#67781,
#67782,#67783,#67784,#67785,#67786,#67787,#67788,#67789,#67790,#67791,#67792,
#67793,#67794,#67795,#67796,#67797,#67798,#67799,#67800,#67801,#67802,#67803,
#67804,#67805,#67806,#67807,#67808,#67809,#67810,#67811,#67812,#67813,#67814,
#67815,#67816,#67817,#67818,#67819,#67820,#67821,#67822,#67823,#67824,#67825,
#67826,#67827,#67828,#67829,#67830,#67831,#67832,#67833,#67834,#67835,#67836,
#67837,#67838,#67839,#67840,#67841,#67842,#67843,#67844,#67845,#67846,#67847,
#67848,#67849,#67850,#67851,#67852,#67853,#67854,#67855,#67856,#67857,#67858,
#67859,#67860,#67861,#67862,#67863,#67864,#67865,#67866,#67867,#67868,#67869,
#67870,#67871,#67872,#67873,#67874,#67875,#67876,#67877,#67878,#67879,#67880,
#67881,#67882,#67883,#67884,#67885,#67886,#67887,#67888,#67889,#67890,#67891,
#67892,#67893,#67894,#67895,#67896,#67897,#67898,#67899,#67900,#67901,#67902,
#67903,#67904,#67905,#67906,#67907,#67908,#67909,#67910,#67911,#67912,#67913,
#67914,#67915,#67916,#67917,#67918,#67919,#67920,#67921,#67922,#67923,#67924,
#67925,#67926,#67927,#67928,#67929,#67930,#67931,#67932,#67933,#67934,#67935,
#67936,#67937,#67938,#67939,#67940,#67941,#67942,#67943,#67944,#67945,#67946,
#67947,#67948,#67949,#67950,#67951,#67952,#67953,#67954,#67955,#67956,#67957,
#67958,#67959,#67960,#67961,#67962,#67963,#67964,#67965,#67966,#67967,#67968,
#67969,#67970,#67971,#67972,#67973,#67974,#67975,#67976,#67977,#67978,#67979,
#67980,#67981,#67982,#67983,#67984,#67985,#67986,#67987,#67988,#67989,#67990,
#67991,#67992,#67993,#67994,#67995,#67996,#67997,#67998,#67999,#68000,#68001,
#68002,#68003,#68004,#68005,#68006,#68007,#68008,#68009,#68010,#68011,#68012,
#68013,#68014,#68015,#68016,#68017,#68018,#68019,#68020,#68021,#68022,#68023,
#68024,#68025,#68026,#68027,#68028,#68029,#68030,#68031,#68032,#68033,#68034,
#68035,#68036,#68037,#68038,#68039,#68040,#68041,#68042,#68043,#68044,#68045,
#68046,#68047,#68048,#68049,#68050,#68051,#68052,#68053,#68054,#68055,#68056,
#68057,#68058,#68059,#68060,#68061,#68062,#68063,#68064,#68065,#68066,#68067,
#68068,#68069,#68070,#68071,#68072,#68073,#68074,#68075,#68076,#68077,#68078,
#68079,#68080,#68081,#68082,#68083,#68084,#68085,#68086,#68087,#68088,#68089,
#68090,#68091,#68092,#68093,#68094,#68095,#68096,#68097,#68098,#68099,#68100,
#68101,#68102,#68103,#68104,#68105,#68106,#68107,#68108,#68109,#68110,#68111,
#68112,#68113,#68114,#68115,#68116,#68117,#68118,#68119,#68120,#68121,#68122,
#68123,#68124,#68125,#68126,#68127,#68128,#68129,#68130,#68131,#68132,#68133,
#68134,#68135,#68136,#68137,#68138,#68139,#68140,#68141,#68142,#68143,#68144,
#68145,#68146,#68147,#68148,#68149,#68150,#68151,#68152,#68153,#68154,#68155,
#68156,#68157,#68158,#68159,#68160,#68161,#68162,#68163,#68164,#68165,#68166,
#68167,#68168,#68169,#68170,#68171,#68172,#68173,#68174,#68175,#68176,#68177,
#68178,#68179,#68180,#68181,#68182,#68183,#68184,#68185,#68186,#68187,#68188,
#68189,#68190,#68191,#68192,#68193,#68194,#68195,#68196,#68197,#68198,#68199,
#68200,#68201,#68202,#68203,#68204,#68205,#68206,#68207,#68208,#68209,#68210,
#68211,#68212,#68213,#68214,#68215,#68216,#68217,#68218,#68219,#68220,#68221,
#68222,#68223,#68224,#68225,#68226,#68227,#68228,#68229,#68230,#68231,#68232,
#68233,#68234,#68235,#68236,#68237,#68238,#68239,#68240,#68241,#68242,#68243,
#68244,#68245,#68246,#68247,#68248,#68249,#68250,#68251,#68252,#68253,#68254,
#68255,#68256,#68257,#68258,#68259,#68260,#68261,#68262,#68263,#68264,#68265,
#68266,#68267,#68268,#68269,#68270,#68271,#68272,#68273,#68274,#68275,#68276,
#68277,#68278,#68279,#68280,#68281,#68282,#68283,#68284,#68285,#68286,#68287,
#68288,#68289,#68290,#68291,#68292,#68293,#68294,#68295,#68296,#68297,#68298,
#68299,#68300,#68301,#68302,#68303,#68304,#68305,#68306,#68307,#68308,#68309,
#68310,#68311,#68312,#68313,#68314,#68315,#68316,#68317,#68318,#68319,#68320,
#68321,#68322,#68323,#68324,#68325,#68326,#68327,#68328,#68329,#68330,#68331,
#68332,#68333,#68334,#68335,#68336,#68337,#68338,#68339,#68340,#68341,#68342,
#68343,#68344,#68345,#68346,#68347,#68348,#68349,#68350,#68351,#68352,#68353,
#68354,#68355,#68356,#68357,#68358,#68359,#68360,#68361,#68362,#68363,#68364,
#68365,#68366,#68367,#68368,#68369,#68370,#68371,#68372,#68373,#68374,#68375,
#68376,#68377,#68378,#68379,#68380,#68381,#68382,#68383,#68384,#68385,#68386,
#68387,#68388,#68389,#68390,#68391,#68392,#68393,#68394,#68395,#68396,#68397,
#68398,#68399,#68400,#68401,#68402,#68403,#68404,#68405,#68406,#68407,#68408,
#68409,#68410,#68411,#68412,#68413,#68414,#68415,#68416,#68417,#68418,#68419,
#68420,#68421,#68422,#68423,#68424,#68425,#68426,#68427,#68428,#68429,#68430,
#68431,#68432,#68433,#68434,#68435,#68436,#68437,#68438,#68439,#68440,#68441,
#68442,#68443,#68444,#68445,#68446,#68447,#68448,#68449,#68450,#68451,#68452,
#68453,#68454,#68455,#68456,#68457,#68458,#68459,#68460,#68461,#68462,#68463,
#68464,#68465,#68466,#68467,#68468,#68469,#68470,#68471,#68472,#68473,#68474,
#68475,#68476,#68477,#68478,#68479,#68480,#68481,#68482,#68483,#68484,#68485,
#68486,#68487,#68488,#68489,#68490,#68491,#68492,#68493,#68494,#68495,#68496,
#68497,#68498,#68499,#68500,#68501,#68502,#68503,#68504,#68505,#68506,#68507,
#68508,#68509,#68510,#68511,#68512,#68513,#68514,#68515,#68516,#68517,#68518,
#68519,#68520,#68521,#68522,#68523,#68524,#68525,#68526,#68527,#68528,#68529,
#68530,#68531,#68532,#68533,#68534,#68535,#68536,#68537,#68538,#68539,#68540,
#68541,#68542,#68543,#68544,#68545,#68546,#68547,#68548,#68549,#68550,#68551,
#68552,#68553,#68554,#68555,#68556,#68557,#68558,#68559,#68560,#68561,#68562,
#68563,#68564,#68565,#68566,#68567,#68568,#68569,#68570,#68571,#68572,#68573,
#68574,#68575,#68576,#68577,#68578,#68579,#68580,#68581,#68582,#68583,#68584,
#68585,#68586,#68587,#68588,#68589,#68590,#68591,#68592,#68593,#68594,#68595,
#68596,#68597,#68598,#68599,#68600,#68601,#68602,#68603,#68604,#68605,#68606,
#68607,#68608,#68609,#68610,#68611,#68612,#68613,#68614,#68615,#68616,#68617,
#68618,#68619,#68620,#68621,#68622,#68623,#68624,#68625,#68626,#68627,#68628,
#68629,#68630,#68631,#68632,#68633,#68634,#68635,#68636,#68637,#68638,#68639,
#68640,#68641,#68642,#68643,#68644),.UNSPECIFIED.,.F.,.F.,(4,3,3,3,3,3,
3,3,3,3,3,3,3,3,3,3,3,3,3,3,3,3,3,3,3,3,3,3,3,3,3,3,3,3,3,3,3,3,3,3,3,3,
3,3,3,3,3,3,3,3,3,3,3,3,3,3,3,3,3,3,3,3,3,3,3,3,3,3,3,3,3,3,3,3,3,3,3,3,
3,3,3,3,3,3,3,3,3,3,3,3,3,3,3,3,3,3,3,3,3,3,3,3,3,3,3,3,3,3,3,3,3,3,3,3,
3,3,3,3,3,3,3,3,3,3,3,3,3,3,3,3,3,3,3,3,3,3,3,3,3,3,3,3,3,3,3,3,3,3,3,3,
3,3,3,3,3,3,3,3,3,3,3,3,3,3,3,3,3,3,3,3,3,3,3,3,3,3,3,3,3,3,3,3,3,3,3,3,
3,3,3,3,3,3,3,3,3,3,3,3,3,3,3,3,3,3,3,3,3,3,3,3,3,3,3,3,3,3,3,3,3,3,3,3,
3,3,3,3,3,3,3,3,3,3,3,3,3,3,3,3,3,3,3,3,3,3,3,3,3,3,3,3,3,3,3,3,3,3,3,3,
3,3,3,3,3,3,3,3,3,3,3,3,3,3,3,3,3,3,3,3,3,3,3,3,3,3,3,3,3,3,3,3,3,3,3,3,
3,3,3,3,3,3,3,3,3,3,3,3,3,3,3,3,3,3,3,3,3,3,3,3,3,3,3,3,4),(0.856370509464718,
0.856739710126176,0.856941604650561,0.857157463028789,0.857728097172609,
0.857889710219808,0.858455007199432,0.858622556190436,0.858856880166661,
0.858856990877825,0.859220635558683,0.859356155617663,0.859900245426217,
0.86008841202652,0.86059414452884,0.860635206101866,0.860820640290637,0.861206260844417,
0.861344429784462,0.861344437291952,0.861554210482135,0.862000485740877,
0.862124540013047,0.862595676556938,0.862653396798758,0.863116747727199,
0.863224409502402,0.863651619529005,0.863752914872577,0.86383188370608,
0.863832010953973,0.864231153625413,0.864379515660299,0.864812069623318,
0.864852826667762,0.865403258519047,0.865808793566429,0.865952319957288,
0.866319330120207,0.866319743320668,0.866688117823291,0.866898517600103,
0.86730618182318,0.867526014023919,0.867925662148695,0.868121848041472,
0.868153510447734,0.868543579726341,0.868757896298623,0.868806776534335,
0.8688072293163,0.869207754885257,0.869618033069385,0.869669922765494,0.870017419969291,
0.870355051628635,0.870732516059687,0.871089200032129,0.87125701384248,
0.871294268262353,0.871360824031647,0.871683079267071,0.871823348435623,
0.872156731118901,0.872283865069682,0.872537946155526,0.87253825597237,
0.873069937605435,0.873548261234971,0.873763600880015,0.87378166936259,
0.873781779373382,0.87408481375249,0.874210878426716,0.874545716993315,
0.874633113921817,0.874753735812206,0.875024584111161,0.875025392569654,
0.875384898969503,0.875447491540601,0.875827691453192,0.875853867950656,
0.876268869897062,0.876269115776718,0.876585265584936,0.876774748855083,
0.876953119288411,0.877343592214753,0.877458393130804,0.877831111513812,
0.877969286193373,0.87840678928135,0.878480179255942,0.878480344993447,
0.87879194090105,0.87910295087439,0.87915231397627,0.879584531980476,0.879802996579847,
0.880111835486817,0.880252435165722,0.880691242735167,0.880691684404755,
0.881074207456304,0.881332551760943,0.881692354816355,0.88201939931933,
0.88246085276686,0.882712790984588,0.882902306214391,0.882903292719097,
0.883209674962912,0.883397627564955,0.883556714133813,0.884042481261811,
0.884544402441087,0.88504328705427,0.885523235920033,0.885724698943558,
0.885752508450121,0.88612212093931,0.886218901433228,0.886219625571857,
0.886537647333598,0.886707761785872,0.886974326236772,0.887211981951545,
0.887551235931704,0.887729114878847,0.8879560400736,0.888300204156477,0.888473221575917,
0.88878646732094,0.889004359113991,0.88928438686396,0.889504870756455,0.889536078306289,
0.889900762160951,0.890116587626518,0.890603106978639,0.891062191854129,
0.891193794261483,0.891194106502742,0.891732405714557,0.891943414975812,
0.89235407755958,0.892537660293242,0.892629451947967,0.892721242487384,
0.892852091870902,0.892852276487536,0.893088279783021,0.893510409052143,
0.893658802645668,0.893821329466465,0.894211435057065,0.894393765759537,
0.89451038948032,0.894510493238327,0.894901352996297,0.895287599092038,
0.895702170859857,0.896103458643209,0.896168687089739,0.896168712319676,
0.896567659105487,0.896754419127474,0.896997800787915,0.896997835894448,
0.897496487037925,0.89772245833648,0.897826936126778,0.897992419076711,
0.898220722714388,0.898769754683305,0.898953707057181,0.899136939501272,
0.899320178893095,0.89948519444784,0.899686677582514,0.90005314101267,0.900314329369707,
0.900419642490131,0.900898645228698,0.901143479480045,0.901152743988307,
0.901492719454058,0.901558081566027,0.901724949122927,0.901972666219304,
0.901972728722703,0.902351164518496,0.902618371808164,0.902801875181428,
0.902801877527412,0.903171552794411,0.903540854898999,0.903952120779196,
0.904084917817704,0.904590636256751,0.904832418839058,0.905379797910794,
0.905550697078066,0.905900919943512,0.906118472746249,0.9061185171396,0.906468240531146,
0.906816938564654,0.906947604592874,0.906947621550958,0.907017340702522,
0.907399284623962,0.907776770355667,0.907776802867114,0.908241313754553,
0.90828552324162,0.908484350706353,0.908990207617589,0.909435067965086,
0.909435144078441,0.90985913862168,0.909951279775271,0.910614001596101,
0.911269042084864,0.911417756555064,0.91164613144431,0.911646157495504,
0.912099113248859,0.912191784393921,0.912742716916304,0.912884559760023,
0.9134021509074,0.913433410843006,0.913819002254019,0.913857194923535,0.913857288302221,
0.914285977812487,0.914418745168495,0.914842047306868,0.915401504308667,
0.915841264194839,0.91595605892196,0.916068258402759,0.91606831730272,0.916453159009049,
0.916798645433519,0.917173790142372,0.917173828804338,0.917622268037278,
0.917776470821123,0.918223528974704,0.918279321881984,0.91827938061333,
0.918754802595467,0.919295871548816,0.919404876537645,0.919964840577214,
0.920059693976517,0.920490385361208,0.920490495469795,0.920953807375547,
0.921500637114346,0.921647287968573,0.922154668126846,0.922333425482766,
0.922701448840433,0.922701525067417,0.923152318153573,0.923698348353999,
0.924166610876225,0.92424665199397,0.924359746449851,0.924359806127616,
0.924837979949728,0.924908244107517,0.925350209741723,0.925896246655443,
0.92601804405927,0.926018077499045,0.926511614483731,0.926685236328919,
0.927275246146838,0.927365910698766,0.92754902089914,0.927676341668688,
0.927676408620273,0.928236970237227,0.928804914273471,0.929334624595944,
0.929334639278107,0.929748496617437,0.930163740203712,0.930163788082816,
0.93058891693644,0.930992811539352,0.930992936887525,0.93140751128988,0.931822021399953,
0.931822085692234,0.931948840165757,0.932345748446948,0.932651066673402,
0.932651234496943,0.933065609618207,0.933065808899298,0.933480208305583,
0.933480383301653,0.933883400287811,0.934150258990416,0.934309417204156,
0.934309532106362,0.934724106508717,0.935138461211252,0.935138680911071,
0.935476768984967,0.935553064830452,0.935553255313426,0.935848405917604,
0.935967680546784,0.93596782971578,0.936254160901786,0.936350378361133),
 .UNSPECIFIED.);
#811=B_SPLINE_CURVE_WITH_KNOTS('',3,(#69014,#69015,#69016,#69017,#69018,
#69019),.UNSPECIFIED.,.F.,.F.,(4,2,4),(0.398092128061379,0.409976953644022,
0.468547233706402),.UNSPECIFIED.);
#812=B_SPLINE_CURVE_WITH_KNOTS('',3,(#69025,#69026,#69027,#69028,#69029,
#69030),.UNSPECIFIED.,.F.,.F.,(4,2,4),(0.254795220936954,0.292840145217421,
0.33426586804347),.UNSPECIFIED.);
#813=B_SPLINE_CURVE_WITH_KNOTS('',3,(#69036,#69037,#69038,#69039,#69040,
#69041),.UNSPECIFIED.,.F.,.F.,(4,2,4),(0.134281365662929,0.17570708848898,
0.213752012769447),.UNSPECIFIED.);
#814=B_SPLINE_CURVE_WITH_KNOTS('',3,(#69047,#69048,#69049,#69050,#69051,
#69052,#69053,#69054,#69055,#69056,#69057),.UNSPECIFIED.,.F.,.F.,(4,2,3,
2,4),(0.86663936176778,0.878524187350423,0.937094467412803,0.995664747475183,
1.00754957305783),.UNSPECIFIED.);
#815=B_SPLINE_CURVE_WITH_KNOTS('',3,(#69063,#69064,#69065,#69066,#69067,
#69068),.UNSPECIFIED.,.F.,.F.,(4,2,4),(0.723342454643356,0.761387378923823,
0.802813101749872),.UNSPECIFIED.);
#816=B_SPLINE_CURVE_WITH_KNOTS('',3,(#69074,#69075,#69076,#69077,#69078,
#69079),.UNSPECIFIED.,.F.,.F.,(4,2,4),(0.602828599369333,0.644254322195382,
0.682299246475849),.UNSPECIFIED.);
#817=B_SPLINE_CURVE_WITH_KNOTS('',3,(#69084,#69085,#69086,#69087,#69088,
#69089),.UNSPECIFIED.,.F.,.F.,(4,2,4),(0.468547233706402,0.527117513768781,
0.539002339351426),.UNSPECIFIED.);
#818=B_SPLINE_CURVE_WITH_KNOTS('',3,(#69093,#69094,#69095,#69096,#69097,
#69098,#69099,#69100,#69101,#69102,#69103,#69104,#69105,#69106,#69107,#69108,
#69109,#69110,#69111,#69112,#69113,#69114),.UNSPECIFIED.,.F.,.F.,(4,2,2,
2,2,2,2,2,2,2,4),(-0.993641732162441,-0.962200652631669,-0.930759573100898,
-0.867877414039355,-0.806554356580593,-0.745231299121831,-0.683908241663068,
-0.622585184204306,-0.559703025142763,-0.528261945611992,-0.49682086608122),
 .UNSPECIFIED.);
#819=B_SPLINE_CURVE_WITH_KNOTS('',3,(#69115,#69116,#69117,#69118,#69119,
#69120,#69121,#69122,#69123,#69124,#69125,#69126,#69127,#69128,#69129,#69130,
#69131,#69132,#69133,#69134,#69135,#69136),.UNSPECIFIED.,.F.,.F.,(4,2,2,
2,2,2,2,2,2,2,4),(-0.49682086608122,-0.465379786550449,-0.433938707019678,
-0.371056547958135,-0.309733490499373,-0.24841043304061,-0.187087375581848,
-0.125764318123086,-0.0628821590615428,-0.0314410795307714,0.),
 .UNSPECIFIED.);
#820=B_SPLINE_CURVE_WITH_KNOTS('',2,(#69959,#69960,#69961),
 .UNSPECIFIED.,.F.,.F.,(3,3),(0.,1.),.UNSPECIFIED.);
#821=B_SPLINE_CURVE_WITH_KNOTS('',2,(#69965,#69966,#69967),
 .UNSPECIFIED.,.F.,.F.,(3,3),(0.,1.),.UNSPECIFIED.);
#822=B_SPLINE_CURVE_WITH_KNOTS('',2,(#69976,#69977,#69978),
 .UNSPECIFIED.,.F.,.F.,(3,3),(0.,1.),.UNSPECIFIED.);
#823=B_SPLINE_CURVE_WITH_KNOTS('',2,(#69981,#69982,#69983),
 .UNSPECIFIED.,.F.,.F.,(3,3),(0.,1.),.UNSPECIFIED.);
#824=B_SPLINE_CURVE_WITH_KNOTS('',2,(#69991,#69992,#69993),
 .UNSPECIFIED.,.F.,.F.,(3,3),(0.,1.),.UNSPECIFIED.);
#825=B_SPLINE_CURVE_WITH_KNOTS('',2,(#69996,#69997,#69998),
 .UNSPECIFIED.,.F.,.F.,(3,3),(0.,1.),.UNSPECIFIED.);
#826=B_SPLINE_CURVE_WITH_KNOTS('',2,(#70006,#70007,#70008),
 .UNSPECIFIED.,.F.,.F.,(3,3),(0.,1.),.UNSPECIFIED.);
#827=B_SPLINE_CURVE_WITH_KNOTS('',2,(#70011,#70012,#70013),
 .UNSPECIFIED.,.F.,.F.,(3,3),(0.,1.),.UNSPECIFIED.);
#828=B_SPLINE_CURVE_WITH_KNOTS('',2,(#70021,#70022,#70023),
 .UNSPECIFIED.,.F.,.F.,(3,3),(0.,1.),.UNSPECIFIED.);
#829=B_SPLINE_CURVE_WITH_KNOTS('',2,(#70026,#70027,#70028),
 .UNSPECIFIED.,.F.,.F.,(3,3),(0.,1.),.UNSPECIFIED.);
#830=B_SPLINE_CURVE_WITH_KNOTS('',2,(#70036,#70037,#70038),
 .UNSPECIFIED.,.F.,.F.,(3,3),(0.,1.),.UNSPECIFIED.);
#831=B_SPLINE_CURVE_WITH_KNOTS('',2,(#70041,#70042,#70043),
 .UNSPECIFIED.,.F.,.F.,(3,3),(0.,1.),.UNSPECIFIED.);
#832=B_SPLINE_CURVE_WITH_KNOTS('',2,(#70051,#70052,#70053),
 .UNSPECIFIED.,.F.,.F.,(3,3),(0.,1.),.UNSPECIFIED.);
#833=B_SPLINE_CURVE_WITH_KNOTS('',2,(#70056,#70057,#70058),
 .UNSPECIFIED.,.F.,.F.,(3,3),(0.,1.),.UNSPECIFIED.);
#834=B_SPLINE_CURVE_WITH_KNOTS('',2,(#70065,#70066,#70067),
 .UNSPECIFIED.,.F.,.F.,(3,3),(0.,1.),.UNSPECIFIED.);
#835=B_SPLINE_CURVE_WITH_KNOTS('',2,(#70068,#70069,#70070),
 .UNSPECIFIED.,.F.,.F.,(3,3),(0.,1.),.UNSPECIFIED.);
#836=B_SPLINE_CURVE_WITH_KNOTS('',2,(#70079,#70080,#70081),
 .UNSPECIFIED.,.F.,.F.,(3,3),(0.,1.),.UNSPECIFIED.);
#837=B_SPLINE_CURVE_WITH_KNOTS('',2,(#70085,#70086,#70087),
 .UNSPECIFIED.,.F.,.F.,(3,3),(0.,1.),.UNSPECIFIED.);
#838=B_SPLINE_CURVE_WITH_KNOTS('',2,(#70096,#70097,#70098),
 .UNSPECIFIED.,.F.,.F.,(3,3),(0.,1.),.UNSPECIFIED.);
#839=B_SPLINE_CURVE_WITH_KNOTS('',2,(#70101,#70102,#70103),
 .UNSPECIFIED.,.F.,.F.,(3,3),(0.,1.),.UNSPECIFIED.);
#840=B_SPLINE_CURVE_WITH_KNOTS('',2,(#70111,#70112,#70113),
 .UNSPECIFIED.,.F.,.F.,(3,3),(0.,1.),.UNSPECIFIED.);
#841=B_SPLINE_CURVE_WITH_KNOTS('',2,(#70116,#70117,#70118),
 .UNSPECIFIED.,.F.,.F.,(3,3),(0.,1.),.UNSPECIFIED.);
#842=B_SPLINE_CURVE_WITH_KNOTS('',2,(#70126,#70127,#70128),
 .UNSPECIFIED.,.F.,.F.,(3,3),(0.,1.),.UNSPECIFIED.);
#843=B_SPLINE_CURVE_WITH_KNOTS('',2,(#70131,#70132,#70133),
 .UNSPECIFIED.,.F.,.F.,(3,3),(0.,1.),.UNSPECIFIED.);
#844=B_SPLINE_CURVE_WITH_KNOTS('',2,(#70141,#70142,#70143),
 .UNSPECIFIED.,.F.,.F.,(3,3),(0.,1.),.UNSPECIFIED.);
#845=B_SPLINE_CURVE_WITH_KNOTS('',2,(#70146,#70147,#70148),
 .UNSPECIFIED.,.F.,.F.,(3,3),(0.,1.),.UNSPECIFIED.);
#846=B_SPLINE_CURVE_WITH_KNOTS('',2,(#70156,#70157,#70158),
 .UNSPECIFIED.,.F.,.F.,(3,3),(0.,1.),.UNSPECIFIED.);
#847=B_SPLINE_CURVE_WITH_KNOTS('',2,(#70161,#70162,#70163),
 .UNSPECIFIED.,.F.,.F.,(3,3),(0.,1.),.UNSPECIFIED.);
#848=B_SPLINE_CURVE_WITH_KNOTS('',2,(#70171,#70172,#70173),
 .UNSPECIFIED.,.F.,.F.,(3,3),(0.,1.),.UNSPECIFIED.);
#849=B_SPLINE_CURVE_WITH_KNOTS('',2,(#70176,#70177,#70178),
 .UNSPECIFIED.,.F.,.F.,(3,3),(0.,1.),.UNSPECIFIED.);
#850=B_SPLINE_CURVE_WITH_KNOTS('',2,(#70186,#70187,#70188),
 .UNSPECIFIED.,.F.,.F.,(3,3),(0.,1.),.UNSPECIFIED.);
#851=B_SPLINE_CURVE_WITH_KNOTS('',2,(#70191,#70192,#70193),
 .UNSPECIFIED.,.F.,.F.,(3,3),(0.,1.),.UNSPECIFIED.);
#852=B_SPLINE_CURVE_WITH_KNOTS('',2,(#70201,#70202,#70203),
 .UNSPECIFIED.,.F.,.F.,(3,3),(0.,1.),.UNSPECIFIED.);
#853=B_SPLINE_CURVE_WITH_KNOTS('',2,(#70206,#70207,#70208),
 .UNSPECIFIED.,.F.,.F.,(3,3),(0.,1.),.UNSPECIFIED.);
#854=B_SPLINE_CURVE_WITH_KNOTS('',2,(#70216,#70217,#70218),
 .UNSPECIFIED.,.F.,.F.,(3,3),(0.,1.),.UNSPECIFIED.);
#855=B_SPLINE_CURVE_WITH_KNOTS('',2,(#70221,#70222,#70223),
 .UNSPECIFIED.,.F.,.F.,(3,3),(0.,1.),.UNSPECIFIED.);
#856=B_SPLINE_CURVE_WITH_KNOTS('',2,(#70231,#70232,#70233),
 .UNSPECIFIED.,.F.,.F.,(3,3),(0.,1.),.UNSPECIFIED.);
#857=B_SPLINE_CURVE_WITH_KNOTS('',2,(#70236,#70237,#70238),
 .UNSPECIFIED.,.F.,.F.,(3,3),(0.,1.),.UNSPECIFIED.);
#858=B_SPLINE_CURVE_WITH_KNOTS('',2,(#70245,#70246,#70247),
 .UNSPECIFIED.,.F.,.F.,(3,3),(0.,1.),.UNSPECIFIED.);
#859=B_SPLINE_CURVE_WITH_KNOTS('',2,(#70248,#70249,#70250),
 .UNSPECIFIED.,.F.,.F.,(3,3),(0.,1.),.UNSPECIFIED.);
#860=B_SPLINE_CURVE_WITH_KNOTS('',2,(#70347,#70348,#70349),
 .UNSPECIFIED.,.F.,.F.,(3,3),(0.,1.),.UNSPECIFIED.);
#861=B_SPLINE_CURVE_WITH_KNOTS('',2,(#70353,#70354,#70355),
 .UNSPECIFIED.,.F.,.F.,(3,3),(0.,1.),.UNSPECIFIED.);
#862=B_SPLINE_CURVE_WITH_KNOTS('',2,(#70364,#70365,#70366),
 .UNSPECIFIED.,.F.,.F.,(3,3),(0.,1.),.UNSPECIFIED.);
#863=B_SPLINE_CURVE_WITH_KNOTS('',2,(#70369,#70370,#70371),
 .UNSPECIFIED.,.F.,.F.,(3,3),(0.,1.),.UNSPECIFIED.);
#864=B_SPLINE_CURVE_WITH_KNOTS('',2,(#70379,#70380,#70381),
 .UNSPECIFIED.,.F.,.F.,(3,3),(0.,1.),.UNSPECIFIED.);
#865=B_SPLINE_CURVE_WITH_KNOTS('',2,(#70384,#70385,#70386),
 .UNSPECIFIED.,.F.,.F.,(3,3),(0.,1.),.UNSPECIFIED.);
#866=B_SPLINE_CURVE_WITH_KNOTS('',2,(#70394,#70395,#70396),
 .UNSPECIFIED.,.F.,.F.,(3,3),(0.,1.),.UNSPECIFIED.);
#867=B_SPLINE_CURVE_WITH_KNOTS('',2,(#70399,#70400,#70401),
 .UNSPECIFIED.,.F.,.F.,(3,3),(0.,1.),.UNSPECIFIED.);
#868=B_SPLINE_CURVE_WITH_KNOTS('',2,(#70409,#70410,#70411),
 .UNSPECIFIED.,.F.,.F.,(3,3),(0.,1.),.UNSPECIFIED.);
#869=B_SPLINE_CURVE_WITH_KNOTS('',2,(#70414,#70415,#70416),
 .UNSPECIFIED.,.F.,.F.,(3,3),(0.,1.),.UNSPECIFIED.);
#870=B_SPLINE_CURVE_WITH_KNOTS('',2,(#70424,#70425,#70426),
 .UNSPECIFIED.,.F.,.F.,(3,3),(0.,1.),.UNSPECIFIED.);
#871=B_SPLINE_CURVE_WITH_KNOTS('',2,(#70429,#70430,#70431),
 .UNSPECIFIED.,.F.,.F.,(3,3),(0.,1.),.UNSPECIFIED.);
#872=B_SPLINE_CURVE_WITH_KNOTS('',2,(#70439,#70440,#70441),
 .UNSPECIFIED.,.F.,.F.,(3,3),(0.,1.),.UNSPECIFIED.);
#873=B_SPLINE_CURVE_WITH_KNOTS('',2,(#70444,#70445,#70446),
 .UNSPECIFIED.,.F.,.F.,(3,3),(0.,1.),.UNSPECIFIED.);
#874=B_SPLINE_CURVE_WITH_KNOTS('',2,(#70453,#70454,#70455),
 .UNSPECIFIED.,.F.,.F.,(3,3),(0.,1.),.UNSPECIFIED.);
#875=B_SPLINE_CURVE_WITH_KNOTS('',2,(#70456,#70457,#70458),
 .UNSPECIFIED.,.F.,.F.,(3,3),(0.,1.),.UNSPECIFIED.);
#876=B_SPLINE_CURVE_WITH_KNOTS('',2,(#70467,#70468,#70469),
 .UNSPECIFIED.,.F.,.F.,(3,3),(0.,1.),.UNSPECIFIED.);
#877=B_SPLINE_CURVE_WITH_KNOTS('',2,(#70473,#70474,#70475),
 .UNSPECIFIED.,.F.,.F.,(3,3),(0.,1.),.UNSPECIFIED.);
#878=B_SPLINE_CURVE_WITH_KNOTS('',2,(#70484,#70485,#70486),
 .UNSPECIFIED.,.F.,.F.,(3,3),(0.,1.),.UNSPECIFIED.);
#879=B_SPLINE_CURVE_WITH_KNOTS('',2,(#70489,#70490,#70491),
 .UNSPECIFIED.,.F.,.F.,(3,3),(0.,1.),.UNSPECIFIED.);
#880=B_SPLINE_CURVE_WITH_KNOTS('',2,(#70499,#70500,#70501),
 .UNSPECIFIED.,.F.,.F.,(3,3),(0.,1.),.UNSPECIFIED.);
#881=B_SPLINE_CURVE_WITH_KNOTS('',2,(#70504,#70505,#70506),
 .UNSPECIFIED.,.F.,.F.,(3,3),(0.,1.),.UNSPECIFIED.);
#882=B_SPLINE_CURVE_WITH_KNOTS('',2,(#70514,#70515,#70516),
 .UNSPECIFIED.,.F.,.F.,(3,3),(0.,1.),.UNSPECIFIED.);
#883=B_SPLINE_CURVE_WITH_KNOTS('',2,(#70519,#70520,#70521),
 .UNSPECIFIED.,.F.,.F.,(3,3),(0.,1.),.UNSPECIFIED.);
#884=B_SPLINE_CURVE_WITH_KNOTS('',2,(#70529,#70530,#70531),
 .UNSPECIFIED.,.F.,.F.,(3,3),(0.,1.),.UNSPECIFIED.);
#885=B_SPLINE_CURVE_WITH_KNOTS('',2,(#70534,#70535,#70536),
 .UNSPECIFIED.,.F.,.F.,(3,3),(0.,1.),.UNSPECIFIED.);
#886=B_SPLINE_CURVE_WITH_KNOTS('',2,(#70544,#70545,#70546),
 .UNSPECIFIED.,.F.,.F.,(3,3),(0.,1.),.UNSPECIFIED.);
#887=B_SPLINE_CURVE_WITH_KNOTS('',2,(#70549,#70550,#70551),
 .UNSPECIFIED.,.F.,.F.,(3,3),(0.,1.),.UNSPECIFIED.);
#888=B_SPLINE_CURVE_WITH_KNOTS('',2,(#70559,#70560,#70561),
 .UNSPECIFIED.,.F.,.F.,(3,3),(0.,1.),.UNSPECIFIED.);
#889=B_SPLINE_CURVE_WITH_KNOTS('',2,(#70564,#70565,#70566),
 .UNSPECIFIED.,.F.,.F.,(3,3),(0.,1.),.UNSPECIFIED.);
#890=B_SPLINE_CURVE_WITH_KNOTS('',2,(#70574,#70575,#70576),
 .UNSPECIFIED.,.F.,.F.,(3,3),(0.,1.),.UNSPECIFIED.);
#891=B_SPLINE_CURVE_WITH_KNOTS('',2,(#70579,#70580,#70581),
 .UNSPECIFIED.,.F.,.F.,(3,3),(0.,1.),.UNSPECIFIED.);
#892=B_SPLINE_CURVE_WITH_KNOTS('',2,(#70589,#70590,#70591),
 .UNSPECIFIED.,.F.,.F.,(3,3),(0.,1.),.UNSPECIFIED.);
#893=B_SPLINE_CURVE_WITH_KNOTS('',2,(#70594,#70595,#70596),
 .UNSPECIFIED.,.F.,.F.,(3,3),(0.,1.),.UNSPECIFIED.);
#894=B_SPLINE_CURVE_WITH_KNOTS('',2,(#70604,#70605,#70606),
 .UNSPECIFIED.,.F.,.F.,(3,3),(0.,1.),.UNSPECIFIED.);
#895=B_SPLINE_CURVE_WITH_KNOTS('',2,(#70609,#70610,#70611),
 .UNSPECIFIED.,.F.,.F.,(3,3),(0.,1.),.UNSPECIFIED.);
#896=B_SPLINE_CURVE_WITH_KNOTS('',2,(#70619,#70620,#70621),
 .UNSPECIFIED.,.F.,.F.,(3,3),(0.,1.),.UNSPECIFIED.);
#897=B_SPLINE_CURVE_WITH_KNOTS('',2,(#70624,#70625,#70626),
 .UNSPECIFIED.,.F.,.F.,(3,3),(0.,1.),.UNSPECIFIED.);
#898=B_SPLINE_CURVE_WITH_KNOTS('',2,(#70633,#70634,#70635),
 .UNSPECIFIED.,.F.,.F.,(3,3),(0.,1.),.UNSPECIFIED.);
#899=B_SPLINE_CURVE_WITH_KNOTS('',2,(#70636,#70637,#70638),
 .UNSPECIFIED.,.F.,.F.,(3,3),(0.,1.),.UNSPECIFIED.);
#900=B_SPLINE_CURVE_WITH_KNOTS('',2,(#70648,#70649,#70650),
 .UNSPECIFIED.,.F.,.F.,(3,3),(0.,1.),.UNSPECIFIED.);
#901=B_SPLINE_CURVE_WITH_KNOTS('',2,(#70654,#70655,#70656),
 .UNSPECIFIED.,.F.,.F.,(3,3),(0.,1.),.UNSPECIFIED.);
#902=B_SPLINE_CURVE_WITH_KNOTS('',2,(#70665,#70666,#70667),
 .UNSPECIFIED.,.F.,.F.,(3,3),(0.,1.),.UNSPECIFIED.);
#903=B_SPLINE_CURVE_WITH_KNOTS('',2,(#70670,#70671,#70672),
 .UNSPECIFIED.,.F.,.F.,(3,3),(0.,1.),.UNSPECIFIED.);
#904=B_SPLINE_CURVE_WITH_KNOTS('',2,(#70680,#70681,#70682),
 .UNSPECIFIED.,.F.,.F.,(3,3),(0.,1.),.UNSPECIFIED.);
#905=B_SPLINE_CURVE_WITH_KNOTS('',2,(#70685,#70686,#70687),
 .UNSPECIFIED.,.F.,.F.,(3,3),(0.,1.),.UNSPECIFIED.);
#906=B_SPLINE_CURVE_WITH_KNOTS('',2,(#70695,#70696,#70697),
 .UNSPECIFIED.,.F.,.F.,(3,3),(0.,1.),.UNSPECIFIED.);
#907=B_SPLINE_CURVE_WITH_KNOTS('',2,(#70700,#70701,#70702),
 .UNSPECIFIED.,.F.,.F.,(3,3),(0.,1.),.UNSPECIFIED.);
#908=B_SPLINE_CURVE_WITH_KNOTS('',2,(#70710,#70711,#70712),
 .UNSPECIFIED.,.F.,.F.,(3,3),(0.,1.),.UNSPECIFIED.);
#909=B_SPLINE_CURVE_WITH_KNOTS('',2,(#70715,#70716,#70717),
 .UNSPECIFIED.,.F.,.F.,(3,3),(0.,1.),.UNSPECIFIED.);
#910=B_SPLINE_CURVE_WITH_KNOTS('',2,(#70725,#70726,#70727),
 .UNSPECIFIED.,.F.,.F.,(3,3),(0.,1.),.UNSPECIFIED.);
#911=B_SPLINE_CURVE_WITH_KNOTS('',2,(#70730,#70731,#70732),
 .UNSPECIFIED.,.F.,.F.,(3,3),(0.,1.),.UNSPECIFIED.);
#912=B_SPLINE_CURVE_WITH_KNOTS('',2,(#70740,#70741,#70742),
 .UNSPECIFIED.,.F.,.F.,(3,3),(0.,1.),.UNSPECIFIED.);
#913=B_SPLINE_CURVE_WITH_KNOTS('',2,(#70745,#70746,#70747),
 .UNSPECIFIED.,.F.,.F.,(3,3),(0.,1.),.UNSPECIFIED.);
#914=B_SPLINE_CURVE_WITH_KNOTS('',2,(#70755,#70756,#70757),
 .UNSPECIFIED.,.F.,.F.,(3,3),(0.,1.),.UNSPECIFIED.);
#915=B_SPLINE_CURVE_WITH_KNOTS('',2,(#70760,#70761,#70762),
 .UNSPECIFIED.,.F.,.F.,(3,3),(0.,1.),.UNSPECIFIED.);
#916=B_SPLINE_CURVE_WITH_KNOTS('',2,(#70770,#70771,#70772),
 .UNSPECIFIED.,.F.,.F.,(3,3),(0.,1.),.UNSPECIFIED.);
#917=B_SPLINE_CURVE_WITH_KNOTS('',2,(#70775,#70776,#70777),
 .UNSPECIFIED.,.F.,.F.,(3,3),(0.,1.),.UNSPECIFIED.);
#918=B_SPLINE_CURVE_WITH_KNOTS('',2,(#70785,#70786,#70787),
 .UNSPECIFIED.,.F.,.F.,(3,3),(0.,1.),.UNSPECIFIED.);
#919=B_SPLINE_CURVE_WITH_KNOTS('',2,(#70790,#70791,#70792),
 .UNSPECIFIED.,.F.,.F.,(3,3),(0.,1.),.UNSPECIFIED.);
#920=B_SPLINE_CURVE_WITH_KNOTS('',2,(#70800,#70801,#70802),
 .UNSPECIFIED.,.F.,.F.,(3,3),(0.,1.),.UNSPECIFIED.);
#921=B_SPLINE_CURVE_WITH_KNOTS('',2,(#70805,#70806,#70807),
 .UNSPECIFIED.,.F.,.F.,(3,3),(0.,1.),.UNSPECIFIED.);
#922=B_SPLINE_CURVE_WITH_KNOTS('',2,(#70815,#70816,#70817),
 .UNSPECIFIED.,.F.,.F.,(3,3),(0.,1.),.UNSPECIFIED.);
#923=B_SPLINE_CURVE_WITH_KNOTS('',2,(#70820,#70821,#70822),
 .UNSPECIFIED.,.F.,.F.,(3,3),(0.,1.),.UNSPECIFIED.);
#924=B_SPLINE_CURVE_WITH_KNOTS('',2,(#70836,#70837,#70838),
 .UNSPECIFIED.,.F.,.F.,(3,3),(0.,1.),.UNSPECIFIED.);
#925=B_SPLINE_CURVE_WITH_KNOTS('',2,(#70841,#70842,#70843),
 .UNSPECIFIED.,.F.,.F.,(3,3),(0.,1.),.UNSPECIFIED.);
#926=B_SPLINE_CURVE_WITH_KNOTS('',2,(#70851,#70852,#70853),
 .UNSPECIFIED.,.F.,.F.,(3,3),(0.,1.),.UNSPECIFIED.);
#927=B_SPLINE_CURVE_WITH_KNOTS('',2,(#70856,#70857,#70858),
 .UNSPECIFIED.,.F.,.F.,(3,3),(0.,1.),.UNSPECIFIED.);
#928=B_SPLINE_CURVE_WITH_KNOTS('',2,(#70866,#70867,#70868),
 .UNSPECIFIED.,.F.,.F.,(3,3),(0.,1.),.UNSPECIFIED.);
#929=B_SPLINE_CURVE_WITH_KNOTS('',2,(#70871,#70872,#70873),
 .UNSPECIFIED.,.F.,.F.,(3,3),(0.,1.),.UNSPECIFIED.);
#930=B_SPLINE_CURVE_WITH_KNOTS('',2,(#70881,#70882,#70883),
 .UNSPECIFIED.,.F.,.F.,(3,3),(0.,1.),.UNSPECIFIED.);
#931=B_SPLINE_CURVE_WITH_KNOTS('',2,(#70886,#70887,#70888),
 .UNSPECIFIED.,.F.,.F.,(3,3),(0.,1.),.UNSPECIFIED.);
#932=B_SPLINE_CURVE_WITH_KNOTS('',2,(#70896,#70897,#70898),
 .UNSPECIFIED.,.F.,.F.,(3,3),(0.,1.),.UNSPECIFIED.);
#933=B_SPLINE_CURVE_WITH_KNOTS('',2,(#70901,#70902,#70903),
 .UNSPECIFIED.,.F.,.F.,(3,3),(0.,1.),.UNSPECIFIED.);
#934=B_SPLINE_CURVE_WITH_KNOTS('',2,(#70911,#70912,#70913),
 .UNSPECIFIED.,.F.,.F.,(3,3),(0.,1.),.UNSPECIFIED.);
#935=B_SPLINE_CURVE_WITH_KNOTS('',2,(#70916,#70917,#70918),
 .UNSPECIFIED.,.F.,.F.,(3,3),(0.,1.),.UNSPECIFIED.);
#936=B_SPLINE_CURVE_WITH_KNOTS('',2,(#70926,#70927,#70928),
 .UNSPECIFIED.,.F.,.F.,(3,3),(0.,1.),.UNSPECIFIED.);
#937=B_SPLINE_CURVE_WITH_KNOTS('',2,(#70931,#70932,#70933),
 .UNSPECIFIED.,.F.,.F.,(3,3),(0.,1.),.UNSPECIFIED.);
#938=B_SPLINE_CURVE_WITH_KNOTS('',2,(#70947,#70948,#70949),
 .UNSPECIFIED.,.F.,.F.,(3,3),(0.,1.),.UNSPECIFIED.);
#939=B_SPLINE_CURVE_WITH_KNOTS('',2,(#70952,#70953,#70954),
 .UNSPECIFIED.,.F.,.F.,(3,3),(0.,1.),.UNSPECIFIED.);
#940=B_SPLINE_CURVE_WITH_KNOTS('',2,(#70962,#70963,#70964),
 .UNSPECIFIED.,.F.,.F.,(3,3),(0.,1.),.UNSPECIFIED.);
#941=B_SPLINE_CURVE_WITH_KNOTS('',2,(#70967,#70968,#70969),
 .UNSPECIFIED.,.F.,.F.,(3,3),(0.,1.),.UNSPECIFIED.);
#942=B_SPLINE_CURVE_WITH_KNOTS('',2,(#70977,#70978,#70979),
 .UNSPECIFIED.,.F.,.F.,(3,3),(0.,1.),.UNSPECIFIED.);
#943=B_SPLINE_CURVE_WITH_KNOTS('',2,(#70982,#70983,#70984),
 .UNSPECIFIED.,.F.,.F.,(3,3),(0.,1.),.UNSPECIFIED.);
#944=B_SPLINE_CURVE_WITH_KNOTS('',2,(#70992,#70993,#70994),
 .UNSPECIFIED.,.F.,.F.,(3,3),(0.,1.),.UNSPECIFIED.);
#945=B_SPLINE_CURVE_WITH_KNOTS('',2,(#70997,#70998,#70999),
 .UNSPECIFIED.,.F.,.F.,(3,3),(0.,1.),.UNSPECIFIED.);
#946=B_SPLINE_CURVE_WITH_KNOTS('',2,(#71007,#71008,#71009),
 .UNSPECIFIED.,.F.,.F.,(3,3),(0.,1.),.UNSPECIFIED.);
#947=B_SPLINE_CURVE_WITH_KNOTS('',2,(#71012,#71013,#71014),
 .UNSPECIFIED.,.F.,.F.,(3,3),(0.,1.),.UNSPECIFIED.);
#948=B_SPLINE_CURVE_WITH_KNOTS('',2,(#71022,#71023,#71024),
 .UNSPECIFIED.,.F.,.F.,(3,3),(0.,1.),.UNSPECIFIED.);
#949=B_SPLINE_CURVE_WITH_KNOTS('',2,(#71027,#71028,#71029),
 .UNSPECIFIED.,.F.,.F.,(3,3),(0.,1.),.UNSPECIFIED.);
#950=B_SPLINE_CURVE_WITH_KNOTS('',2,(#71037,#71038,#71039),
 .UNSPECIFIED.,.F.,.F.,(3,3),(0.,1.),.UNSPECIFIED.);
#951=B_SPLINE_CURVE_WITH_KNOTS('',2,(#71042,#71043,#71044),
 .UNSPECIFIED.,.F.,.F.,(3,3),(0.,1.),.UNSPECIFIED.);
#952=B_SPLINE_CURVE_WITH_KNOTS('',2,(#71057,#71058,#71059),
 .UNSPECIFIED.,.F.,.F.,(3,3),(0.,1.),.UNSPECIFIED.);
#953=B_SPLINE_CURVE_WITH_KNOTS('',2,(#71060,#71061,#71062),
 .UNSPECIFIED.,.F.,.F.,(3,3),(0.,1.),.UNSPECIFIED.);
#954=B_SPLINE_CURVE_WITH_KNOTS('',2,(#71073,#71074,#71075),
 .UNSPECIFIED.,.F.,.F.,(3,3),(0.,1.),.UNSPECIFIED.);
#955=B_SPLINE_CURVE_WITH_KNOTS('',2,(#71079,#71080,#71081),
 .UNSPECIFIED.,.F.,.F.,(3,3),(0.,1.),.UNSPECIFIED.);
#956=B_SPLINE_CURVE_WITH_KNOTS('',2,(#71090,#71091,#71092),
 .UNSPECIFIED.,.F.,.F.,(3,3),(0.,1.),.UNSPECIFIED.);
#957=B_SPLINE_CURVE_WITH_KNOTS('',2,(#71095,#71096,#71097),
 .UNSPECIFIED.,.F.,.F.,(3,3),(0.,1.),.UNSPECIFIED.);
#958=B_SPLINE_CURVE_WITH_KNOTS('',2,(#71105,#71106,#71107),
 .UNSPECIFIED.,.F.,.F.,(3,3),(0.,1.),.UNSPECIFIED.);
#959=B_SPLINE_CURVE_WITH_KNOTS('',2,(#71110,#71111,#71112),
 .UNSPECIFIED.,.F.,.F.,(3,3),(0.,1.),.UNSPECIFIED.);
#960=B_SPLINE_CURVE_WITH_KNOTS('',2,(#71120,#71121,#71122),
 .UNSPECIFIED.,.F.,.F.,(3,3),(0.,1.),.UNSPECIFIED.);
#961=B_SPLINE_CURVE_WITH_KNOTS('',2,(#71125,#71126,#71127),
 .UNSPECIFIED.,.F.,.F.,(3,3),(0.,1.),.UNSPECIFIED.);
#962=B_SPLINE_CURVE_WITH_KNOTS('',2,(#71135,#71136,#71137),
 .UNSPECIFIED.,.F.,.F.,(3,3),(0.,1.),.UNSPECIFIED.);
#963=B_SPLINE_CURVE_WITH_KNOTS('',2,(#71140,#71141,#71142),
 .UNSPECIFIED.,.F.,.F.,(3,3),(0.,1.),.UNSPECIFIED.);
#964=B_SPLINE_CURVE_WITH_KNOTS('',2,(#71150,#71151,#71152),
 .UNSPECIFIED.,.F.,.F.,(3,3),(0.,1.),.UNSPECIFIED.);
#965=B_SPLINE_CURVE_WITH_KNOTS('',2,(#71155,#71156,#71157),
 .UNSPECIFIED.,.F.,.F.,(3,3),(0.,1.),.UNSPECIFIED.);
#966=B_SPLINE_CURVE_WITH_KNOTS('',2,(#71165,#71166,#71167),
 .UNSPECIFIED.,.F.,.F.,(3,3),(0.,1.),.UNSPECIFIED.);
#967=B_SPLINE_CURVE_WITH_KNOTS('',2,(#71170,#71171,#71172),
 .UNSPECIFIED.,.F.,.F.,(3,3),(0.,1.),.UNSPECIFIED.);
#968=B_SPLINE_CURVE_WITH_KNOTS('',2,(#71179,#71180,#71181),
 .UNSPECIFIED.,.F.,.F.,(3,3),(0.,1.),.UNSPECIFIED.);
#969=B_SPLINE_CURVE_WITH_KNOTS('',2,(#71182,#71183,#71184),
 .UNSPECIFIED.,.F.,.F.,(3,3),(0.,1.),.UNSPECIFIED.);
#970=B_SPLINE_CURVE_WITH_KNOTS('',2,(#71193,#71194,#71195),
 .UNSPECIFIED.,.F.,.F.,(3,3),(0.,1.),.UNSPECIFIED.);
#971=B_SPLINE_CURVE_WITH_KNOTS('',2,(#71199,#71200,#71201),
 .UNSPECIFIED.,.F.,.F.,(3,3),(0.,1.),.UNSPECIFIED.);
#972=B_SPLINE_CURVE_WITH_KNOTS('',2,(#71210,#71211,#71212),
 .UNSPECIFIED.,.F.,.F.,(3,3),(0.,1.),.UNSPECIFIED.);
#973=B_SPLINE_CURVE_WITH_KNOTS('',2,(#71215,#71216,#71217),
 .UNSPECIFIED.,.F.,.F.,(3,3),(0.,1.),.UNSPECIFIED.);
#974=B_SPLINE_CURVE_WITH_KNOTS('',2,(#71225,#71226,#71227),
 .UNSPECIFIED.,.F.,.F.,(3,3),(0.,1.),.UNSPECIFIED.);
#975=B_SPLINE_CURVE_WITH_KNOTS('',2,(#71230,#71231,#71232),
 .UNSPECIFIED.,.F.,.F.,(3,3),(0.,1.),.UNSPECIFIED.);
#976=B_SPLINE_CURVE_WITH_KNOTS('',2,(#71240,#71241,#71242),
 .UNSPECIFIED.,.F.,.F.,(3,3),(0.,1.),.UNSPECIFIED.);
#977=B_SPLINE_CURVE_WITH_KNOTS('',2,(#71245,#71246,#71247),
 .UNSPECIFIED.,.F.,.F.,(3,3),(0.,1.),.UNSPECIFIED.);
#978=B_SPLINE_CURVE_WITH_KNOTS('',2,(#71255,#71256,#71257),
 .UNSPECIFIED.,.F.,.F.,(3,3),(0.,1.),.UNSPECIFIED.);
#979=B_SPLINE_CURVE_WITH_KNOTS('',2,(#71260,#71261,#71262),
 .UNSPECIFIED.,.F.,.F.,(3,3),(0.,1.),.UNSPECIFIED.);
#980=B_SPLINE_CURVE_WITH_KNOTS('',2,(#71270,#71271,#71272),
 .UNSPECIFIED.,.F.,.F.,(3,3),(0.,1.),.UNSPECIFIED.);
#981=B_SPLINE_CURVE_WITH_KNOTS('',2,(#71275,#71276,#71277),
 .UNSPECIFIED.,.F.,.F.,(3,3),(0.,1.),.UNSPECIFIED.);
#982=B_SPLINE_CURVE_WITH_KNOTS('',2,(#71285,#71286,#71287),
 .UNSPECIFIED.,.F.,.F.,(3,3),(0.,1.),.UNSPECIFIED.);
#983=B_SPLINE_CURVE_WITH_KNOTS('',2,(#71290,#71291,#71292),
 .UNSPECIFIED.,.F.,.F.,(3,3),(0.,1.),.UNSPECIFIED.);
#984=B_SPLINE_CURVE_WITH_KNOTS('',2,(#71300,#71301,#71302),
 .UNSPECIFIED.,.F.,.F.,(3,3),(0.,1.),.UNSPECIFIED.);
#985=B_SPLINE_CURVE_WITH_KNOTS('',2,(#71305,#71306,#71307),
 .UNSPECIFIED.,.F.,.F.,(3,3),(0.,1.),.UNSPECIFIED.);
#986=B_SPLINE_CURVE_WITH_KNOTS('',2,(#71315,#71316,#71317),
 .UNSPECIFIED.,.F.,.F.,(3,3),(0.,1.),.UNSPECIFIED.);
#987=B_SPLINE_CURVE_WITH_KNOTS('',2,(#71320,#71321,#71322),
 .UNSPECIFIED.,.F.,.F.,(3,3),(0.,1.),.UNSPECIFIED.);
#988=B_SPLINE_CURVE_WITH_KNOTS('',2,(#71330,#71331,#71332),
 .UNSPECIFIED.,.F.,.F.,(3,3),(0.,1.),.UNSPECIFIED.);
#989=B_SPLINE_CURVE_WITH_KNOTS('',2,(#71335,#71336,#71337),
 .UNSPECIFIED.,.F.,.F.,(3,3),(0.,1.),.UNSPECIFIED.);
#990=B_SPLINE_CURVE_WITH_KNOTS('',2,(#71345,#71346,#71347),
 .UNSPECIFIED.,.F.,.F.,(3,3),(0.,1.),.UNSPECIFIED.);
#991=B_SPLINE_CURVE_WITH_KNOTS('',2,(#71350,#71351,#71352),
 .UNSPECIFIED.,.F.,.F.,(3,3),(0.,1.),.UNSPECIFIED.);
#992=B_SPLINE_CURVE_WITH_KNOTS('',2,(#71359,#71360,#71361),
 .UNSPECIFIED.,.F.,.F.,(3,3),(0.,1.),.UNSPECIFIED.);
#993=B_SPLINE_CURVE_WITH_KNOTS('',2,(#71362,#71363,#71364),
 .UNSPECIFIED.,.F.,.F.,(3,3),(0.,1.),.UNSPECIFIED.);
#994=B_SPLINE_CURVE_WITH_KNOTS('',2,(#71374,#71375,#71376),
 .UNSPECIFIED.,.F.,.F.,(3,3),(0.,1.),.UNSPECIFIED.);
#995=B_SPLINE_CURVE_WITH_KNOTS('',2,(#71380,#71381,#71382),
 .UNSPECIFIED.,.F.,.F.,(3,3),(0.,1.),.UNSPECIFIED.);
#996=B_SPLINE_CURVE_WITH_KNOTS('',2,(#71391,#71392,#71393),
 .UNSPECIFIED.,.F.,.F.,(3,3),(0.,1.),.UNSPECIFIED.);
#997=B_SPLINE_CURVE_WITH_KNOTS('',2,(#71396,#71397,#71398),
 .UNSPECIFIED.,.F.,.F.,(3,3),(0.,1.),.UNSPECIFIED.);
#998=B_SPLINE_CURVE_WITH_KNOTS('',2,(#71406,#71407,#71408),
 .UNSPECIFIED.,.F.,.F.,(3,3),(0.,1.),.UNSPECIFIED.);
#999=B_SPLINE_CURVE_WITH_KNOTS('',2,(#71411,#71412,#71413),
 .UNSPECIFIED.,.F.,.F.,(3,3),(0.,1.),.UNSPECIFIED.);
#1000=B_SPLINE_CURVE_WITH_KNOTS('',2,(#71421,#71422,#71423),
 .UNSPECIFIED.,.F.,.F.,(3,3),(0.,1.),.UNSPECIFIED.);
#1001=B_SPLINE_CURVE_WITH_KNOTS('',2,(#71426,#71427,#71428),
 .UNSPECIFIED.,.F.,.F.,(3,3),(0.,1.),.UNSPECIFIED.);
#1002=B_SPLINE_CURVE_WITH_KNOTS('',2,(#71436,#71437,#71438),
 .UNSPECIFIED.,.F.,.F.,(3,3),(0.,1.),.UNSPECIFIED.);
#1003=B_SPLINE_CURVE_WITH_KNOTS('',2,(#71441,#71442,#71443),
 .UNSPECIFIED.,.F.,.F.,(3,3),(0.,1.),.UNSPECIFIED.);
#1004=B_SPLINE_CURVE_WITH_KNOTS('',2,(#71451,#71452,#71453),
 .UNSPECIFIED.,.F.,.F.,(3,3),(0.,1.),.UNSPECIFIED.);
#1005=B_SPLINE_CURVE_WITH_KNOTS('',2,(#71456,#71457,#71458),
 .UNSPECIFIED.,.F.,.F.,(3,3),(0.,1.),.UNSPECIFIED.);
#1006=B_SPLINE_CURVE_WITH_KNOTS('',2,(#71466,#71467,#71468),
 .UNSPECIFIED.,.F.,.F.,(3,3),(0.,1.),.UNSPECIFIED.);
#1007=B_SPLINE_CURVE_WITH_KNOTS('',2,(#71471,#71472,#71473),
 .UNSPECIFIED.,.F.,.F.,(3,3),(0.,1.),.UNSPECIFIED.);
#1008=B_SPLINE_CURVE_WITH_KNOTS('',2,(#71481,#71482,#71483),
 .UNSPECIFIED.,.F.,.F.,(3,3),(0.,1.),.UNSPECIFIED.);
#1009=B_SPLINE_CURVE_WITH_KNOTS('',2,(#71486,#71487,#71488),
 .UNSPECIFIED.,.F.,.F.,(3,3),(0.,1.),.UNSPECIFIED.);
#1010=B_SPLINE_CURVE_WITH_KNOTS('',2,(#71496,#71497,#71498),
 .UNSPECIFIED.,.F.,.F.,(3,3),(0.,1.),.UNSPECIFIED.);
#1011=B_SPLINE_CURVE_WITH_KNOTS('',2,(#71501,#71502,#71503),
 .UNSPECIFIED.,.F.,.F.,(3,3),(0.,1.),.UNSPECIFIED.);
#1012=B_SPLINE_CURVE_WITH_KNOTS('',2,(#71517,#71518,#71519),
 .UNSPECIFIED.,.F.,.F.,(3,3),(0.,1.),.UNSPECIFIED.);
#1013=B_SPLINE_CURVE_WITH_KNOTS('',2,(#71522,#71523,#71524),
 .UNSPECIFIED.,.F.,.F.,(3,3),(0.,1.),.UNSPECIFIED.);
#1014=B_SPLINE_CURVE_WITH_KNOTS('',2,(#71532,#71533,#71534),
 .UNSPECIFIED.,.F.,.F.,(3,3),(0.,1.),.UNSPECIFIED.);
#1015=B_SPLINE_CURVE_WITH_KNOTS('',2,(#71537,#71538,#71539),
 .UNSPECIFIED.,.F.,.F.,(3,3),(0.,1.),.UNSPECIFIED.);
#1016=B_SPLINE_CURVE_WITH_KNOTS('',2,(#71547,#71548,#71549),
 .UNSPECIFIED.,.F.,.F.,(3,3),(0.,1.),.UNSPECIFIED.);
#1017=B_SPLINE_CURVE_WITH_KNOTS('',2,(#71552,#71553,#71554),
 .UNSPECIFIED.,.F.,.F.,(3,3),(0.,1.),.UNSPECIFIED.);
#1018=B_SPLINE_CURVE_WITH_KNOTS('',2,(#71562,#71563,#71564),
 .UNSPECIFIED.,.F.,.F.,(3,3),(0.,1.),.UNSPECIFIED.);
#1019=B_SPLINE_CURVE_WITH_KNOTS('',2,(#71567,#71568,#71569),
 .UNSPECIFIED.,.F.,.F.,(3,3),(0.,1.),.UNSPECIFIED.);
#1020=B_SPLINE_CURVE_WITH_KNOTS('',2,(#71577,#71578,#71579),
 .UNSPECIFIED.,.F.,.F.,(3,3),(0.,1.),.UNSPECIFIED.);
#1021=B_SPLINE_CURVE_WITH_KNOTS('',2,(#71582,#71583,#71584),
 .UNSPECIFIED.,.F.,.F.,(3,3),(0.,1.),.UNSPECIFIED.);
#1022=B_SPLINE_CURVE_WITH_KNOTS('',2,(#71592,#71593,#71594),
 .UNSPECIFIED.,.F.,.F.,(3,3),(0.,1.),.UNSPECIFIED.);
#1023=B_SPLINE_CURVE_WITH_KNOTS('',2,(#71597,#71598,#71599),
 .UNSPECIFIED.,.F.,.F.,(3,3),(0.,1.),.UNSPECIFIED.);
#1024=B_SPLINE_CURVE_WITH_KNOTS('',2,(#71607,#71608,#71609),
 .UNSPECIFIED.,.F.,.F.,(3,3),(0.,1.),.UNSPECIFIED.);
#1025=B_SPLINE_CURVE_WITH_KNOTS('',2,(#71612,#71613,#71614),
 .UNSPECIFIED.,.F.,.F.,(3,3),(0.,1.),.UNSPECIFIED.);
#1026=B_SPLINE_CURVE_WITH_KNOTS('',2,(#71622,#71623,#71624),
 .UNSPECIFIED.,.F.,.F.,(3,3),(0.,1.),.UNSPECIFIED.);
#1027=B_SPLINE_CURVE_WITH_KNOTS('',2,(#71627,#71628,#71629),
 .UNSPECIFIED.,.F.,.F.,(3,3),(0.,1.),.UNSPECIFIED.);
#1028=B_SPLINE_CURVE_WITH_KNOTS('',2,(#71637,#71638,#71639),
 .UNSPECIFIED.,.F.,.F.,(3,3),(0.,1.),.UNSPECIFIED.);
#1029=B_SPLINE_CURVE_WITH_KNOTS('',2,(#71642,#71643,#71644),
 .UNSPECIFIED.,.F.,.F.,(3,3),(0.,1.),.UNSPECIFIED.);
#1030=B_SPLINE_CURVE_WITH_KNOTS('',2,(#71670,#71671,#71672),
 .UNSPECIFIED.,.F.,.F.,(3,3),(0.,1.),.UNSPECIFIED.);
#1031=B_SPLINE_CURVE_WITH_KNOTS('',2,(#71676,#71677,#71678),
 .UNSPECIFIED.,.F.,.F.,(3,3),(0.,1.),.UNSPECIFIED.);
#1032=B_SPLINE_CURVE_WITH_KNOTS('',2,(#71687,#71688,#71689),
 .UNSPECIFIED.,.F.,.F.,(3,3),(0.,1.),.UNSPECIFIED.);
#1033=B_SPLINE_CURVE_WITH_KNOTS('',2,(#71692,#71693,#71694),
 .UNSPECIFIED.,.F.,.F.,(3,3),(0.,1.),.UNSPECIFIED.);
#1034=B_SPLINE_CURVE_WITH_KNOTS('',2,(#71702,#71703,#71704),
 .UNSPECIFIED.,.F.,.F.,(3,3),(0.,1.),.UNSPECIFIED.);
#1035=B_SPLINE_CURVE_WITH_KNOTS('',2,(#71707,#71708,#71709),
 .UNSPECIFIED.,.F.,.F.,(3,3),(0.,1.),.UNSPECIFIED.);
#1036=B_SPLINE_CURVE_WITH_KNOTS('',2,(#71717,#71718,#71719),
 .UNSPECIFIED.,.F.,.F.,(3,3),(0.,1.),.UNSPECIFIED.);
#1037=B_SPLINE_CURVE_WITH_KNOTS('',2,(#71722,#71723,#71724),
 .UNSPECIFIED.,.F.,.F.,(3,3),(0.,1.),.UNSPECIFIED.);
#1038=B_SPLINE_CURVE_WITH_KNOTS('',2,(#71732,#71733,#71734),
 .UNSPECIFIED.,.F.,.F.,(3,3),(0.,1.),.UNSPECIFIED.);
#1039=B_SPLINE_CURVE_WITH_KNOTS('',2,(#71737,#71738,#71739),
 .UNSPECIFIED.,.F.,.F.,(3,3),(0.,1.),.UNSPECIFIED.);
#1040=B_SPLINE_CURVE_WITH_KNOTS('',2,(#71747,#71748,#71749),
 .UNSPECIFIED.,.F.,.F.,(3,3),(0.,1.),.UNSPECIFIED.);
#1041=B_SPLINE_CURVE_WITH_KNOTS('',2,(#71752,#71753,#71754),
 .UNSPECIFIED.,.F.,.F.,(3,3),(0.,1.),.UNSPECIFIED.);
#1042=B_SPLINE_CURVE_WITH_KNOTS('',2,(#71762,#71763,#71764),
 .UNSPECIFIED.,.F.,.F.,(3,3),(0.,1.),.UNSPECIFIED.);
#1043=B_SPLINE_CURVE_WITH_KNOTS('',2,(#71767,#71768,#71769),
 .UNSPECIFIED.,.F.,.F.,(3,3),(0.,1.),.UNSPECIFIED.);
#1044=B_SPLINE_CURVE_WITH_KNOTS('',2,(#71776,#71777,#71778),
 .UNSPECIFIED.,.F.,.F.,(3,3),(0.,1.),.UNSPECIFIED.);
#1045=B_SPLINE_CURVE_WITH_KNOTS('',2,(#71779,#71780,#71781),
 .UNSPECIFIED.,.F.,.F.,(3,3),(0.,1.),.UNSPECIFIED.);
#1046=B_SPLINE_CURVE_WITH_KNOTS('',2,(#71790,#71791,#71792),
 .UNSPECIFIED.,.F.,.F.,(3,3),(0.,1.),.UNSPECIFIED.);
#1047=B_SPLINE_CURVE_WITH_KNOTS('',2,(#71796,#71797,#71798),
 .UNSPECIFIED.,.F.,.F.,(3,3),(0.,1.),.UNSPECIFIED.);
#1048=B_SPLINE_CURVE_WITH_KNOTS('',2,(#71807,#71808,#71809),
 .UNSPECIFIED.,.F.,.F.,(3,3),(0.,1.),.UNSPECIFIED.);
#1049=B_SPLINE_CURVE_WITH_KNOTS('',2,(#71812,#71813,#71814),
 .UNSPECIFIED.,.F.,.F.,(3,3),(0.,1.),.UNSPECIFIED.);
#1050=B_SPLINE_CURVE_WITH_KNOTS('',2,(#71822,#71823,#71824),
 .UNSPECIFIED.,.F.,.F.,(3,3),(0.,1.),.UNSPECIFIED.);
#1051=B_SPLINE_CURVE_WITH_KNOTS('',2,(#71827,#71828,#71829),
 .UNSPECIFIED.,.F.,.F.,(3,3),(0.,1.),.UNSPECIFIED.);
#1052=B_SPLINE_CURVE_WITH_KNOTS('',2,(#71837,#71838,#71839),
 .UNSPECIFIED.,.F.,.F.,(3,3),(0.,1.),.UNSPECIFIED.);
#1053=B_SPLINE_CURVE_WITH_KNOTS('',2,(#71842,#71843,#71844),
 .UNSPECIFIED.,.F.,.F.,(3,3),(0.,1.),.UNSPECIFIED.);
#1054=B_SPLINE_CURVE_WITH_KNOTS('',2,(#71852,#71853,#71854),
 .UNSPECIFIED.,.F.,.F.,(3,3),(0.,1.),.UNSPECIFIED.);
#1055=B_SPLINE_CURVE_WITH_KNOTS('',2,(#71857,#71858,#71859),
 .UNSPECIFIED.,.F.,.F.,(3,3),(0.,1.),.UNSPECIFIED.);
#1056=B_SPLINE_CURVE_WITH_KNOTS('',2,(#71867,#71868,#71869),
 .UNSPECIFIED.,.F.,.F.,(3,3),(0.,1.),.UNSPECIFIED.);
#1057=B_SPLINE_CURVE_WITH_KNOTS('',2,(#71872,#71873,#71874),
 .UNSPECIFIED.,.F.,.F.,(3,3),(0.,1.),.UNSPECIFIED.);
#1058=B_SPLINE_CURVE_WITH_KNOTS('',2,(#71882,#71883,#71884),
 .UNSPECIFIED.,.F.,.F.,(3,3),(0.,1.),.UNSPECIFIED.);
#1059=B_SPLINE_CURVE_WITH_KNOTS('',2,(#71887,#71888,#71889),
 .UNSPECIFIED.,.F.,.F.,(3,3),(0.,1.),.UNSPECIFIED.);
#1060=B_SPLINE_CURVE_WITH_KNOTS('',2,(#71897,#71898,#71899),
 .UNSPECIFIED.,.F.,.F.,(3,3),(0.,1.),.UNSPECIFIED.);
#1061=B_SPLINE_CURVE_WITH_KNOTS('',2,(#71902,#71903,#71904),
 .UNSPECIFIED.,.F.,.F.,(3,3),(0.,1.),.UNSPECIFIED.);
#1062=B_SPLINE_CURVE_WITH_KNOTS('',2,(#71912,#71913,#71914),
 .UNSPECIFIED.,.F.,.F.,(3,3),(0.,1.),.UNSPECIFIED.);
#1063=B_SPLINE_CURVE_WITH_KNOTS('',2,(#71917,#71918,#71919),
 .UNSPECIFIED.,.F.,.F.,(3,3),(0.,1.),.UNSPECIFIED.);
#1064=B_SPLINE_CURVE_WITH_KNOTS('',2,(#71927,#71928,#71929),
 .UNSPECIFIED.,.F.,.F.,(3,3),(0.,1.),.UNSPECIFIED.);
#1065=B_SPLINE_CURVE_WITH_KNOTS('',2,(#71932,#71933,#71934),
 .UNSPECIFIED.,.F.,.F.,(3,3),(0.,1.),.UNSPECIFIED.);
#1066=B_SPLINE_CURVE_WITH_KNOTS('',2,(#71942,#71943,#71944),
 .UNSPECIFIED.,.F.,.F.,(3,3),(0.,1.),.UNSPECIFIED.);
#1067=B_SPLINE_CURVE_WITH_KNOTS('',2,(#71947,#71948,#71949),
 .UNSPECIFIED.,.F.,.F.,(3,3),(0.,1.),.UNSPECIFIED.);
#1068=B_SPLINE_CURVE_WITH_KNOTS('',2,(#71956,#71957,#71958),
 .UNSPECIFIED.,.F.,.F.,(3,3),(0.,1.),.UNSPECIFIED.);
#1069=B_SPLINE_CURVE_WITH_KNOTS('',2,(#71959,#71960,#71961),
 .UNSPECIFIED.,.F.,.F.,(3,3),(0.,1.),.UNSPECIFIED.);
#1070=B_SPLINE_CURVE_WITH_KNOTS('',2,(#71979,#71980,#71981),
 .UNSPECIFIED.,.F.,.F.,(3,3),(0.,1.),.UNSPECIFIED.);
#1071=B_SPLINE_CURVE_WITH_KNOTS('',2,(#71984,#71985,#71986),
 .UNSPECIFIED.,.F.,.F.,(3,3),(0.,1.),.UNSPECIFIED.);
#1072=B_SPLINE_CURVE_WITH_KNOTS('',2,(#71994,#71995,#71996),
 .UNSPECIFIED.,.F.,.F.,(3,3),(0.,1.),.UNSPECIFIED.);
#1073=B_SPLINE_CURVE_WITH_KNOTS('',2,(#71999,#72000,#72001),
 .UNSPECIFIED.,.F.,.F.,(3,3),(0.,1.),.UNSPECIFIED.);
#1074=B_SPLINE_CURVE_WITH_KNOTS('',2,(#72015,#72016,#72017),
 .UNSPECIFIED.,.F.,.F.,(3,3),(0.,1.),.UNSPECIFIED.);
#1075=B_SPLINE_CURVE_WITH_KNOTS('',2,(#72020,#72021,#72022),
 .UNSPECIFIED.,.F.,.F.,(3,3),(0.,1.),.UNSPECIFIED.);
#1076=B_SPLINE_CURVE_WITH_KNOTS('',2,(#72030,#72031,#72032),
 .UNSPECIFIED.,.F.,.F.,(3,3),(0.,1.),.UNSPECIFIED.);
#1077=B_SPLINE_CURVE_WITH_KNOTS('',2,(#72035,#72036,#72037),
 .UNSPECIFIED.,.F.,.F.,(3,3),(0.,1.),.UNSPECIFIED.);
#1078=B_SPLINE_CURVE_WITH_KNOTS('',2,(#72063,#72064,#72065),
 .UNSPECIFIED.,.F.,.F.,(3,3),(0.,1.),.UNSPECIFIED.);
#1079=B_SPLINE_CURVE_WITH_KNOTS('',2,(#72069,#72070,#72071),
 .UNSPECIFIED.,.F.,.F.,(3,3),(0.,1.),.UNSPECIFIED.);
#1080=B_SPLINE_CURVE_WITH_KNOTS('',2,(#72080,#72081,#72082),
 .UNSPECIFIED.,.F.,.F.,(3,3),(0.,1.),.UNSPECIFIED.);
#1081=B_SPLINE_CURVE_WITH_KNOTS('',2,(#72085,#72086,#72087),
 .UNSPECIFIED.,.F.,.F.,(3,3),(0.,1.),.UNSPECIFIED.);
#1082=B_SPLINE_CURVE_WITH_KNOTS('',2,(#72095,#72096,#72097),
 .UNSPECIFIED.,.F.,.F.,(3,3),(0.,1.),.UNSPECIFIED.);
#1083=B_SPLINE_CURVE_WITH_KNOTS('',2,(#72100,#72101,#72102),
 .UNSPECIFIED.,.F.,.F.,(3,3),(0.,1.),.UNSPECIFIED.);
#1084=B_SPLINE_CURVE_WITH_KNOTS('',2,(#72110,#72111,#72112),
 .UNSPECIFIED.,.F.,.F.,(3,3),(0.,1.),.UNSPECIFIED.);
#1085=B_SPLINE_CURVE_WITH_KNOTS('',2,(#72115,#72116,#72117),
 .UNSPECIFIED.,.F.,.F.,(3,3),(0.,1.),.UNSPECIFIED.);
#1086=B_SPLINE_CURVE_WITH_KNOTS('',2,(#72125,#72126,#72127),
 .UNSPECIFIED.,.F.,.F.,(3,3),(0.,1.),.UNSPECIFIED.);
#1087=B_SPLINE_CURVE_WITH_KNOTS('',2,(#72130,#72131,#72132),
 .UNSPECIFIED.,.F.,.F.,(3,3),(0.,1.),.UNSPECIFIED.);
#1088=B_SPLINE_CURVE_WITH_KNOTS('',2,(#72140,#72141,#72142),
 .UNSPECIFIED.,.F.,.F.,(3,3),(0.,1.),.UNSPECIFIED.);
#1089=B_SPLINE_CURVE_WITH_KNOTS('',2,(#72145,#72146,#72147),
 .UNSPECIFIED.,.F.,.F.,(3,3),(0.,1.),.UNSPECIFIED.);
#1090=B_SPLINE_CURVE_WITH_KNOTS('',2,(#72155,#72156,#72157),
 .UNSPECIFIED.,.F.,.F.,(3,3),(0.,1.),.UNSPECIFIED.);
#1091=B_SPLINE_CURVE_WITH_KNOTS('',2,(#72160,#72161,#72162),
 .UNSPECIFIED.,.F.,.F.,(3,3),(0.,1.),.UNSPECIFIED.);
#1092=B_SPLINE_CURVE_WITH_KNOTS('',2,(#72169,#72170,#72171),
 .UNSPECIFIED.,.F.,.F.,(3,3),(0.,1.),.UNSPECIFIED.);
#1093=B_SPLINE_CURVE_WITH_KNOTS('',2,(#72172,#72173,#72174),
 .UNSPECIFIED.,.F.,.F.,(3,3),(0.,1.),.UNSPECIFIED.);
#1094=B_SPLINE_CURVE_WITH_KNOTS('',2,(#72183,#72184,#72185),
 .UNSPECIFIED.,.F.,.F.,(3,3),(0.,1.),.UNSPECIFIED.);
#1095=B_SPLINE_CURVE_WITH_KNOTS('',2,(#72189,#72190,#72191),
 .UNSPECIFIED.,.F.,.F.,(3,3),(0.,1.),.UNSPECIFIED.);
#1096=B_SPLINE_CURVE_WITH_KNOTS('',2,(#72200,#72201,#72202),
 .UNSPECIFIED.,.F.,.F.,(3,3),(0.,1.),.UNSPECIFIED.);
#1097=B_SPLINE_CURVE_WITH_KNOTS('',2,(#72205,#72206,#72207),
 .UNSPECIFIED.,.F.,.F.,(3,3),(0.,1.),.UNSPECIFIED.);
#1098=B_SPLINE_CURVE_WITH_KNOTS('',2,(#72215,#72216,#72217),
 .UNSPECIFIED.,.F.,.F.,(3,3),(0.,1.),.UNSPECIFIED.);
#1099=B_SPLINE_CURVE_WITH_KNOTS('',2,(#72220,#72221,#72222),
 .UNSPECIFIED.,.F.,.F.,(3,3),(0.,1.),.UNSPECIFIED.);
#1100=B_SPLINE_CURVE_WITH_KNOTS('',2,(#72230,#72231,#72232),
 .UNSPECIFIED.,.F.,.F.,(3,3),(0.,1.),.UNSPECIFIED.);
#1101=B_SPLINE_CURVE_WITH_KNOTS('',2,(#72235,#72236,#72237),
 .UNSPECIFIED.,.F.,.F.,(3,3),(0.,1.),.UNSPECIFIED.);
#1102=B_SPLINE_CURVE_WITH_KNOTS('',2,(#72245,#72246,#72247),
 .UNSPECIFIED.,.F.,.F.,(3,3),(0.,1.),.UNSPECIFIED.);
#1103=B_SPLINE_CURVE_WITH_KNOTS('',2,(#72250,#72251,#72252),
 .UNSPECIFIED.,.F.,.F.,(3,3),(0.,1.),.UNSPECIFIED.);
#1104=B_SPLINE_CURVE_WITH_KNOTS('',2,(#72260,#72261,#72262),
 .UNSPECIFIED.,.F.,.F.,(3,3),(0.,1.),.UNSPECIFIED.);
#1105=B_SPLINE_CURVE_WITH_KNOTS('',2,(#72265,#72266,#72267),
 .UNSPECIFIED.,.F.,.F.,(3,3),(0.,1.),.UNSPECIFIED.);
#1106=B_SPLINE_CURVE_WITH_KNOTS('',2,(#72275,#72276,#72277),
 .UNSPECIFIED.,.F.,.F.,(3,3),(0.,1.),.UNSPECIFIED.);
#1107=B_SPLINE_CURVE_WITH_KNOTS('',2,(#72280,#72281,#72282),
 .UNSPECIFIED.,.F.,.F.,(3,3),(0.,1.),.UNSPECIFIED.);
#1108=B_SPLINE_CURVE_WITH_KNOTS('',2,(#72290,#72291,#72292),
 .UNSPECIFIED.,.F.,.F.,(3,3),(0.,1.),.UNSPECIFIED.);
#1109=B_SPLINE_CURVE_WITH_KNOTS('',2,(#72295,#72296,#72297),
 .UNSPECIFIED.,.F.,.F.,(3,3),(0.,1.),.UNSPECIFIED.);
#1110=B_SPLINE_CURVE_WITH_KNOTS('',2,(#72305,#72306,#72307),
 .UNSPECIFIED.,.F.,.F.,(3,3),(0.,1.),.UNSPECIFIED.);
#1111=B_SPLINE_CURVE_WITH_KNOTS('',2,(#72310,#72311,#72312),
 .UNSPECIFIED.,.F.,.F.,(3,3),(0.,1.),.UNSPECIFIED.);
#1112=B_SPLINE_CURVE_WITH_KNOTS('',2,(#72320,#72321,#72322),
 .UNSPECIFIED.,.F.,.F.,(3,3),(0.,1.),.UNSPECIFIED.);
#1113=B_SPLINE_CURVE_WITH_KNOTS('',2,(#72325,#72326,#72327),
 .UNSPECIFIED.,.F.,.F.,(3,3),(0.,1.),.UNSPECIFIED.);
#1114=B_SPLINE_CURVE_WITH_KNOTS('',2,(#72335,#72336,#72337),
 .UNSPECIFIED.,.F.,.F.,(3,3),(0.,1.),.UNSPECIFIED.);
#1115=B_SPLINE_CURVE_WITH_KNOTS('',2,(#72340,#72341,#72342),
 .UNSPECIFIED.,.F.,.F.,(3,3),(0.,1.),.UNSPECIFIED.);
#1116=B_SPLINE_CURVE_WITH_KNOTS('',2,(#72349,#72350,#72351),
 .UNSPECIFIED.,.F.,.F.,(3,3),(0.,1.),.UNSPECIFIED.);
#1117=B_SPLINE_CURVE_WITH_KNOTS('',2,(#72352,#72353,#72354),
 .UNSPECIFIED.,.F.,.F.,(3,3),(0.,1.),.UNSPECIFIED.);
#1118=B_SPLINE_CURVE_WITH_KNOTS('',2,(#72365,#72366,#72367),
 .UNSPECIFIED.,.F.,.F.,(3,3),(0.,1.),.UNSPECIFIED.);
#1119=B_SPLINE_CURVE_WITH_KNOTS('',2,(#72371,#72372,#72373),
 .UNSPECIFIED.,.F.,.F.,(3,3),(0.,1.),.UNSPECIFIED.);
#1120=B_SPLINE_CURVE_WITH_KNOTS('',2,(#72382,#72383,#72384),
 .UNSPECIFIED.,.F.,.F.,(3,3),(0.,1.),.UNSPECIFIED.);
#1121=B_SPLINE_CURVE_WITH_KNOTS('',2,(#72387,#72388,#72389),
 .UNSPECIFIED.,.F.,.F.,(3,3),(0.,1.),.UNSPECIFIED.);
#1122=B_SPLINE_CURVE_WITH_KNOTS('',2,(#72397,#72398,#72399),
 .UNSPECIFIED.,.F.,.F.,(3,3),(0.,1.),.UNSPECIFIED.);
#1123=B_SPLINE_CURVE_WITH_KNOTS('',2,(#72402,#72403,#72404),
 .UNSPECIFIED.,.F.,.F.,(3,3),(0.,1.),.UNSPECIFIED.);
#1124=B_SPLINE_CURVE_WITH_KNOTS('',2,(#72412,#72413,#72414),
 .UNSPECIFIED.,.F.,.F.,(3,3),(0.,1.),.UNSPECIFIED.);
#1125=B_SPLINE_CURVE_WITH_KNOTS('',2,(#72417,#72418,#72419),
 .UNSPECIFIED.,.F.,.F.,(3,3),(0.,1.),.UNSPECIFIED.);
#1126=B_SPLINE_CURVE_WITH_KNOTS('',2,(#72427,#72428,#72429),
 .UNSPECIFIED.,.F.,.F.,(3,3),(0.,1.),.UNSPECIFIED.);
#1127=B_SPLINE_CURVE_WITH_KNOTS('',2,(#72432,#72433,#72434),
 .UNSPECIFIED.,.F.,.F.,(3,3),(0.,1.),.UNSPECIFIED.);
#1128=B_SPLINE_CURVE_WITH_KNOTS('',2,(#72442,#72443,#72444),
 .UNSPECIFIED.,.F.,.F.,(3,3),(0.,1.),.UNSPECIFIED.);
#1129=B_SPLINE_CURVE_WITH_KNOTS('',2,(#72447,#72448,#72449),
 .UNSPECIFIED.,.F.,.F.,(3,3),(0.,1.),.UNSPECIFIED.);
#1130=B_SPLINE_CURVE_WITH_KNOTS('',2,(#72457,#72458,#72459),
 .UNSPECIFIED.,.F.,.F.,(3,3),(0.,1.),.UNSPECIFIED.);
#1131=B_SPLINE_CURVE_WITH_KNOTS('',2,(#72462,#72463,#72464),
 .UNSPECIFIED.,.F.,.F.,(3,3),(0.,1.),.UNSPECIFIED.);
#1132=B_SPLINE_CURVE_WITH_KNOTS('',2,(#72471,#72472,#72473),
 .UNSPECIFIED.,.F.,.F.,(3,3),(0.,1.),.UNSPECIFIED.);
#1133=B_SPLINE_CURVE_WITH_KNOTS('',2,(#72474,#72475,#72476),
 .UNSPECIFIED.,.F.,.F.,(3,3),(0.,1.),.UNSPECIFIED.);
#1134=B_SPLINE_CURVE_WITH_KNOTS('',2,(#72485,#72486,#72487),
 .UNSPECIFIED.,.F.,.F.,(3,3),(0.,1.),.UNSPECIFIED.);
#1135=B_SPLINE_CURVE_WITH_KNOTS('',2,(#72491,#72492,#72493),
 .UNSPECIFIED.,.F.,.F.,(3,3),(0.,1.),.UNSPECIFIED.);
#1136=B_SPLINE_CURVE_WITH_KNOTS('',2,(#72502,#72503,#72504),
 .UNSPECIFIED.,.F.,.F.,(3,3),(0.,1.),.UNSPECIFIED.);
#1137=B_SPLINE_CURVE_WITH_KNOTS('',2,(#72507,#72508,#72509),
 .UNSPECIFIED.,.F.,.F.,(3,3),(0.,1.),.UNSPECIFIED.);
#1138=B_SPLINE_CURVE_WITH_KNOTS('',2,(#72517,#72518,#72519),
 .UNSPECIFIED.,.F.,.F.,(3,3),(0.,1.),.UNSPECIFIED.);
#1139=B_SPLINE_CURVE_WITH_KNOTS('',2,(#72522,#72523,#72524),
 .UNSPECIFIED.,.F.,.F.,(3,3),(0.,1.),.UNSPECIFIED.);
#1140=B_SPLINE_CURVE_WITH_KNOTS('',2,(#72532,#72533,#72534),
 .UNSPECIFIED.,.F.,.F.,(3,3),(0.,1.),.UNSPECIFIED.);
#1141=B_SPLINE_CURVE_WITH_KNOTS('',2,(#72537,#72538,#72539),
 .UNSPECIFIED.,.F.,.F.,(3,3),(0.,1.),.UNSPECIFIED.);
#1142=B_SPLINE_CURVE_WITH_KNOTS('',2,(#72547,#72548,#72549),
 .UNSPECIFIED.,.F.,.F.,(3,3),(0.,1.),.UNSPECIFIED.);
#1143=B_SPLINE_CURVE_WITH_KNOTS('',2,(#72552,#72553,#72554),
 .UNSPECIFIED.,.F.,.F.,(3,3),(0.,1.),.UNSPECIFIED.);
#1144=B_SPLINE_CURVE_WITH_KNOTS('',2,(#72562,#72563,#72564),
 .UNSPECIFIED.,.F.,.F.,(3,3),(0.,1.),.UNSPECIFIED.);
#1145=B_SPLINE_CURVE_WITH_KNOTS('',2,(#72567,#72568,#72569),
 .UNSPECIFIED.,.F.,.F.,(3,3),(0.,1.),.UNSPECIFIED.);
#1146=B_SPLINE_CURVE_WITH_KNOTS('',2,(#72577,#72578,#72579),
 .UNSPECIFIED.,.F.,.F.,(3,3),(0.,1.),.UNSPECIFIED.);
#1147=B_SPLINE_CURVE_WITH_KNOTS('',2,(#72582,#72583,#72584),
 .UNSPECIFIED.,.F.,.F.,(3,3),(0.,1.),.UNSPECIFIED.);
#1148=B_SPLINE_CURVE_WITH_KNOTS('',2,(#72592,#72593,#72594),
 .UNSPECIFIED.,.F.,.F.,(3,3),(0.,1.),.UNSPECIFIED.);
#1149=B_SPLINE_CURVE_WITH_KNOTS('',2,(#72597,#72598,#72599),
 .UNSPECIFIED.,.F.,.F.,(3,3),(0.,1.),.UNSPECIFIED.);
#1150=B_SPLINE_CURVE_WITH_KNOTS('',2,(#72607,#72608,#72609),
 .UNSPECIFIED.,.F.,.F.,(3,3),(0.,1.),.UNSPECIFIED.);
#1151=B_SPLINE_CURVE_WITH_KNOTS('',2,(#72612,#72613,#72614),
 .UNSPECIFIED.,.F.,.F.,(3,3),(0.,1.),.UNSPECIFIED.);
#1152=B_SPLINE_CURVE_WITH_KNOTS('',2,(#72622,#72623,#72624),
 .UNSPECIFIED.,.F.,.F.,(3,3),(0.,1.),.UNSPECIFIED.);
#1153=B_SPLINE_CURVE_WITH_KNOTS('',2,(#72627,#72628,#72629),
 .UNSPECIFIED.,.F.,.F.,(3,3),(0.,1.),.UNSPECIFIED.);
#1154=B_SPLINE_CURVE_WITH_KNOTS('',2,(#72637,#72638,#72639),
 .UNSPECIFIED.,.F.,.F.,(3,3),(0.,1.),.UNSPECIFIED.);
#1155=B_SPLINE_CURVE_WITH_KNOTS('',2,(#72642,#72643,#72644),
 .UNSPECIFIED.,.F.,.F.,(3,3),(0.,1.),.UNSPECIFIED.);
#1156=B_SPLINE_CURVE_WITH_KNOTS('',2,(#72651,#72652,#72653),
 .UNSPECIFIED.,.F.,.F.,(3,3),(0.,1.),.UNSPECIFIED.);
#1157=B_SPLINE_CURVE_WITH_KNOTS('',2,(#72654,#72655,#72656),
 .UNSPECIFIED.,.F.,.F.,(3,3),(0.,1.),.UNSPECIFIED.);
#1158=B_SPLINE_CURVE_WITH_KNOTS('',2,(#72674,#72675,#72676),
 .UNSPECIFIED.,.F.,.F.,(3,3),(0.,1.),.UNSPECIFIED.);
#1159=B_SPLINE_CURVE_WITH_KNOTS('',2,(#72679,#72680,#72681),
 .UNSPECIFIED.,.F.,.F.,(3,3),(0.,1.),.UNSPECIFIED.);
#1160=B_SPLINE_CURVE_WITH_KNOTS('',2,(#72689,#72690,#72691),
 .UNSPECIFIED.,.F.,.F.,(3,3),(0.,1.),.UNSPECIFIED.);
#1161=B_SPLINE_CURVE_WITH_KNOTS('',2,(#72694,#72695,#72696),
 .UNSPECIFIED.,.F.,.F.,(3,3),(0.,1.),.UNSPECIFIED.);
#1162=B_SPLINE_CURVE_WITH_KNOTS('',2,(#72710,#72711,#72712),
 .UNSPECIFIED.,.F.,.F.,(3,3),(0.,1.),.UNSPECIFIED.);
#1163=B_SPLINE_CURVE_WITH_KNOTS('',2,(#72715,#72716,#72717),
 .UNSPECIFIED.,.F.,.F.,(3,3),(0.,1.),.UNSPECIFIED.);
#1164=B_SPLINE_CURVE_WITH_KNOTS('',2,(#72725,#72726,#72727),
 .UNSPECIFIED.,.F.,.F.,(3,3),(0.,1.),.UNSPECIFIED.);
#1165=B_SPLINE_CURVE_WITH_KNOTS('',2,(#72730,#72731,#72732),
 .UNSPECIFIED.,.F.,.F.,(3,3),(0.,1.),.UNSPECIFIED.);
#1166=B_SPLINE_CURVE_WITH_KNOTS('',2,(#72758,#72759,#72760),
 .UNSPECIFIED.,.F.,.F.,(3,3),(0.,1.),.UNSPECIFIED.);
#1167=B_SPLINE_CURVE_WITH_KNOTS('',2,(#72764,#72765,#72766),
 .UNSPECIFIED.,.F.,.F.,(3,3),(0.,1.),.UNSPECIFIED.);
#1168=B_SPLINE_CURVE_WITH_KNOTS('',2,(#72775,#72776,#72777),
 .UNSPECIFIED.,.F.,.F.,(3,3),(0.,1.),.UNSPECIFIED.);
#1169=B_SPLINE_CURVE_WITH_KNOTS('',2,(#72780,#72781,#72782),
 .UNSPECIFIED.,.F.,.F.,(3,3),(0.,1.),.UNSPECIFIED.);
#1170=B_SPLINE_CURVE_WITH_KNOTS('',2,(#72790,#72791,#72792),
 .UNSPECIFIED.,.F.,.F.,(3,3),(0.,1.),.UNSPECIFIED.);
#1171=B_SPLINE_CURVE_WITH_KNOTS('',2,(#72795,#72796,#72797),
 .UNSPECIFIED.,.F.,.F.,(3,3),(0.,1.),.UNSPECIFIED.);
#1172=B_SPLINE_CURVE_WITH_KNOTS('',2,(#72805,#72806,#72807),
 .UNSPECIFIED.,.F.,.F.,(3,3),(0.,1.),.UNSPECIFIED.);
#1173=B_SPLINE_CURVE_WITH_KNOTS('',2,(#72810,#72811,#72812),
 .UNSPECIFIED.,.F.,.F.,(3,3),(0.,1.),.UNSPECIFIED.);
#1174=B_SPLINE_CURVE_WITH_KNOTS('',2,(#72820,#72821,#72822),
 .UNSPECIFIED.,.F.,.F.,(3,3),(0.,1.),.UNSPECIFIED.);
#1175=B_SPLINE_CURVE_WITH_KNOTS('',2,(#72825,#72826,#72827),
 .UNSPECIFIED.,.F.,.F.,(3,3),(0.,1.),.UNSPECIFIED.);
#1176=B_SPLINE_CURVE_WITH_KNOTS('',2,(#72835,#72836,#72837),
 .UNSPECIFIED.,.F.,.F.,(3,3),(0.,1.),.UNSPECIFIED.);
#1177=B_SPLINE_CURVE_WITH_KNOTS('',2,(#72840,#72841,#72842),
 .UNSPECIFIED.,.F.,.F.,(3,3),(0.,1.),.UNSPECIFIED.);
#1178=B_SPLINE_CURVE_WITH_KNOTS('',2,(#72850,#72851,#72852),
 .UNSPECIFIED.,.F.,.F.,(3,3),(0.,1.),.UNSPECIFIED.);
#1179=B_SPLINE_CURVE_WITH_KNOTS('',2,(#72855,#72856,#72857),
 .UNSPECIFIED.,.F.,.F.,(3,3),(0.,1.),.UNSPECIFIED.);
#1180=B_SPLINE_CURVE_WITH_KNOTS('',2,(#72864,#72865,#72866),
 .UNSPECIFIED.,.F.,.F.,(3,3),(0.,1.),.UNSPECIFIED.);
#1181=B_SPLINE_CURVE_WITH_KNOTS('',2,(#72867,#72868,#72869),
 .UNSPECIFIED.,.F.,.F.,(3,3),(0.,1.),.UNSPECIFIED.);
#1182=B_SPLINE_CURVE_WITH_KNOTS('',2,(#72878,#72879,#72880),
 .UNSPECIFIED.,.F.,.F.,(3,3),(0.,1.),.UNSPECIFIED.);
#1183=B_SPLINE_CURVE_WITH_KNOTS('',2,(#72884,#72885,#72886),
 .UNSPECIFIED.,.F.,.F.,(3,3),(0.,1.),.UNSPECIFIED.);
#1184=B_SPLINE_CURVE_WITH_KNOTS('',2,(#72895,#72896,#72897),
 .UNSPECIFIED.,.F.,.F.,(3,3),(0.,1.),.UNSPECIFIED.);
#1185=B_SPLINE_CURVE_WITH_KNOTS('',2,(#72900,#72901,#72902),
 .UNSPECIFIED.,.F.,.F.,(3,3),(0.,1.),.UNSPECIFIED.);
#1186=B_SPLINE_CURVE_WITH_KNOTS('',2,(#72910,#72911,#72912),
 .UNSPECIFIED.,.F.,.F.,(3,3),(0.,1.),.UNSPECIFIED.);
#1187=B_SPLINE_CURVE_WITH_KNOTS('',2,(#72915,#72916,#72917),
 .UNSPECIFIED.,.F.,.F.,(3,3),(0.,1.),.UNSPECIFIED.);
#1188=B_SPLINE_CURVE_WITH_KNOTS('',2,(#72925,#72926,#72927),
 .UNSPECIFIED.,.F.,.F.,(3,3),(0.,1.),.UNSPECIFIED.);
#1189=B_SPLINE_CURVE_WITH_KNOTS('',2,(#72930,#72931,#72932),
 .UNSPECIFIED.,.F.,.F.,(3,3),(0.,1.),.UNSPECIFIED.);
#1190=B_SPLINE_CURVE_WITH_KNOTS('',2,(#72940,#72941,#72942),
 .UNSPECIFIED.,.F.,.F.,(3,3),(0.,1.),.UNSPECIFIED.);
#1191=B_SPLINE_CURVE_WITH_KNOTS('',2,(#72945,#72946,#72947),
 .UNSPECIFIED.,.F.,.F.,(3,3),(0.,1.),.UNSPECIFIED.);
#1192=B_SPLINE_CURVE_WITH_KNOTS('',2,(#72955,#72956,#72957),
 .UNSPECIFIED.,.F.,.F.,(3,3),(0.,1.),.UNSPECIFIED.);
#1193=B_SPLINE_CURVE_WITH_KNOTS('',2,(#72960,#72961,#72962),
 .UNSPECIFIED.,.F.,.F.,(3,3),(0.,1.),.UNSPECIFIED.);
#1194=B_SPLINE_CURVE_WITH_KNOTS('',2,(#72970,#72971,#72972),
 .UNSPECIFIED.,.F.,.F.,(3,3),(0.,1.),.UNSPECIFIED.);
#1195=B_SPLINE_CURVE_WITH_KNOTS('',2,(#72975,#72976,#72977),
 .UNSPECIFIED.,.F.,.F.,(3,3),(0.,1.),.UNSPECIFIED.);
#1196=B_SPLINE_CURVE_WITH_KNOTS('',2,(#72985,#72986,#72987),
 .UNSPECIFIED.,.F.,.F.,(3,3),(0.,1.),.UNSPECIFIED.);
#1197=B_SPLINE_CURVE_WITH_KNOTS('',2,(#72990,#72991,#72992),
 .UNSPECIFIED.,.F.,.F.,(3,3),(0.,1.),.UNSPECIFIED.);
#1198=B_SPLINE_CURVE_WITH_KNOTS('',2,(#73000,#73001,#73002),
 .UNSPECIFIED.,.F.,.F.,(3,3),(0.,1.),.UNSPECIFIED.);
#1199=B_SPLINE_CURVE_WITH_KNOTS('',2,(#73005,#73006,#73007),
 .UNSPECIFIED.,.F.,.F.,(3,3),(0.,1.),.UNSPECIFIED.);
#1200=B_SPLINE_CURVE_WITH_KNOTS('',2,(#73015,#73016,#73017),
 .UNSPECIFIED.,.F.,.F.,(3,3),(0.,1.),.UNSPECIFIED.);
#1201=B_SPLINE_CURVE_WITH_KNOTS('',2,(#73020,#73021,#73022),
 .UNSPECIFIED.,.F.,.F.,(3,3),(0.,1.),.UNSPECIFIED.);
#1202=B_SPLINE_CURVE_WITH_KNOTS('',2,(#73030,#73031,#73032),
 .UNSPECIFIED.,.F.,.F.,(3,3),(0.,1.),.UNSPECIFIED.);
#1203=B_SPLINE_CURVE_WITH_KNOTS('',2,(#73035,#73036,#73037),
 .UNSPECIFIED.,.F.,.F.,(3,3),(0.,1.),.UNSPECIFIED.);
#1204=B_SPLINE_CURVE_WITH_KNOTS('',2,(#73044,#73045,#73046),
 .UNSPECIFIED.,.F.,.F.,(3,3),(0.,1.),.UNSPECIFIED.);
#1205=B_SPLINE_CURVE_WITH_KNOTS('',2,(#73047,#73048,#73049),
 .UNSPECIFIED.,.F.,.F.,(3,3),(0.,1.),.UNSPECIFIED.);
#1206=B_SPLINE_CURVE_WITH_KNOTS('',2,(#73059,#73060,#73061),
 .UNSPECIFIED.,.F.,.F.,(3,3),(0.,1.),.UNSPECIFIED.);
#1207=B_SPLINE_CURVE_WITH_KNOTS('',2,(#73065,#73066,#73067),
 .UNSPECIFIED.,.F.,.F.,(3,3),(0.,1.),.UNSPECIFIED.);
#1208=B_SPLINE_CURVE_WITH_KNOTS('',2,(#73076,#73077,#73078),
 .UNSPECIFIED.,.F.,.F.,(3,3),(0.,1.),.UNSPECIFIED.);
#1209=B_SPLINE_CURVE_WITH_KNOTS('',2,(#73081,#73082,#73083),
 .UNSPECIFIED.,.F.,.F.,(3,3),(0.,1.),.UNSPECIFIED.);
#1210=B_SPLINE_CURVE_WITH_KNOTS('',2,(#73091,#73092,#73093),
 .UNSPECIFIED.,.F.,.F.,(3,3),(0.,1.),.UNSPECIFIED.);
#1211=B_SPLINE_CURVE_WITH_KNOTS('',2,(#73096,#73097,#73098),
 .UNSPECIFIED.,.F.,.F.,(3,3),(0.,1.),.UNSPECIFIED.);
#1212=B_SPLINE_CURVE_WITH_KNOTS('',2,(#73106,#73107,#73108),
 .UNSPECIFIED.,.F.,.F.,(3,3),(0.,1.),.UNSPECIFIED.);
#1213=B_SPLINE_CURVE_WITH_KNOTS('',2,(#73111,#73112,#73113),
 .UNSPECIFIED.,.F.,.F.,(3,3),(0.,1.),.UNSPECIFIED.);
#1214=B_SPLINE_CURVE_WITH_KNOTS('',2,(#73121,#73122,#73123),
 .UNSPECIFIED.,.F.,.F.,(3,3),(0.,1.),.UNSPECIFIED.);
#1215=B_SPLINE_CURVE_WITH_KNOTS('',2,(#73126,#73127,#73128),
 .UNSPECIFIED.,.F.,.F.,(3,3),(0.,1.),.UNSPECIFIED.);
#1216=B_SPLINE_CURVE_WITH_KNOTS('',2,(#73136,#73137,#73138),
 .UNSPECIFIED.,.F.,.F.,(3,3),(0.,1.),.UNSPECIFIED.);
#1217=B_SPLINE_CURVE_WITH_KNOTS('',2,(#73141,#73142,#73143),
 .UNSPECIFIED.,.F.,.F.,(3,3),(0.,1.),.UNSPECIFIED.);
#1218=B_SPLINE_CURVE_WITH_KNOTS('',2,(#73151,#73152,#73153),
 .UNSPECIFIED.,.F.,.F.,(3,3),(0.,1.),.UNSPECIFIED.);
#1219=B_SPLINE_CURVE_WITH_KNOTS('',2,(#73156,#73157,#73158),
 .UNSPECIFIED.,.F.,.F.,(3,3),(0.,1.),.UNSPECIFIED.);
#1220=B_SPLINE_CURVE_WITH_KNOTS('',2,(#73166,#73167,#73168),
 .UNSPECIFIED.,.F.,.F.,(3,3),(0.,1.),.UNSPECIFIED.);
#1221=B_SPLINE_CURVE_WITH_KNOTS('',2,(#73171,#73172,#73173),
 .UNSPECIFIED.,.F.,.F.,(3,3),(0.,1.),.UNSPECIFIED.);
#1222=B_SPLINE_CURVE_WITH_KNOTS('',2,(#73181,#73182,#73183),
 .UNSPECIFIED.,.F.,.F.,(3,3),(0.,1.),.UNSPECIFIED.);
#1223=B_SPLINE_CURVE_WITH_KNOTS('',2,(#73186,#73187,#73188),
 .UNSPECIFIED.,.F.,.F.,(3,3),(0.,1.),.UNSPECIFIED.);
#1224=B_SPLINE_CURVE_WITH_KNOTS('',2,(#73202,#73203,#73204),
 .UNSPECIFIED.,.F.,.F.,(3,3),(0.,1.),.UNSPECIFIED.);
#1225=B_SPLINE_CURVE_WITH_KNOTS('',2,(#73207,#73208,#73209),
 .UNSPECIFIED.,.F.,.F.,(3,3),(0.,1.),.UNSPECIFIED.);
#1226=B_SPLINE_CURVE_WITH_KNOTS('',2,(#73217,#73218,#73219),
 .UNSPECIFIED.,.F.,.F.,(3,3),(0.,1.),.UNSPECIFIED.);
#1227=B_SPLINE_CURVE_WITH_KNOTS('',2,(#73222,#73223,#73224),
 .UNSPECIFIED.,.F.,.F.,(3,3),(0.,1.),.UNSPECIFIED.);
#1228=B_SPLINE_CURVE_WITH_KNOTS('',2,(#73232,#73233,#73234),
 .UNSPECIFIED.,.F.,.F.,(3,3),(0.,1.),.UNSPECIFIED.);
#1229=B_SPLINE_CURVE_WITH_KNOTS('',2,(#73237,#73238,#73239),
 .UNSPECIFIED.,.F.,.F.,(3,3),(0.,1.),.UNSPECIFIED.);
#1230=B_SPLINE_CURVE_WITH_KNOTS('',2,(#73247,#73248,#73249),
 .UNSPECIFIED.,.F.,.F.,(3,3),(0.,1.),.UNSPECIFIED.);
#1231=B_SPLINE_CURVE_WITH_KNOTS('',2,(#73252,#73253,#73254),
 .UNSPECIFIED.,.F.,.F.,(3,3),(0.,1.),.UNSPECIFIED.);
#1232=B_SPLINE_CURVE_WITH_KNOTS('',2,(#73262,#73263,#73264),
 .UNSPECIFIED.,.F.,.F.,(3,3),(0.,1.),.UNSPECIFIED.);
#1233=B_SPLINE_CURVE_WITH_KNOTS('',2,(#73267,#73268,#73269),
 .UNSPECIFIED.,.F.,.F.,(3,3),(0.,1.),.UNSPECIFIED.);
#1234=B_SPLINE_CURVE_WITH_KNOTS('',2,(#73277,#73278,#73279),
 .UNSPECIFIED.,.F.,.F.,(3,3),(0.,1.),.UNSPECIFIED.);
#1235=B_SPLINE_CURVE_WITH_KNOTS('',2,(#73282,#73283,#73284),
 .UNSPECIFIED.,.F.,.F.,(3,3),(0.,1.),.UNSPECIFIED.);
#1236=B_SPLINE_CURVE_WITH_KNOTS('',2,(#73292,#73293,#73294),
 .UNSPECIFIED.,.F.,.F.,(3,3),(0.,1.),.UNSPECIFIED.);
#1237=B_SPLINE_CURVE_WITH_KNOTS('',2,(#73297,#73298,#73299),
 .UNSPECIFIED.,.F.,.F.,(3,3),(0.,1.),.UNSPECIFIED.);
#1238=B_SPLINE_CURVE_WITH_KNOTS('',2,(#73307,#73308,#73309),
 .UNSPECIFIED.,.F.,.F.,(3,3),(0.,1.),.UNSPECIFIED.);
#1239=B_SPLINE_CURVE_WITH_KNOTS('',2,(#73312,#73313,#73314),
 .UNSPECIFIED.,.F.,.F.,(3,3),(0.,1.),.UNSPECIFIED.);
#1240=B_SPLINE_CURVE_WITH_KNOTS('',2,(#73322,#73323,#73324),
 .UNSPECIFIED.,.F.,.F.,(3,3),(0.,1.),.UNSPECIFIED.);
#1241=B_SPLINE_CURVE_WITH_KNOTS('',2,(#73327,#73328,#73329),
 .UNSPECIFIED.,.F.,.F.,(3,3),(0.,1.),.UNSPECIFIED.);
#1242=B_SPLINE_CURVE_WITH_KNOTS('',2,(#73355,#73356,#73357),
 .UNSPECIFIED.,.F.,.F.,(3,3),(0.,1.),.UNSPECIFIED.);
#1243=B_SPLINE_CURVE_WITH_KNOTS('',2,(#73361,#73362,#73363),
 .UNSPECIFIED.,.F.,.F.,(3,3),(0.,1.),.UNSPECIFIED.);
#1244=B_SPLINE_CURVE_WITH_KNOTS('',2,(#73372,#73373,#73374),
 .UNSPECIFIED.,.F.,.F.,(3,3),(0.,1.),.UNSPECIFIED.);
#1245=B_SPLINE_CURVE_WITH_KNOTS('',2,(#73377,#73378,#73379),
 .UNSPECIFIED.,.F.,.F.,(3,3),(0.,1.),.UNSPECIFIED.);
#1246=B_SPLINE_CURVE_WITH_KNOTS('',2,(#73387,#73388,#73389),
 .UNSPECIFIED.,.F.,.F.,(3,3),(0.,1.),.UNSPECIFIED.);
#1247=B_SPLINE_CURVE_WITH_KNOTS('',2,(#73392,#73393,#73394),
 .UNSPECIFIED.,.F.,.F.,(3,3),(0.,1.),.UNSPECIFIED.);
#1248=B_SPLINE_CURVE_WITH_KNOTS('',2,(#73402,#73403,#73404),
 .UNSPECIFIED.,.F.,.F.,(3,3),(0.,1.),.UNSPECIFIED.);
#1249=B_SPLINE_CURVE_WITH_KNOTS('',2,(#73407,#73408,#73409),
 .UNSPECIFIED.,.F.,.F.,(3,3),(0.,1.),.UNSPECIFIED.);
#1250=B_SPLINE_CURVE_WITH_KNOTS('',2,(#73417,#73418,#73419),
 .UNSPECIFIED.,.F.,.F.,(3,3),(0.,1.),.UNSPECIFIED.);
#1251=B_SPLINE_CURVE_WITH_KNOTS('',2,(#73422,#73423,#73424),
 .UNSPECIFIED.,.F.,.F.,(3,3),(0.,1.),.UNSPECIFIED.);
#1252=B_SPLINE_CURVE_WITH_KNOTS('',2,(#73432,#73433,#73434),
 .UNSPECIFIED.,.F.,.F.,(3,3),(0.,1.),.UNSPECIFIED.);
#1253=B_SPLINE_CURVE_WITH_KNOTS('',2,(#73437,#73438,#73439),
 .UNSPECIFIED.,.F.,.F.,(3,3),(0.,1.),.UNSPECIFIED.);
#1254=B_SPLINE_CURVE_WITH_KNOTS('',2,(#73447,#73448,#73449),
 .UNSPECIFIED.,.F.,.F.,(3,3),(0.,1.),.UNSPECIFIED.);
#1255=B_SPLINE_CURVE_WITH_KNOTS('',2,(#73452,#73453,#73454),
 .UNSPECIFIED.,.F.,.F.,(3,3),(0.,1.),.UNSPECIFIED.);
#1256=B_SPLINE_CURVE_WITH_KNOTS('',2,(#73461,#73462,#73463),
 .UNSPECIFIED.,.F.,.F.,(3,3),(0.,1.),.UNSPECIFIED.);
#1257=B_SPLINE_CURVE_WITH_KNOTS('',2,(#73464,#73465,#73466),
 .UNSPECIFIED.,.F.,.F.,(3,3),(0.,1.),.UNSPECIFIED.);
#1258=B_SPLINE_CURVE_WITH_KNOTS('',2,(#73475,#73476,#73477),
 .UNSPECIFIED.,.F.,.F.,(3,3),(0.,1.),.UNSPECIFIED.);
#1259=B_SPLINE_CURVE_WITH_KNOTS('',2,(#73481,#73482,#73483),
 .UNSPECIFIED.,.F.,.F.,(3,3),(0.,1.),.UNSPECIFIED.);
#1260=B_SPLINE_CURVE_WITH_KNOTS('',2,(#73492,#73493,#73494),
 .UNSPECIFIED.,.F.,.F.,(3,3),(0.,1.),.UNSPECIFIED.);
#1261=B_SPLINE_CURVE_WITH_KNOTS('',2,(#73497,#73498,#73499),
 .UNSPECIFIED.,.F.,.F.,(3,3),(0.,1.),.UNSPECIFIED.);
#1262=B_SPLINE_CURVE_WITH_KNOTS('',2,(#73507,#73508,#73509),
 .UNSPECIFIED.,.F.,.F.,(3,3),(0.,1.),.UNSPECIFIED.);
#1263=B_SPLINE_CURVE_WITH_KNOTS('',2,(#73512,#73513,#73514),
 .UNSPECIFIED.,.F.,.F.,(3,3),(0.,1.),.UNSPECIFIED.);
#1264=B_SPLINE_CURVE_WITH_KNOTS('',2,(#73522,#73523,#73524),
 .UNSPECIFIED.,.F.,.F.,(3,3),(0.,1.),.UNSPECIFIED.);
#1265=B_SPLINE_CURVE_WITH_KNOTS('',2,(#73527,#73528,#73529),
 .UNSPECIFIED.,.F.,.F.,(3,3),(0.,1.),.UNSPECIFIED.);
#1266=B_SPLINE_CURVE_WITH_KNOTS('',2,(#73537,#73538,#73539),
 .UNSPECIFIED.,.F.,.F.,(3,3),(0.,1.),.UNSPECIFIED.);
#1267=B_SPLINE_CURVE_WITH_KNOTS('',2,(#73542,#73543,#73544),
 .UNSPECIFIED.,.F.,.F.,(3,3),(0.,1.),.UNSPECIFIED.);
#1268=B_SPLINE_CURVE_WITH_KNOTS('',2,(#73552,#73553,#73554),
 .UNSPECIFIED.,.F.,.F.,(3,3),(0.,1.),.UNSPECIFIED.);
#1269=B_SPLINE_CURVE_WITH_KNOTS('',2,(#73557,#73558,#73559),
 .UNSPECIFIED.,.F.,.F.,(3,3),(0.,1.),.UNSPECIFIED.);
#1270=B_SPLINE_CURVE_WITH_KNOTS('',2,(#73567,#73568,#73569),
 .UNSPECIFIED.,.F.,.F.,(3,3),(0.,1.),.UNSPECIFIED.);
#1271=B_SPLINE_CURVE_WITH_KNOTS('',2,(#73572,#73573,#73574),
 .UNSPECIFIED.,.F.,.F.,(3,3),(0.,1.),.UNSPECIFIED.);
#1272=B_SPLINE_CURVE_WITH_KNOTS('',2,(#73582,#73583,#73584),
 .UNSPECIFIED.,.F.,.F.,(3,3),(0.,1.),.UNSPECIFIED.);
#1273=B_SPLINE_CURVE_WITH_KNOTS('',2,(#73587,#73588,#73589),
 .UNSPECIFIED.,.F.,.F.,(3,3),(0.,1.),.UNSPECIFIED.);
#1274=B_SPLINE_CURVE_WITH_KNOTS('',2,(#73597,#73598,#73599),
 .UNSPECIFIED.,.F.,.F.,(3,3),(0.,1.),.UNSPECIFIED.);
#1275=B_SPLINE_CURVE_WITH_KNOTS('',2,(#73602,#73603,#73604),
 .UNSPECIFIED.,.F.,.F.,(3,3),(0.,1.),.UNSPECIFIED.);
#1276=B_SPLINE_CURVE_WITH_KNOTS('',2,(#73612,#73613,#73614),
 .UNSPECIFIED.,.F.,.F.,(3,3),(0.,1.),.UNSPECIFIED.);
#1277=B_SPLINE_CURVE_WITH_KNOTS('',2,(#73617,#73618,#73619),
 .UNSPECIFIED.,.F.,.F.,(3,3),(0.,1.),.UNSPECIFIED.);
#1278=B_SPLINE_CURVE_WITH_KNOTS('',2,(#73627,#73628,#73629),
 .UNSPECIFIED.,.F.,.F.,(3,3),(0.,1.),.UNSPECIFIED.);
#1279=B_SPLINE_CURVE_WITH_KNOTS('',2,(#73632,#73633,#73634),
 .UNSPECIFIED.,.F.,.F.,(3,3),(0.,1.),.UNSPECIFIED.);
#1280=B_SPLINE_CURVE_WITH_KNOTS('',2,(#73641,#73642,#73643),
 .UNSPECIFIED.,.F.,.F.,(3,3),(0.,1.),.UNSPECIFIED.);
#1281=B_SPLINE_CURVE_WITH_KNOTS('',2,(#73644,#73645,#73646),
 .UNSPECIFIED.,.F.,.F.,(3,3),(0.,1.),.UNSPECIFIED.);
#1282=B_SPLINE_CURVE_WITH_KNOTS('',2,(#73656,#73657,#73658),
 .UNSPECIFIED.,.F.,.F.,(3,3),(0.,1.),.UNSPECIFIED.);
#1283=B_SPLINE_CURVE_WITH_KNOTS('',2,(#73662,#73663,#73664),
 .UNSPECIFIED.,.F.,.F.,(3,3),(0.,1.),.UNSPECIFIED.);
#1284=B_SPLINE_CURVE_WITH_KNOTS('',2,(#73673,#73674,#73675),
 .UNSPECIFIED.,.F.,.F.,(3,3),(0.,1.),.UNSPECIFIED.);
#1285=B_SPLINE_CURVE_WITH_KNOTS('',2,(#73678,#73679,#73680),
 .UNSPECIFIED.,.F.,.F.,(3,3),(0.,1.),.UNSPECIFIED.);
#1286=B_SPLINE_CURVE_WITH_KNOTS('',2,(#73688,#73689,#73690),
 .UNSPECIFIED.,.F.,.F.,(3,3),(0.,1.),.UNSPECIFIED.);
#1287=B_SPLINE_CURVE_WITH_KNOTS('',2,(#73693,#73694,#73695),
 .UNSPECIFIED.,.F.,.F.,(3,3),(0.,1.),.UNSPECIFIED.);
#1288=B_SPLINE_CURVE_WITH_KNOTS('',2,(#73703,#73704,#73705),
 .UNSPECIFIED.,.F.,.F.,(3,3),(0.,1.),.UNSPECIFIED.);
#1289=B_SPLINE_CURVE_WITH_KNOTS('',2,(#73708,#73709,#73710),
 .UNSPECIFIED.,.F.,.F.,(3,3),(0.,1.),.UNSPECIFIED.);
#1290=B_SPLINE_CURVE_WITH_KNOTS('',2,(#73718,#73719,#73720),
 .UNSPECIFIED.,.F.,.F.,(3,3),(0.,1.),.UNSPECIFIED.);
#1291=B_SPLINE_CURVE_WITH_KNOTS('',2,(#73723,#73724,#73725),
 .UNSPECIFIED.,.F.,.F.,(3,3),(0.,1.),.UNSPECIFIED.);
#1292=B_SPLINE_CURVE_WITH_KNOTS('',2,(#73733,#73734,#73735),
 .UNSPECIFIED.,.F.,.F.,(3,3),(0.,1.),.UNSPECIFIED.);
#1293=B_SPLINE_CURVE_WITH_KNOTS('',2,(#73738,#73739,#73740),
 .UNSPECIFIED.,.F.,.F.,(3,3),(0.,1.),.UNSPECIFIED.);
#1294=B_SPLINE_CURVE_WITH_KNOTS('',2,(#73748,#73749,#73750),
 .UNSPECIFIED.,.F.,.F.,(3,3),(0.,1.),.UNSPECIFIED.);
#1295=B_SPLINE_CURVE_WITH_KNOTS('',2,(#73753,#73754,#73755),
 .UNSPECIFIED.,.F.,.F.,(3,3),(0.,1.),.UNSPECIFIED.);
#1296=B_SPLINE_CURVE_WITH_KNOTS('',2,(#73763,#73764,#73765),
 .UNSPECIFIED.,.F.,.F.,(3,3),(0.,1.),.UNSPECIFIED.);
#1297=B_SPLINE_CURVE_WITH_KNOTS('',2,(#73768,#73769,#73770),
 .UNSPECIFIED.,.F.,.F.,(3,3),(0.,1.),.UNSPECIFIED.);
#1298=B_SPLINE_CURVE_WITH_KNOTS('',2,(#73778,#73779,#73780),
 .UNSPECIFIED.,.F.,.F.,(3,3),(0.,1.),.UNSPECIFIED.);
#1299=B_SPLINE_CURVE_WITH_KNOTS('',2,(#73783,#73784,#73785),
 .UNSPECIFIED.,.F.,.F.,(3,3),(0.,1.),.UNSPECIFIED.);
#1300=B_SPLINE_CURVE_WITH_KNOTS('',2,(#73793,#73794,#73795),
 .UNSPECIFIED.,.F.,.F.,(3,3),(0.,1.),.UNSPECIFIED.);
#1301=B_SPLINE_CURVE_WITH_KNOTS('',2,(#73798,#73799,#73800),
 .UNSPECIFIED.,.F.,.F.,(3,3),(0.,1.),.UNSPECIFIED.);
#1302=B_SPLINE_CURVE_WITH_KNOTS('',2,(#73808,#73809,#73810),
 .UNSPECIFIED.,.F.,.F.,(3,3),(0.,1.),.UNSPECIFIED.);
#1303=B_SPLINE_CURVE_WITH_KNOTS('',2,(#73813,#73814,#73815),
 .UNSPECIFIED.,.F.,.F.,(3,3),(0.,1.),.UNSPECIFIED.);
#1304=B_SPLINE_CURVE_WITH_KNOTS('',2,(#73823,#73824,#73825),
 .UNSPECIFIED.,.F.,.F.,(3,3),(0.,1.),.UNSPECIFIED.);
#1305=B_SPLINE_CURVE_WITH_KNOTS('',2,(#73828,#73829,#73830),
 .UNSPECIFIED.,.F.,.F.,(3,3),(0.,1.),.UNSPECIFIED.);
#1306=B_SPLINE_CURVE_WITH_KNOTS('',2,(#73844,#73845,#73846),
 .UNSPECIFIED.,.F.,.F.,(3,3),(0.,1.),.UNSPECIFIED.);
#1307=B_SPLINE_CURVE_WITH_KNOTS('',2,(#73849,#73850,#73851),
 .UNSPECIFIED.,.F.,.F.,(3,3),(0.,1.),.UNSPECIFIED.);
#1308=B_SPLINE_CURVE_WITH_KNOTS('',2,(#73859,#73860,#73861),
 .UNSPECIFIED.,.F.,.F.,(3,3),(0.,1.),.UNSPECIFIED.);
#1309=B_SPLINE_CURVE_WITH_KNOTS('',2,(#73864,#73865,#73866),
 .UNSPECIFIED.,.F.,.F.,(3,3),(0.,1.),.UNSPECIFIED.);
#1310=B_SPLINE_CURVE_WITH_KNOTS('',2,(#73874,#73875,#73876),
 .UNSPECIFIED.,.F.,.F.,(3,3),(0.,1.),.UNSPECIFIED.);
#1311=B_SPLINE_CURVE_WITH_KNOTS('',2,(#73879,#73880,#73881),
 .UNSPECIFIED.,.F.,.F.,(3,3),(0.,1.),.UNSPECIFIED.);
#1312=B_SPLINE_CURVE_WITH_KNOTS('',2,(#73889,#73890,#73891),
 .UNSPECIFIED.,.F.,.F.,(3,3),(0.,1.),.UNSPECIFIED.);
#1313=B_SPLINE_CURVE_WITH_KNOTS('',2,(#73894,#73895,#73896),
 .UNSPECIFIED.,.F.,.F.,(3,3),(0.,1.),.UNSPECIFIED.);
#1314=B_SPLINE_CURVE_WITH_KNOTS('',2,(#73904,#73905,#73906),
 .UNSPECIFIED.,.F.,.F.,(3,3),(0.,1.),.UNSPECIFIED.);
#1315=B_SPLINE_CURVE_WITH_KNOTS('',2,(#73909,#73910,#73911),
 .UNSPECIFIED.,.F.,.F.,(3,3),(0.,1.),.UNSPECIFIED.);
#1316=B_SPLINE_CURVE_WITH_KNOTS('',2,(#73919,#73920,#73921),
 .UNSPECIFIED.,.F.,.F.,(3,3),(0.,1.),.UNSPECIFIED.);
#1317=B_SPLINE_CURVE_WITH_KNOTS('',2,(#73924,#73925,#73926),
 .UNSPECIFIED.,.F.,.F.,(3,3),(0.,1.),.UNSPECIFIED.);
#1318=B_SPLINE_CURVE_WITH_KNOTS('',2,(#73934,#73935,#73936),
 .UNSPECIFIED.,.F.,.F.,(3,3),(0.,1.),.UNSPECIFIED.);
#1319=B_SPLINE_CURVE_WITH_KNOTS('',2,(#73939,#73940,#73941),
 .UNSPECIFIED.,.F.,.F.,(3,3),(0.,1.),.UNSPECIFIED.);
#1320=B_SPLINE_CURVE_WITH_KNOTS('',2,(#73955,#73956,#73957),
 .UNSPECIFIED.,.F.,.F.,(3,3),(0.,1.),.UNSPECIFIED.);
#1321=B_SPLINE_CURVE_WITH_KNOTS('',2,(#73960,#73961,#73962),
 .UNSPECIFIED.,.F.,.F.,(3,3),(0.,1.),.UNSPECIFIED.);
#1322=B_SPLINE_CURVE_WITH_KNOTS('',2,(#73970,#73971,#73972),
 .UNSPECIFIED.,.F.,.F.,(3,3),(0.,1.),.UNSPECIFIED.);
#1323=B_SPLINE_CURVE_WITH_KNOTS('',2,(#73975,#73976,#73977),
 .UNSPECIFIED.,.F.,.F.,(3,3),(0.,1.),.UNSPECIFIED.);
#1324=B_SPLINE_CURVE_WITH_KNOTS('',2,(#73985,#73986,#73987),
 .UNSPECIFIED.,.F.,.F.,(3,3),(0.,1.),.UNSPECIFIED.);
#1325=B_SPLINE_CURVE_WITH_KNOTS('',2,(#73990,#73991,#73992),
 .UNSPECIFIED.,.F.,.F.,(3,3),(0.,1.),.UNSPECIFIED.);
#1326=B_SPLINE_CURVE_WITH_KNOTS('',2,(#74000,#74001,#74002),
 .UNSPECIFIED.,.F.,.F.,(3,3),(0.,1.),.UNSPECIFIED.);
#1327=B_SPLINE_CURVE_WITH_KNOTS('',2,(#74005,#74006,#74007),
 .UNSPECIFIED.,.F.,.F.,(3,3),(0.,1.),.UNSPECIFIED.);
#1328=B_SPLINE_CURVE_WITH_KNOTS('',2,(#74015,#74016,#74017),
 .UNSPECIFIED.,.F.,.F.,(3,3),(0.,1.),.UNSPECIFIED.);
#1329=B_SPLINE_CURVE_WITH_KNOTS('',2,(#74020,#74021,#74022),
 .UNSPECIFIED.,.F.,.F.,(3,3),(0.,1.),.UNSPECIFIED.);
#1330=B_SPLINE_CURVE_WITH_KNOTS('',2,(#74030,#74031,#74032),
 .UNSPECIFIED.,.F.,.F.,(3,3),(0.,1.),.UNSPECIFIED.);
#1331=B_SPLINE_CURVE_WITH_KNOTS('',2,(#74035,#74036,#74037),
 .UNSPECIFIED.,.F.,.F.,(3,3),(0.,1.),.UNSPECIFIED.);
#1332=B_SPLINE_CURVE_WITH_KNOTS('',2,(#74045,#74046,#74047),
 .UNSPECIFIED.,.F.,.F.,(3,3),(0.,1.),.UNSPECIFIED.);
#1333=B_SPLINE_CURVE_WITH_KNOTS('',2,(#74050,#74051,#74052),
 .UNSPECIFIED.,.F.,.F.,(3,3),(0.,1.),.UNSPECIFIED.);
#1334=B_SPLINE_CURVE_WITH_KNOTS('',2,(#74065,#74066,#74067),
 .UNSPECIFIED.,.F.,.F.,(3,3),(0.,1.),.UNSPECIFIED.);
#1335=B_SPLINE_CURVE_WITH_KNOTS('',2,(#74068,#74069,#74070),
 .UNSPECIFIED.,.F.,.F.,(3,3),(0.,1.),.UNSPECIFIED.);
#1336=B_SPLINE_CURVE_WITH_KNOTS('',2,(#74081,#74082,#74083),
 .UNSPECIFIED.,.F.,.F.,(3,3),(0.,1.),.UNSPECIFIED.);
#1337=B_SPLINE_CURVE_WITH_KNOTS('',2,(#74087,#74088,#74089),
 .UNSPECIFIED.,.F.,.F.,(3,3),(0.,1.),.UNSPECIFIED.);
#1338=B_SPLINE_CURVE_WITH_KNOTS('',2,(#74098,#74099,#74100),
 .UNSPECIFIED.,.F.,.F.,(3,3),(0.,1.),.UNSPECIFIED.);
#1339=B_SPLINE_CURVE_WITH_KNOTS('',2,(#74103,#74104,#74105),
 .UNSPECIFIED.,.F.,.F.,(3,3),(0.,1.),.UNSPECIFIED.);
#1340=B_SPLINE_CURVE_WITH_KNOTS('',2,(#74113,#74114,#74115),
 .UNSPECIFIED.,.F.,.F.,(3,3),(0.,1.),.UNSPECIFIED.);
#1341=B_SPLINE_CURVE_WITH_KNOTS('',2,(#74118,#74119,#74120),
 .UNSPECIFIED.,.F.,.F.,(3,3),(0.,1.),.UNSPECIFIED.);
#1342=B_SPLINE_CURVE_WITH_KNOTS('',2,(#74128,#74129,#74130),
 .UNSPECIFIED.,.F.,.F.,(3,3),(0.,1.),.UNSPECIFIED.);
#1343=B_SPLINE_CURVE_WITH_KNOTS('',2,(#74133,#74134,#74135),
 .UNSPECIFIED.,.F.,.F.,(3,3),(0.,1.),.UNSPECIFIED.);
#1344=B_SPLINE_CURVE_WITH_KNOTS('',2,(#74143,#74144,#74145),
 .UNSPECIFIED.,.F.,.F.,(3,3),(0.,1.),.UNSPECIFIED.);
#1345=B_SPLINE_CURVE_WITH_KNOTS('',2,(#74148,#74149,#74150),
 .UNSPECIFIED.,.F.,.F.,(3,3),(0.,1.),.UNSPECIFIED.);
#1346=B_SPLINE_CURVE_WITH_KNOTS('',2,(#74158,#74159,#74160),
 .UNSPECIFIED.,.F.,.F.,(3,3),(0.,1.),.UNSPECIFIED.);
#1347=B_SPLINE_CURVE_WITH_KNOTS('',2,(#74163,#74164,#74165),
 .UNSPECIFIED.,.F.,.F.,(3,3),(0.,1.),.UNSPECIFIED.);
#1348=B_SPLINE_CURVE_WITH_KNOTS('',2,(#74173,#74174,#74175),
 .UNSPECIFIED.,.F.,.F.,(3,3),(0.,1.),.UNSPECIFIED.);
#1349=B_SPLINE_CURVE_WITH_KNOTS('',2,(#74178,#74179,#74180),
 .UNSPECIFIED.,.F.,.F.,(3,3),(0.,1.),.UNSPECIFIED.);
#1350=B_SPLINE_CURVE_WITH_KNOTS('',2,(#74187,#74188,#74189),
 .UNSPECIFIED.,.F.,.F.,(3,3),(0.,1.),.UNSPECIFIED.);
#1351=B_SPLINE_CURVE_WITH_KNOTS('',2,(#74190,#74191,#74192),
 .UNSPECIFIED.,.F.,.F.,(3,3),(0.,1.),.UNSPECIFIED.);
#1352=B_SPLINE_CURVE_WITH_KNOTS('',2,(#74201,#74202,#74203),
 .UNSPECIFIED.,.F.,.F.,(3,3),(0.,1.),.UNSPECIFIED.);
#1353=B_SPLINE_CURVE_WITH_KNOTS('',2,(#74207,#74208,#74209),
 .UNSPECIFIED.,.F.,.F.,(3,3),(0.,1.),.UNSPECIFIED.);
#1354=B_SPLINE_CURVE_WITH_KNOTS('',2,(#74218,#74219,#74220),
 .UNSPECIFIED.,.F.,.F.,(3,3),(0.,1.),.UNSPECIFIED.);
#1355=B_SPLINE_CURVE_WITH_KNOTS('',2,(#74223,#74224,#74225),
 .UNSPECIFIED.,.F.,.F.,(3,3),(0.,1.),.UNSPECIFIED.);
#1356=B_SPLINE_CURVE_WITH_KNOTS('',2,(#74233,#74234,#74235),
 .UNSPECIFIED.,.F.,.F.,(3,3),(0.,1.),.UNSPECIFIED.);
#1357=B_SPLINE_CURVE_WITH_KNOTS('',2,(#74238,#74239,#74240),
 .UNSPECIFIED.,.F.,.F.,(3,3),(0.,1.),.UNSPECIFIED.);
#1358=B_SPLINE_CURVE_WITH_KNOTS('',2,(#74248,#74249,#74250),
 .UNSPECIFIED.,.F.,.F.,(3,3),(0.,1.),.UNSPECIFIED.);
#1359=B_SPLINE_CURVE_WITH_KNOTS('',2,(#74253,#74254,#74255),
 .UNSPECIFIED.,.F.,.F.,(3,3),(0.,1.),.UNSPECIFIED.);
#1360=B_SPLINE_CURVE_WITH_KNOTS('',2,(#74263,#74264,#74265),
 .UNSPECIFIED.,.F.,.F.,(3,3),(0.,1.),.UNSPECIFIED.);
#1361=B_SPLINE_CURVE_WITH_KNOTS('',2,(#74268,#74269,#74270),
 .UNSPECIFIED.,.F.,.F.,(3,3),(0.,1.),.UNSPECIFIED.);
#1362=B_SPLINE_CURVE_WITH_KNOTS('',2,(#74278,#74279,#74280),
 .UNSPECIFIED.,.F.,.F.,(3,3),(0.,1.),.UNSPECIFIED.);
#1363=B_SPLINE_CURVE_WITH_KNOTS('',2,(#74283,#74284,#74285),
 .UNSPECIFIED.,.F.,.F.,(3,3),(0.,1.),.UNSPECIFIED.);
#1364=B_SPLINE_CURVE_WITH_KNOTS('',2,(#74293,#74294,#74295),
 .UNSPECIFIED.,.F.,.F.,(3,3),(0.,1.),.UNSPECIFIED.);
#1365=B_SPLINE_CURVE_WITH_KNOTS('',2,(#74298,#74299,#74300),
 .UNSPECIFIED.,.F.,.F.,(3,3),(0.,1.),.UNSPECIFIED.);
#1366=B_SPLINE_CURVE_WITH_KNOTS('',2,(#74308,#74309,#74310),
 .UNSPECIFIED.,.F.,.F.,(3,3),(0.,1.),.UNSPECIFIED.);
#1367=B_SPLINE_CURVE_WITH_KNOTS('',2,(#74313,#74314,#74315),
 .UNSPECIFIED.,.F.,.F.,(3,3),(0.,1.),.UNSPECIFIED.);
#1368=B_SPLINE_CURVE_WITH_KNOTS('',2,(#74323,#74324,#74325),
 .UNSPECIFIED.,.F.,.F.,(3,3),(0.,1.),.UNSPECIFIED.);
#1369=B_SPLINE_CURVE_WITH_KNOTS('',2,(#74328,#74329,#74330),
 .UNSPECIFIED.,.F.,.F.,(3,3),(0.,1.),.UNSPECIFIED.);
#1370=B_SPLINE_CURVE_WITH_KNOTS('',2,(#74338,#74339,#74340),
 .UNSPECIFIED.,.F.,.F.,(3,3),(0.,1.),.UNSPECIFIED.);
#1371=B_SPLINE_CURVE_WITH_KNOTS('',2,(#74343,#74344,#74345),
 .UNSPECIFIED.,.F.,.F.,(3,3),(0.,1.),.UNSPECIFIED.);
#1372=B_SPLINE_CURVE_WITH_KNOTS('',2,(#74353,#74354,#74355),
 .UNSPECIFIED.,.F.,.F.,(3,3),(0.,1.),.UNSPECIFIED.);
#1373=B_SPLINE_CURVE_WITH_KNOTS('',2,(#74358,#74359,#74360),
 .UNSPECIFIED.,.F.,.F.,(3,3),(0.,1.),.UNSPECIFIED.);
#1374=B_SPLINE_CURVE_WITH_KNOTS('',2,(#74367,#74368,#74369),
 .UNSPECIFIED.,.F.,.F.,(3,3),(0.,1.),.UNSPECIFIED.);
#1375=B_SPLINE_CURVE_WITH_KNOTS('',2,(#74370,#74371,#74372),
 .UNSPECIFIED.,.F.,.F.,(3,3),(0.,1.),.UNSPECIFIED.);
#1376=B_SPLINE_CURVE_WITH_KNOTS('',3,(#77159,#77160,#77161,#77162,#77163,
#77164,#77165,#77166,#77167,#77168,#77169,#77170,#77171,#77172,#77173,#77174,
#77175,#77176,#77177,#77178,#77179,#77180,#77181,#77182,#77183,#77184,#77185,
#77186,#77187,#77188,#77189,#77190,#77191,#77192,#77193,#77194,#77195,#77196,
#77197,#77198,#77199,#77200,#77201,#77202,#77203,#77204,#77205,#77206,#77207,
#77208,#77209,#77210,#77211,#77212,#77213,#77214,#77215,#77216),
 .UNSPECIFIED.,.F.,.F.,(4,2,2,2,2,2,2,2,2,2,2,2,2,2,2,2,2,2,2,2,2,2,2,2,
2,2,2,2,4),(-1.21754206946651,-1.17821980543779,-1.16405746250061,-1.15855947211459,
-1.1545321686619,-1.15022795752816,-1.14324756109432,-1.11173425539269,
-1.09692945396154,-1.08835253727485,-1.08512595789204,-1.08284305354597,
-1.08021521852638,-1.07520106907232,-1.05375326158949,-1.03212994516716,
-1.01905512594296,-1.01371235037151,-1.00971978407183,-1.00537977987688,
-0.998174601131823,-0.963190262851774,-0.950068242946656,-0.942099905926401,
-0.938979922381813,-0.936737330856261,-0.934120072671351,-0.929211478009695,
-0.921419482998929),.UNSPECIFIED.);
#1377=B_SPLINE_CURVE_WITH_KNOTS('',3,(#77219,#77220,#77221,#77222,#77223,
#77224,#77225,#77226,#77227,#77228,#77229,#77230,#77231,#77232,#77233,#77234,
#77235,#77236,#77237,#77238,#77239,#77240,#77241,#77242,#77243,#77244,#77245,
#77246,#77247,#77248,#77249),.UNSPECIFIED.,.F.,.F.,(4,3,3,3,3,3,3,3,3,3,
4),(0.,0.115845454600529,0.231625391685987,0.347372408915667,0.4631235693031,
0.578915929492123,0.69488330926515,0.810943764469935,0.927248476443398,
0.99587989836565,1.12274180646096),.UNSPECIFIED.);
#1378=B_SPLINE_CURVE_WITH_KNOTS('',3,(#77254,#77255,#77256,#77257,#77258,
#77259,#77260,#77261,#77262,#77263,#77264,#77265,#77266,#77267,#77268,#77269,
#77270,#77271,#77272,#77273,#77274,#77275,#77276,#77277,#77278,#77279,#77280,
#77281,#77282,#77283,#77284,#77285,#77286,#77287,#77288,#77289,#77290,#77291,
#77292,#77293,#77294,#77295,#77296,#77297,#77298,#77299,#77300,#77301,#77302,
#77303,#77304,#77305,#77306,#77307,#77308,#77309,#77310,#77311,#77312,#77313,
#77314,#77315,#77316,#77317,#77318,#77319,#77320,#77321,#77322,#77323,#77324,
#77325,#77326,#77327,#77328,#77329,#77330,#77331,#77332,#77333,#77334,#77335,
#77336,#77337,#77338,#77339,#77340,#77341,#77342,#77343,#77344,#77345,#77346,
#77347,#77348,#77349,#77350,#77351,#77352,#77353,#77354,#77355,#77356,#77357,
#77358,#77359,#77360,#77361,#77362,#77363,#77364,#77365,#77366,#77367,#77368,
#77369,#77370,#77371,#77372,#77373,#77374,#77375,#77376,#77377,#77378,#77379,
#77380,#77381,#77382,#77383,#77384,#77385,#77386,#77387,#77388,#77389,#77390,
#77391,#77392,#77393,#77394,#77395,#77396,#77397,#77398,#77399,#77400,#77401,
#77402,#77403,#77404,#77405,#77406,#77407,#77408,#77409,#77410,#77411,#77412,
#77413,#77414,#77415,#77416,#77417,#77418,#77419,#77420,#77421,#77422,#77423,
#77424,#77425),.UNSPECIFIED.,.F.,.F.,(4,2,2,2,2,2,2,2,2,2,2,2,2,2,2,2,2,
2,2,2,2,2,2,2,2,2,2,2,2,2,2,2,2,2,2,2,2,2,2,2,2,2,2,2,2,2,2,2,2,2,2,2,2,
2,2,2,2,2,2,2,2,2,2,2,2,2,2,2,2,2,2,2,2,2,2,2,2,2,2,2,2,2,2,2,2,4),(-0.921419482998929,
-0.907688316791177,-0.885977525693296,-0.872886081562645,-0.867573627709282,
-0.863620021806596,-0.859340338471167,-0.852285820281842,-0.817068960538186,
-0.803848529175472,-0.795853892356727,-0.792748022050185,-0.7905163487824,
-0.787901135493465,-0.783029899170039,-0.763563232406315,-0.745175363618844,
-0.727769961376288,-0.721951181979324,-0.717894343967278,-0.713735439938429,
-0.707376468863512,-0.68265736518924,-0.66121073259976,-0.650652455375354,
-0.647221057566939,-0.644928541426486,-0.642442848946966,-0.638067258217649,
-0.608821864626192,-0.58498089779175,-0.577643940843088,-0.573291994864995,
-0.569330639238763,-0.564094456953282,-0.551677011438918,-0.53193566151644,
-0.507251176775778,-0.502465995418774,-0.499868632875132,-0.497623283392536,
-0.494462217094089,-0.486137962898804,-0.472047790880579,-0.43783436812367,
-0.431066025429978,-0.426831354822855,-0.422832748507351,-0.41731951470546,
-0.40276097029277,-0.376056281360347,-0.359534421781043,-0.355618511890536,
-0.353232508861721,-0.350881150748675,-0.347133669219491,-0.332694769079542,
-0.314588300276116,-0.290783010636688,-0.284507014961167,-0.280367699863515,
-0.276304767597177,-0.270432530198454,-0.252375906212504,-0.234530960463338,
-0.2153034103759,-0.210445276682928,-0.207832350266125,-0.205589527875254,
-0.202453875215916,-0.194323277172034,-0.180756703969854,-0.145451744314263,
-0.138838184308752,-0.134632742059005,-0.130615121903102,-0.124997860543144,
-0.109547987206611,-0.0788702916803572,-0.0669285629089969,-0.063284529861049,
-0.0611845516338545,-0.0588379538520908,-0.0551131392442454,-0.0410185576883546,
-6.1401681533555E-5),.UNSPECIFIED.);
#1379=B_SPLINE_CURVE_WITH_KNOTS('',3,(#77426,#77427,#77428,#77429,#77430,
#77431,#77432,#77433,#77434,#77435,#77436,#77437,#77438,#77439,#77440,#77441,
#77442,#77443,#77444,#77445,#77446,#77447,#77448,#77449,#77450,#77451,#77452,
#77453,#77454,#77455,#77456,#77457,#77458,#77459,#77460,#77461,#77462,#77463,
#77464,#77465,#77466,#77467,#77468,#77469,#77470,#77471,#77472,#77473,#77474,
#77475,#77476,#77477,#77478,#77479,#77480,#77481,#77482,#77483,#77484,#77485,
#77486,#77487,#77488,#77489,#77490,#77491,#77492,#77493,#77494,#77495,#77496,
#77497,#77498,#77499,#77500,#77501,#77502,#77503,#77504,#77505,#77506,#77507,
#77508,#77509,#77510,#77511,#77512,#77513,#77514,#77515,#77516,#77517,#77518,
#77519,#77520,#77521,#77522,#77523,#77524,#77525,#77526,#77527,#77528,#77529,
#77530,#77531,#77532,#77533,#77534,#77535,#77536,#77537,#77538,#77539,#77540,
#77541,#77542,#77543,#77544,#77545,#77546,#77547,#77548,#77549,#77550,#77551,
#77552,#77553,#77554,#77555,#77556,#77557,#77558,#77559,#77560,#77561,#77562,
#77563,#77564,#77565,#77566,#77567,#77568,#77569,#77570,#77571,#77572,#77573,
#77574,#77575,#77576,#77577,#77578,#77579,#77580,#77581,#77582,#77583,#77584,
#77585,#77586,#77587,#77588,#77589,#77590,#77591,#77592,#77593,#77594,#77595,
#77596,#77597,#77598,#77599,#77600,#77601,#77602,#77603,#77604,#77605,#77606,
#77607,#77608,#77609,#77610,#77611,#77612,#77613,#77614,#77615,#77616,#77617,
#77618,#77619,#77620,#77621,#77622,#77623,#77624,#77625,#77626,#77627,#77628,
#77629,#77630,#77631,#77632,#77633,#77634,#77635,#77636,#77637,#77638,#77639),
 .UNSPECIFIED.,.F.,.F.,(4,3,3,3,3,3,3,3,3,3,3,3,3,3,3,3,3,3,3,3,3,3,3,3,
3,3,3,3,3,3,3,3,3,3,3,3,3,3,3,3,3,3,3,3,3,3,3,3,3,3,3,3,3,3,3,3,3,3,3,3,
3,3,3,3,3,3,3,3,3,3,3,4),(1.12274180646096,1.23373504789904,1.34459002212884,
1.45535479623447,1.55989672892336,1.56607726185873,1.67688568467484,1.78773354109534,
1.89879266001346,1.99171671473048,1.9917597967313,2.09518566569704,2.10522016410668,
2.21847423059868,2.33161337714145,2.4446824646528,2.55772625044323,2.67087099529545,
2.78406492035342,2.89747197121009,2.9876011371121,2.98763969509696,3.09165900030874,
3.10124740420088,3.21465736692644,3.32795751893579,3.44119241833077,3.55440652592882,
3.6677272400545,3.7811005346835,3.89469031251206,3.9834802329205,3.98351959346261,
4.08724850520171,4.09685637681465,4.20998806900548,4.32300567198192,4.43595426307203,
4.54887881688974,4.66190726618895,4.77498633572913,4.88828238191216,4.97935950968077,
4.97939949182826,5.08314209235908,5.09284419837543,5.20608568010895,5.31921413328377,
5.43227443626529,5.54531136614965,5.65845232226374,5.77164415146343,5.88505194316747,
5.97523993044046,5.97527939019391,6.07908252879731,6.08873073478065,6.20197956676853,
6.3151158004847,6.42818430022515,6.54122982955544,6.65437994550042,6.76758125938584,
6.88099895560384,6.97111969950722,6.97115928855956,7.07900809076849,7.09416685512428,
7.21066939468956,7.21683096983575,7.33897298823794,7.40592711304532),
 .UNSPECIFIED.);
#1380=B_SPLINE_CURVE_WITH_KNOTS('',3,(#77644,#77645,#77646,#77647,#77648,
#77649,#77650,#77651,#77652,#77653,#77654,#77655,#77656,#77657,#77658,#77659,
#77660,#77661,#77662,#77663,#77664,#77665,#77666,#77667,#77668,#77669,#77670,
#77671,#77672,#77673,#77674,#77675,#77676,#77677,#77678,#77679,#77680,#77681,
#77682,#77683,#77684,#77685,#77686,#77687,#77688,#77689,#77690,#77691,#77692,
#77693,#77694,#77695,#77696,#77697,#77698,#77699,#77700,#77701,#77702,#77703,
#77704,#77705,#77706,#77707,#77708,#77709,#77710,#77711,#77712,#77713,#77714,
#77715,#77716,#77717,#77718,#77719,#77720,#77721,#77722,#77723,#77724,#77725,
#77726,#77727,#77728,#77729,#77730,#77731,#77732,#77733,#77734,#77735,#77736,
#77737,#77738,#77739,#77740,#77741,#77742,#77743,#77744,#77745,#77746,#77747,
#77748,#77749,#77750,#77751,#77752,#77753,#77754,#77755,#77756,#77757,#77758,
#77759,#77760,#77761,#77762,#77763,#77764,#77765,#77766,#77767,#77768,#77769,
#77770,#77771,#77772,#77773,#77774,#77775,#77776,#77777,#77778,#77779,#77780,
#77781,#77782,#77783,#77784,#77785,#77786,#77787,#77788,#77789,#77790,#77791,
#77792,#77793,#77794,#77795,#77796,#77797,#77798,#77799,#77800,#77801,#77802,
#77803,#77804,#77805,#77806,#77807,#77808,#77809,#77810,#77811,#77812,#77813,
#77814,#77815,#77816,#77817,#77818,#77819,#77820,#77821,#77822,#77823,#77824,
#77825,#77826,#77827,#77828,#77829,#77830,#77831,#77832,#77833,#77834,#77835,
#77836,#77837,#77838,#77839,#77840,#77841,#77842,#77843,#77844,#77845,#77846,
#77847,#77848,#77849,#77850,#77851,#77852,#77853,#77854),.UNSPECIFIED.,
 .F.,.F.,(4,3,3,3,3,3,3,3,3,3,3,3,3,3,3,3,3,3,3,3,3,3,3,3,3,3,3,3,3,3,3,
3,3,3,3,3,3,3,3,3,3,3,3,3,3,3,3,3,3,3,3,3,3,3,3,3,3,3,3,3,3,3,3,3,3,3,3,
3,3,3,4),(-16.6574965103488,-16.5463313103564,-16.4343301060372,-16.322344109605,
-16.2102494790042,-16.0980936348029,-15.9924244225728,-15.9857348554638,
-15.934117974039,-15.9340783738505,-15.8303032419388,-15.8206442770722,
-15.7074132532074,-15.5942951569007,-15.4812450908478,-15.3682182588957,
-15.2550871008504,-15.1419049191215,-15.0285064012669,-14.938238075336,
-14.9381984754848,-14.8344232571971,-14.8247643455127,-14.7115332877515,
-14.5984151571454,-14.4853650564546,-14.3723381895906,-14.2592069964952,
-14.1460247795845,-14.0326262267835,-13.942358177767,-13.9423185771191,
-13.8385435760761,-13.8288846569355,-13.7156538090858,-13.6025358883135,
-13.4894859970134,-13.3764593387315,-13.2633283513034,-13.1501463387721,
-13.0367479856472,-12.9464782790693,-12.9464386787535,-12.8426635582421,
-12.8330044289798,-12.7197732542598,-12.6066550085104,-12.4936047946711,
-12.380577816835,-12.2674465169873,-12.1542641954907,-12.0408655429596,
-11.9505983780519,-11.9505587803878,-11.8467830017773,-11.8371243762114,
-11.7238930404563,-11.6107746297512,-11.4977242473709,-11.384697097739,
-11.2715656225024,-11.1583831233508,-11.0449842917532,-10.9547184870581,
-10.9546788820222,-10.8497976193126,-10.8389884949821,-10.7230435781436,
-10.6077612699342,-10.4914850487812,-10.3752088276281),.UNSPECIFIED.);
#1381=B_SPLINE_CURVE_WITH_KNOTS('',3,(#77855,#77856,#77857,#77858,#77859,
#77860,#77861,#77862,#77863,#77864,#77865,#77866,#77867,#77868,#77869,#77870,
#77871,#77872,#77873,#77874,#77875,#77876,#77877,#77878,#77879,#77880,#77881,
#77882,#77883,#77884,#77885,#77886,#77887,#77888,#77889,#77890,#77891,#77892,
#77893,#77894,#77895,#77896,#77897,#77898,#77899,#77900,#77901,#77902,#77903,
#77904,#77905,#77906,#77907,#77908,#77909,#77910,#77911,#77912,#77913,#77914,
#77915,#77916,#77917,#77918,#77919,#77920,#77921,#77922,#77923,#77924,#77925,
#77926,#77927,#77928,#77929,#77930,#77931,#77932,#77933,#77934,#77935,#77936,
#77937,#77938,#77939,#77940,#77941,#77942,#77943,#77944,#77945,#77946,#77947,
#77948,#77949,#77950,#77951,#77952,#77953,#77954,#77955,#77956,#77957,#77958,
#77959,#77960,#77961,#77962,#77963,#77964,#77965,#77966,#77967,#77968,#77969,
#77970,#77971,#77972,#77973,#77974,#77975,#77976,#77977,#77978,#77979,#77980,
#77981,#77982,#77983,#77984,#77985,#77986,#77987,#77988,#77989,#77990,#77991,
#77992,#77993,#77994,#77995,#77996,#77997,#77998,#77999,#78000,#78001,#78002,
#78003,#78004,#78005,#78006,#78007,#78008,#78009,#78010,#78011,#78012,#78013,
#78014,#78015,#78016,#78017,#78018,#78019,#78020,#78021,#78022,#78023,#78024,
#78025,#78026,#78027,#78028,#78029,#78030,#78031,#78032,#78033,#78034,#78035,
#78036,#78037,#78038),.UNSPECIFIED.,.F.,.F.,(4,2,2,2,2,2,2,2,2,2,2,2,2,
2,2,2,2,2,2,2,2,2,2,2,2,2,2,2,2,2,2,2,2,2,2,2,2,2,2,2,2,2,2,2,2,2,2,2,2,
2,2,2,2,2,2,2,2,2,2,2,2,2,2,2,2,2,2,2,2,2,2,2,2,2,2,2,2,2,2,2,2,2,2,2,2,
2,2,2,2,2,2,4),(7.55331046094257E-5,0.00311488062742005,0.00589275104345637,
0.00957822560877077,0.0136874178462499,0.0196924847782724,0.0409279650768497,
0.0549894800395652,0.0692347333575978,0.0750056140336835,0.0794705133763708,
0.0819628446481993,0.0841961839693353,0.0869680298364656,0.0940489209653037,
0.129814111425115,0.146099950504705,0.151785217588427,0.155795564055968,
0.159453751928995,0.165433805290373,0.182940478931749,0.207240700533897,
0.222307455662279,0.226079429552293,0.228426586761477,0.23078666401458,
0.234620974103604,0.249432251355507,0.277557223302338,0.292445953223121,
0.297979106518716,0.301963020846168,0.306155184921126,0.312793013872007,
0.347827135873415,0.361540513352248,0.369716897813443,0.372846972694969,
0.375076835859076,0.377660756070977,0.382430268818484,0.405438098633203,
0.426320205326456,0.439129906572397,0.44439978553307,0.448343075832583,
0.452631913781975,0.459751362689939,0.494720362864264,0.507857683034686,
0.51581555707109,0.518915196993098,0.521141161944093,0.523742195593142,
0.528592249214605,0.547902250767208,0.565126197412152,0.583669666253345,
0.589560417299322,0.593607282150156,0.597705592918242,0.603867947078983,
0.624922258499583,0.655514298780022,0.662278005328982,0.665197397890851,
0.667196094429105,0.669816617220415,0.67475964111456,0.696085820423846,
0.717922799335886,0.731055622848822,0.736369783015217,0.740319640023491,
0.744590515419098,0.751619654650834,0.783667918036271,0.798887961548889,
0.80760501751015,0.810806816097925,0.813046735586465,0.815593959750254,
0.820191227049956,0.846466054625532,0.865368695833238,0.877457066491806,
0.882624456523596,0.886554289123994,0.890890438772885,0.898244410878047,
0.921379800955709),.UNSPECIFIED.);
#1382=B_SPLINE_CURVE_WITH_KNOTS('',3,(#78044,#78045,#78046,#78047,#78048,
#78049,#78050,#78051,#78052,#78053,#78054,#78055,#78056,#78057,#78058,#78059,
#78060,#78061,#78062,#78063,#78064,#78065,#78066,#78067,#78068,#78069,#78070,
#78071,#78072,#78073,#78074,#78075,#78076,#78077,#78078,#78079,#78080,#78081,
#78082,#78083,#78084,#78085,#78086,#78087,#78088,#78089,#78090,#78091,#78092,
#78093,#78094,#78095,#78096,#78097,#78098,#78099,#78100,#78101,#78102,#78103,
#78104,#78105,#78106,#78107,#78108,#78109,#78110,#78111,#78112,#78113,#78114,
#78115,#78116,#78117,#78118,#78119,#78120,#78121,#78122,#78123,#78124,#78125,
#78126,#78127,#78128,#78129,#78130,#78131,#78132,#78133,#78134,#78135,#78136,
#78137,#78138,#78139,#78140,#78141,#78142,#78143,#78144,#78145,#78146,#78147,
#78148,#78149,#78150,#78151,#78152,#78153,#78154,#78155,#78156,#78157,#78158,
#78159,#78160,#78161,#78162,#78163,#78164,#78165,#78166,#78167,#78168,#78169,
#78170,#78171,#78172,#78173,#78174,#78175,#78176,#78177,#78178,#78179,#78180,
#78181,#78182,#78183,#78184,#78185,#78186,#78187,#78188,#78189,#78190,#78191,
#78192,#78193,#78194,#78195,#78196,#78197,#78198,#78199,#78200,#78201,#78202,
#78203,#78204,#78205,#78206,#78207,#78208,#78209,#78210,#78211,#78212,#78213,
#78214,#78215,#78216,#78217,#78218,#78219,#78220,#78221,#78222,#78223),
 .UNSPECIFIED.,.F.,.F.,(4,2,2,2,2,2,2,2,2,2,2,2,2,2,2,2,2,2,2,2,2,2,2,2,
2,2,2,2,2,2,2,2,2,2,2,2,2,2,2,2,2,2,2,2,2,2,2,2,2,2,2,2,2,2,2,2,2,2,2,2,
2,2,2,2,2,2,2,2,2,2,2,2,2,2,2,2,2,2,2,2,2,2,2,2,2,2,2,2,2,4),(0.921350305018577,
0.921389876624562,0.924778351317925,0.927037052310556,0.929523336688975,
0.933909319231592,0.956539494608926,0.987309347251915,0.994485423914873,
0.998803284581335,1.00277147317402,1.00807376621736,1.02097866000226,1.04210375396098,
1.0645803887481,1.06942020706886,1.07202853433207,1.0742712679726,1.07741171247261,
1.08558062454395,1.09925152423885,1.13435370175234,1.14099825146805,1.14520924348174,
1.14922237985182,1.15481702416113,1.17007308473251,1.19982027276487,1.21271906572539,
1.21644741108376,1.21856275817168,1.22089123008652,1.22452877455692,1.23742122425125,
1.27188899511206,1.28349027612361,1.28869318828847,1.29266019279346,1.29698089226977,
1.30417190236956,1.32646153627304,1.35215637825488,1.35995878365049,1.36312058726059,
1.36536602189029,1.36796236389115,1.37288653830946,1.39177683800695,1.42619710890516,
1.43293802757295,1.43716799625277,1.44117067547864,1.44670370535482,1.46142612404115,
1.48881206170003,1.50445213009386,1.50832697709802,1.51070479095477,1.51306379954949,
1.51685016199031,1.53193445644289,1.55624909699754,1.57386860269962,1.57980106586157,
1.58346687670161,1.58751537895101,1.59331612571466,1.61059459442548,1.62861744095523,
1.64849768185189,1.65339889357475,1.65601991617009,1.6582594648806,1.66137646992562,
1.66937874648447,1.68261100872528,1.71804363796523,1.72485063701832,1.72909376915813,
1.73308998369107,1.73858333515089,1.75297381136775,1.7790423411234,1.79629129359712,
1.80023499046673,1.80262740654097,1.80497314347554,1.8086963080364,1.82277639645548,
1.84239058989693),.UNSPECIFIED.);
#1383=B_SPLINE_CURVE_WITH_KNOTS('',3,(#78224,#78225,#78226,#78227),
 .UNSPECIFIED.,.F.,.F.,(4,4),(-16.6583941348077,-16.6574965103488),
 .UNSPECIFIED.);
#1384=B_SPLINE_CURVE_WITH_KNOTS('',3,(#78229,#78230,#78231,#78232,#78233,
#78234,#78235,#78236,#78237,#78238,#78239,#78240,#78241,#78242,#78243,#78244,
#78245,#78246,#78247,#78248,#78249,#78250,#78251,#78252,#78253,#78254,#78255,
#78256,#78257,#78258,#78259,#78260,#78261,#78262,#78263,#78264,#78265,#78266,
#78267,#78268,#78269,#78270,#78271,#78272,#78273,#78274,#78275,#78276,#78277,
#78278,#78279,#78280,#78281,#78282,#78283,#78284,#78285,#78286,#78287,#78288,
#78289,#78290,#78291,#78292,#78293,#78294,#78295,#78296,#78297,#78298,#78299,
#78300,#78301,#78302,#78303,#78304,#78305,#78306,#78307,#78308,#78309,#78310,
#78311,#78312,#78313,#78314,#78315,#78316,#78317,#78318,#78319,#78320,#78321,
#78322,#78323,#78324,#78325,#78326,#78327,#78328,#78329,#78330,#78331,#78332,
#78333,#78334,#78335,#78336,#78337,#78338,#78339,#78340,#78341,#78342,#78343,
#78344,#78345,#78346,#78347,#78348,#78349,#78350,#78351,#78352,#78353,#78354,
#78355,#78356,#78357,#78358,#78359,#78360,#78361,#78362,#78363,#78364,#78365,
#78366,#78367,#78368,#78369,#78370,#78371,#78372,#78373,#78374,#78375,#78376,
#78377,#78378,#78379,#78380,#78381,#78382,#78383,#78384,#78385,#78386,#78387,
#78388,#78389,#78390,#78391,#78392,#78393,#78394,#78395,#78396,#78397,#78398,
#78399,#78400,#78401,#78402,#78403,#78404,#78405,#78406,#78407,#78408,#78409,
#78410,#78411,#78412,#78413,#78414),.UNSPECIFIED.,.F.,.F.,(4,2,2,2,2,2,
2,2,2,2,2,2,2,2,2,2,2,2,2,2,2,2,2,2,2,2,2,2,2,2,2,2,2,2,2,2,2,2,2,2,2,2,
2,2,2,2,2,2,2,2,2,2,2,2,2,2,2,2,2,2,2,2,2,2,2,2,2,2,2,2,2,2,2,2,2,2,2,2,
2,2,2,2,2,2,2,2,2,2,2,2,2,2,4),(0.921379800955709,0.921511462072376,0.949406248900438,
0.954915878085833,0.957616084348176,0.959806098671794,0.962742035540181,
0.96960888206462,0.980108126735474,1.00265005569605,1.02138548779191,1.02742513364255,
1.03109303754262,1.03509348211883,1.04072477727184,1.05649993293572,1.08901049958424,
1.09907574790631,1.10253013184978,1.10479041416925,1.10722834732382,1.11142941842079,
1.13312603579934,1.16548672629248,1.17248247257583,1.17674652018402,1.1806986241325,
1.1860290933367,1.19928598585736,1.22150457988203,1.24240677180674,1.24725670356296,
1.24985764546148,1.25208359260461,1.25518332106303,1.26314120661243,1.27627928776522,
1.3112403102158,1.31837539785881,1.32266744792816,1.32660980377609,1.33187256392618,
1.34463145702576,1.36536819263287,1.38857317872476,1.39333372078013,1.39591574062321,
1.39814594896,1.40127939764684,1.40948097186301,1.42326311865662,1.45817393361484,
1.46483153706146,1.46902739883502,1.47300880978117,1.4785285638421,1.49330621716269,
1.52096743689291,1.53631940261687,1.5401709433473,1.54253445619872,1.54487702556269,
1.54863004027595,1.56338839100655,1.58122608546742,1.6050017060548,1.61125098564634,
1.61536591180166,1.61939852067159,1.6252131035489,1.64287033869637,1.6606426259535,
1.68037916149352,1.68525719244088,1.68786396930375,1.69008857146817,1.69317790260395,
1.70106276347702,1.71401242767589,1.74818141044997,1.75581602328968,1.76024956431239,
1.7641593971117,1.76914879252055,1.78008055903901,1.79616279955146,1.81413094267229,
1.82842328418419,1.8322129424923,1.83456320436152,1.83660820322032,1.8392493161768,
1.84253082468574),.UNSPECIFIED.);
#1385=B_SPLINE_CURVE_WITH_KNOTS('',3,(#78415,#78416,#78417,#78418),
 .UNSPECIFIED.,.F.,.F.,(4,4),(0.000123955660990716,0.0001645492752207),
 .UNSPECIFIED.);
#1386=B_SPLINE_CURVE_WITH_KNOTS('',3,(#78424,#78425,#78426,#78427),
 .UNSPECIFIED.,.F.,.F.,(4,4),(1.84262518595721,1.84272753034819),
 .UNSPECIFIED.);
#1387=B_SPLINE_CURVE_WITH_KNOTS('',3,(#78428,#78429,#78430,#78431,#78432,
#78433,#78434,#78435,#78436,#78437,#78438,#78439,#78440,#78441,#78442,#78443,
#78444,#78445,#78446,#78447,#78448,#78449,#78450,#78451,#78452,#78453,#78454,
#78455,#78456,#78457,#78458,#78459,#78460,#78461,#78462,#78463,#78464,#78465,
#78466,#78467,#78468,#78469,#78470,#78471,#78472,#78473,#78474,#78475,#78476,
#78477,#78478,#78479,#78480,#78481,#78482,#78483,#78484,#78485,#78486,#78487,
#78488,#78489,#78490,#78491,#78492,#78493,#78494,#78495,#78496,#78497,#78498,
#78499,#78500,#78501,#78502,#78503,#78504,#78505,#78506,#78507,#78508,#78509,
#78510,#78511,#78512,#78513,#78514,#78515,#78516,#78517,#78518,#78519,#78520,
#78521,#78522,#78523,#78524,#78525,#78526,#78527,#78528,#78529,#78530,#78531,
#78532,#78533,#78534,#78535,#78536,#78537,#78538,#78539,#78540,#78541,#78542,
#78543,#78544,#78545,#78546,#78547,#78548,#78549,#78550,#78551,#78552,#78553,
#78554,#78555,#78556,#78557,#78558,#78559,#78560,#78561,#78562,#78563,#78564,
#78565,#78566,#78567,#78568,#78569,#78570,#78571,#78572,#78573,#78574,#78575,
#78576,#78577,#78578,#78579,#78580,#78581,#78582,#78583,#78584,#78585,#78586,
#78587,#78588,#78589,#78590,#78591,#78592,#78593,#78594,#78595,#78596,#78597,
#78598,#78599),.UNSPECIFIED.,.F.,.F.,(4,2,2,2,2,2,2,2,2,2,2,2,2,2,2,2,2,
2,2,2,2,2,2,2,2,2,2,2,2,2,2,2,2,2,2,2,2,2,2,2,2,2,2,2,2,2,2,2,2,2,2,2,2,
2,2,2,2,2,2,2,2,2,2,2,2,2,2,2,2,2,2,2,2,2,2,2,2,2,2,2,2,2,2,2,2,4),(0.000101250613919574,
0.0302450781019042,0.0444693089741603,0.048202616836321,0.0505509261682221,
0.0529418146572406,0.0568763595433419,0.0738308452279146,0.100165398608602,
0.114628320004093,0.120131598164091,0.124130240185373,0.128371621848128,
0.135166089952892,0.169197205263441,0.183373526745438,0.191729771658096,
0.194895901941542,0.197142258991893,0.199737091617328,0.204512301270677,
0.227753295369034,0.248457049667915,0.26121689088981,0.266499614624906,
0.270465432826506,0.27479249297983,0.282012960789868,0.318171579784247,
0.334826615024971,0.339497205227342,0.342042612703549,0.344303756540027,
0.347570816901137,0.356059279481411,0.390234599894148,0.406298758104433,
0.411981482289126,0.416010022219744,0.419698990950769,0.425764705896488,
0.444622609706147,0.467061494019179,0.482443352428587,0.4862472681405,0.488610382004106,
0.490697520615568,0.494271250091231,0.505416415789197,0.536846216390167,
0.552439637728479,0.558072084942697,0.562091870391891,0.56629202441881,
0.57288091121604,0.608347517683316,0.621836962244223,0.629938062082391,
0.633069279511645,0.635311051863348,0.637924964797009,0.642790613214213,
0.663545652246991,0.684417200905839,0.698805868700279,0.704300132714303,
0.708297292275137,0.712541668231052,0.719351275541517,0.753270451451571,
0.767501439975446,0.775877538070527,0.779046303895663,0.781292986687984,
0.78388634654955,0.788654740534721,0.813455991135851,0.833121567861134,
0.845508422174809,0.850738386794919,0.854697108755072,0.859048102965697,
0.86638800917551,0.891151523568089,0.911193271661736,0.921350305018577),
 .UNSPECIFIED.);
#1388=B_SPLINE_CURVE_WITH_KNOTS('',3,(#78600,#78601,#78602,#78603,#78604,
#78605,#78606,#78607,#78608,#78609,#78610,#78611,#78612,#78613,#78614,#78615,
#78616,#78617,#78618,#78619,#78620,#78621,#78622,#78623,#78624,#78625,#78626,
#78627,#78628,#78629,#78630,#78631,#78632,#78633,#78634,#78635,#78636,#78637,
#78638,#78639,#78640,#78641,#78642,#78643,#78644,#78645,#78646,#78647,#78648,
#78649,#78650,#78651,#78652,#78653,#78654,#78655,#78656,#78657,#78658,#78659,
#78660,#78661,#78662,#78663,#78664,#78665,#78666,#78667,#78668,#78669,#78670,
#78671,#78672,#78673,#78674,#78675,#78676,#78677,#78678,#78679,#78680,#78681,
#78682,#78683,#78684,#78685,#78686,#78687,#78688,#78689,#78690,#78691,#78692,
#78693,#78694,#78695,#78696,#78697,#78698,#78699,#78700,#78701,#78702,#78703,
#78704,#78705,#78706,#78707,#78708,#78709,#78710,#78711,#78712,#78713,#78714,
#78715,#78716,#78717,#78718,#78719,#78720,#78721,#78722,#78723,#78724,#78725,
#78726,#78727,#78728,#78729,#78730,#78731,#78732,#78733,#78734,#78735,#78736,
#78737,#78738,#78739,#78740,#78741,#78742,#78743,#78744,#78745,#78746,#78747,
#78748,#78749,#78750,#78751,#78752,#78753,#78754,#78755,#78756,#78757,#78758,
#78759,#78760,#78761,#78762,#78763,#78764,#78765,#78766,#78767,#78768,#78769,
#78770,#78771,#78772,#78773),.UNSPECIFIED.,.F.,.F.,(4,2,2,2,2,2,2,2,2,2,
2,2,2,2,2,2,2,2,2,2,2,2,2,2,2,2,2,2,2,2,2,2,2,2,2,2,2,2,2,2,2,2,2,2,2,2,
2,2,2,2,2,2,2,2,2,2,2,2,2,2,2,2,2,2,2,2,2,2,2,2,2,2,2,2,2,2,2,2,2,2,2,2,
2,2,2,2,4),(0.0001645492752207,0.0231231113283336,0.0440247145262724,0.0568414829277775,
0.0621126527407258,0.0660564396362311,0.0703453847668487,0.0774640022785633,
0.108660747718192,0.131319845940176,0.135489869597789,0.137921304680615,
0.140185427288329,0.14366028213544,0.153913582838174,0.182803578276252,
0.201388672488877,0.207282905464499,0.211330470171896,0.215428123865974,
0.221586788162412,0.24252798283675,0.273214312903204,0.280000499247005,
0.28292355142068,0.285112828225382,0.287823363414176,0.293387548960966,
0.324723500013775,0.339563594116051,0.349934723300853,0.354832419533883,
0.358734943685334,0.363229968466276,0.371159132904426,0.407708492072248,
0.42402670893179,0.427865641516943,0.430226702815742,0.432291046781632,
0.435786717467062,0.446240905938236,0.478381687212749,0.494094307894705,
0.499719202510841,0.503718595034805,0.507883224011601,0.514382956291043,
0.550350705476149,0.563629030650189,0.571641195575328,0.574748671206292,
0.576975784506754,0.579572707208546,0.584402893756101,0.603309224116719,
0.619578186751874,0.632818447115015,0.642418762535818,0.647183402032388,
0.650700407219525,0.65515200889598,0.662871020297927,0.696919740217704,
0.709838242108691,0.71771166935532,0.720799650228814,0.72302441774324,0.725632684635717,
0.730516651035866,0.753022988740741,0.774118812094353,0.78700277371131,
0.792283367704293,0.796228638313861,0.800513891447624,0.807613466615827,
0.839008140632725,0.85459062049883,0.863431683566498,0.866649425094912,
0.868891847886336,0.871431721516379,0.875994372056908,0.902899908240868,
0.921434484064485,0.921536811180233),.UNSPECIFIED.);
#1389=B_SPLINE_CURVE_WITH_KNOTS('',3,(#78778,#78779,#78780,#78781,#78782,
#78783,#78784,#78785,#78786,#78787,#78788,#78789,#78790,#78791,#78792,#78793,
#78794,#78795,#78796,#78797,#78798,#78799,#78800,#78801,#78802,#78803,#78804,
#78805,#78806,#78807,#78808,#78809,#78810,#78811,#78812,#78813,#78814,#78815,
#78816,#78817,#78818,#78819,#78820,#78821,#78822,#78823,#78824,#78825,#78826,
#78827,#78828,#78829,#78830,#78831,#78832,#78833,#78834,#78835,#78836,#78837,
#78838,#78839,#78840,#78841,#78842,#78843,#78844,#78845,#78846,#78847,#78848,
#78849,#78850,#78851,#78852,#78853,#78854,#78855,#78856,#78857,#78858,#78859,
#78860,#78861,#78862,#78863,#78864,#78865,#78866,#78867,#78868,#78869,#78870,
#78871,#78872,#78873,#78874,#78875,#78876,#78877,#78878,#78879,#78880,#78881,
#78882,#78883,#78884,#78885,#78886,#78887,#78888,#78889,#78890,#78891,#78892,
#78893,#78894,#78895,#78896,#78897,#78898,#78899,#78900,#78901,#78902,#78903,
#78904,#78905,#78906,#78907,#78908,#78909,#78910,#78911,#78912,#78913,#78914,
#78915,#78916,#78917,#78918,#78919,#78920,#78921,#78922,#78923,#78924,#78925,
#78926,#78927,#78928,#78929,#78930,#78931,#78932,#78933,#78934,#78935,#78936,
#78937,#78938,#78939,#78940,#78941,#78942,#78943,#78944,#78945,#78946,#78947,
#78948,#78949,#78950,#78951,#78952,#78953,#78954,#78955,#78956,#78957,#78958,
#78959),.UNSPECIFIED.,.F.,.F.,(4,2,2,2,2,2,2,2,2,2,2,2,2,2,2,2,2,2,2,2,
2,2,2,2,2,2,2,2,2,2,2,2,2,2,2,2,2,2,2,2,2,2,2,2,2,2,2,2,2,2,2,2,2,2,2,2,
2,2,2,2,2,2,2,2,2,2,2,2,2,2,2,2,2,2,2,2,2,2,2,2,2,2,2,2,2,2,2,2,2,2,4),
(0.921425937241738,0.935047588256698,0.940596973306458,0.944602639488585,
0.948827892202315,0.955543837834373,0.963625969364764,0.981492657083748,
1.00956823508816,1.01407697961797,1.01658874030863,1.01886211690919,1.02220611035665,
1.03200166121431,1.0506028430488,1.07733983428292,1.0846753778969,1.08902528628111,
1.09298389631013,1.09821502602709,1.11061271826728,1.13030873267281,1.15501536779979,
1.15979223001154,1.16238724385352,1.16463319329929,1.1677980888709,1.17614649239289,
1.19030271680065,1.22439648347554,1.2311842498732,1.23542395882675,1.23942267523241,
1.24492875803767,1.25942023585298,1.2858747359802,1.30265034347765,1.30657720259476,
1.30896627169807,1.31131558884073,1.31505481806986,1.32937156117902,1.34754896807697,
1.37142222633636,1.37770318371716,1.38184237853992,1.38590260595661,1.39176618685812,
1.40974047130409,1.42744414604826,1.44686941447829,1.45173788682739,1.45435223758731,
1.45659358839019,1.45972323955726,1.4678142219022,1.48127828301263,1.51682186482659,
1.52340141545502,1.52759940482106,1.53161972987439,1.53725736973447,1.55290470618805,
1.58464369795291,1.59544347409396,1.5989852568477,1.60106655126147,1.60343745002039,
1.60727905533835,1.62336514281784,1.65875083645647,1.6667510328446,1.67167856689287,
1.67560529463892,1.68013003452993,1.68835039969846,1.71359658097977,1.73932021414089,
1.7439548620375,1.7465194259263,1.74877365808267,1.75199791340774,1.7607997997127,
1.77624126834546,1.80922584955855,1.81562822009077,1.81979101679094,1.82351117961273,
1.82747030048524,1.83372067269811,1.84262518595721),.UNSPECIFIED.);
#1390=B_SPLINE_CURVE_WITH_KNOTS('',3,(#78960,#78961,#78962,#78963,#78964,
#78965,#78966,#78967,#78968,#78969,#78970,#78971,#78972,#78973,#78974,#78975,
#78976,#78977,#78978,#78979,#78980,#78981,#78982,#78983,#78984,#78985,#78986,
#78987,#78988,#78989,#78990,#78991,#78992,#78993,#78994,#78995,#78996,#78997,
#78998,#78999,#79000,#79001,#79002,#79003,#79004,#79005,#79006,#79007,#79008,
#79009,#79010,#79011,#79012,#79013,#79014,#79015,#79016,#79017,#79018,#79019,
#79020,#79021,#79022,#79023,#79024,#79025,#79026,#79027,#79028,#79029,#79030,
#79031,#79032,#79033,#79034,#79035,#79036,#79037,#79038,#79039,#79040,#79041,
#79042,#79043,#79044,#79045,#79046,#79047,#79048,#79049,#79050,#79051,#79052,
#79053,#79054,#79055,#79056,#79057,#79058,#79059,#79060,#79061,#79062,#79063,
#79064,#79065,#79066,#79067,#79068,#79069,#79070,#79071,#79072,#79073,#79074,
#79075,#79076,#79077,#79078,#79079,#79080,#79081,#79082,#79083,#79084,#79085,
#79086,#79087,#79088,#79089,#79090,#79091,#79092,#79093,#79094,#79095,#79096,
#79097,#79098,#79099,#79100,#79101,#79102,#79103,#79104,#79105,#79106,#79107,
#79108,#79109,#79110,#79111,#79112,#79113,#79114,#79115,#79116,#79117,#79118,
#79119,#79120,#79121,#79122,#79123,#79124,#79125,#79126,#79127,#79128,#79129,
#79130,#79131,#79132,#79133,#79134,#79135,#79136,#79137,#79138,#79139),
 .UNSPECIFIED.,.F.,.F.,(4,2,2,2,2,2,2,2,2,2,2,2,2,2,2,2,2,2,2,2,2,2,2,2,
2,2,2,2,2,2,2,2,2,2,2,2,2,2,2,2,2,2,2,2,2,2,2,2,2,2,2,2,2,2,2,2,2,2,2,2,
2,2,2,2,2,2,2,2,2,2,2,2,2,2,2,2,2,2,2,2,2,2,2,2,2,2,2,2,2,4),(0.921536811180233,
0.933102305825647,0.93829814936006,0.942244392776091,0.946526181407856,
0.953609051144324,0.975225115898132,1.00636807831321,1.01114863381681,1.01373509769844,
1.01596460421077,1.01909092016773,1.02723855626277,1.04087524380193,1.07610123448567,
1.08271456454244,1.08690191698484,1.09088854307265,1.09643757221683,1.11146515620285,
1.14020497718251,1.15427347636024,1.1580719595924,1.16042437349447,1.16277828739304,
1.16658391377995,1.18225107578502,1.21552044046769,1.22607044466416,1.23099793363849,
1.23490269947428,1.23937704554867,1.24742687727401,1.27418521079061,1.29851254812712,
1.30324974413601,1.30582693994069,1.30805858526487,1.31120167090468,1.31947285944942,
1.33344233575875,1.36796840418727,1.37468191474462,1.37888924183572,1.38286548417652,
1.38835180196037,1.40284329110401,1.42934183738193,1.4461111482636,1.45002365352312,
1.45240028330528,1.45473148007281,1.45842948352441,1.47233375164659,1.50578096121556,
1.51730256505604,1.52247392006901,1.52641636542503,1.53070854130175,1.53784399265397,
1.55985146052565,1.58490301413319,1.59346807218349,1.5967335364347,1.59898318655205,
1.60150084039512,1.60608435904497,1.61206071541396,1.62719168951254,1.65942690059912,
1.66643651562949,1.6707031660692,1.67465395077992,1.6799768566265,1.69317879305881,
1.7152293506433,1.73637636394252,1.74122156651758,1.74382140746739,1.74604740527106,
1.74914854381478,1.75711740949147,1.77028454270463,1.80305818921991,1.81057782345509,
1.81535723619063,1.81925261036891,1.82294237665107,1.82746270499088,1.84281035796432),
 .UNSPECIFIED.);
#1391=B_SPLINE_CURVE_WITH_KNOTS('',3,(#79144,#79145,#79146,#79147,#79148,
#79149,#79150,#79151,#79152,#79153,#79154,#79155,#79156,#79157,#79158,#79159,
#79160,#79161,#79162,#79163,#79164,#79165,#79166,#79167,#79168,#79169,#79170,
#79171,#79172,#79173,#79174,#79175,#79176,#79177,#79178,#79179,#79180,#79181,
#79182,#79183,#79184,#79185,#79186,#79187,#79188,#79189,#79190,#79191,#79192,
#79193,#79194,#79195,#79196,#79197,#79198,#79199,#79200,#79201,#79202,#79203,
#79204,#79205,#79206,#79207,#79208,#79209,#79210,#79211,#79212,#79213,#79214,
#79215,#79216,#79217,#79218,#79219,#79220,#79221,#79222,#79223,#79224,#79225,
#79226,#79227,#79228,#79229,#79230,#79231,#79232,#79233,#79234,#79235,#79236,
#79237,#79238,#79239,#79240,#79241,#79242,#79243,#79244,#79245,#79246,#79247,
#79248,#79249,#79250,#79251,#79252,#79253,#79254,#79255,#79256,#79257,#79258,
#79259,#79260,#79261,#79262,#79263,#79264,#79265,#79266,#79267,#79268,#79269,
#79270,#79271,#79272,#79273,#79274,#79275,#79276,#79277,#79278,#79279,#79280,
#79281,#79282,#79283,#79284,#79285,#79286,#79287,#79288,#79289,#79290,#79291,
#79292,#79293,#79294,#79295,#79296,#79297,#79298,#79299,#79300,#79301,#79302,
#79303,#79304,#79305,#79306,#79307,#79308,#79309,#79310,#79311,#79312,#79313,
#79314,#79315,#79316,#79317,#79318,#79319),.UNSPECIFIED.,.F.,.F.,(4,2,2,
2,2,2,2,2,2,2,2,2,2,2,2,2,2,2,2,2,2,2,2,2,2,2,2,2,2,2,2,2,2,2,2,2,2,2,2,
2,2,2,2,2,2,2,2,2,2,2,2,2,2,2,2,2,2,2,2,2,2,2,2,2,2,2,2,2,2,2,2,2,2,2,2,
2,2,2,2,2,2,2,2,2,2,2,2,4),(0.000151238077915164,0.00640778730925637,0.0241768538239276,
0.0443967716212503,0.0590010604211495,0.064521123245535,0.0685223682871949,
0.0727579144485144,0.0795236907992127,0.113759664550157,0.127834666857619,
0.136153776683449,0.139314846465747,0.141560478828986,0.144157909720819,
0.148945579093672,0.173563724311456,0.193328512494067,0.205751787152006,
0.210986928466309,0.214946285907897,0.219294769585089,0.226622332152765,
0.254155110444918,0.272168588386821,0.281791588150937,0.285115860822626,
0.287386046279402,0.289906115344984,0.294454548663721,0.32219268496662,
0.345957217577991,0.354028451919345,0.358524384173052,0.362454721541285,
0.367425137127329,0.378125390087704,0.411182228591696,0.426792792689984,
0.430609147265738,0.432974769041553,0.435059838106147,0.438622607759043,
0.449646953942215,0.481189474948909,0.496803212158547,0.502437544228046,
0.506457399582265,0.510656521033133,0.517241402763472,0.552728545424471,
0.566205989494761,0.574302306092487,0.577432697203122,0.579674215979176,
0.582288240746136,0.587155034969317,0.606549158563455,0.624289437562284,
0.642286709307247,0.64815265127695,0.652213355222013,0.656352072615005,
0.662630417998326,0.686469790386345,0.70461978232871,0.718970555238927,
0.722711782011883,0.725061547901424,0.72715827122535,0.730786062017507,
0.742569403168577,0.773388740911311,0.78886397038524,0.794483058935702,
0.798500239609215,0.802703698255418,0.809310815798728,0.844644609390707,
0.858192513107553,0.866315337534283,0.869449333425159,0.871691242973195,
0.874303083820267,0.879159761816994,0.89837576450849,0.921314446213366,
0.921425937241738),.UNSPECIFIED.);
#1392=B_SPLINE_CURVE_WITH_KNOTS('',3,(#79321,#79322,#79323,#79324),
 .UNSPECIFIED.,.F.,.F.,(4,4),(1.84281035796432,1.84292178567195),
 .UNSPECIFIED.);
#1393=B_SPLINE_CURVE_WITH_KNOTS('',3,(#79325,#79326,#79327,#79328,#79329,
#79330,#79331,#79332,#79333,#79334,#79335,#79336,#79337,#79338,#79339,#79340,
#79341,#79342,#79343,#79344,#79345,#79346,#79347,#79348,#79349,#79350,#79351,
#79352,#79353,#79354,#79355,#79356,#79357,#79358,#79359,#79360,#79361,#79362,
#79363,#79364,#79365,#79366,#79367,#79368,#79369,#79370,#79371,#79372,#79373,
#79374,#79375,#79376,#79377,#79378,#79379,#79380,#79381,#79382,#79383,#79384,
#79385,#79386,#79387,#79388,#79389,#79390,#79391,#79392,#79393,#79394,#79395,
#79396,#79397,#79398,#79399,#79400,#79401,#79402,#79403,#79404,#79405,#79406,
#79407,#79408,#79409,#79410,#79411,#79412,#79413,#79414,#79415,#79416,#79417,
#79418,#79419,#79420,#79421,#79422,#79423,#79424,#79425,#79426,#79427,#79428,
#79429,#79430,#79431,#79432,#79433,#79434,#79435,#79436,#79437,#79438,#79439,
#79440,#79441,#79442,#79443,#79444,#79445,#79446,#79447,#79448,#79449,#79450,
#79451,#79452,#79453,#79454,#79455,#79456,#79457,#79458,#79459,#79460,#79461,
#79462,#79463,#79464,#79465,#79466,#79467,#79468,#79469,#79470,#79471,#79472,
#79473,#79474,#79475,#79476,#79477,#79478,#79479,#79480,#79481,#79482,#79483,
#79484,#79485,#79486,#79487,#79488,#79489,#79490,#79491,#79492,#79493,#79494,
#79495,#79496,#79497,#79498),.UNSPECIFIED.,.F.,.F.,(4,2,2,2,2,2,2,2,2,2,
2,2,2,2,2,2,2,2,2,2,2,2,2,2,2,2,2,2,2,2,2,2,2,2,2,2,2,2,2,2,2,2,2,2,2,2,
2,2,2,2,2,2,2,2,2,2,2,2,2,2,2,2,2,2,2,2,2,2,2,2,2,2,2,2,2,2,2,2,2,2,2,2,
2,2,2,2,4),(9.51235209599495E-5,0.0254712809801649,0.036344157606092,0.0433755455167485,
0.0463376544890454,0.0485498550574796,0.051240824885174,0.0567007971363031,
0.0881640135096535,0.10302453771775,0.113405108105549,0.118304349458389,
0.122171220469519,0.126651569142186,0.134509915824775,0.168374895491002,
0.181248800535287,0.189104648942411,0.192189999063907,0.194414328269927,
0.197023845472009,0.201914280949435,0.224412910071305,0.255222317976374,
0.261936602416707,0.266143988178005,0.270119998901647,0.275605528739687,
0.289023923727613,0.32138809083701,0.333994082834365,0.337595368661739,
0.339906772155914,0.342308150281517,0.346337149371391,0.368338412255291,
0.390887833173197,0.404251145501673,0.409595843611872,0.413550050819569,
0.417808465770291,0.424776318516942,0.457346218286631,0.472286149789644,
0.480905779082826,0.484094930147705,0.486332944179747,0.488886250864103,
0.49351202097049,0.519250868680626,0.538470628798861,0.550679285488755,
0.555864135195988,0.559796109285014,0.564123666843638,0.571435193356866,
0.598732957987925,0.616943959622223,0.626615219183135,0.629932692322875,
0.632190900907919,0.634686592727932,0.639164003504284,0.667453160389326,
0.685248457400381,0.696900922679556,0.702002996726931,0.705924664579863,
0.71029350628798,0.717811876018003,0.752234438789054,0.765241567059644,
0.773148921190863,0.776241360224881,0.77846633646503,0.781071218632888,
0.785940392266249,0.805559282827188,0.828216195149896,0.842104568460713,
0.847516653777062,0.851480837172484,0.855713344411704,0.862553637736423,
0.89612254154228,0.917253116128758,0.921229644102655),.UNSPECIFIED.);
#1394=B_SPLINE_CURVE_WITH_KNOTS('',3,(#79504,#79505,#79506,#79507,#79508,
#79509,#79510,#79511,#79512,#79513,#79514,#79515,#79516,#79517,#79518,#79519,
#79520,#79521,#79522,#79523,#79524,#79525,#79526,#79527,#79528,#79529,#79530,
#79531,#79532,#79533,#79534,#79535,#79536,#79537,#79538,#79539,#79540,#79541,
#79542,#79543,#79544,#79545,#79546,#79547,#79548,#79549,#79550,#79551,#79552,
#79553,#79554,#79555,#79556,#79557,#79558,#79559,#79560,#79561,#79562,#79563,
#79564,#79565,#79566,#79567,#79568,#79569,#79570,#79571,#79572,#79573,#79574,
#79575,#79576,#79577,#79578,#79579,#79580,#79581,#79582,#79583,#79584,#79585,
#79586,#79587,#79588,#79589,#79590,#79591,#79592,#79593,#79594,#79595,#79596,
#79597,#79598,#79599,#79600,#79601,#79602,#79603,#79604,#79605,#79606,#79607,
#79608,#79609,#79610,#79611,#79612,#79613,#79614,#79615,#79616,#79617,#79618,
#79619,#79620,#79621,#79622,#79623,#79624,#79625,#79626,#79627,#79628,#79629,
#79630,#79631,#79632,#79633,#79634,#79635,#79636,#79637,#79638,#79639,#79640,
#79641,#79642,#79643,#79644,#79645,#79646,#79647,#79648,#79649,#79650,#79651,
#79652,#79653,#79654,#79655,#79656,#79657,#79658,#79659,#79660,#79661,#79662,
#79663,#79664,#79665,#79666,#79667,#79668,#79669,#79670,#79671,#79672,#79673,
#79674,#79675,#79676,#79677,#79678,#79679,#79680,#79681,#79682,#79683,#79684,
#79685,#79686,#79687),.UNSPECIFIED.,.F.,.F.,(4,2,2,2,2,2,2,2,2,2,2,2,2,
2,2,2,2,2,2,2,2,2,2,2,2,2,2,2,2,2,2,2,2,2,2,2,2,2,2,2,2,2,2,2,2,2,2,2,2,
2,2,2,2,2,2,2,2,2,2,2,2,2,2,2,2,2,2,2,2,2,2,2,2,2,2,2,2,2,2,2,2,2,2,2,2,
2,2,2,2,2,2,4),(0.921842322598426,0.921971004497343,0.953992808066859,0.95863137835825,
0.961196190559706,0.963450209066568,0.96667227576309,0.975452321063484,
0.990826999153283,1.02258444635569,1.02966656685149,1.03396661469429,1.03794294671248,
1.04329390430075,1.05654948664906,1.07872654003213,1.09963636127533,1.10449896000988,
1.10711284661048,1.10935544198543,1.11248945502758,1.12060776202534,1.13414219482962,
1.16954541820336,1.17614788821059,1.18035113388906,1.18436999604957,1.18999463742742,
1.20551365643492,1.23655745542615,1.24809404399398,1.25170122820025,1.25379448311335,
1.25614950189284,1.25991490605654,1.27463773786905,1.29250516226475,1.31626705750933,
1.32253758684407,1.32667515477448,1.33073766666332,1.33661152548057,1.35469749621604,
1.37258465769031,1.39173335279365,1.39658698975407,1.39919843186789,1.40144092021604,
1.40457695660832,1.4127109907312,1.42628742327495,1.46160319547748,1.46821889530715,
1.47242474818155,1.4764420752362,1.48205780680045,1.49749644282553,1.52813234737186,
1.54009096004661,1.54373725114703,1.54583768562363,1.54818391752498,1.55190670803212,
1.56596634234,1.60015381234387,1.61129708631472,1.61633952572813,1.62027689499638,
1.62472830561035,1.6325711421564,1.64252632257581,1.66957029060646,1.68563487863911,
1.68953089677225,1.69191363141661,1.69426928176339,1.69803771557473,1.71281034555871,
1.73063199953393,1.75438234934481,1.76065187104284,1.76478925975218,1.76885197036206,
1.7747268198483,1.79282492422776,1.8166379608318,1.824977963108,1.83309108917276,
1.83630120185999,1.83851390674685,1.84074373157238,1.84320277452714),
 .UNSPECIFIED.);
#1395=B_SPLINE_CURVE_WITH_KNOTS('',3,(#79688,#79689,#79690,#79691),
 .UNSPECIFIED.,.F.,.F.,(4,4),(0.000126975314923754,0.000151238077915164),
 .UNSPECIFIED.);
#1396=B_SPLINE_CURVE_WITH_KNOTS('',3,(#79693,#79694,#79695,#79696,#79697,
#79698,#79699,#79700,#79701,#79702,#79703,#79704,#79705,#79706,#79707,#79708,
#79709,#79710,#79711,#79712,#79713,#79714,#79715,#79716,#79717,#79718,#79719,
#79720,#79721,#79722,#79723,#79724,#79725,#79726,#79727,#79728,#79729,#79730,
#79731,#79732,#79733,#79734,#79735,#79736,#79737,#79738,#79739,#79740,#79741,
#79742,#79743,#79744,#79745,#79746,#79747,#79748,#79749,#79750,#79751,#79752,
#79753,#79754,#79755,#79756,#79757,#79758,#79759,#79760,#79761,#79762,#79763,
#79764,#79765,#79766,#79767,#79768,#79769,#79770,#79771,#79772,#79773,#79774,
#79775,#79776,#79777,#79778,#79779,#79780,#79781,#79782,#79783,#79784,#79785,
#79786,#79787,#79788,#79789,#79790,#79791,#79792,#79793,#79794,#79795,#79796,
#79797,#79798,#79799,#79800,#79801,#79802,#79803,#79804,#79805,#79806,#79807,
#79808,#79809,#79810,#79811,#79812,#79813,#79814,#79815,#79816,#79817,#79818,
#79819,#79820,#79821,#79822,#79823,#79824,#79825,#79826,#79827,#79828,#79829,
#79830,#79831,#79832,#79833,#79834,#79835,#79836,#79837,#79838,#79839,#79840,
#79841,#79842,#79843,#79844,#79845,#79846,#79847,#79848,#79849,#79850,#79851,
#79852,#79853,#79854,#79855,#79856,#79857,#79858,#79859,#79860,#79861,#79862,
#79863,#79864,#79865,#79866,#79867,#79868,#79869,#79870,#79871,#79872,#79873,
#79874,#79875,#79876,#79877,#79878),.UNSPECIFIED.,.F.,.F.,(4,2,2,2,2,2,
2,2,2,2,2,2,2,2,2,2,2,2,2,2,2,2,2,2,2,2,2,2,2,2,2,2,2,2,2,2,2,2,2,2,2,2,
2,2,2,2,2,2,2,2,2,2,2,2,2,2,2,2,2,2,2,2,2,2,2,2,2,2,2,2,2,2,2,2,2,2,2,2,
2,2,2,2,2,2,2,2,2,2,2,2,2,2,4),(0.921229644102655,0.921252861741337,0.923647958621843,
0.925963893240356,0.92958803755803,0.9424822474088,0.977059571664178,0.988600431906422,
0.993774773620674,0.997717424179817,1.00200779006674,1.00913525694689,1.03108540419854,
1.05601803235829,1.06472589268181,1.0680103578849,1.0702629688971,1.07277213983572,
1.07731506511373,1.08322095399415,1.09804365324033,1.13085739837009,1.13779700975506,
1.14204933806114,1.14600506734153,1.15136306540535,1.16483280765513,1.18772466977566,
1.20759536430365,1.21248386352344,1.21509268159662,1.2173166054511,1.22040173936432,
1.22825836083793,1.24113624670114,1.27500920657182,1.28286768889638,1.28734752976231,
1.29121360756154,1.29611137448384,1.3064872218076,1.32133792104234,1.35278193480356,
1.35823782508062,1.36092764899221,1.36313937728964,1.36610152882785,1.37313577565245,
1.38401722438189,1.41905708523396,1.4280787614883,1.43279225763882,1.43668544448536,
1.44132861139383,1.45026601369845,1.46221771666168,1.47991780114922,1.49960777676112,
1.50448173207187,1.50708739755177,1.50931178499273,1.51240179746173,1.52029366159329,
1.53326247170346,1.56751420358692,1.57508125479721,1.57950022734373,1.58341166315637,
1.58842308980116,1.59949579375397,1.61590354368184,1.64226795947809,1.64923120363644,
1.65198465555012,1.65423578332787,1.65674773842603,1.66130505856827,1.66723622154103,
1.68217083741537,1.71476876415928,1.72172914268572,1.72598528623175,1.72993883950468,
1.73528495096963,1.74866756738684,1.77128479313777,1.79315816394817,1.79717905604436,
1.79957825716694,1.80188984567116,1.80549507613821,1.81815989221302,1.84218579280452),
 .UNSPECIFIED.);
#1397=B_SPLINE_CURVE_WITH_KNOTS('',3,(#79879,#79880,#79881,#79882),
 .UNSPECIFIED.,.F.,.F.,(4,4),(8.31121291700962E-5,0.000212271119411096),
 .UNSPECIFIED.);
#1398=B_SPLINE_CURVE_WITH_KNOTS('',3,(#79887,#79888,#79889,#79890,#79891,
#79892,#79893,#79894,#79895,#79896,#79897,#79898,#79899,#79900,#79901,#79902,
#79903,#79904,#79905,#79906,#79907,#79908,#79909,#79910,#79911,#79912,#79913,
#79914,#79915,#79916,#79917,#79918,#79919,#79920,#79921,#79922,#79923,#79924,
#79925,#79926,#79927,#79928,#79929,#79930,#79931,#79932,#79933,#79934,#79935,
#79936,#79937,#79938,#79939,#79940,#79941,#79942,#79943,#79944,#79945,#79946,
#79947,#79948,#79949,#79950,#79951,#79952,#79953,#79954,#79955,#79956,#79957,
#79958,#79959,#79960,#79961,#79962,#79963,#79964,#79965,#79966,#79967,#79968,
#79969,#79970,#79971,#79972,#79973,#79974,#79975,#79976,#79977,#79978,#79979,
#79980,#79981,#79982,#79983,#79984,#79985,#79986,#79987,#79988,#79989,#79990,
#79991,#79992,#79993,#79994,#79995,#79996,#79997,#79998,#79999,#80000,#80001,
#80002,#80003,#80004,#80005,#80006,#80007,#80008,#80009,#80010,#80011,#80012,
#80013,#80014,#80015,#80016,#80017,#80018,#80019,#80020,#80021,#80022,#80023,
#80024,#80025,#80026,#80027,#80028,#80029,#80030,#80031,#80032,#80033,#80034,
#80035,#80036,#80037,#80038,#80039,#80040,#80041,#80042,#80043,#80044,#80045,
#80046,#80047,#80048,#80049,#80050,#80051,#80052,#80053,#80054,#80055,#80056,
#80057,#80058,#80059,#80060,#80061,#80062,#80063,#80064,#80065,#80066,#80067,
#80068),.UNSPECIFIED.,.F.,.F.,(4,2,2,2,2,2,2,2,2,2,2,2,2,2,2,2,2,2,2,2,
2,2,2,2,2,2,2,2,2,2,2,2,2,2,2,2,2,2,2,2,2,2,2,2,2,2,2,2,2,2,2,2,2,2,2,2,
2,2,2,2,2,2,2,2,2,2,2,2,2,2,2,2,2,2,2,2,2,2,2,2,2,2,2,2,2,2,2,2,2,2,4),
(0.000409495598106863,0.00411624641659977,0.00763961738565761,0.0112036564741097,
0.0151649190678298,0.0211020083759937,0.0401696307536014,0.0696775020094234,
0.0808615608811188,0.0842468300984096,0.0864683303915771,0.0888753657548912,
0.0929102841698461,0.1151298837162,0.13769433779516,0.151127845037877,0.15653232530443,
0.160545597077753,0.164885726680577,0.172045944542388,0.201674149848935,
0.217525111103473,0.226457858934173,0.229730217775301,0.232019891080921,
0.234623937612574,0.239519452166005,0.257980716661014,0.281866326541254,
0.295650904773997,0.30108708962904,0.305093059636614,0.309395012481321,
0.316411725077301,0.351641300955629,0.364817368041932,0.372806612421837,
0.375929395255939,0.378172261243137,0.380787642424671,0.385687728159702,
0.405590755672584,0.428461440360474,0.441926331415388,0.447288278283224,
0.451248924134294,0.455508397536511,0.46246369176431,0.497800596861752,
0.511045504275207,0.519049549901295,0.522156552013692,0.524388250971347,
0.527002496885108,0.531869713372902,0.551271791746638,0.569022418895147,
0.581147515764566,0.590189786786111,0.594875004103136,0.598799592790457,
0.603548366629588,0.612638933064306,0.647472553043876,0.663425292944995,
0.667264405827028,0.66963865230539,0.671724945080156,0.675284495131672,
0.686249434792894,0.717842019912523,0.73346494739358,0.73910226002657,0.743124524387538,
0.747326509768823,0.753916794824024,0.789411244238249,0.802900186259938,
0.811002065689626,0.814133937038144,0.816375819054558,0.818988612152688,
0.823851887188071,0.843188569044613,0.860438188133539,0.878909724832397,
0.884814292786726,0.888880771019699,0.893008252364856,0.899235153875353,
0.921842322598426),.UNSPECIFIED.);
#1399=B_SPLINE_CURVE_WITH_KNOTS('',3,(#80069,#80070,#80071,#80072,#80073,
#80074,#80075,#80076,#80077,#80078,#80079,#80080,#80081,#80082,#80083,#80084,
#80085,#80086,#80087,#80088,#80089,#80090,#80091,#80092,#80093,#80094,#80095,
#80096,#80097,#80098,#80099,#80100,#80101,#80102,#80103,#80104,#80105,#80106,
#80107,#80108,#80109,#80110,#80111,#80112,#80113,#80114,#80115,#80116,#80117,
#80118,#80119,#80120,#80121,#80122,#80123,#80124,#80125,#80126,#80127,#80128,
#80129,#80130,#80131,#80132,#80133,#80134,#80135,#80136,#80137,#80138,#80139,
#80140,#80141,#80142,#80143,#80144,#80145,#80146,#80147,#80148,#80149,#80150,
#80151,#80152,#80153,#80154,#80155,#80156,#80157,#80158,#80159,#80160,#80161,
#80162,#80163,#80164,#80165,#80166,#80167,#80168,#80169,#80170,#80171,#80172,
#80173,#80174,#80175,#80176,#80177,#80178,#80179,#80180,#80181,#80182,#80183,
#80184,#80185,#80186,#80187,#80188,#80189,#80190,#80191,#80192,#80193,#80194,
#80195,#80196,#80197,#80198,#80199,#80200,#80201,#80202,#80203,#80204,#80205,
#80206,#80207,#80208,#80209,#80210,#80211,#80212,#80213,#80214,#80215,#80216,
#80217,#80218,#80219,#80220,#80221,#80222,#80223,#80224,#80225,#80226,#80227,
#80228,#80229,#80230,#80231,#80232,#80233,#80234,#80235,#80236,#80237,#80238,
#80239,#80240,#80241,#80242,#80243,#80244,#80245,#80246,#80247,#80248,#80249,
#80250,#80251,#80252),.UNSPECIFIED.,.F.,.F.,(4,2,2,2,2,2,2,2,2,2,2,2,2,
2,2,2,2,2,2,2,2,2,2,2,2,2,2,2,2,2,2,2,2,2,2,2,2,2,2,2,2,2,2,2,2,2,2,2,2,
2,2,2,2,2,2,2,2,2,2,2,2,2,2,2,2,2,2,2,2,2,2,2,2,2,2,2,2,2,2,2,2,2,2,2,2,
2,2,2,2,2,2,4),(0.000212271119411096,0.0184268769916361,0.0236198335754554,
0.0275033491686757,0.0314545942917832,0.0357215569034563,0.0427312808188781,
0.0770023918457398,0.0907424764220856,0.0989289238335929,0.102060439672156,
0.10429061668719,0.106874158474456,0.111640871476838,0.136168695473555,
0.156036812196146,0.168486747688842,0.173706794257779,0.17764386491016,
0.181956000702848,0.189188684272954,0.218973749821132,0.235507685860731,
0.244662825852073,0.247919720916535,0.250168463491246,0.252691371725201,
0.25729738996751,0.289759207007853,0.304846801269719,0.315331942567293,
0.320249118054466,0.324118070074919,0.328587599438841,0.336391443921904,
0.370329630345493,0.383220768259483,0.391083377394536,0.394169727893822,
0.396393713088988,0.399000675774037,0.403883778725287,0.423689832784035,
0.44151716200985,0.45336605122852,0.462248390380849,0.466880445984012,0.470772425874221,
0.475494243934464,0.484563724267043,0.522621234162304,0.535893049872872,
0.539544970708945,0.541866135222855,0.544254344338416,0.548219381464529,
0.567633765934114,0.598862226160437,0.608110550277805,0.612813124860416,
0.616708997101244,0.621369365724602,0.630109692230653,0.641888483931618,
0.659838638339606,0.679589654221265,0.684470598521228,0.687079480259172,
0.689309007572819,0.692409143629907,0.700341149783576,0.713410856060205,
0.748164606225848,0.755388263697132,0.759701958755032,0.763645254168221,
0.768881291304163,0.781417411278475,0.8015094835942,0.825737252797056,0.830476980431821,
0.833054615275502,0.835275731146635,0.838393724790873,0.846560243905356,
0.860258557245317,0.895607680430056,0.90222007170262,0.906392735315957,
0.9103542814628,0.915848105643038,0.92152398119564),.UNSPECIFIED.);
#1400=B_SPLINE_CURVE_WITH_KNOTS('',3,(#80258,#80259,#80260,#80261,#80262,
#80263,#80264,#80265,#80266,#80267,#80268,#80269,#80270,#80271,#80272,#80273,
#80274,#80275,#80276,#80277,#80278,#80279,#80280,#80281,#80282,#80283,#80284,
#80285,#80286,#80287,#80288,#80289,#80290,#80291,#80292,#80293,#80294,#80295,
#80296,#80297,#80298,#80299,#80300,#80301,#80302,#80303,#80304,#80305,#80306,
#80307,#80308,#80309,#80310,#80311,#80312,#80313,#80314,#80315,#80316,#80317,
#80318,#80319,#80320,#80321,#80322,#80323,#80324,#80325,#80326,#80327,#80328,
#80329,#80330,#80331,#80332,#80333,#80334,#80335,#80336,#80337,#80338,#80339,
#80340,#80341,#80342,#80343,#80344,#80345,#80346,#80347,#80348,#80349,#80350,
#80351,#80352,#80353,#80354,#80355,#80356,#80357,#80358,#80359,#80360,#80361,
#80362,#80363,#80364,#80365,#80366,#80367,#80368,#80369,#80370,#80371,#80372,
#80373,#80374,#80375,#80376,#80377,#80378,#80379,#80380,#80381,#80382,#80383,
#80384,#80385,#80386,#80387),.UNSPECIFIED.,.F.,.F.,(4,2,2,2,2,2,2,2,2,2,
2,2,2,2,2,2,2,2,2,2,2,2,2,2,2,2,2,2,2,2,2,2,2,2,2,2,2,2,2,2,2,2,2,2,2,2,
2,2,2,2,2,2,2,2,2,2,2,2,2,2,2,2,2,2,4),(-0.589266859322642,-0.583170718802222,
-0.579282628579395,-0.576924566074347,-0.57452032528388,-0.570412233191057,
-0.565139040401791,-0.55198759141902,-0.528926529180157,-0.522537395514901,
-0.518409672101166,-0.51436475306196,-0.50843254142529,-0.48635380224999,
-0.46600745613857,-0.461886461509982,-0.459478543697714,-0.457114571232146,
-0.453217738090236,-0.435024959395931,-0.411351068044394,-0.405015281957827,
-0.400894937262368,-0.396837082845925,-0.390846789372038,-0.369237742364032,
-0.348468253784916,-0.344366071710034,-0.341963344537253,-0.339618433922597,
-0.335756960468933,-0.330900902638634,-0.319540174427223,-0.292928533939326,
-0.286899037196489,-0.28325680050945,-0.279254808303444,-0.27347579982458,
-0.251111995620155,-0.230726430683364,-0.226613577869565,-0.224214201521056,
-0.221850241821066,-0.217964566466566,-0.213079026155885,-0.201639775208353,
-0.175312646047459,-0.169228113439053,-0.165548630702281,-0.161499412822675,
-0.155632464107968,-0.132699692598671,-0.113296622916967,-0.109066948012962,
-0.106625296331815,-0.104230015179095,-0.100293912091128,-0.0834054084904788,
-0.0590223232485894,-0.0528309458458233,-0.0487145198233409,-0.0445880120408051,
-0.0383459587393695,-0.0308954481058898,-5.3213449454262E-5),
 .UNSPECIFIED.);
#1401=B_SPLINE_CURVE_WITH_KNOTS('',3,(#80390,#80391,#80392,#80393,#80394,
#80395,#80396,#80397,#80398,#80399,#80400,#80401,#80402,#80403,#80404,#80405,
#80406,#80407,#80408,#80409,#80410,#80411,#80412,#80413,#80414,#80415,#80416,
#80417,#80418,#80419,#80420,#80421,#80422,#80423,#80424,#80425,#80426,#80427,
#80428,#80429,#80430,#80431,#80432,#80433,#80434,#80435,#80436,#80437,#80438,
#80439,#80440,#80441,#80442,#80443,#80444,#80445,#80446,#80447,#80448,#80449,
#80450,#80451,#80452,#80453,#80454,#80455,#80456,#80457,#80458,#80459,#80460,
#80461,#80462,#80463,#80464,#80465,#80466,#80467,#80468,#80469,#80470,#80471,
#80472,#80473,#80474,#80475,#80476,#80477,#80478,#80479,#80480,#80481,#80482,
#80483,#80484,#80485),.UNSPECIFIED.,.F.,.F.,(4,2,2,2,2,2,2,2,2,2,2,2,2,
2,2,2,2,2,2,2,2,2,2,2,2,2,2,2,2,2,2,2,2,2,2,2,2,2,2,2,2,2,2,2,2,2,2,4),
(-4.19276052999992,-4.18994930679582,-4.18594508777967,-4.16986863132682,
-4.15061368004302,-4.14354516891226,-4.13898217474332,-4.13444468871921,
-4.12758398506696,-4.10080057567627,-4.08183773106484,-4.07790888789601,
-4.07551930049204,-4.07316304090163,-4.06917333893694,-4.04805153823428,
-4.02702609715168,-4.0213060269127,-4.01739784825908,-4.01341394757536,
-4.0072877679487,-3.98038949311294,-3.9627452339993,-3.9591534892204,-3.95690556319255,
-3.95448562980752,-3.95031807462353,-3.93056727411159,-3.90816359210308,
-3.90200162654388,-3.89787209907124,-3.89370785084629,-3.88734825741719,
-3.86478161281914,-3.8519079261705,-3.84668583278294,-3.84259510490349,
-3.84015915922247,-3.83772960223034,-3.83360376691708,-3.81293046552367,
-3.79818007879994,-3.79123456879836,-3.78530836193634,-3.78123107649018,
-3.77753256329089,-3.77142850268503,-3.74878577142885),.UNSPECIFIED.);
#1402=B_SPLINE_CURVE_WITH_KNOTS('',3,(#80490,#80491,#80492,#80493,#80494,
#80495,#80496,#80497,#80498,#80499,#80500,#80501,#80502,#80503,#80504,#80505,
#80506,#80507,#80508,#80509,#80510,#80511,#80512,#80513,#80514,#80515,#80516,
#80517,#80518,#80519,#80520,#80521,#80522,#80523,#80524,#80525,#80526,#80527,
#80528,#80529,#80530,#80531,#80532,#80533,#80534,#80535,#80536,#80537,#80538,
#80539,#80540,#80541,#80542,#80543,#80544,#80545,#80546,#80547,#80548,#80549,
#80550,#80551,#80552,#80553,#80554,#80555,#80556,#80557,#80558,#80559,#80560,
#80561,#80562,#80563,#80564,#80565,#80566,#80567,#80568,#80569,#80570,#80571,
#80572,#80573,#80574,#80575,#80576,#80577,#80578,#80579,#80580,#80581,#80582,
#80583,#80584,#80585,#80586,#80587,#80588,#80589,#80590,#80591,#80592,#80593,
#80594,#80595,#80596,#80597,#80598,#80599,#80600,#80601,#80602,#80603,#80604,
#80605,#80606,#80607,#80608,#80609,#80610,#80611,#80612,#80613,#80614,#80615,
#80616,#80617,#80618,#80619,#80620,#80621,#80622,#80623,#80624,#80625,#80626,
#80627,#80628,#80629,#80630,#80631,#80632,#80633,#80634,#80635,#80636,#80637,
#80638,#80639,#80640,#80641,#80642,#80643,#80644,#80645,#80646,#80647,#80648,
#80649,#80650,#80651,#80652,#80653,#80654,#80655,#80656,#80657),
 .UNSPECIFIED.,.F.,.F.,(4,2,2,2,2,2,2,2,2,2,2,2,2,2,2,2,2,2,2,2,2,2,2,2,
2,2,2,2,2,2,2,2,2,2,2,2,2,2,2,2,2,2,2,2,2,2,2,2,2,2,2,2,2,2,2,2,2,2,2,2,
2,2,2,2,2,2,2,2,2,2,2,2,2,2,2,2,2,2,2,2,2,2,2,4),(-1.33107822423028,-1.3050320018944,
-1.29352334269686,-1.28862725477286,-1.28473927003311,-1.28238102649599,
-1.27997764655231,-1.27586998909895,-1.25527317844522,-1.24040299895147,
-1.23344479071331,-1.22752376544648,-1.22348303462989,-1.21935697758132,
-1.21296521024282,-1.19000648247202,-1.17679209785019,-1.17150596072924,
-1.167391345638,-1.16498651647294,-1.16262929642075,-1.15874699505247,-1.13586594724723,
-1.12214752262523,-1.11548487203495,-1.10974961776421,-1.10574044463247,
-1.10156804175507,-1.09492964179377,-1.06354709468678,-1.05596461857385,
-1.0506361941307,-1.04799435732233,-1.0457517447292,-1.0425264939916,-1.03300562585385,
-1.01250018669264,-1.00745771142861,-0.99629042329858,-0.991266084053232,
-0.987344994471621,-0.982927031662876,-0.974978443716631,-0.945943537066251,
-0.935095497126092,-0.93162620033597,-0.929369219910836,-0.926848823166088,
-0.92216173012559,-0.915839981154276,-0.896890053774975,-0.879939422309999,
-0.874368673094545,-0.870385474534947,-0.866163061257192,-0.859262813163703,
-0.836215843092881,-0.817929596279315,-0.814260367344161,-0.812172704452408,
-0.809788344228874,-0.80577706139847,-0.800671402384763,-0.7882705433584,
-0.7639355910793,-0.757650361450218,-0.753542860816598,-0.749483832103811,
-0.743466064666463,-0.720266428187892,-0.701448604858594,-0.697198526567655,
-0.69476553986039,-0.692431470813763,-0.688662429614172,-0.683967144826868,
-0.673267357442596,-0.64537574701729,-0.639534887130647,-0.635549041738243,
-0.631415436602443,-0.624978196448166,-0.60603202519002,-0.589266859322642),
 .UNSPECIFIED.);
#1403=B_SPLINE_CURVE_WITH_KNOTS('',3,(#80658,#80659,#80660,#80661,#80662,
#80663,#80664,#80665,#80666,#80667,#80668,#80669,#80670,#80671,#80672,#80673,
#80674,#80675,#80676,#80677,#80678,#80679,#80680,#80681,#80682,#80683,#80684,
#80685,#80686,#80687,#80688,#80689,#80690,#80691,#80692,#80693,#80694,#80695,
#80696,#80697,#80698,#80699,#80700,#80701,#80702,#80703,#80704,#80705,#80706,
#80707,#80708,#80709,#80710,#80711,#80712,#80713,#80714,#80715,#80716,#80717,
#80718,#80719,#80720,#80721,#80722,#80723,#80724,#80725,#80726,#80727,#80728,
#80729,#80730,#80731,#80732,#80733,#80734,#80735,#80736,#80737,#80738,#80739,
#80740,#80741,#80742,#80743,#80744,#80745,#80746,#80747,#80748,#80749,#80750,
#80751,#80752,#80753,#80754,#80755,#80756,#80757,#80758,#80759,#80760,#80761,
#80762,#80763,#80764,#80765,#80766,#80767,#80768,#80769,#80770,#80771,#80772,
#80773,#80774,#80775,#80776,#80777,#80778,#80779,#80780,#80781,#80782,#80783,
#80784,#80785,#80786,#80787,#80788,#80789,#80790,#80791,#80792,#80793,#80794,
#80795,#80796,#80797,#80798,#80799,#80800,#80801,#80802,#80803,#80804,#80805,
#80806,#80807,#80808,#80809,#80810,#80811,#80812,#80813,#80814,#80815,#80816,
#80817,#80818,#80819,#80820,#80821,#80822,#80823,#80824,#80825,#80826,#80827,
#80828,#80829,#80830,#80831),.UNSPECIFIED.,.F.,.F.,(4,2,2,2,2,2,2,2,2,2,
2,2,2,2,2,2,2,2,2,2,2,2,2,2,2,2,2,2,2,2,2,2,2,2,2,2,2,2,2,2,2,2,2,2,2,2,
2,2,2,2,2,2,2,2,2,2,2,2,2,2,2,2,2,2,2,2,2,2,2,2,2,2,2,2,2,2,2,2,2,2,2,2,
2,2,2,2,4),(-3.74878577142885,-3.74513268586829,-3.73368516973695,-3.72879060302111,
-3.72489574378074,-3.72252099603933,-3.72010128721677,-3.71593252466715,
-3.6962709835695,-3.6808830932062,-3.67379693917892,-3.66779525735489,-3.66373675479838,
-3.65962168377017,-3.65330880991156,-3.62900949669526,-3.61108907877409,
-3.60719463421898,-3.60483402410306,-3.60241642523591,-3.59828561734588,
-3.5779777972868,-3.55623228815388,-3.55011924059378,-3.54602175634493,
-3.54189259994483,-3.53560409840515,-3.51121683643263,-3.49369077938276,
-3.48974210793145,-3.4873584592989,-3.4849397112567,-3.48081012651282,-3.46045026784276,
-3.4386217365211,-3.43259050123225,-3.42851016267578,-3.4243693682092,-3.41800433983943,
-3.39433840732508,-3.3756601741496,-3.37194792679964,-3.36961426406217,
-3.36714145326678,-3.36273622494596,-3.34552910478588,-3.32880988610618,
-3.32140918127248,-3.31520775321776,-3.31109996549892,-3.30699802673909,
-3.30082904944937,-3.27525597638523,-3.2634835716586,-3.25851721587624,
-3.25458366732408,-3.2522074408767,-3.24979151647253,-3.24566953670843,
-3.22513373692306,-3.21024022498641,-3.20326485573878,-3.19732507142642,
-3.19326147317916,-3.18959120945997,-3.18357432911096,-3.15683174931789,
-3.14563307576243,-3.14080486450673,-3.13695218847295,-3.13459080225662,
-3.13215408713309,-3.12793120403522,-3.10855641959898,-3.09304243394775,
-3.08591678787807,-3.07988378275844,-3.07580424071015,-3.0716659719809,
-3.06530866194832,-3.04157478379966,-3.0233397238207,-3.01943395513676,
-3.01706231224811,-3.0146391799905,-3.01048184697966,-3.00705510852159),
 .UNSPECIFIED.);
#1404=B_SPLINE_CURVE_WITH_KNOTS('',3,(#80836,#80837,#80838,#80839,#80840,
#80841,#80842,#80843,#80844,#80845,#80846,#80847,#80848,#80849,#80850,#80851,
#80852,#80853,#80854,#80855,#80856,#80857,#80858,#80859,#80860,#80861,#80862,
#80863,#80864,#80865,#80866,#80867,#80868,#80869,#80870,#80871,#80872,#80873,
#80874,#80875,#80876,#80877,#80878,#80879,#80880,#80881,#80882,#80883,#80884,
#80885,#80886,#80887,#80888,#80889,#80890,#80891,#80892,#80893,#80894,#80895,
#80896,#80897,#80898,#80899,#80900,#80901,#80902,#80903,#80904,#80905,#80906,
#80907,#80908,#80909,#80910,#80911,#80912,#80913,#80914,#80915,#80916,#80917,
#80918,#80919,#80920,#80921,#80922,#80923,#80924,#80925,#80926,#80927,#80928,
#80929,#80930,#80931,#80932,#80933,#80934,#80935,#80936,#80937,#80938,#80939,
#80940,#80941,#80942,#80943,#80944,#80945,#80946,#80947,#80948,#80949,#80950,
#80951,#80952,#80953,#80954,#80955,#80956,#80957,#80958,#80959,#80960,#80961,
#80962,#80963,#80964,#80965,#80966,#80967,#80968,#80969,#80970,#80971,#80972,
#80973,#80974,#80975,#80976,#80977,#80978,#80979,#80980,#80981,#80982,#80983,
#80984,#80985,#80986,#80987,#80988,#80989,#80990,#80991,#80992,#80993,#80994,
#80995,#80996,#80997,#80998,#80999),.UNSPECIFIED.,.F.,.F.,(4,2,2,2,2,2,
2,2,2,2,2,2,2,2,2,2,2,2,2,2,2,2,2,2,2,2,2,2,2,2,2,2,2,2,2,2,2,2,2,2,2,2,
2,2,2,2,2,2,2,2,2,2,2,2,2,2,2,2,2,2,2,2,2,2,2,2,2,2,2,2,2,2,2,2,2,2,2,2,
2,2,2,4),(-2.07270848450232,-2.05637947900051,-2.05041870419527,-2.04637147445068,
-2.04225505343102,-2.03591271074969,-2.01900120304341,-1.99397215540331,
-1.99006327819747,-1.98770094498518,-1.98530267068136,-1.98121909476245,
-1.9602542642696,-1.93879416667414,-1.93285129288563,-1.9288071244785,-1.92468663844824,
-1.91832282391021,-1.89492544567431,-1.88197921092116,-1.87675187753393,
-1.8726711616138,-1.87027351041234,-1.86791062294112,-1.8639991628537,-1.84138088300711,
-1.82231447415694,-1.8158623812433,-1.81172544622901,-1.80774035593035,
-1.80190771595934,-1.77396521320056,-1.76329097847408,-1.75860209243932,
-1.75483715834937,-1.75250358932328,-1.75006987929346,-1.74581338271324,
-1.72667238834097,-1.71104858767693,-1.70390826063274,-1.69787418030314,
-1.6938137410089,-1.68971226005504,-1.68345198973634,-1.65885125465335,
-1.64142704406966,-1.63747153795965,-1.635099585313,-1.63271141137436,-1.62867733838942,
-1.60716657590448,-1.58643072462178,-1.58036082221973,-1.57629391359855,
-1.57219943018413,-1.5659776091017,-1.54101187658049,-1.52382727082877,
-1.51989520821546,-1.51752802383727,-1.51513466295542,-1.5110755888295,
-1.48981970540655,-1.46859311414981,-1.46265374384937,-1.45860994192361,
-1.45448823171113,-1.44811913016952,-1.4308368298893,-1.40617903421335,
-1.40229525404027,-1.39993784924348,-1.39753348908643,-1.39342103817434,
-1.37293331858767,-1.35070763700637,-1.34491619039688,-1.34089785200684,
-1.33723427328462,-1.33114995542605,-1.33107822423028),.UNSPECIFIED.);
#1405=B_SPLINE_CURVE_WITH_KNOTS('',3,(#81000,#81001,#81002,#81003,#81004,
#81005,#81006,#81007,#81008,#81009,#81010,#81011,#81012,#81013,#81014,#81015,
#81016,#81017,#81018,#81019,#81020,#81021,#81022,#81023,#81024,#81025,#81026,
#81027,#81028,#81029,#81030,#81031,#81032,#81033,#81034,#81035,#81036,#81037,
#81038,#81039,#81040,#81041,#81042,#81043,#81044,#81045,#81046,#81047,#81048,
#81049,#81050,#81051,#81052,#81053,#81054,#81055,#81056,#81057,#81058,#81059,
#81060,#81061,#81062,#81063,#81064,#81065,#81066,#81067,#81068,#81069,#81070,
#81071,#81072,#81073,#81074,#81075,#81076,#81077,#81078,#81079,#81080,#81081,
#81082,#81083,#81084,#81085,#81086,#81087,#81088,#81089,#81090,#81091,#81092,
#81093,#81094,#81095,#81096,#81097,#81098,#81099,#81100,#81101,#81102,#81103,
#81104,#81105,#81106,#81107,#81108,#81109,#81110,#81111,#81112,#81113,#81114,
#81115,#81116,#81117,#81118,#81119,#81120,#81121,#81122,#81123,#81124,#81125,
#81126,#81127,#81128,#81129,#81130,#81131,#81132,#81133,#81134,#81135,#81136,
#81137,#81138,#81139,#81140,#81141,#81142,#81143,#81144,#81145,#81146,#81147,
#81148,#81149,#81150,#81151,#81152,#81153,#81154,#81155,#81156,#81157,#81158,
#81159,#81160,#81161,#81162,#81163,#81164,#81165),.UNSPECIFIED.,.F.,.F.,
(4,2,2,2,2,2,2,2,2,2,2,2,2,2,2,2,2,2,2,2,2,2,2,2,2,2,2,2,2,2,2,2,2,2,2,
2,2,2,2,2,2,2,2,2,2,2,2,2,2,2,2,2,2,2,2,2,2,2,2,2,2,2,2,2,2,2,2,2,2,2,2,
2,2,2,2,2,2,2,2,2,2,2,4),(-3.00705510852159,-2.99066778701684,-2.97535706723338,
-2.96828011428466,-2.96227735705098,-2.95820333716234,-2.9540589908238,
-2.9476677608138,-2.92440443875771,-2.90605684392387,-2.90199760030823,
-2.89959460569648,-2.89749579459065,-2.893812614373,-2.87538609653752,-2.85857897514339,
-2.85115740883379,-2.84494223005598,-2.84082979221944,-2.83672630758988,
-2.83056066040117,-2.80495584792262,-2.79320589740186,-2.78824406211796,
-2.78431261076756,-2.7819355940785,-2.77951792592766,-2.77538828798524,
-2.75504082516254,-2.74003446454397,-2.73303124844353,-2.727074172347,-2.72300772256983,
-2.71885246721819,-2.71240459472735,-2.69054132386259,-2.67067293183992,
-2.66673775545666,-2.66435999039269,-2.66194316037602,-2.65781774004939,
-2.63734685283338,-2.61547407786365,-2.60950158177183,-2.60543244923887,
-2.60128067696156,-2.59485153613769,-2.57229696340073,-2.55884039432496,
-2.55349409043209,-2.54934006442613,-2.54691740584065,-2.54454476056624,
-2.540635024459,-2.51789603891595,-2.49890838366919,-2.49244803036325,-2.48829042305874,
-2.48427283417218,-2.47836517267547,-2.45081600945923,-2.43997171718694,
-2.43523173627998,-2.4314315041655,-2.42908066210213,-2.42663059159411,
-2.42234272789024,-2.40333497306155,-2.38765371948162,-2.38048792560325,
-2.37442983460341,-2.3703454847996,-2.36621179171921,-2.35988125592821,
-2.33581952172769,-2.31772508169142,-2.31388477411611,-2.31152598528055,
-2.30908621145489,-2.30484908733473,-2.28666045454533,-2.27038572531952,
-2.26522078838353),.UNSPECIFIED.);
#1406=B_SPLINE_CURVE_WITH_KNOTS('',3,(#81171,#81172,#81173,#81174,#81175,
#81176,#81177,#81178,#81179,#81180,#81181,#81182,#81183,#81184,#81185,#81186,
#81187,#81188,#81189,#81190,#81191,#81192,#81193,#81194,#81195,#81196,#81197,
#81198,#81199,#81200,#81201,#81202,#81203,#81204,#81205,#81206,#81207,#81208,
#81209,#81210,#81211,#81212,#81213,#81214,#81215,#81216,#81217,#81218,#81219,
#81220,#81221,#81222,#81223,#81224,#81225,#81226,#81227,#81228,#81229,#81230,
#81231,#81232,#81233,#81234,#81235,#81236,#81237,#81238,#81239,#81240,#81241,
#81242,#81243,#81244,#81245,#81246,#81247,#81248,#81249,#81250,#81251,#81252,
#81253,#81254,#81255,#81256,#81257,#81258,#81259,#81260,#81261,#81262,#81263,
#81264,#81265,#81266,#81267,#81268,#81269,#81270,#81271,#81272,#81273,#81274,
#81275,#81276,#81277,#81278,#81279,#81280,#81281,#81282,#81283,#81284,#81285,
#81286,#81287,#81288,#81289,#81290,#81291,#81292,#81293,#81294,#81295,#81296,
#81297,#81298,#81299,#81300,#81301,#81302,#81303,#81304,#81305,#81306,#81307,
#81308,#81309,#81310,#81311,#81312,#81313,#81314,#81315,#81316,#81317,#81318,
#81319,#81320),.UNSPECIFIED.,.F.,.F.,(4,2,2,2,2,2,2,2,2,2,2,2,2,2,2,2,2,
2,2,2,2,2,2,2,2,2,2,2,2,2,2,2,2,2,2,2,2,2,2,2,2,2,2,2,2,2,2,2,2,2,2,2,2,
2,2,2,2,2,2,2,2,2,2,2,2,2,2,2,2,2,2,2,2,2,4),(-0.702969042438947,-0.701710412156898,
-0.699304623373738,-0.696946789994431,-0.693063925851947,-0.675881103467728,
-0.650796750698558,-0.644587498125185,-0.640494108134618,-0.636422922864456,
-0.630336176978641,-0.60886710145751,-0.58820624356317,-0.584098319843403,
-0.581694293400333,-0.579334819354786,-0.575444035329181,-0.557324263373413,
-0.533436234334152,-0.527108439139577,-0.522993158497826,-0.518941020346384,
-0.512961586389197,-0.491995501255123,-0.470471222025247,-0.466433132016482,
-0.464043431903924,-0.461670750216529,-0.457715418868478,-0.443561735531553,
-0.415153030706521,-0.409143632244394,-0.405491093668681,-0.401458881544609,
-0.395593521140241,-0.374220510307328,-0.352888789319575,-0.348831777321994,
-0.346438183941091,-0.344069178654129,-0.340131772873462,-0.322381201113179,
-0.298148375546142,-0.291850957097087,-0.287741225879504,-0.283684262644293,
-0.277677933974262,-0.256200256198579,-0.235353036769286,-0.231255926029211,
-0.228854042713106,-0.226492452653876,-0.22259162930125,-0.204814033399233,
-0.18052728933845,-0.174234695293368,-0.17012577339749,-0.166067910415485,
-0.160056974156436,-0.138653700615305,-0.117730904718132,-0.113638918266303,
-0.111238046138738,-0.108875434001243,-0.104969789486363,-0.100045096670016,
-0.0884202357153979,-0.0625486134681136,-0.0564319505365755,-0.0523550865526347,
-0.048266814175015,-0.0420873623547596,-0.0347113065829079,-0.0181409958602746,
-1.00000007552392E-6),.UNSPECIFIED.);
#1407=B_SPLINE_CURVE_WITH_KNOTS('',3,(#81321,#81322,#81323,#81324,#81325,
#81326,#81327,#81328,#81329,#81330,#81331,#81332,#81333,#81334,#81335,#81336,
#81337,#81338),.UNSPECIFIED.,.F.,.F.,(4,2,2,2,2,2,2,2,4),(-2.1117112384367,
-2.10803374113042,-2.10593836275868,-2.10373839514592,-2.10054077715998,
-2.09188679008812,-2.08281374733337,-2.07698764942234,-2.07270848450232),
 .UNSPECIFIED.);
#1408=B_SPLINE_CURVE_WITH_KNOTS('',3,(#81339,#81340,#81341,#81342,#81343,
#81344,#81345,#81346,#81347,#81348,#81349,#81350,#81351,#81352,#81353,#81354,
#81355,#81356,#81357,#81358,#81359,#81360,#81361,#81362,#81363,#81364,#81365,
#81366,#81367,#81368,#81369,#81370,#81371,#81372,#81373,#81374,#81375,#81376,
#81377,#81378,#81379,#81380,#81381,#81382,#81383,#81384,#81385,#81386,#81387,
#81388,#81389,#81390,#81391,#81392,#81393,#81394,#81395,#81396,#81397,#81398,
#81399,#81400,#81401,#81402,#81403,#81404,#81405,#81406,#81407,#81408,#81409,
#81410,#81411,#81412,#81413,#81414,#81415,#81416,#81417,#81418,#81419,#81420,
#81421,#81422,#81423,#81424,#81425,#81426,#81427,#81428,#81429,#81430,#81431,
#81432,#81433,#81434,#81435,#81436,#81437,#81438,#81439,#81440,#81441,#81442,
#81443,#81444,#81445,#81446,#81447,#81448,#81449,#81450,#81451,#81452,#81453,
#81454,#81455,#81456,#81457,#81458,#81459,#81460,#81461,#81462,#81463,#81464,
#81465,#81466,#81467,#81468,#81469,#81470,#81471,#81472,#81473,#81474,#81475,
#81476,#81477,#81478,#81479,#81480,#81481,#81482,#81483,#81484,#81485,#81486,
#81487,#81488,#81489,#81490,#81491,#81492,#81493,#81494,#81495,#81496,#81497,
#81498,#81499,#81500,#81501,#81502),.UNSPECIFIED.,.F.,.F.,(4,2,2,2,2,2,
2,2,2,2,2,2,2,2,2,2,2,2,2,2,2,2,2,2,2,2,2,2,2,2,2,2,2,2,2,2,2,2,2,2,2,2,
2,2,2,2,2,2,2,2,2,2,2,2,2,2,2,2,2,2,2,2,2,2,2,2,2,2,2,2,2,2,2,2,2,2,2,2,
2,2,2,4),(-2.26522078838353,-2.26308259399794,-2.25693981258274,-2.25284023844681,
-2.24872310822732,-2.24248348732369,-2.21750899752247,-2.20543732093632,
-2.20039952742394,-2.1964235329202,-2.19403734234458,-2.19162935858353,
-2.18754755221769,-2.16640898644128,-2.14528568850764,-2.13923643914338,
-2.13515356477946,-2.13101788062724,-2.12467702396361,-2.09653581488787,
-2.08206501963415,-2.07846030043459,-2.07616926507124,-2.07366955470286,
-2.06913589658524,-2.06310929138984,-2.04607122842413,-2.02841709108233,
-2.02201797082035,-2.01787146061176,-2.01379734268439,-2.00779834596808,
-1.98670039739742,-1.96536878402952,-1.96130208973809,-1.95889716275352,
-1.9565078201508,-1.95251701460299,-1.93475222207607,-1.91066124033276,
-1.90433542056805,-1.90020236482691,-1.89611681467631,-1.89005348759323,
-1.87021973428132,-1.84747068003657,-1.84355865588313,-1.84118535254758,
-1.83876269661744,-1.83460999337062,-1.8140591977983,-1.79330225303937,
-1.78685491281584,-1.78269934330518,-1.7786320627314,-1.77267286688305,
-1.75185578865277,-1.73006736381159,-1.72604729590666,-1.72365191112282,
-1.72125300185075,-1.71721599286741,-1.70024448108599,-1.67525693782621,
-1.66902112061544,-1.66490444095437,-1.66080373410641,-1.65465621681128,
-1.64734474690047,-1.63103832060014,-1.61286868402723,-1.60862889674959,
-1.60618844063525,-1.60382972574878,-1.5999907989241,-1.581928508261,-1.55784573596996,
-1.55151885739459,-1.54738549450721,-1.54329992039968,-1.53723709969949,
-1.52324866675719),.UNSPECIFIED.);
#1409=B_SPLINE_CURVE_WITH_KNOTS('',3,(#81507,#81508,#81509,#81510,#81511,
#81512,#81513,#81514,#81515,#81516,#81517,#81518,#81519,#81520,#81521,#81522,
#81523,#81524,#81525,#81526,#81527,#81528,#81529,#81530,#81531,#81532,#81533,
#81534,#81535,#81536,#81537,#81538,#81539,#81540,#81541,#81542,#81543,#81544,
#81545,#81546,#81547,#81548,#81549,#81550,#81551,#81552,#81553,#81554,#81555,
#81556,#81557,#81558,#81559,#81560,#81561,#81562,#81563,#81564,#81565,#81566,
#81567,#81568,#81569,#81570,#81571,#81572,#81573,#81574,#81575,#81576,#81577,
#81578,#81579,#81580,#81581,#81582,#81583,#81584,#81585,#81586,#81587,#81588,
#81589,#81590,#81591,#81592,#81593,#81594,#81595,#81596,#81597,#81598,#81599,
#81600,#81601,#81602,#81603,#81604,#81605,#81606,#81607,#81608,#81609,#81610,
#81611,#81612,#81613,#81614,#81615,#81616,#81617,#81618,#81619,#81620,#81621,
#81622,#81623,#81624,#81625,#81626,#81627,#81628,#81629,#81630,#81631,#81632,
#81633,#81634,#81635,#81636,#81637,#81638,#81639,#81640,#81641,#81642,#81643,
#81644,#81645,#81646,#81647,#81648,#81649,#81650,#81651,#81652,#81653,#81654,
#81655,#81656,#81657,#81658,#81659,#81660,#81661,#81662,#81663,#81664,#81665,
#81666,#81667,#81668,#81669,#81670),.UNSPECIFIED.,.F.,.F.,(4,2,2,2,2,2,
2,2,2,2,2,2,2,2,2,2,2,2,2,2,2,2,2,2,2,2,2,2,2,2,2,2,2,2,2,2,2,2,2,2,2,2,
2,2,2,2,2,2,2,2,2,2,2,2,2,2,2,2,2,2,2,2,2,2,2,2,2,2,2,2,2,2,2,2,2,2,2,2,
2,2,2,4),(-1.44487526904064,-1.43062984737927,-1.41166932931502,-1.40738566975182,
-1.40494593260971,-1.40261535681389,-1.39886860241393,-1.38034851879148,
-1.35661436093033,-1.35027508300439,-1.34615806805642,-1.34210834452718,
-1.33614034048275,-1.31407616250411,-1.29378691300726,-1.28966528623936,
-1.28725860501692,-1.28490189182519,-1.28102395582219,-1.27614599694567,
-1.26471335572167,-1.23845100779924,-1.23238592469723,-1.22872469179893,
-1.224701890561,-1.21888964878338,-1.21210482210727,-1.19792500750346,-1.17595889299071,
-1.1719687088649,-1.16958908958452,-1.16720714548371,-1.16320585665983,
-1.15811723983238,-1.14579098721926,-1.12130193050571,-1.11503026308992,
-1.11092564053181,-1.10686519674277,-1.10083722408066,-1.09370686577349,
-1.07813340894207,-1.05882589996639,-1.05459191763482,-1.05216222693181,
-1.04982406904773,-1.04603904753365,-1.02759080370476,-1.00385776998816,
-0.997518042517896,-0.993400815502081,-0.989350940765807,-0.983382823305888,
-0.961874524430739,-0.940974418390339,-0.936881568598389,-0.934480732566327,
-0.932118705269316,-0.928214880816489,-0.923293047667827,-0.911678893979217,
-0.885792076631254,-0.879678596145071,-0.876009379186951,-0.871993660070933,
-0.86622411731811,-0.844011970483475,-0.823407319914528,-0.81929679327984,
-0.816892282487142,-0.814533376066198,-0.810645143388851,-0.791982867570228,
-0.768730887866824,-0.762356001231897,-0.758232079599996,-0.754187146462191,
-0.748248162228047,-0.741261224667227,-0.726281828059949,-0.705827098954992,
-0.702969042438947),.UNSPECIFIED.);
#1410=B_SPLINE_CURVE_WITH_KNOTS('',3,(#81671,#81672,#81673,#81674,#81675,
#81676,#81677,#81678,#81679,#81680,#81681,#81682,#81683,#81684,#81685,#81686,
#81687,#81688,#81689,#81690,#81691,#81692,#81693,#81694,#81695,#81696,#81697,
#81698,#81699,#81700,#81701,#81702,#81703,#81704,#81705,#81706,#81707,#81708,
#81709,#81710,#81711,#81712,#81713,#81714,#81715,#81716,#81717,#81718,#81719,
#81720,#81721,#81722,#81723,#81724,#81725,#81726,#81727,#81728,#81729,#81730,
#81731,#81732,#81733,#81734,#81735,#81736,#81737,#81738,#81739,#81740,#81741,
#81742,#81743,#81744,#81745,#81746,#81747,#81748,#81749,#81750,#81751,#81752,
#81753,#81754,#81755,#81756,#81757,#81758,#81759,#81760,#81761,#81762,#81763,
#81764,#81765,#81766,#81767,#81768,#81769,#81770,#81771,#81772,#81773,#81774,
#81775,#81776,#81777,#81778,#81779,#81780,#81781,#81782,#81783,#81784,#81785,
#81786,#81787,#81788,#81789,#81790,#81791,#81792,#81793,#81794,#81795,#81796,
#81797,#81798,#81799,#81800,#81801,#81802,#81803,#81804,#81805,#81806,#81807,
#81808,#81809,#81810,#81811,#81812,#81813,#81814,#81815,#81816,#81817,#81818,
#81819,#81820,#81821,#81822,#81823,#81824,#81825,#81826,#81827,#81828,#81829,
#81830,#81831,#81832,#81833,#81834,#81835,#81836,#81837,#81838,#81839,#81840),
 .UNSPECIFIED.,.F.,.F.,(4,2,2,2,2,2,2,2,2,2,2,2,2,2,2,2,2,2,2,2,2,2,2,2,
2,2,2,2,2,2,2,2,2,2,2,2,2,2,2,2,2,2,2,2,2,2,2,2,2,2,2,2,2,2,2,2,2,2,2,2,
2,2,2,2,2,2,2,2,2,2,2,2,2,2,2,2,2,2,2,2,2,2,2,2,4),(-1.52324866675719,-1.52033948694185,
-1.49491652761532,-1.49086149540555,-1.48845884410359,-1.48606693510808,
-1.48206423426943,-1.464576274536,-1.44016478020395,-1.43386843330214,-1.42974055809692,
-1.42564983927897,-1.4195587965746,-1.39891350013134,-1.37726247730706,
-1.37322738445059,-1.3708288110181,-1.36843281177055,-1.36441037142123,
-1.34646534694613,-1.3226601758809,-1.31630893348182,-1.31217090829117,
-1.30808887530338,-1.30204703954764,-1.28028628276023,-1.2598149297332,
-1.25568711508309,-1.2532694336227,-1.2508912980067,-1.24695636826099,-1.24198963825706,
-1.23021989051971,-1.20466919832499,-1.19849760428866,-1.19439229965558,
-1.19027961413292,-1.18406736747959,-1.17665043516656,-1.15987311712153,
-1.14271501280928,-1.13830323226994,-1.13582773944788,-1.13349360265352,
-1.12978172171059,-1.11115855411566,-1.08744806506716,-1.08108884163973,
-1.07694922259553,-1.07286822135788,-1.06683292266412,-1.05970369631855,
-1.0441831043046,-1.0247689918805,-1.02054565334965,-1.01810838082529,-1.01574667637118,
-1.01189359919665,-1.00706569330692,-0.995869645306252,-0.969116546126487,
-0.963099356335427,-0.959428488351477,-0.955363899608925,-0.949422276953992,
-0.942443702819668,-0.92754338698631,-0.906973265529007,-0.902849440832177,
-0.900432550286804,-0.898053627391007,-0.894114959012901,-0.889141887826747,
-0.877345590066338,-0.851847482107216,-0.845669416357442,-0.841562888099976,
-0.837451298463795,-0.831245387628963,-0.823838877088501,-0.807109187457589,
-0.789873717327814,-0.785464752593549,-0.782989798471485,-0.781189504183713),
 .UNSPECIFIED.);
#1411=B_SPLINE_CURVE_WITH_KNOTS('',3,(#81845,#81846,#81847,#81848,#81849,
#81850,#81851,#81852,#81853,#81854,#81855,#81856,#81857,#81858,#81859,#81860,
#81861,#81862,#81863,#81864,#81865,#81866,#81867,#81868,#81869,#81870,#81871,
#81872,#81873,#81874,#81875,#81876,#81877,#81878,#81879,#81880,#81881,#81882,
#81883,#81884,#81885,#81886,#81887,#81888,#81889,#81890,#81891,#81892,#81893,
#81894,#81895,#81896,#81897,#81898,#81899,#81900,#81901,#81902,#81903,#81904,
#81905,#81906,#81907,#81908,#81909,#81910,#81911,#81912,#81913,#81914,#81915,
#81916,#81917,#81918,#81919,#81920,#81921,#81922,#81923,#81924,#81925,#81926,
#81927,#81928,#81929,#81930,#81931,#81932,#81933,#81934,#81935,#81936,#81937,
#81938,#81939,#81940,#81941,#81942,#81943,#81944,#81945,#81946,#81947,#81948,
#81949,#81950,#81951,#81952,#81953,#81954,#81955,#81956,#81957,#81958,#81959,
#81960,#81961,#81962,#81963,#81964,#81965,#81966,#81967,#81968,#81969,#81970,
#81971,#81972,#81973,#81974,#81975,#81976,#81977,#81978,#81979,#81980,#81981,
#81982,#81983,#81984,#81985,#81986,#81987,#81988,#81989,#81990,#81991,#81992,
#81993,#81994,#81995,#81996,#81997,#81998,#81999,#82000,#82001,#82002,#82003,
#82004,#82005,#82006,#82007,#82008,#82009,#82010,#82011,#82012,#82013,#82014,
#82015,#82016,#82017,#82018,#82019,#82020),.UNSPECIFIED.,.F.,.F.,(4,2,2,
2,2,2,2,2,2,2,2,2,2,2,2,2,2,2,2,2,2,2,2,2,2,2,2,2,2,2,2,2,2,2,2,2,2,2,2,
2,2,2,2,2,2,2,2,2,2,2,2,2,2,2,2,2,2,2,2,2,2,2,2,2,2,2,2,2,2,2,2,2,2,2,2,
2,2,2,2,2,2,2,2,2,2,2,2,4),(-2.18666954650822,-2.18265430661059,-2.17468325395502,
-2.1702613950192,-2.16634123326651,-2.16132410480541,-2.15020514347348,
-2.14447159053473,-2.12444638312029,-2.11796898048221,-2.1132001078031,
-2.11066396280014,-2.10838765255901,-2.10493605848464,-2.09267281405792,
-2.07197258198025,-2.05955812829991,-2.0543982159289,-2.0504608443663,-2.04611481916996,
-2.03855579425183,-2.02444249740545,-1.99920150751317,-1.99512526147699,
-1.99272810294192,-1.99036352894282,-1.98644589225988,-1.98150026422559,
-1.96978503799143,-1.94411305634687,-1.93797456013878,-1.933894650906,-1.92981200322807,
-1.92365851057852,-1.90544749943925,-1.88345742636239,-1.87830264824371,
-1.87569276320194,-1.87344170959043,-1.87015480057966,-1.85999980296953,
-1.83600964276,-1.82414778657502,-1.81908582455218,-1.81516018202226,-1.81076274478065,
-1.8029276613258,-1.77430265071792,-1.77195557261618,-1.76247473502744,
-1.75918039220243,-1.75692824579638,-1.75432182041591,-1.74918606042188,
-1.74199495318082,-1.71567166662637,-1.70559280344456,-1.7008144805518,
-1.69691602218718,-1.69226136869109,-1.68295731706708,-1.66957680557475,
-1.64636771777372,-1.6423400942397,-1.6399528415437,-1.63757868581714,-1.63361475909319,
-1.61704110497047,-1.59135934274745,-1.58522148386188,-1.58114151147117,
-1.57705843394237,-1.57090355729544,-1.55053878980004,-1.52874292237262,
-1.52473443215855,-1.52235110593306,-1.51997306880478,-1.51599037480901,
-1.51093363831038,-1.4987455538975,-1.47399873796849,-1.46775386383331,
-1.46365430058627,-1.45958971446674,-1.45353777798196,-1.44636855480763,
-1.44487526904064),.UNSPECIFIED.);
#1412=B_SPLINE_CURVE_WITH_KNOTS('',3,(#82021,#82022,#82023,#82024,#82025,
#82026,#82027,#82028,#82029,#82030,#82031,#82032,#82033,#82034,#82035,#82036,
#82037,#82038,#82039,#82040,#82041,#82042,#82043,#82044,#82045,#82046,#82047,
#82048,#82049,#82050,#82051,#82052,#82053,#82054,#82055,#82056,#82057,#82058,
#82059,#82060,#82061,#82062,#82063,#82064,#82065,#82066,#82067,#82068,#82069,
#82070,#82071,#82072,#82073,#82074,#82075,#82076,#82077,#82078,#82079,#82080,
#82081,#82082,#82083,#82084,#82085,#82086,#82087,#82088,#82089,#82090,#82091,
#82092,#82093,#82094,#82095,#82096,#82097,#82098,#82099,#82100,#82101,#82102,
#82103,#82104,#82105,#82106,#82107,#82108,#82109,#82110,#82111,#82112,#82113,
#82114,#82115,#82116,#82117,#82118,#82119,#82120,#82121,#82122,#82123,#82124,
#82125,#82126,#82127,#82128,#82129,#82130,#82131,#82132,#82133,#82134,#82135,
#82136,#82137,#82138,#82139,#82140,#82141,#82142,#82143,#82144,#82145,#82146,
#82147,#82148,#82149,#82150,#82151,#82152,#82153,#82154,#82155,#82156,#82157,
#82158,#82159,#82160,#82161,#82162,#82163,#82164,#82165,#82166,#82167,#82168,
#82169,#82170,#82171,#82172,#82173,#82174,#82175,#82176,#82177,#82178,#82179,
#82180,#82181,#82182,#82183,#82184,#82185,#82186,#82187,#82188,#82189,#82190),
 .UNSPECIFIED.,.F.,.F.,(4,2,2,2,2,2,2,2,2,2,2,2,2,2,2,2,2,2,2,2,2,2,2,2,
2,2,2,2,2,2,2,2,2,2,2,2,2,2,2,2,2,2,2,2,2,2,2,2,2,2,2,2,2,2,2,2,2,2,2,2,
2,2,2,2,2,2,2,2,2,2,2,2,2,2,2,2,2,2,2,2,2,2,2,2,4),(-0.781189504183713,
-0.780655240613857,-0.776941305076245,-0.772346214995282,-0.762066513925456,
-0.733221143074392,-0.727502757707771,-0.723515724568544,-0.719307952888275,
-0.712583482918676,-0.704309153500262,-0.683011120065911,-0.670596162685293,
-0.667063335226089,-0.664784680501353,-0.662259524594123,-0.657598599701539,
-0.651336361507989,-0.63283805493482,-0.615360290646342,-0.609755522501097,
-0.605746772659503,-0.601494157462634,-0.594531425340019,-0.571028994014777,
-0.554561149728483,-0.55020148730562,-0.547736514630781,-0.545395355475079,
-0.541646881678502,-0.536994339466273,-0.52649342671482,-0.498172460105221,
-0.492377186122633,-0.488377701902321,-0.484190979180804,-0.477578411693701,
-0.469494672792845,-0.449330386791692,-0.435490534037347,-0.431901374537632,
-0.429612920216069,-0.427107573766107,-0.422546551843302,-0.416469818003131,
-0.399134176424358,-0.381844159685263,-0.375456601816089,-0.371311887830329,
-0.367235452957319,-0.361225258681097,-0.354136395734053,-0.338783707851385,
-0.319007134063997,-0.314840540477088,-0.312414950353729,-0.310043825312622,
-0.306143347690164,-0.288820184287301,-0.263951657589763,-0.257702282803172,
-0.253582946323682,-0.249484256515147,-0.243348992444438,-0.236057639434028,
-0.219840712904032,-0.201532657939523,-0.197292273574692,-0.194851596625662,
-0.192492786310851,-0.188653884258802,-0.170597841935886,-0.146503855945698,
-0.140177451709205,-0.136043989488405,-0.131958019614313,-0.125894034856154,
-0.104317490247526,-0.0836976283859776,-0.0795762443453795,-0.0771598789088768,
-0.0747805548886755,-0.0708397932613529,-0.0542443252368777,-0.0391649357543273),
 .UNSPECIFIED.);
#1413=B_SPLINE_CURVE_WITH_KNOTS('',3,(#82195,#82196,#82197,#82198,#82199,
#82200,#82201,#82202,#82203,#82204,#82205,#82206,#82207,#82208,#82209,#82210,
#82211,#82212,#82213,#82214,#82215,#82216,#82217,#82218,#82219,#82220,#82221,
#82222,#82223,#82224,#82225,#82226,#82227,#82228,#82229,#82230,#82231,#82232,
#82233,#82234,#82235,#82236,#82237,#82238,#82239,#82240,#82241,#82242,#82243,
#82244,#82245,#82246,#82247,#82248,#82249,#82250,#82251,#82252,#82253,#82254,
#82255,#82256,#82257,#82258,#82259,#82260,#82261,#82262,#82263,#82264,#82265,
#82266,#82267,#82268,#82269,#82270,#82271,#82272,#82273,#82274,#82275,#82276,
#82277,#82278,#82279,#82280,#82281,#82282,#82283,#82284,#82285,#82286,#82287,
#82288,#82289,#82290,#82291,#82292,#82293,#82294,#82295,#82296,#82297,#82298,
#82299,#82300,#82301,#82302,#82303,#82304,#82305,#82306,#82307,#82308,#82309,
#82310,#82311,#82312,#82313,#82314,#82315,#82316,#82317,#82318,#82319,#82320,
#82321,#82322,#82323,#82324,#82325,#82326,#82327,#82328,#82329,#82330,#82331,
#82332,#82333,#82334,#82335,#82336,#82337,#82338,#82339,#82340,#82341,#82342,
#82343,#82344,#82345,#82346,#82347,#82348,#82349,#82350,#82351,#82352,#82353,
#82354,#82355,#82356,#82357,#82358,#82359,#82360,#82361,#82362),
 .UNSPECIFIED.,.F.,.F.,(4,2,2,2,2,2,2,2,2,2,2,2,2,2,2,2,2,2,2,2,2,2,2,2,
2,2,2,2,2,2,2,2,2,2,2,2,2,2,2,2,2,2,2,2,2,2,2,2,2,2,2,2,2,2,2,2,2,2,2,2,
2,2,2,2,2,2,2,2,2,2,2,2,2,2,2,2,2,2,2,2,2,2,2,4),(-2.92834915174502,-2.92648539545499,
-2.90657057780971,-2.88440378746991,-2.87834464423708,-2.87427953806933,
-2.87018271217011,-2.86394878545922,-2.83909422789314,-2.82695520076427,
-2.82190997785814,-2.81793460290906,-2.81555847767098,-2.81317439141761,
-2.80916037975621,-2.78745591004364,-2.76686983205887,-2.76080249131816,
-2.75673596941759,-2.75264085626061,-2.74641599461634,-2.72147563514041,
-2.70444372036,-2.70041885332621,-2.69803253890805,-2.69565860262891,-2.69169391475909,
-2.66953917970941,-2.65547278015069,-2.64871870517574,-2.64292574917221,
-2.63890705093035,-2.63524358385147,-2.62916052005398,-2.60303018211162,
-2.59152658888631,-2.58663165037125,-2.58274430789586,-2.58038614041258,
-2.5779824849785,-2.57387378004309,-2.55329554679192,-2.53114252347342,
-2.52535505457331,-2.52133725612151,-2.51767274506948,-2.51158340607721,
-2.48550217216042,-2.47397517831889,-2.46907458387598,-2.46518390366944,
-2.46282504496422,-2.46042215164099,-2.45631714677906,-2.43566536328569,
-2.42082590755425,-2.41387522508392,-2.40795885290461,-2.40391883798699,
-2.39979155408719,-2.39339369901535,-2.37054695202645,-2.35125846276003,
-2.34750404798006,-2.34517231985751,-2.34273531303893,-2.33846368736868,
-2.32355460516355,-2.31000987357397,-2.29985826215516,-2.29210107993466,
-2.28771846644346,-2.28379029529415,-2.27870285381457,-2.26662145045314,
-2.26299184174589,-2.24220586632793,-2.23562527315064,-2.23080228818918,
-2.22825562140187,-2.22600963290834,-2.22260711010118,-2.21177168803733,
-2.18666954650822),.UNSPECIFIED.);
#1414=B_SPLINE_CURVE_WITH_KNOTS('',3,(#82364,#82365,#82366,#82367,#82368,
#82369,#82370,#82371,#82372,#82373,#82374,#82375,#82376,#82377),
 .UNSPECIFIED.,.F.,.F.,(4,2,2,2,2,2,4),(-0.0391649357543273,-0.028591756921446,
-0.0224048677175574,-0.0182968878252835,-0.014597475923147,-0.0105493853881568,
-1.00000004773365E-6),.UNSPECIFIED.);
#1415=B_SPLINE_CURVE_WITH_KNOTS('',3,(#82378,#82379,#82380,#82381,#82382,
#82383,#82384,#82385,#82386,#82387,#82388,#82389,#82390,#82391,#82392,#82393,
#82394,#82395,#82396,#82397,#82398,#82399,#82400,#82401,#82402,#82403,#82404,
#82405,#82406,#82407,#82408,#82409,#82410,#82411,#82412,#82413,#82414,#82415,
#82416,#82417,#82418,#82419,#82420,#82421,#82422,#82423,#82424,#82425,#82426,
#82427,#82428,#82429,#82430,#82431,#82432,#82433,#82434,#82435,#82436,#82437,
#82438,#82439,#82440,#82441,#82442,#82443,#82444,#82445,#82446,#82447,#82448,
#82449,#82450,#82451,#82452,#82453,#82454,#82455,#82456,#82457,#82458,#82459,
#82460,#82461,#82462,#82463,#82464,#82465,#82466,#82467,#82468,#82469,#82470,
#82471,#82472,#82473,#82474,#82475,#82476,#82477,#82478,#82479,#82480,#82481,
#82482,#82483,#82484,#82485,#82486,#82487,#82488,#82489,#82490,#82491,#82492,
#82493,#82494,#82495,#82496,#82497,#82498,#82499,#82500,#82501,#82502,#82503,
#82504,#82505,#82506,#82507,#82508,#82509,#82510,#82511,#82512,#82513,#82514,
#82515,#82516,#82517,#82518,#82519,#82520,#82521,#82522,#82523,#82524,#82525,
#82526,#82527,#82528,#82529,#82530,#82531,#82532,#82533,#82534,#82535,#82536,
#82537,#82538,#82539),.UNSPECIFIED.,.F.,.F.,(4,2,2,2,2,2,2,2,2,2,2,2,2,
2,2,2,2,2,2,2,2,2,2,2,2,2,2,2,2,2,2,2,2,2,2,2,2,2,2,2,2,2,2,2,2,2,2,2,2,
2,2,2,2,2,2,2,2,2,2,2,2,2,2,2,2,2,2,2,2,2,2,2,2,2,2,2,2,2,2,2,4),(-2.14624791579464,
-2.11682697548836,-2.11191450843237,-2.10801217294024,-2.10564120580342,
-2.10321708034896,-2.09905535929736,-2.07928053471196,-2.05878385807118,
-2.05182022040338,-2.04756841143487,-2.04356121279034,-2.0379600049088,
-2.02061003096647,-2.001997857921,-1.99571792954008,-1.99104833667306,-1.98852199165158,
-1.98624496507717,-1.98271872719268,-1.97035451983186,-1.94903929875685,
-1.94076551026284,-1.93404135305729,-1.92983454252486,-1.92584884944796,
-1.92013323004753,-1.89126559413484,-1.88098907506257,-1.87639513136064,
-1.87268248936122,-1.87034867987337,-1.8678743549837,-1.86346634259697,
-1.8462841980142,-1.82954674218639,-1.8221404544652,-1.81593460737231,-1.81182386836759,
-1.80771874310254,-1.80154399454501,-1.77601191669446,-1.7642245860807,
-1.75925383792374,-1.75531715352806,-1.75293909285403,-1.75052261720979,
-1.74639889067038,-1.72588776350962,-1.70411878866479,-1.69811592715585,
-1.69404148523728,-1.68989640962819,-1.68350336256872,-1.66025901138639,
-1.64189400989191,-1.63783412083529,-1.6354307787598,-1.63333181093117,
-1.62964835604535,-1.61123777804337,-1.59441803341239,-1.58699348297927,
-1.58077639757357,-1.57666346996609,-1.57256008239933,-1.56639577500432,
-1.54077333289484,-1.52902954345837,-1.52406903556741,-1.52013830817635,
-1.51776137542678,-1.51534336024632,-1.5112125542358,-1.49089173662272,
-1.46855338366538,-1.46272685059151,-1.4586826412617,-1.45499297466204,
-1.4488554269585,-1.44355213348337),.UNSPECIFIED.);
#1416=B_SPLINE_CURVE_WITH_KNOTS('',3,(#82544,#82545,#82546,#82547,#82548,
#82549,#82550,#82551,#82552,#82553,#82554,#82555,#82556,#82557,#82558,#82559,
#82560,#82561,#82562,#82563,#82564,#82565,#82566,#82567,#82568,#82569,#82570,
#82571,#82572,#82573,#82574,#82575,#82576,#82577,#82578,#82579,#82580,#82581,
#82582,#82583,#82584,#82585,#82586,#82587,#82588,#82589,#82590,#82591,#82592,
#82593,#82594,#82595,#82596,#82597,#82598,#82599,#82600,#82601,#82602,#82603,
#82604,#82605,#82606,#82607,#82608,#82609,#82610,#82611,#82612,#82613,#82614,
#82615,#82616,#82617,#82618,#82619,#82620,#82621,#82622,#82623,#82624,#82625,
#82626,#82627,#82628,#82629,#82630,#82631,#82632,#82633,#82634,#82635,#82636,
#82637,#82638,#82639,#82640,#82641,#82642,#82643,#82644,#82645,#82646,#82647,
#82648,#82649,#82650,#82651,#82652,#82653,#82654,#82655,#82656,#82657,#82658,
#82659,#82660,#82661,#82662,#82663,#82664,#82665,#82666,#82667,#82668,#82669,
#82670,#82671,#82672,#82673,#82674,#82675,#82676,#82677,#82678,#82679,#82680,
#82681,#82682,#82683,#82684,#82685,#82686,#82687,#82688,#82689,#82690,#82691,
#82692,#82693,#82694,#82695,#82696,#82697,#82698,#82699,#82700,#82701,#82702,
#82703,#82704,#82705,#82706,#82707,#82708,#82709,#82710,#82711,#82712,#82713),
 .UNSPECIFIED.,.F.,.F.,(4,2,2,2,2,2,2,2,2,2,2,2,2,2,2,2,2,2,2,2,2,2,2,2,
2,2,2,2,2,2,2,2,2,2,2,2,2,2,2,2,2,2,2,2,2,2,2,2,2,2,2,2,2,2,2,2,2,2,2,2,
2,2,2,2,2,2,2,2,2,2,2,2,2,2,2,2,2,2,2,2,2,2,2,2,4),(-3.66997076696365,-3.66294180694855,
-3.64426115795585,-3.64050467059312,-3.63818112719387,-3.63575399153715,
-3.63152917797224,-3.612213653117,-3.59665330604222,-3.58952479255085,-3.58349585925373,
-3.57943245828912,-3.5753224675822,-3.56903605589188,-3.54480508468909,
-3.53239640017913,-3.52728865662214,-3.52327589590202,-3.52088882330274,
-3.51850752236118,-3.51451282651347,-3.49262660089069,-3.47843969843768,
-3.47165429679745,-3.46584137656891,-3.46181817679182,-3.45815644616426,
-3.45209017892872,-3.4258089356034,-3.41437171898407,-3.40949255675202,
-3.4056143842269,-3.40325796395558,-3.40085359489583,-3.39673715889808,
-3.37639514003859,-3.36137687286919,-3.35438339029674,-3.34844121742013,
-3.34439872436269,-3.34028110822169,-3.33392473282489,-3.31041384368027,
-3.29175818348476,-3.28797315464772,-3.28563649178251,-3.28320878672761,
-3.27898223096482,-3.25967453651895,-3.23676792931688,-3.23084402376541,
-3.22680248622695,-3.22267645110078,-3.21628629275609,-3.19332372429606,
-3.17471753181634,-3.17066722116852,-3.16827529780673,-3.16590587466695,
-3.16196356985642,-3.13961256319151,-3.11943373479543,-3.1134164099454,
-3.10935878072073,-3.10525356706946,-3.09897397222717,-3.07456046435438,
-3.05691482608817,-3.05299613987827,-3.05063168832136,-3.04823552090782,
-3.04416238790833,-3.02306482803221,-3.00148036166669,-2.99564343064258,
-2.99161758065946,-2.98796242830071,-2.98192893430487,-2.95542319602778,
-2.94409808144442,-2.93924667132723,-2.93538510583023,-2.93303231518504,
-2.93062283455467,-2.92834915174502),.UNSPECIFIED.);
#1417=B_SPLINE_CURVE_WITH_KNOTS('',3,(#82714,#82715,#82716,#82717,#82718,
#82719,#82720,#82721,#82722,#82723,#82724,#82725,#82726,#82727,#82728,#82729,
#82730,#82731,#82732,#82733,#82734,#82735,#82736,#82737,#82738,#82739,#82740,
#82741,#82742,#82743,#82744,#82745,#82746,#82747,#82748,#82749,#82750,#82751,
#82752,#82753,#82754,#82755,#82756,#82757,#82758,#82759,#82760,#82761,#82762,
#82763,#82764,#82765,#82766,#82767,#82768,#82769,#82770,#82771,#82772,#82773,
#82774,#82775,#82776,#82777,#82778,#82779,#82780,#82781,#82782,#82783,#82784,
#82785,#82786,#82787,#82788,#82789,#82790,#82791,#82792,#82793,#82794,#82795,
#82796,#82797,#82798,#82799,#82800,#82801,#82802,#82803,#82804,#82805,#82806,
#82807,#82808,#82809,#82810,#82811,#82812,#82813,#82814,#82815,#82816,#82817,
#82818,#82819,#82820,#82821,#82822,#82823,#82824,#82825,#82826,#82827,#82828,
#82829,#82830,#82831,#82832,#82833,#82834,#82835,#82836,#82837,#82838,#82839,
#82840,#82841,#82842,#82843,#82844,#82845,#82846,#82847,#82848,#82849,#82850,
#82851,#82852,#82853,#82854,#82855,#82856,#82857,#82858,#82859,#82860,#82861,
#82862,#82863,#82864,#82865,#82866,#82867),.UNSPECIFIED.,.F.,.F.,(4,2,2,
2,2,2,2,2,2,2,2,2,2,2,2,2,2,2,2,2,2,2,2,2,2,2,2,2,2,2,2,2,2,2,2,2,2,2,2,
2,2,2,2,2,2,2,2,2,2,2,2,2,2,2,2,2,2,2,2,2,2,2,2,2,2,2,2,2,2,2,2,2,2,2,2,
2,4),(-1.44355213348337,-1.42301543780805,-1.40655434363128,-1.40257766687356,
-1.40019134752506,-1.39778355717221,-1.39370257389229,-1.37255529451872,
-1.35153902219749,-1.34544338593644,-1.34135230270311,-1.33722610537493,
-1.33093665219751,-1.30643778848766,-1.29411604231323,-1.28902046629015,
-1.28501082378166,-1.28261775410596,-1.28021701256442,-1.27617031134857,
-1.25466502244134,-1.23393195372578,-1.22784136521807,-1.22375115021584,
-1.21962388911123,-1.21332880743686,-1.18888661429008,-1.17127249369206,
-1.16734094647008,-1.16496377779633,-1.16254573364486,-1.15841528914934,
-1.1380780290576,-1.11605602989744,-1.11009331423373,-1.10602556694194,
-1.10187100172189,-1.0954285010926,-1.07326504094764,-1.05434362231351,
-1.05004722443417,-1.04759531103085,-1.04524565591727,-1.04145175831556,
-1.02328210548449,-0.999225218586492,-0.992896463345815,-0.988763089298828,
-0.984678413869209,-0.978618734925012,-0.971449588671737,-0.955757844739731,
-0.936736786583105,-0.932446677685336,-0.929996119836072,-0.92764540003064,
-0.923846597217638,-0.905564985962089,-0.88165398141841,-0.875311969236898,
-0.871175831619516,-0.867092669699315,-0.861043370105454,-0.84033442210889,
-0.818657937267153,-0.814625936221056,-0.81222798593872,-0.809830686461947,
-0.805803478545767,-0.788459744445454,-0.763940411053372,-0.757656361673641,
-0.753530381495941,-0.749436906878411,-0.743332543829005,-0.721970195697778,
-0.701564423551126),.UNSPECIFIED.);
#1418=B_SPLINE_CURVE_WITH_KNOTS('',3,(#82870,#82871,#82872,#82873,#82874,
#82875,#82876,#82877,#82878,#82879,#82880,#82881,#82882,#82883,#82884,#82885,
#82886,#82887,#82888,#82889,#82890,#82891,#82892,#82893,#82894,#82895,#82896,
#82897,#82898,#82899,#82900,#82901,#82902,#82903,#82904,#82905,#82906,#82907,
#82908,#82909,#82910,#82911,#82912,#82913,#82914,#82915,#82916,#82917,#82918,
#82919,#82920,#82921,#82922,#82923,#82924,#82925,#82926,#82927,#82928,#82929,
#82930,#82931,#82932,#82933,#82934,#82935,#82936,#82937,#82938,#82939,#82940,
#82941,#82942,#82943,#82944,#82945,#82946,#82947,#82948,#82949,#82950,#82951,
#82952,#82953,#82954,#82955,#82956,#82957,#82958,#82959,#82960,#82961,#82962,
#82963,#82964,#82965,#82966,#82967,#82968,#82969,#82970,#82971,#82972,#82973,
#82974,#82975,#82976,#82977,#82978,#82979,#82980,#82981,#82982,#82983,#82984,
#82985,#82986,#82987,#82988,#82989,#82990,#82991,#82992,#82993,#82994,#82995,
#82996,#82997,#82998,#82999,#83000,#83001,#83002,#83003,#83004,#83005,#83006,
#83007,#83008,#83009,#83010,#83011,#83012,#83013,#83014,#83015,#83016,#83017,
#83018,#83019,#83020,#83021,#83022,#83023,#83024,#83025),.UNSPECIFIED.,
 .F.,.F.,(4,2,2,2,2,2,2,2,2,2,2,2,2,2,2,2,2,2,2,2,2,2,2,2,2,2,2,2,2,2,2,
2,2,2,2,2,2,2,2,2,2,2,2,2,2,2,2,2,2,2,2,2,2,2,2,2,2,2,2,2,2,2,2,2,2,2,2,
2,2,2,2,2,2,2,2,2,2,4),(-0.701564423551126,-0.70120887792929,-0.697095716149052,
-0.694681121607495,-0.692302216844747,-0.688358159211799,-0.671215668528298,
-0.646207462961748,-0.639973371958886,-0.635858658508875,-0.63176077592468,
-0.625619644994713,-0.618317381956628,-0.602047279863736,-0.583817118074423,
-0.57957988052083,-0.577140638947338,-0.574781543544154,-0.570941971037803,
-0.552883380963188,-0.528778706105412,-0.522450294566862,-0.518315221127886,
-0.51422732897638,-0.508159518769005,-0.486448779636048,-0.465998345568823,
-0.461868937046329,-0.459449672004075,-0.457064787709155,-0.453113098979084,
-0.435276881029289,-0.411288538973521,-0.4049621879785,-0.400824959155111,
-0.396731659601096,-0.39064872841958,-0.368705608078459,-0.348488244140866,
-0.344351519882306,-0.341932094030867,-0.339571230028095,-0.335678923917613,
-0.330778486760952,-0.319266448756615,-0.292994857381811,-0.286904445355541,
-0.283235428695515,-0.279209860939718,-0.273405467744888,-0.251123711630572,
-0.230683987863599,-0.226561196860336,-0.22415020383434,-0.221765645110252,
-0.217826991987676,-0.212859430033859,-0.201111108768999,-0.175443825837061,
-0.16925949427639,-0.165546772028951,-0.161479507727689,-0.155621091119772,
-0.148784180969686,-0.134471932177159,-0.112908310051021,-0.10885362024273,
-0.106437488582663,-0.10398511976884,-0.0998182124646509,-0.0860912770649259,
-0.0578102541858007,-0.0521234685116127,-0.0480733705491654,-0.0437859888948185,
-0.0367789174125886,-0.0191482594977915,-9.9999999203515E-7),
 .UNSPECIFIED.);
#1419=B_SPLINE_CURVE_WITH_KNOTS('',3,(#83028,#83029,#83030,#83031,#83032,
#83033,#83034,#83035,#83036,#83037,#83038,#83039,#83040,#83041,#83042,#83043,
#83044,#83045,#83046,#83047,#83048,#83049,#83050,#83051,#83052,#83053,#83054,
#83055,#83056,#83057,#83058,#83059,#83060,#83061,#83062,#83063,#83064,#83065,
#83066,#83067,#83068,#83069,#83070,#83071,#83072,#83073,#83074,#83075,#83076,
#83077,#83078,#83079,#83080,#83081,#83082,#83083,#83084,#83085,#83086,#83087,
#83088,#83089,#83090,#83091,#83092,#83093,#83094,#83095,#83096,#83097,#83098,
#83099,#83100,#83101,#83102,#83103,#83104,#83105,#83106,#83107,#83108,#83109,
#83110,#83111,#83112,#83113,#83114,#83115,#83116,#83117,#83118,#83119,#83120,
#83121,#83122,#83123,#83124,#83125,#83126,#83127,#83128,#83129,#83130,#83131,
#83132,#83133,#83134,#83135,#83136,#83137,#83138,#83139,#83140,#83141,#83142,
#83143,#83144,#83145,#83146,#83147,#83148,#83149),.UNSPECIFIED.,.F.,.F.,
(4,2,2,2,2,2,2,2,2,2,2,2,2,2,2,2,2,2,2,2,2,2,2,2,2,2,2,2,2,2,2,2,2,2,2,
2,2,2,2,2,2,2,2,2,2,2,2,2,2,2,2,2,2,2,2,2,2,2,2,2,4),(-4.22604418082236,
-4.22327808819264,-4.21936102739766,-4.20446094842647,-4.18747903018636,
-4.1784044142109,-4.17352044405151,-4.16917793782232,-4.16354724173028,
-4.15022279373838,-4.1247504044384,-4.11405063405918,-4.1106751761705,-4.10840872753587,
-4.10591099704085,-4.10114736551919,-4.07911669802533,-4.05988874042377,
-4.05439438983799,-4.05054390573677,-4.04654084487888,-4.04021988412612,
-4.01078559856294,-3.99592082562229,-3.99242451620271,-3.99020252309191,
-3.98778065258953,-3.98355602167842,-3.96532102768477,-3.94893593290557,
-3.94159330497221,-3.9354178205971,-3.93130514256401,-3.92717969575918,
-3.92092861481171,-3.89716054925069,-3.87997595375218,-3.87594227719154,
-3.87352789074872,-3.87111022066475,-3.86699429741439,-3.84635401791738,
-3.82500461185571,-3.81891287446586,-3.8148259907035,-3.81070524239449,
-3.80442740071324,-3.77975359558416,-3.76221884051506,-3.75831568850624,
-3.75594897840387,-3.75355536725498,-3.74946674208105,-3.72866181678669,
-3.7139093692567,-3.70698993964141,-3.70109998253778,-3.69708028489806,
-3.69297748624435,-3.68663051522063,-3.66997076696365),.UNSPECIFIED.);
#1420=B_SPLINE_CURVE_WITH_KNOTS('',3,(#83152,#83153,#83154,#83155,#83156,
#83157,#83158,#83159,#83160,#83161,#83162,#83163,#83164,#83165,#83166,#83167,
#83168,#83169,#83170,#83171,#83172,#83173,#83174,#83175,#83176,#83177,#83178,
#83179,#83180,#83181,#83182,#83183,#83184,#83185,#83186,#83187,#83188,#83189,
#83190,#83191,#83192,#83193,#83194,#83195,#83196,#83197,#83198,#83199,#83200,
#83201,#83202,#83203,#83204,#83205,#83206,#83207,#83208,#83209,#83210,#83211,
#83212,#83213),.UNSPECIFIED.,.F.,.F.,(4,2,2,2,2,2,2,2,2,2,2,2,2,2,2,2,2,
2,2,2,2,2,2,2,2,2,2,2,2,2,4),(0.92152398119564,0.930542222948303,0.957906397135821,
0.973640877462175,0.977498361941586,0.979857594612128,0.982204734629106,
0.985951860520987,1.00046378666866,1.01856980625822,1.04243182151719,1.04871023144959,
1.05284712047941,1.05690439042067,1.0627623999138,1.08071549850968,1.09844311768674,
1.11777276359001,1.12263743664607,1.12525436516788,1.12752019267841,1.13070941500142,
1.13909585654484,1.15339032086897,1.18592444577795,1.192762696269,1.19702020211664,
1.20102944399565,1.20654207318242,1.22099205936091,1.25994577360142),
 .UNSPECIFIED.);
#1421=B_SPLINE_CURVE_WITH_KNOTS('',3,(#83216,#83217,#83218,#83219,#83220,
#83221,#83222,#83223,#83224,#83225,#83226,#83227,#83228,#83229,#83230,#83231,
#83232,#83233,#83234,#83235,#83236,#83237,#83238,#83239,#83240,#83241,#83242,
#83243,#83244,#83245,#83246,#83247,#83248,#83249,#83250,#83251,#83252,#83253,
#83254,#83255),.UNSPECIFIED.,.F.,.F.,(4,3,3,3,3,3,3,3,3,3,3,3,3,4),(-55.7692743084766,
-55.6534283704756,-55.5376479305359,-55.4219003996767,-55.3061487166547,
-55.1903558265821,-55.0743879116938,-54.9583269182872,-54.8420216706817,
-54.7733944101109,-54.6509097908543,-54.5288171495205,-54.4072911748158,
-54.357512134614),.UNSPECIFIED.);
#1422=B_SPLINE_CURVE_WITH_KNOTS('',3,(#83260,#83261,#83262,#83263,#83264,
#83265,#83266,#83267,#83268,#83269,#83270,#83271,#83272,#83273,#83274,#83275,
#83276,#83277,#83278,#83279,#83280,#83281,#83282,#83283,#83284,#83285,#83286,
#83287,#83288,#83289,#83290,#83291,#83292,#83293,#83294,#83295,#83296,#83297,
#83298,#83299,#83300,#83301,#83302,#83303,#83304,#83305,#83306,#83307,#83308,
#83309,#83310,#83311,#83312,#83313,#83314,#83315,#83316,#83317,#83318,#83319,
#83320,#83321,#83322,#83323,#83324,#83325,#83326,#83327,#83328,#83329,#83330,
#83331,#83332,#83333,#83334,#83335,#83336,#83337,#83338,#83339,#83340,#83341),
 .UNSPECIFIED.,.F.,.F.,(4,3,3,3,3,3,3,3,3,3,3,3,3,3,3,3,3,3,3,3,3,3,3,3,
3,3,3,4),(-0.272764230797882,-0.263475368935032,-0.246182477441445,-0.240296053772436,
-0.236376273825625,-0.219184076385875,-0.207427596460933,-0.200432152586668,
-0.196882035074211,-0.180129152494627,-0.163789452319017,-0.154125148485847,
-0.147447841209237,-0.144264614013768,-0.128407246391035,-0.125132236986337,
-0.108107959964319,-0.100850780960037,-0.0956258708151819,-0.0925979657742817,
-0.0768293113674334,-0.0611426794964475,-0.0532929528702713,-0.0475077680039616,
-0.044709499816088,-0.0296052680449404,-0.0148026340224702,0.),
 .UNSPECIFIED.);
#1423=B_SPLINE_CURVE_WITH_KNOTS('',3,(#83342,#83343,#83344,#83345,#83346,
#83347,#83348,#83349,#83350,#83351,#83352,#83353,#83354,#83355),
 .UNSPECIFIED.,.F.,.F.,(4,2,2,2,2,2,4),(9.99999998373441E-7,0.0491146626752611,
0.105092462623141,0.156860905302085,0.207178766483019,0.253689158846026,
0.301589346947622),.UNSPECIFIED.);
#1424=B_SPLINE_CURVE_WITH_KNOTS('',3,(#83593,#83594,#83595,#83596,#83597,
#83598),.UNSPECIFIED.,.F.,.F.,(4,2,4),(8.94639846984786E-5,0.00139415313563322,
0.00270203214836627),.UNSPECIFIED.);
#1425=B_SPLINE_CURVE_WITH_KNOTS('',3,(#83600,#83601,#83602,#83603,#83604,
#83605,#83606,#83607,#83608,#83609,#83610,#83611,#83612,#83613,#83614,#83615,
#83616,#83617,#83618,#83619,#83620,#83621,#83622,#83623,#83624,#83625,#83626,
#83627,#83628,#83629,#83630,#83631,#83632,#83633,#83634,#83635,#83636,#83637,
#83638,#83639,#83640,#83641,#83642,#83643,#83644,#83645,#83646,#83647,#83648,
#83649,#83650,#83651,#83652,#83653,#83654,#83655,#83656,#83657,#83658,#83659,
#83660,#83661,#83662,#83663,#83664,#83665,#83666,#83667,#83668,#83669,#83670,
#83671,#83672,#83673,#83674,#83675,#83676,#83677,#83678,#83679,#83680,#83681,
#83682,#83683,#83684),.UNSPECIFIED.,.F.,.F.,(4,3,3,3,3,3,3,3,3,3,3,3,3,
3,3,3,3,3,3,3,3,3,3,3,3,3,3,3,4),(-0.276631791712689,-0.266883590802822,
-0.252249399427331,-0.244999997209827,-0.241627787357496,-0.226344420306036,
-0.215574858042148,-0.211659554221128,-0.208411272807924,-0.192637118028121,
-0.176589721765353,-0.167489271872747,-0.162477936424474,-0.159585284717452,
-0.143058486365342,-0.14018792219493,-0.124233629563743,-0.116077598840496,
-0.111101224229059,-0.107818411217943,-0.0912654477597725,-0.0743517206583661,
-0.0648501306250925,-0.0586269416525286,-0.0554893882620879,-0.0380440320810531,
-0.0205562383343915,-0.0034758551960099,0.),.UNSPECIFIED.);
#1426=B_SPLINE_CURVE_WITH_KNOTS('',3,(#83685,#83686,#83687,#83688),
 .UNSPECIFIED.,.F.,.F.,(4,4),(-0.0126687472591452,0.),.UNSPECIFIED.);
#1427=B_SPLINE_CURVE_WITH_KNOTS('',3,(#83694,#83695,#83696,#83697,#83698,
#83699,#83700,#83701,#83702,#83703,#83704,#83705,#83706,#83707,#83708,#83709,
#83710,#83711,#83712,#83713,#83714,#83715,#83716,#83717,#83718,#83719,#83720,
#83721,#83722,#83723,#83724,#83725,#83726,#83727,#83728,#83729,#83730,#83731,
#83732,#83733,#83734,#83735,#83736,#83737,#83738,#83739,#83740,#83741,#83742,
#83743,#83744,#83745,#83746,#83747,#83748,#83749,#83750,#83751,#83752,#83753,
#83754,#83755,#83756,#83757,#83758,#83759,#83760,#83761,#83762,#83763,#83764,
#83765,#83766,#83767,#83768,#83769,#83770,#83771,#83772,#83773,#83774,#83775),
 .UNSPECIFIED.,.F.,.F.,(4,3,3,3,3,3,3,3,3,3,3,3,3,3,3,3,3,3,3,3,3,3,3,3,
3,3,3,4),(-0.272764372285567,-0.263475368935033,-0.246182477441449,-0.240296056377085,
-0.236376276566156,-0.219184079084204,-0.207427598821973,-0.200432157374891,
-0.196882034480836,-0.180129152830584,-0.163789459713166,-0.154125154031464,
-0.147447858424305,-0.144264611189609,-0.128407250478866,-0.12513223698636,
-0.108107874550581,-0.100850758306321,-0.0956258537310135,-0.0925979610886074,
-0.0768293076421143,-0.0611426692443636,-0.0532929493125631,-0.0475077621206312,
-0.0447094944615889,-0.0296052542868889,-0.0148026271434445,0.),
 .UNSPECIFIED.);
#1428=B_SPLINE_CURVE_WITH_KNOTS('',3,(#84012,#84013,#84014,#84015,#84016,
#84017),.UNSPECIFIED.,.F.,.F.,(4,2,4),(-0.0027018865616397,-0.00139407808319273,
-8.94593391793846E-5),.UNSPECIFIED.);
#1429=B_SPLINE_CURVE_WITH_KNOTS('',3,(#84340,#84341,#84342,#84343,#84344,
#84345,#84346,#84347,#84348,#84349,#84350,#84351,#84352,#84353,#84354,#84355,
#84356,#84357,#84358,#84359,#84360,#84361,#84362,#84363,#84364,#84365,#84366,
#84367,#84368,#84369,#84370,#84371,#84372,#84373,#84374,#84375,#84376,#84377,
#84378,#84379,#84380,#84381,#84382,#84383,#84384,#84385,#84386,#84387,#84388,
#84389,#84390,#84391,#84392,#84393,#84394,#84395,#84396,#84397,#84398,#84399,
#84400,#84401,#84402,#84403,#84404,#84405,#84406,#84407,#84408,#84409),
 .UNSPECIFIED.,.F.,.F.,(4,2,2,2,2,2,2,2,2,2,2,2,2,2,2,2,2,2,2,2,2,2,2,2,
2,2,2,2,2,2,2,2,2,2,4),(2.76421125033917,2.77723201547172,2.77936414641811,
2.78041526769368,2.78124968604004,2.78223337735643,2.78402129528137,2.79321622328922,
2.83823089709693,2.84905302946592,2.85195012161635,2.85366978347659,2.85517171837985,
2.85702938956112,2.86065133867415,2.89285528030678,2.92143673575942,2.92472338498418,
2.92600594046501,2.92688020515189,2.92776295475109,2.92867181547554,2.9312066033969,
2.93465924463195,2.94366503037432,2.96357410075447,2.99173096918496,2.99493755243625,
2.99689366405073,2.99842510750741,3.00010057231402,3.0028156070367,3.01237607072373,
3.02909331213562,3.06016904789425),.UNSPECIFIED.);
#1430=B_SPLINE_CURVE_WITH_KNOTS('',3,(#84412,#84413,#84414,#84415,#84416,
#84417,#84418,#84419,#84420,#84421,#84422,#84423,#84424,#84425,#84426,#84427,
#84428,#84429,#84430,#84431,#84432,#84433,#84434,#84435,#84436,#84437,#84438,
#84439,#84440,#84441,#84442),.UNSPECIFIED.,.F.,.F.,(4,3,3,3,3,3,3,3,3,3,
4),(0.,0.116076982094954,0.232097056693097,0.348088955573432,0.464088864439995,
0.580132969108435,0.696353414548085,0.812667965282534,0.929223837127315,
0.994694278845732,1.12274180646094),.UNSPECIFIED.);
#1431=B_SPLINE_CURVE_WITH_KNOTS('',3,(#84447,#84448,#84449,#84450,#84451,
#84452,#84453,#84454,#84455,#84456,#84457,#84458,#84459,#84460,#84461,#84462,
#84463,#84464,#84465,#84466,#84467,#84468,#84469,#84470,#84471,#84472,#84473,
#84474,#84475,#84476,#84477,#84478,#84479,#84480,#84481,#84482,#84483,#84484,
#84485,#84486,#84487,#84488,#84489,#84490,#84491,#84492,#84493,#84494,#84495,
#84496,#84497,#84498,#84499,#84500,#84501,#84502,#84503,#84504,#84505,#84506,
#84507,#84508,#84509,#84510,#84511,#84512,#84513,#84514,#84515,#84516,#84517,
#84518,#84519,#84520,#84521,#84522,#84523,#84524,#84525,#84526,#84527,#84528,
#84529,#84530,#84531,#84532,#84533,#84534,#84535,#84536,#84537,#84538,#84539,
#84540,#84541,#84542,#84543,#84544,#84545,#84546,#84547,#84548,#84549,#84550,
#84551,#84552,#84553,#84554,#84555,#84556,#84557,#84558,#84559,#84560,#84561,
#84562,#84563,#84564,#84565,#84566,#84567,#84568,#84569,#84570,#84571,#84572,
#84573,#84574,#84575,#84576,#84577,#84578,#84579,#84580,#84581,#84582,#84583,
#84584,#84585,#84586,#84587,#84588,#84589,#84590,#84591,#84592,#84593,#84594,
#84595,#84596,#84597,#84598,#84599,#84600,#84601,#84602,#84603,#84604,#84605,
#84606,#84607,#84608,#84609,#84610,#84611,#84612,#84613,#84614,#84615,#84616,
#84617,#84618,#84619,#84620,#84621,#84622,#84623,#84624,#84625,#84626,#84627,
#84628,#84629,#84630,#84631,#84632,#84633,#84634,#84635,#84636,#84637,#84638,
#84639,#84640,#84641,#84642,#84643,#84644,#84645,#84646,#84647,#84648,#84649,
#84650,#84651,#84652,#84653,#84654,#84655,#84656,#84657,#84658,#84659,#84660),
 .UNSPECIFIED.,.F.,.F.,(4,2,2,2,2,2,2,2,2,2,2,2,2,2,2,2,2,2,2,2,2,2,2,2,
2,2,2,2,2,2,2,2,2,2,2,2,2,2,2,2,2,2,2,2,2,2,2,2,2,2,2,2,2,2,2,2,2,2,2,2,
2,2,2,2,2,2,2,2,2,2,2,2,2,2,2,2,2,2,2,2,2,2,2,2,2,2,2,2,2,2,2,2,2,2,2,2,
2,2,2,2,2,2,2,2,2,2,4),(1.84293212233226,1.84972675322102,1.89363004897352,
1.90253426724827,1.90421589751822,1.90527580132308,1.9061130180743,1.9070948894541,
1.90887607843526,1.91796374894772,1.96157588217745,1.9734275382624,1.97640543895408,
1.97813895591688,1.97963236349955,1.98145336963407,1.98492176112329,2.01127384547126,
2.03291890050351,2.03832564164711,2.048326749289,2.0500660438755,2.0511434476079,
2.05198233428802,2.05295244920587,2.05467801496651,2.06279629205082,2.08110985780627,
2.11599054523974,2.12097348378096,2.12292408285825,2.12434187368452,2.12586235332593,
2.12790854361059,2.13254366392763,2.15218614503713,2.17780798049297,2.19379892891233,
2.19594487901795,2.19700277548369,2.1978394715261,2.19882168401008,2.20060773195666,
2.20981355884135,2.25541638217924,2.26546442898909,2.26831135435854,2.26999727050283,
2.2713438929194,2.27315473618654,2.27658094594453,2.30095979807754,2.32755419651397,
2.33987540445844,2.34188814996879,2.34293155802555,2.34376710176236,2.34476042910123,
2.34659636222363,2.35679143941954,2.38524668656633,2.41008306395605,2.41330020671868,
2.41524359566025,2.41675309473676,2.418392185887,2.42102039518425,2.42997986942142,
2.4452871348725,2.47210216811407,2.47541844504838,2.48584383743905,2.48760480136674,
2.48868922252973,2.48953029356983,2.49050003240097,2.49221452784788,2.50009751299538,
2.51750384842348,2.5534564041636,2.5583405689607,2.56027666589274,2.56169249343251,
2.56321902214452,2.56528780056284,2.57003814006713,2.59059509311346,2.61634377357414,
2.62069829041445,2.6314517094385,2.63322921971431,2.63430640465496,2.635145025162,
2.63609429682987,2.63774973012023,2.64496969787454,2.66005364578665,2.69826158559999,
2.70411087848331,2.7064138930993,2.70781844494032,2.70932809953151,2.71136549642641,
2.71600495017063,2.73580471338088,2.7612174323221,2.76421125033917),
 .UNSPECIFIED.);
#1432=B_SPLINE_CURVE_WITH_KNOTS('',3,(#84661,#84662,#84663,#84664,#84665,
#84666,#84667,#84668,#84669,#84670,#84671,#84672,#84673,#84674,#84675,#84676,
#84677,#84678,#84679,#84680,#84681,#84682,#84683,#84684,#84685,#84686,#84687,
#84688,#84689,#84690,#84691,#84692,#84693,#84694,#84695,#84696,#84697,#84698,
#84699,#84700,#84701,#84702,#84703,#84704,#84705,#84706,#84707,#84708,#84709,
#84710,#84711,#84712,#84713,#84714,#84715,#84716,#84717,#84718,#84719,#84720,
#84721,#84722,#84723,#84724,#84725,#84726,#84727,#84728,#84729,#84730,#84731,
#84732,#84733,#84734,#84735,#84736,#84737,#84738,#84739,#84740,#84741,#84742,
#84743,#84744,#84745,#84746,#84747,#84748,#84749,#84750,#84751,#84752,#84753,
#84754,#84755,#84756,#84757,#84758,#84759,#84760,#84761,#84762,#84763,#84764,
#84765,#84766,#84767,#84768,#84769,#84770,#84771,#84772,#84773,#84774,#84775,
#84776,#84777,#84778,#84779,#84780,#84781,#84782,#84783,#84784,#84785,#84786,
#84787,#84788,#84789,#84790,#84791,#84792,#84793,#84794,#84795,#84796,#84797,
#84798,#84799,#84800,#84801,#84802,#84803,#84804,#84805,#84806,#84807,#84808,
#84809,#84810,#84811,#84812,#84813,#84814,#84815,#84816,#84817,#84818,#84819,
#84820,#84821,#84822,#84823,#84824,#84825,#84826,#84827,#84828,#84829,#84830,
#84831,#84832,#84833,#84834,#84835,#84836,#84837,#84838,#84839,#84840,#84841,
#84842,#84843,#84844,#84845,#84846,#84847,#84848,#84849,#84850,#84851,#84852,
#84853,#84854,#84855,#84856,#84857,#84858,#84859,#84860,#84861,#84862,#84863,
#84864,#84865,#84866,#84867,#84868),.UNSPECIFIED.,.F.,.F.,(4,3,3,3,3,3,
3,3,3,3,3,3,3,3,3,3,3,3,3,3,3,3,3,3,3,3,3,3,3,3,3,3,3,3,3,3,3,3,3,3,3,3,
3,3,3,3,3,3,3,3,3,3,3,3,3,3,3,3,3,3,3,3,3,3,3,3,3,3,3,4),(1.12274180646094,
1.23344303714648,1.34400474281886,1.45447521756778,1.5649025668582,1.675415346116,
1.78596714841024,1.89673028703231,1.98934601636245,1.98938855769146,2.09290450097165,
2.10300342145843,2.21641547630216,2.32971463245747,2.44294544481904,2.55615236718893,
2.66946071373613,2.78281897934694,2.89638843688897,2.98404626656238,2.98408283653719,
3.08824929947587,3.09772634541184,3.21117354665859,3.32451180574917,3.43778560999423,
3.5510393504477,3.66440012200753,3.77781400505187,3.89144367555841,3.9787386776113,
3.97877711538292,4.08250992410144,4.09207993213216,4.2051770493851,4.31815974498299,
4.43107315443572,4.5439623100504,4.6569549041463,4.76999804301306,4.88325740232231,
4.97343231611545,4.97347139422865,5.07727163318845,5.08695471027319,5.20023564231666,
5.31340404657688,5.42650472777391,5.53958238998565,5.65276390933596,5.76599650655475,
5.87944381868563,5.96812747436669,5.96816567307438,6.0720443952783,6.08163892013194,
6.19491039730512,6.30806973027035,6.42116174058675,6.53423114964273,6.64740513625744,
6.76063058862048,6.87407149018942,6.96282142730057,6.96285995192011,7.07055002716601,
7.08522649739166,7.20726927241575,7.32882665127003,7.40592683901607),
 .UNSPECIFIED.);
#1433=B_SPLINE_CURVE_WITH_KNOTS('',3,(#84873,#84874,#84875,#84876,#84877,
#84878,#84879,#84880,#84881,#84882,#84883,#84884,#84885,#84886,#84887,#84888,
#84889,#84890,#84891,#84892,#84893,#84894,#84895,#84896,#84897,#84898,#84899,
#84900,#84901,#84902,#84903,#84904,#84905,#84906,#84907,#84908,#84909,#84910,
#84911,#84912,#84913,#84914,#84915,#84916,#84917,#84918,#84919,#84920,#84921,
#84922,#84923,#84924,#84925,#84926,#84927,#84928,#84929,#84930,#84931,#84932,
#84933,#84934,#84935,#84936,#84937,#84938,#84939,#84940,#84941,#84942,#84943,
#84944,#84945,#84946,#84947,#84948,#84949,#84950,#84951,#84952,#84953,#84954,
#84955,#84956,#84957,#84958,#84959,#84960,#84961,#84962,#84963,#84964,#84965,
#84966,#84967,#84968,#84969,#84970,#84971,#84972,#84973,#84974,#84975,#84976,
#84977,#84978,#84979,#84980,#84981,#84982,#84983,#84984,#84985,#84986,#84987,
#84988,#84989,#84990,#84991,#84992,#84993,#84994,#84995,#84996,#84997,#84998,
#84999,#85000,#85001,#85002,#85003,#85004,#85005,#85006,#85007,#85008,#85009,
#85010,#85011,#85012,#85013,#85014,#85015,#85016,#85017,#85018,#85019,#85020,
#85021,#85022,#85023,#85024,#85025,#85026,#85027,#85028,#85029,#85030,#85031,
#85032,#85033,#85034,#85035,#85036,#85037,#85038,#85039,#85040,#85041,#85042,
#85043,#85044,#85045,#85046,#85047,#85048,#85049,#85050,#85051,#85052,#85053,
#85054,#85055,#85056,#85057,#85058,#85059,#85060,#85061,#85062,#85063,#85064,
#85065,#85066,#85067,#85068,#85069,#85070,#85071,#85072,#85073,#85074,#85075,
#85076,#85077,#85078,#85079,#85080,#85081,#85082,#85083,#85084,#85085,#85086,
#85087,#85088,#85089,#85090,#85091,#85092,#85093,#85094,#85095,#85096,#85097,
#85098),.UNSPECIFIED.,.F.,.F.,(4,2,2,2,2,2,2,2,2,2,2,2,2,2,2,2,2,2,2,2,
2,2,2,2,2,2,2,2,2,2,2,2,2,2,2,2,2,2,2,2,2,2,2,2,2,2,2,2,2,2,2,2,2,2,2,2,
2,2,2,2,2,2,2,2,2,2,2,2,2,2,2,2,2,2,2,2,2,2,2,2,2,2,2,2,2,2,2,2,2,2,2,2,
2,2,2,2,2,2,2,2,2,2,2,2,2,2,2,2,2,2,2,2,4),(0.921387803811605,0.926936758225414,
0.951373435828612,0.954804129395882,0.956617246048519,0.958110270005632,
0.959850259882243,0.962856479766152,0.975079366926509,0.979298190100335,
1.00936617713551,1.02525132937347,1.02835895414191,1.02958776700503,1.03044937020407,
1.03124081678934,1.03255472306991,1.03595728245377,1.05898895715911,1.07817757773221,
1.09572983648825,1.10009857587304,1.10209620322965,1.10360857411728,1.10523801182131,
1.10782317757969,1.1155528309422,1.16382109239489,1.17316224137613,1.17495699305652,
1.17594186589962,1.17677894771174,1.17783525422895,1.17997284248409,1.20478848107481,
1.22082347451628,1.2411536123937,1.24587177542103,1.24793238674917,1.24945505889899,
1.2508688142991,1.25280436776222,1.25769863891246,1.29382767544972,1.31129686844298,
1.31919614341598,1.32090736093341,1.3218740905318,1.32271329120114,1.32379516492506,
1.3255492457444,1.33585272962387,1.36377732188093,1.38901927785068,1.39246754258527,
1.39428454541659,1.39577801246737,1.39751538686612,1.40050929998135,1.41256425465499,
1.41678080299792,1.44711181859249,1.46294864718872,1.46605180321614,1.46728005483372,
1.46814167197881,1.46893344949856,1.47024853535171,1.47365750653068,1.49781380886419,
1.51969966924817,1.53009515824971,1.53676229020505,1.53920193144259,1.54064011778627,
1.54214955195102,1.54412539444957,1.54837552616952,1.56503137066043,1.5956648933522,
1.59975803175512,1.61049786588383,1.61227542886662,1.61335274298968,1.61419339272617,
1.61515160916936,1.61682389224284,1.62414366865277,1.63953154623754,1.6788830119811,
1.68346257349327,1.68534439024082,1.68674465313799,1.68827785157124,1.69039828910737,
1.69546656522473,1.70251767402919,1.73728983718405,1.75607952096858,1.7582557449891,
1.75931975099058,1.76015732887981,1.76113625723186,1.7629039629578,1.77174743009627,
1.81195911880053,1.82704847853715,1.82996837258339,1.83184298204354,1.83334004767241,
1.83503409198855,1.83791243905998,1.84293212233226),.UNSPECIFIED.);
#1434=B_SPLINE_CURVE_WITH_KNOTS('',3,(#85099,#85100,#85101,#85102,#85103,
#85104,#85105,#85106,#85107,#85108,#85109,#85110,#85111,#85112,#85113,#85114,
#85115,#85116,#85117,#85118,#85119,#85120,#85121,#85122,#85123,#85124,#85125,
#85126,#85127,#85128,#85129,#85130,#85131,#85132,#85133,#85134,#85135,#85136,
#85137,#85138,#85139,#85140,#85141,#85142,#85143,#85144,#85145,#85146,#85147,
#85148,#85149,#85150,#85151,#85152,#85153,#85154,#85155,#85156,#85157,#85158,
#85159,#85160,#85161,#85162,#85163,#85164,#85165,#85166,#85167,#85168,#85169,
#85170,#85171,#85172,#85173,#85174,#85175,#85176,#85177,#85178,#85179,#85180,
#85181,#85182,#85183,#85184,#85185,#85186,#85187,#85188,#85189,#85190,#85191,
#85192,#85193,#85194,#85195,#85196,#85197,#85198,#85199,#85200,#85201,#85202,
#85203,#85204,#85205,#85206,#85207,#85208,#85209,#85210,#85211,#85212,#85213,
#85214,#85215,#85216,#85217,#85218,#85219,#85220,#85221,#85222,#85223,#85224,
#85225,#85226,#85227,#85228,#85229,#85230,#85231,#85232,#85233,#85234,#85235,
#85236,#85237,#85238,#85239,#85240,#85241,#85242,#85243,#85244,#85245,#85246,
#85247,#85248,#85249,#85250,#85251,#85252,#85253,#85254,#85255,#85256,#85257,
#85258,#85259,#85260,#85261,#85262,#85263,#85264,#85265,#85266,#85267,#85268,
#85269,#85270,#85271,#85272,#85273,#85274,#85275,#85276,#85277,#85278,#85279,
#85280,#85281,#85282,#85283,#85284,#85285,#85286,#85287,#85288,#85289,#85290,
#85291,#85292,#85293,#85294,#85295,#85296,#85297,#85298,#85299,#85300,#85301,
#85302,#85303,#85304,#85305,#85306,#85307,#85308,#85309,#85310,#85311,#85312,
#85313,#85314,#85315,#85316,#85317,#85318,#85319,#85320,#85321,#85322,#85323,
#85324,#85325,#85326,#85327,#85328),.UNSPECIFIED.,.F.,.F.,(4,2,2,2,2,2,
2,2,2,2,2,2,2,2,2,2,2,2,2,2,2,2,2,2,2,2,2,2,2,2,2,2,2,2,2,2,2,2,2,2,2,2,
2,2,2,2,2,2,2,2,2,2,2,2,2,2,2,2,2,2,2,2,2,2,2,2,2,2,2,2,2,2,2,2,2,2,2,2,
2,2,2,2,2,2,2,2,2,2,2,2,2,2,2,2,2,2,2,2,2,2,2,2,2,2,2,2,2,2,2,2,2,2,2,2,
4),(0.000426663060224215,0.00334372776168892,0.00580548779923299,0.00727670778860057,
0.00871198391145891,0.0103315383843915,0.0128741686173557,0.0203085926939853,
0.0570868697109929,0.0714978925426921,0.0785257927530299,0.0801760904562657,
0.0811289542299877,0.0819704945671239,0.0830555745788977,0.0848588062267121,
0.0962351159769923,0.124063785064045,0.144501615681988,0.148544548354182,
0.150879174383388,0.152958208756853,0.154465811855288,0.155862769167813,
0.157728227317054,0.162314579956924,0.201686626305909,0.217047735981436,
0.224361138723218,0.226033975478501,0.226992862053752,0.227834109826924,
0.228912417961401,0.230692415220932,0.241510509066355,0.244482135005218,
0.271276682493469,0.29205639712943,0.296828998085613,0.298899590976447,
0.300424423771155,0.301836496266812,0.303764032652648,0.308608390476885,
0.345338042413753,0.362412884989664,0.370207396717381,0.371912159294307,
0.372877647242888,0.37371731505439,0.374801833290118,0.376564235549385,
0.387031484103116,0.40087227956388,0.438028661835564,0.44277751871448,0.444843806690825,
0.446367740496281,0.447780588628643,0.449711675069913,0.454577974334288,
0.491047669072744,0.50829002406265,0.51612937759542,0.517837022891107,0.518803123761574,
0.519642776758211,0.52072649754364,0.522485930166044,0.532888793509432,
0.537685758523827,0.565364551675045,0.584238306850816,0.588778130912684,
0.590807702261349,0.592325859451261,0.593748738852321,0.595717826580927,
0.600812133804884,0.633552216646864,0.65343742337661,0.661944835688176,
0.663694087838166,0.664669428112848,0.665507959022381,0.666578467197476,
0.668293955913746,0.677810385494339,0.681259025973914,0.708955282841503,
0.724322315414994,0.733307540591152,0.735939228265369,0.737579590421914,
0.739089652993197,0.741032922774273,0.744248044375697,0.768803454566392,
0.787489297391622,0.805480861800272,0.808788876760162,0.810048993630402,
0.810917125895629,0.811702758296273,0.812984199204998,0.816186915099057,
0.847096413183407,0.873857696524386,0.879947728043436,0.882227479436006,
0.883792101937034,0.88532504005613,0.887523684488924,0.892682153255465,
0.922069490131181),.UNSPECIFIED.);
#1435=B_SPLINE_CURVE_WITH_KNOTS('',3,(#85334,#85335,#85336,#85337),
 .UNSPECIFIED.,.F.,.F.,(4,4),(1.84334373110974,1.8434049874987),
 .UNSPECIFIED.);
#1436=B_SPLINE_CURVE_WITH_KNOTS('',3,(#85338,#85339,#85340,#85341,#85342,
#85343,#85344,#85345,#85346,#85347,#85348,#85349,#85350,#85351,#85352,#85353,
#85354,#85355,#85356,#85357,#85358,#85359,#85360,#85361,#85362,#85363,#85364,
#85365,#85366,#85367,#85368,#85369,#85370,#85371,#85372,#85373,#85374,#85375,
#85376,#85377,#85378,#85379,#85380,#85381,#85382,#85383,#85384,#85385,#85386,
#85387,#85388,#85389,#85390,#85391,#85392,#85393,#85394,#85395,#85396,#85397,
#85398,#85399,#85400,#85401,#85402,#85403,#85404,#85405,#85406,#85407,#85408,
#85409,#85410,#85411,#85412,#85413,#85414,#85415,#85416,#85417,#85418,#85419,
#85420,#85421,#85422,#85423,#85424,#85425,#85426,#85427,#85428,#85429,#85430,
#85431,#85432,#85433,#85434,#85435,#85436,#85437,#85438,#85439,#85440,#85441,
#85442,#85443,#85444,#85445,#85446,#85447,#85448,#85449,#85450,#85451,#85452,
#85453,#85454,#85455,#85456,#85457,#85458,#85459,#85460,#85461,#85462,#85463,
#85464,#85465,#85466,#85467,#85468,#85469,#85470,#85471,#85472,#85473,#85474,
#85475,#85476,#85477,#85478,#85479,#85480,#85481,#85482,#85483,#85484,#85485,
#85486,#85487,#85488,#85489,#85490,#85491,#85492,#85493,#85494,#85495,#85496,
#85497,#85498,#85499,#85500,#85501,#85502,#85503,#85504,#85505,#85506,#85507,
#85508,#85509,#85510,#85511,#85512,#85513,#85514,#85515,#85516,#85517,#85518,
#85519,#85520,#85521,#85522,#85523,#85524,#85525,#85526,#85527,#85528,#85529,
#85530,#85531,#85532,#85533,#85534,#85535,#85536,#85537,#85538,#85539,#85540,
#85541,#85542,#85543,#85544,#85545,#85546,#85547,#85548,#85549,#85550,#85551,
#85552,#85553,#85554,#85555,#85556,#85557,#85558,#85559,#85560,#85561,#85562,
#85563),.UNSPECIFIED.,.F.,.F.,(4,2,2,2,2,2,2,2,2,2,2,2,2,2,2,2,2,2,2,2,
2,2,2,2,2,2,2,2,2,2,2,2,2,2,2,2,2,2,2,2,2,2,2,2,2,2,2,2,2,2,2,2,2,2,2,2,
2,2,2,2,2,2,2,2,2,2,2,2,2,2,2,2,2,2,2,2,2,2,2,2,2,2,2,2,2,2,2,2,2,2,2,2,
2,2,2,2,2,2,2,2,2,2,2,2,2,2,2,2,2,2,2,2,4),(4.54905144340028E-6,0.0041094722612925,
0.00657049432095091,0.00771703352774657,0.00856563552563301,0.00935905819477919,
0.0101513018477034,0.0112525102515206,0.0140957116269979,0.0202980545450212,
0.0571463629281216,0.0746692716473391,0.0790340547558608,0.0810308935860163,
0.0825430852926223,0.0841727321326731,0.0867590920214259,0.0944986618932328,
0.130569489967454,0.145182799602654,0.149899830617738,0.152085823271165,
0.15335599822209,0.154482544528838,0.155315474323859,0.156238600428662,
0.157753602802971,0.162619840773681,0.210861806819959,0.222996281103226,
0.225898028138964,0.227597040939179,0.229093154496347,0.230959537339959,
0.233853109776184,0.248458457689565,0.289122425916873,0.297998275161044,
0.299767493740607,0.300746630223574,0.301583914535132,0.302646990995203,
0.304819680187474,0.322878272352124,0.324540037977519,0.358531980468752,
0.36909426516359,0.371871770213025,0.37354343423058,0.37504400973174,0.376954647423715,
0.379993338243799,0.397512267815056,0.425638329177515,0.441759870436782,
0.444890375655771,0.446122625691342,0.446984755870316,0.447775216055932,
0.449084579933711,0.452460116085028,0.478883733400005,0.509681405675604,
0.515906323967581,0.518204308451354,0.519771780931139,0.521300044481074,
0.523138237493501,0.527755482070769,0.567363111941259,0.582588715178668,
0.58986023005568,0.591528517627079,0.592485562766307,0.593325964847073,
0.594403933394872,0.59618451519723,0.606963369452004,0.611006890031077,
0.641645532284795,0.658301289750189,0.662550377430304,0.664525545119753,
0.6660343825478,0.667673146911211,0.670301678615058,0.678378247575453,0.726218018928619,
0.735537722002927,0.737331071839674,0.738315513007524,0.73915242755395,
0.740208778752125,0.742347299492102,0.757929978258259,0.782837246365346,
0.798045982360694,0.80696640652479,0.809590353565831,0.811228301061834,
0.812737764605744,0.814682524675043,0.817905007259305,0.844149739035602,
0.879397424834421,0.882512753585785,0.883742791169759,0.884604639141543,
0.885395829428673,0.886708359948769,0.890102331529588,0.915669479233778,
0.921387803811605),.UNSPECIFIED.);
#1437=B_SPLINE_CURVE_WITH_KNOTS('',3,(#85565,#85566,#85567,#85568,#85569,
#85570,#85571,#85572,#85573,#85574,#85575,#85576,#85577,#85578,#85579,#85580,
#85581,#85582,#85583,#85584,#85585,#85586,#85587,#85588,#85589,#85590,#85591,
#85592,#85593,#85594,#85595,#85596,#85597,#85598,#85599,#85600,#85601,#85602,
#85603,#85604,#85605,#85606,#85607,#85608,#85609,#85610,#85611,#85612,#85613,
#85614,#85615,#85616,#85617,#85618,#85619,#85620,#85621,#85622,#85623,#85624,
#85625,#85626,#85627,#85628,#85629,#85630,#85631,#85632,#85633,#85634,#85635,
#85636,#85637,#85638,#85639,#85640,#85641,#85642,#85643,#85644,#85645,#85646,
#85647,#85648,#85649,#85650,#85651,#85652,#85653,#85654,#85655,#85656,#85657,
#85658,#85659,#85660,#85661,#85662,#85663,#85664,#85665,#85666,#85667,#85668,
#85669,#85670,#85671,#85672,#85673,#85674,#85675,#85676,#85677,#85678,#85679,
#85680,#85681,#85682,#85683,#85684,#85685,#85686,#85687,#85688,#85689,#85690,
#85691,#85692,#85693,#85694,#85695,#85696,#85697,#85698,#85699,#85700,#85701,
#85702,#85703,#85704,#85705,#85706,#85707,#85708,#85709,#85710,#85711,#85712,
#85713,#85714,#85715,#85716,#85717,#85718,#85719,#85720,#85721,#85722,#85723,
#85724,#85725,#85726,#85727,#85728,#85729,#85730,#85731,#85732,#85733,#85734,
#85735,#85736,#85737,#85738,#85739,#85740,#85741,#85742,#85743,#85744,#85745,
#85746,#85747,#85748,#85749,#85750,#85751,#85752,#85753,#85754,#85755,#85756,
#85757,#85758,#85759,#85760,#85761,#85762,#85763,#85764,#85765,#85766,#85767,
#85768,#85769,#85770,#85771,#85772,#85773,#85774,#85775,#85776,#85777,#85778,
#85779,#85780,#85781,#85782,#85783,#85784,#85785,#85786,#85787,#85788,#85789,
#85790,#85791,#85792,#85793,#85794,#85795,#85796,#85797,#85798,#85799,#85800,
#85801,#85802,#85803,#85804,#85805,#85806,#85807,#85808,#85809,#85810,#85811,
#85812,#85813,#85814),.UNSPECIFIED.,.F.,.F.,(4,2,2,2,2,2,2,2,2,2,2,2,2,
2,2,2,2,2,2,2,2,2,2,2,2,2,2,2,2,2,2,2,2,2,2,2,2,2,2,2,2,2,2,2,2,2,2,2,2,
2,2,2,2,2,2,2,2,2,2,2,2,2,2,2,2,2,2,2,2,2,2,2,2,2,2,2,2,2,2,2,2,2,2,2,2,
2,2,2,2,2,2,2,2,2,2,2,2,2,2,2,2,2,2,2,2,2,2,2,2,2,2,2,2,2,2,2,2,2,2,2,2,
2,2,2,4),(0.922069490131181,0.92220125174563,0.951353304736987,0.954625118117278,
0.955918284162328,0.956706101202181,0.957571992931478,0.958820890154348,
0.962054932510227,0.979247484172206,1.00036945292123,1.02345131949731,1.02664415263097,
1.0285808536907,1.03008993408803,1.03173338397707,1.03437917454588,1.04350453637844,
1.05922352184658,1.08007867971714,1.09888348680942,1.10106046688351,1.10212487690641,
1.10296284130973,1.1039423551793,1.10571125425586,1.11456408315627,1.15488282919892,
1.16986590015639,1.17278119368915,1.17465492521696,1.17615263670132,1.17784886041334,
1.18073449162112,1.19263221391073,1.23748888475154,1.24545914765856,1.24708532537392,
1.24812860072792,1.24896527332474,1.24996139839117,1.25180738041548,1.26219220371598,
1.29185987101013,1.31527353737618,1.31847267636831,1.32041115918665,1.32192041053508,
1.32356281958281,1.32620423043858,1.33528718868746,1.35089906839215,1.38267770403834,
1.3912721222959,1.39293640903918,1.39399132599825,1.39482861099182,1.3958152612933,
1.39761719545511,1.40708742309575,1.45851884214338,1.46378698568197,1.46600360995306,
1.46740011670142,1.46893709676678,1.47107743577679,1.47626536388673,1.48353248270139,
1.50458633090199,1.53510174824096,1.53830950661935,1.53959157107798,1.5403771548807,
1.54124482781781,1.5425035857501,1.54580408246349,1.5637206453313,1.58310976211004,
1.60706307088978,1.61027039268239,1.61221104274299,1.61372032223805,1.61536109321222,
1.61799620218171,1.62702076197512,1.64248692143862,1.67446271177295,1.68306009096076,
1.68472427982311,1.6857790387771,1.68656908530414,1.68657222812386,1.68657530886022,
1.68657812929896,1.68658093692676,1.68658373179912,1.68658651403093,1.68658928366336,
1.6865920407385,1.68659478537549,1.68659751764687,1.68755659423814,1.68925853591206,
1.69138130109429,1.69590718357968,1.70958926057312,1.72872751629385,1.75289560636979,
1.75610588003528,1.75804742952256,1.75955688190076,1.76119731173892,1.76383071174866,
1.77283784978246,1.78825994119835,1.81850986985775,1.82477561214273,1.82952459293217,
1.8310257783573,1.83194604873785,1.83274910090807,1.83358616232252,1.83470060027602,
1.83785306587972,1.84354018446068),.UNSPECIFIED.);
#1438=B_SPLINE_CURVE_WITH_KNOTS('',3,(#85815,#85816,#85817,#85818),
 .UNSPECIFIED.,.F.,.F.,(4,4),(0.000539378737039987,0.000599447974599068),
 .UNSPECIFIED.);
#1439=B_SPLINE_CURVE_WITH_KNOTS('',3,(#85823,#85824,#85825,#85826,#85827,
#85828,#85829,#85830,#85831,#85832,#85833,#85834,#85835,#85836,#85837,#85838,
#85839,#85840,#85841,#85842,#85843,#85844,#85845,#85846,#85847,#85848,#85849,
#85850,#85851,#85852,#85853,#85854,#85855,#85856,#85857,#85858,#85859,#85860,
#85861,#85862,#85863,#85864,#85865,#85866,#85867,#85868,#85869,#85870,#85871,
#85872,#85873,#85874,#85875,#85876,#85877,#85878,#85879,#85880,#85881,#85882,
#85883,#85884,#85885,#85886,#85887,#85888,#85889,#85890,#85891,#85892,#85893,
#85894,#85895,#85896,#85897,#85898,#85899,#85900,#85901,#85902,#85903,#85904,
#85905,#85906,#85907,#85908,#85909,#85910,#85911,#85912,#85913,#85914,#85915,
#85916,#85917,#85918,#85919,#85920,#85921,#85922,#85923,#85924,#85925,#85926,
#85927,#85928,#85929,#85930,#85931,#85932,#85933,#85934,#85935,#85936,#85937,
#85938,#85939,#85940,#85941,#85942,#85943,#85944,#85945,#85946,#85947,#85948,
#85949,#85950,#85951,#85952,#85953,#85954,#85955,#85956,#85957,#85958,#85959,
#85960,#85961,#85962,#85963,#85964,#85965,#85966,#85967,#85968,#85969,#85970,
#85971,#85972,#85973,#85974,#85975,#85976,#85977,#85978,#85979,#85980,#85981,
#85982,#85983,#85984,#85985,#85986,#85987,#85988,#85989,#85990,#85991,#85992,
#85993,#85994,#85995,#85996,#85997,#85998,#85999,#86000,#86001,#86002,#86003,
#86004,#86005,#86006,#86007,#86008,#86009,#86010,#86011,#86012,#86013,#86014,
#86015,#86016,#86017,#86018,#86019,#86020,#86021,#86022,#86023,#86024,#86025,
#86026,#86027,#86028,#86029,#86030,#86031,#86032,#86033,#86034,#86035,#86036,
#86037,#86038,#86039,#86040,#86041,#86042,#86043,#86044,#86045,#86046,#86047,
#86048,#86049,#86050,#86051,#86052,#86053,#86054,#86055,#86056,#86057,#86058,
#86059,#86060,#86061,#86062),.UNSPECIFIED.,.F.,.F.,(4,2,2,2,2,2,2,2,2,2,
2,2,2,2,2,2,2,2,2,2,2,2,2,2,2,2,2,2,2,2,2,2,2,2,2,2,2,2,2,2,2,2,2,2,2,2,
2,2,2,2,2,2,2,2,2,2,2,2,2,2,2,2,2,2,2,2,2,2,2,2,2,2,2,2,2,2,2,2,2,2,2,2,
2,2,2,2,2,2,2,2,2,2,2,2,2,2,2,2,2,2,2,2,2,2,2,2,2,2,2,2,2,2,2,2,2,2,2,2,
2,4),(0.921708299814284,0.921789731266711,0.94590707435828,0.971652614281142,
0.975043877985191,0.976356194554188,0.977147502257003,0.978009700204245,
0.979240615055326,0.982360138460563,0.998362981766927,1.02774351448395,
1.0333326511807,1.04487915695327,1.04783400141833,1.0495625129385,1.05105668939971,
1.05288503461159,1.05638726784014,1.08491818002176,1.11813826540223,1.12111213088128,
1.12223220538517,1.12302961781011,1.12388701080135,1.1250921851985,1.1280509299624,
1.14246814861644,1.16168854550644,1.16954298334344,1.18994376038308,1.19307220768716,
1.19501045022373,1.19651505779055,1.19817327328402,1.20088713256837,1.2107232720813,
1.22831520302462,1.25335771752399,1.26550016535475,1.26733204145147,1.26842534373202,
1.26926803438747,1.27021676249985,1.27184596911428,1.27858159303533,1.29205337294686,
1.3129678169058,1.33571659974108,1.33890185416102,1.34083606715715,1.34234446318853,
1.34398843099019,1.34663783660143,1.35580368006252,1.37162666360741,1.40328457701521,
1.4117186746368,1.41337326519574,1.41442511900194,1.41526206444115,1.41625074633227,
1.41806265135896,1.42773493086101,1.45155602192279,1.48159686249775,1.48479702192268,
1.48673559873559,1.4882446057992,1.48988642553663,1.49252616713353,1.50159589293146,
1.5171748457098,1.54873879091301,1.55757950899064,1.559257930194,1.56031703561855,
1.56115443131396,1.56213745575501,1.56392319429677,1.5730889512963,1.61795557119905,
1.62865978357502,1.63157197593149,1.63327374429509,1.63475600232024,1.63661328644093,
1.6402569547735,1.67010809551642,1.68559854168956,1.70302311104751,1.70518502925304,
1.7062461782991,1.7070578572778,1.707062235329,1.70706655878106,1.70707082867284,
1.70707504605706,1.70707921191129,1.70708332714614,1.70708739269483,1.70709140946424,
1.7070953783664,1.7070993002579,1.70710317601657,1.7071070064775,1.70807797953287,
1.70912532094375,1.71076424036142,1.71390999278722,1.72183028100631,1.76418609796086,
1.7746137816538,1.77749980448296,1.77919566084649,1.78054296907062,1.7823454420134,
1.78572527668427,1.80810802194668,1.84334373110974),.UNSPECIFIED.);
#1440=B_SPLINE_CURVE_WITH_KNOTS('',3,(#86063,#86064,#86065,#86066,#86067,
#86068,#86069,#86070,#86071,#86072,#86073,#86074,#86075,#86076,#86077,#86078,
#86079,#86080,#86081,#86082,#86083,#86084,#86085,#86086,#86087,#86088,#86089,
#86090,#86091,#86092,#86093,#86094,#86095,#86096,#86097,#86098,#86099,#86100,
#86101,#86102,#86103,#86104,#86105,#86106,#86107,#86108,#86109,#86110,#86111,
#86112,#86113,#86114,#86115,#86116,#86117,#86118,#86119,#86120,#86121,#86122,
#86123,#86124,#86125,#86126,#86127,#86128,#86129,#86130,#86131,#86132,#86133,
#86134,#86135,#86136,#86137,#86138,#86139,#86140,#86141,#86142,#86143,#86144,
#86145,#86146,#86147,#86148,#86149,#86150,#86151,#86152,#86153,#86154,#86155,
#86156,#86157,#86158,#86159,#86160,#86161,#86162,#86163,#86164,#86165,#86166,
#86167,#86168,#86169,#86170,#86171,#86172,#86173,#86174,#86175,#86176,#86177,
#86178,#86179,#86180,#86181,#86182,#86183,#86184,#86185,#86186,#86187,#86188,
#86189,#86190,#86191,#86192,#86193,#86194,#86195,#86196,#86197,#86198,#86199,
#86200,#86201,#86202,#86203,#86204,#86205,#86206,#86207,#86208,#86209,#86210,
#86211,#86212,#86213,#86214,#86215,#86216,#86217,#86218,#86219,#86220,#86221,
#86222,#86223,#86224,#86225,#86226,#86227,#86228,#86229,#86230,#86231,#86232,
#86233,#86234,#86235,#86236,#86237,#86238,#86239,#86240,#86241,#86242,#86243,
#86244,#86245,#86246,#86247,#86248,#86249,#86250,#86251,#86252,#86253,#86254,
#86255,#86256,#86257,#86258,#86259,#86260,#86261,#86262,#86263,#86264,#86265,
#86266,#86267,#86268,#86269,#86270,#86271,#86272,#86273,#86274,#86275,#86276,
#86277,#86278,#86279,#86280,#86281,#86282,#86283,#86284),.UNSPECIFIED.,
 .F.,.F.,(4,2,2,2,2,2,2,2,2,2,2,2,2,2,2,2,2,2,2,2,2,2,2,2,2,2,2,2,2,2,2,
2,2,2,2,2,2,2,2,2,2,2,2,2,2,2,2,2,2,2,2,2,2,2,2,2,2,2,2,2,2,2,2,2,2,2,2,
2,2,2,2,2,2,2,2,2,2,2,2,2,2,2,2,2,2,2,2,2,2,2,2,2,2,2,2,2,2,2,2,2,2,2,2,
2,2,2,2,2,2,2,4),(0.000599447974599068,0.0316058343624691,0.0559765062106575,
0.0594065575766221,0.0612199114777653,0.0627134313290408,0.0644543456907345,
0.0674630407632168,0.0797103299225923,0.0838689340102289,0.113979531472804,
0.1259644542748,0.130121023356855,0.132119106774741,0.133722103550208,0.134667972504823,
0.135460246533888,0.136519301770196,0.138600674711707,0.153014955338879,
0.179757526025723,0.199859918933514,0.204550761093584,0.20660675735005,
0.208128831328901,0.209544038389503,0.211484713821694,0.216408393520337,
0.252154743076204,0.269874841602856,0.27784025270698,0.279555874845522,
0.280523658843792,0.281362871268922,0.282443592499416,0.284193516071882,
0.294407151238243,0.324622262655388,0.340095833821893,0.349122682942974,
0.351758123255411,0.353399020355675,0.35490836131806,0.356849013692629,
0.360056151691328,0.388757790755906,0.413625845140476,0.423508107512758,
0.425330280655839,0.426321179919503,0.427157984637327,0.428207136025029,
0.42985287271923,0.438140159811396,0.470089785829843,0.485828253098796,
0.494959683161271,0.497605616320123,0.49924880392347,0.500757407702729,
0.502693169520043,0.505883727193834,0.528897271108723,0.549423171677817,
0.562938892862379,0.569688593767652,0.57131884102101,0.572267789937073,
0.573110413999905,0.574203320701592,0.576033893173099,0.588140420692956,
0.618338736506903,0.637574875924401,0.642159239819632,0.644196328871069,
0.645715244828897,0.647135319990179,0.64909496239278,0.654133365625509,
0.688076099415013,0.713905071715865,0.716564481614196,0.717718906419336,
0.718567639260335,0.719379581544169,0.720797048959808,0.724900360469889,
0.732708270428822,0.735733864282571,0.760472217420362,0.777105431807572,
0.786582605608628,0.789262494582738,0.790913177848279,0.792419661684219,
0.794340356414039,0.797479780449177,0.818310957521071,0.825597637369747,
0.844690401519224,0.859273284321613,0.862249334135628,0.863457303400389,
0.864315189735906,0.865111883286627,0.866229333326279,0.869183841100843,
0.902580934070594,0.921827501307929,0.921911067911426),.UNSPECIFIED.);
#1441=B_SPLINE_CURVE_WITH_KNOTS('',3,(#86289,#86290,#86291,#86292,#86293,
#86294,#86295,#86296,#86297,#86298,#86299,#86300,#86301,#86302,#86303,#86304,
#86305,#86306,#86307,#86308,#86309,#86310,#86311,#86312,#86313,#86314,#86315,
#86316,#86317,#86318,#86319,#86320,#86321,#86322,#86323,#86324,#86325,#86326,
#86327,#86328,#86329,#86330,#86331,#86332,#86333,#86334,#86335,#86336,#86337,
#86338,#86339,#86340,#86341,#86342,#86343,#86344,#86345,#86346,#86347,#86348,
#86349,#86350,#86351,#86352,#86353,#86354,#86355,#86356,#86357,#86358,#86359,
#86360,#86361,#86362,#86363,#86364,#86365,#86366,#86367,#86368,#86369,#86370,
#86371,#86372,#86373,#86374,#86375,#86376,#86377,#86378,#86379,#86380,#86381,
#86382,#86383,#86384,#86385,#86386,#86387,#86388,#86389,#86390,#86391,#86392,
#86393,#86394,#86395,#86396,#86397,#86398,#86399,#86400,#86401,#86402,#86403,
#86404,#86405,#86406,#86407,#86408,#86409,#86410,#86411,#86412,#86413,#86414,
#86415,#86416,#86417,#86418,#86419,#86420,#86421,#86422,#86423,#86424,#86425,
#86426,#86427,#86428,#86429,#86430,#86431,#86432,#86433,#86434,#86435,#86436,
#86437,#86438,#86439,#86440,#86441,#86442,#86443,#86444,#86445,#86446,#86447,
#86448,#86449,#86450,#86451,#86452,#86453,#86454,#86455,#86456,#86457,#86458,
#86459,#86460,#86461,#86462,#86463,#86464,#86465,#86466,#86467,#86468,#86469,
#86470,#86471,#86472,#86473,#86474,#86475,#86476,#86477,#86478,#86479,#86480,
#86481,#86482,#86483,#86484,#86485,#86486,#86487,#86488,#86489,#86490,#86491,
#86492,#86493,#86494,#86495,#86496,#86497,#86498,#86499,#86500,#86501,#86502,
#86503,#86504,#86505,#86506,#86507,#86508,#86509,#86510,#86511,#86512,#86513,
#86514,#86515,#86516,#86517,#86518),.UNSPECIFIED.,.F.,.F.,(4,2,2,2,2,2,
2,2,2,2,2,2,2,2,2,2,2,2,2,2,2,2,2,2,2,2,2,2,2,2,2,2,2,2,2,2,2,2,2,2,2,2,
2,2,2,2,2,2,2,2,2,2,2,2,2,2,2,2,2,2,2,2,2,2,2,2,2,2,2,2,2,2,2,2,2,2,2,2,
2,2,2,2,2,2,2,2,2,2,2,2,2,2,2,2,2,2,2,2,2,2,2,2,2,2,2,2,2,2,2,2,2,2,2,2,
4),(0.000214697203212984,0.0160514925799108,0.0231282367207183,0.0254863851464672,
0.0271276107098235,0.0285295300915837,0.0300305745001698,0.0319418376304527,
0.0349815799780459,0.0525094072768143,0.064162534249541,0.0763414403195431,
0.0916808737339768,0.0989864539099635,0.100657443960427,0.101615233837524,
0.102455755710174,0.103533196016409,0.105311507480465,0.116063282985645,
0.116526333666239,0.144585197536107,0.16498866789945,0.169029260291844,
0.172259618593857,0.174023050365629,0.175501559721651,0.177248191605193,
0.18028319852455,0.192878898492621,0.224836677878989,0.242416819340641,
0.245686354163779,0.246940251979115,0.247806806685877,0.248593076365453,
0.24987951232973,0.253114206518393,0.283318632878354,0.290213340483236,
0.314615176939245,0.31804518230156,0.319858186682743,0.321351247099808,
0.323091426357392,0.326098340072308,0.338329663363518,0.34252944998083,
0.381802540076032,0.390568592898111,0.392331988507076,0.393310021502913,
0.394147673939351,0.395212904663296,0.397395599149604,0.41846926761471,
0.447989135166039,0.461283953489719,0.464266384567512,0.465983461799876,
0.467478195262668,0.469320549325389,0.472134979459764,0.485496686589406,
0.527479398662504,0.536454924390792,0.53823010447395,0.539210742250717,
0.540048203858205,0.541110087276293,0.543275660348879,0.560994786650693,
0.58180503566487,0.60408392751185,0.609030074556835,0.611129977332169,0.612659468916105,
0.614064059631685,0.616326109056425,0.621873214146587,0.660201877032794,
0.675306612768332,0.682543764088235,0.684210122161386,0.685167005928949,
0.686007895483813,0.687087293549919,0.688871888851967,0.699809609921197,
0.703508054607814,0.730498545966056,0.750391612974393,0.75505695456852,
0.757108358999092,0.758629564388107,0.76004577000708,0.762370145589266,
0.768289401515878,0.806216899890256,0.821239691086843,0.828452754316401,
0.830117461666343,0.831074018203979,0.831915033711835,0.832995122419306,
0.834781948020924,0.845770141194436,0.873154912323348,0.898203379129927,
0.901648020116273,0.903464388228047,0.904957984613752,0.906696248962834,
0.909693533631725,0.921708299814284),.UNSPECIFIED.);
#1442=B_SPLINE_CURVE_WITH_KNOTS('',3,(#86519,#86520,#86521,#86522,#86523,
#86524,#86525,#86526,#86527,#86528,#86529,#86530,#86531,#86532,#86533,#86534,
#86535,#86536,#86537,#86538,#86539,#86540,#86541,#86542,#86543,#86544,#86545,
#86546,#86547,#86548,#86549,#86550,#86551,#86552,#86553,#86554,#86555,#86556,
#86557,#86558,#86559,#86560,#86561,#86562,#86563,#86564,#86565,#86566,#86567,
#86568,#86569,#86570,#86571,#86572,#86573,#86574,#86575,#86576,#86577,#86578,
#86579,#86580,#86581,#86582,#86583,#86584,#86585,#86586,#86587,#86588,#86589,
#86590,#86591,#86592,#86593,#86594,#86595,#86596,#86597,#86598,#86599,#86600,
#86601,#86602,#86603,#86604,#86605,#86606,#86607,#86608,#86609,#86610,#86611,
#86612,#86613,#86614,#86615,#86616,#86617,#86618,#86619,#86620,#86621,#86622,
#86623,#86624,#86625,#86626,#86627,#86628,#86629,#86630,#86631,#86632,#86633,
#86634,#86635,#86636,#86637,#86638,#86639,#86640,#86641,#86642,#86643,#86644,
#86645,#86646,#86647,#86648,#86649,#86650,#86651,#86652,#86653,#86654,#86655,
#86656,#86657,#86658,#86659,#86660,#86661,#86662,#86663,#86664,#86665,#86666,
#86667,#86668,#86669,#86670,#86671,#86672,#86673,#86674,#86675,#86676,#86677,
#86678,#86679,#86680,#86681,#86682,#86683,#86684,#86685,#86686,#86687,#86688,
#86689,#86690,#86691,#86692,#86693,#86694,#86695,#86696,#86697,#86698,#86699,
#86700,#86701,#86702,#86703,#86704,#86705,#86706,#86707,#86708,#86709,#86710,
#86711,#86712,#86713,#86714,#86715,#86716,#86717,#86718,#86719,#86720,#86721,
#86722,#86723,#86724,#86725,#86726,#86727,#86728,#86729,#86730,#86731,#86732,
#86733,#86734,#86735,#86736,#86737,#86738,#86739,#86740,#86741,#86742,#86743,
#86744),.UNSPECIFIED.,.F.,.F.,(4,2,2,2,2,2,2,2,2,2,2,2,2,2,2,2,2,2,2,2,
2,2,2,2,2,2,2,2,2,2,2,2,2,2,2,2,2,2,2,2,2,2,2,2,2,2,2,2,2,2,2,2,2,2,2,2,
2,2,2,2,2,2,2,2,2,2,2,2,2,2,2,2,2,2,2,2,2,2,2,2,2,2,2,2,2,2,2,2,2,2,2,2,
2,2,2,2,2,2,2,2,2,2,2,2,2,2,2,2,2,2,2,2,4),(0.921911067911426,0.932057510574157,
0.934924512857622,0.936616411754293,0.937964562576898,0.939773288637249,
0.943181744868466,0.966647054738132,0.998596004945917,1.00688034467127,
1.00852574948545,1.0095747433567,1.01041145525951,1.01140227903129,1.01322441113245,
1.02310817570771,1.04798556341299,1.07669719648176,1.07990303696367,1.08184318333282,
1.08335230447239,1.08499313794199,1.08762886268935,1.09666067905984,1.11214562213073,
1.14268795106139,1.15255376393477,1.15428648229455,1.15536195955285,1.15620058621139,
1.15717166785449,1.15890274818593,1.1671175206504,1.18581259318349,1.22018566656015,
1.22520160674482,1.22715746888381,1.22857647307731,1.23009580462306,1.23213617402151,
1.23673963255853,1.2561292339163,1.28634040710973,1.29823263753587,1.30005521174384,
1.30114572279265,1.3019879577464,1.30293810587292,1.30457408750186,1.31140002537676,
1.32515913252836,1.34334903434381,1.3683395239452,1.37155708646108,1.3735006468175,
1.37501024103969,1.37664939910462,1.37927763419326,1.38823614880114,1.40353720091919,
1.42981948241854,1.4330803026184,1.44410327821361,1.44589133026969,1.44697171891923,
1.44781269366585,1.44876889839803,1.45043232239574,1.45762926841595,1.47260173335774,
1.51026920629644,1.51642618574486,1.51878717278402,1.52021018406596,1.52172698162709,
1.52375215328918,1.52827124515601,1.54698800140676,1.57234872007764,1.58965236270196,
1.59181295230498,1.59287380777954,1.59371115701819,1.59469248550477,1.59647101296352,
1.60550892465014,1.64840323755668,1.66089378565031,1.66392101937986,1.66566578872729,
1.66714425530211,1.66890948400089,1.67214302644645,1.67619197921456,1.69777064272047,
1.7179331817276,1.73547837295413,1.73764117613713,1.73870236080801,1.73953959930982,
1.74052036834784,1.74229679957767,1.75130046012535,1.76796782335889,1.78455164984034,
1.80590713024781,1.8090588792184,1.81098283232641,1.81248929892418,1.81413734079802,
1.81583126495222,1.81831832708071,1.84303969707496),.UNSPECIFIED.);
#1443=B_SPLINE_CURVE_WITH_KNOTS('',3,(#86750,#86751,#86752,#86753,#86754,
#86755,#86756,#86757,#86758,#86759,#86760,#86761,#86762,#86763,#86764,#86765,
#86766,#86767,#86768,#86769,#86770,#86771,#86772,#86773,#86774,#86775,#86776,
#86777,#86778,#86779,#86780,#86781,#86782,#86783,#86784,#86785,#86786,#86787,
#86788,#86789,#86790,#86791,#86792,#86793,#86794,#86795,#86796,#86797,#86798,
#86799,#86800,#86801,#86802,#86803,#86804,#86805,#86806,#86807,#86808,#86809,
#86810,#86811,#86812,#86813,#86814,#86815,#86816,#86817,#86818,#86819,#86820,
#86821,#86822,#86823,#86824,#86825,#86826,#86827,#86828,#86829,#86830,#86831,
#86832,#86833,#86834,#86835,#86836,#86837,#86838,#86839,#86840,#86841,#86842,
#86843,#86844,#86845,#86846,#86847,#86848,#86849,#86850,#86851,#86852,#86853,
#86854,#86855,#86856,#86857,#86858,#86859,#86860,#86861,#86862,#86863,#86864,
#86865,#86866,#86867,#86868,#86869,#86870,#86871,#86872,#86873,#86874,#86875,
#86876,#86877,#86878,#86879,#86880,#86881,#86882,#86883,#86884,#86885,#86886,
#86887,#86888,#86889,#86890,#86891,#86892,#86893,#86894,#86895,#86896,#86897,
#86898,#86899,#86900,#86901,#86902,#86903,#86904,#86905,#86906,#86907,#86908,
#86909,#86910,#86911,#86912,#86913,#86914,#86915,#86916,#86917,#86918,#86919,
#86920,#86921,#86922,#86923,#86924,#86925,#86926,#86927,#86928,#86929,#86930,
#86931,#86932,#86933,#86934,#86935,#86936,#86937,#86938,#86939,#86940,#86941,
#86942,#86943,#86944,#86945,#86946,#86947,#86948,#86949,#86950,#86951,#86952,
#86953,#86954,#86955,#86956,#86957,#86958,#86959,#86960,#86961,#86962,#86963,
#86964,#86965,#86966,#86967,#86968,#86969,#86970,#86971,#86972,#86973,#86974,
#86975,#86976,#86977,#86978,#86979),.UNSPECIFIED.,.F.,.F.,(4,2,2,2,2,2,
2,2,2,2,2,2,2,2,2,2,2,2,2,2,2,2,2,2,2,2,2,2,2,2,2,2,2,2,2,2,2,2,2,2,2,2,
2,2,2,2,2,2,2,2,2,2,2,2,2,2,2,2,2,2,2,2,2,2,2,2,2,2,2,2,2,2,2,2,2,2,2,2,
2,2,2,2,2,2,2,2,2,2,2,2,2,2,2,2,2,2,2,2,2,2,2,2,2,2,2,2,2,2,2,2,2,2,2,2,
4),(0.92195427717175,0.921973901496767,0.923091497504975,0.923888218207204,
0.924746030748282,0.925953709841547,0.928928085237592,0.943495821713098,
0.96262116175145,0.969950594700634,0.990774739088636,0.993914235461341,
0.995834912646202,0.997341347758119,0.998991938783069,1.00167158252704,
1.01114675507128,1.02777167317095,1.05232768032855,1.05543805573243,1.06642651098004,
1.06821325573149,1.06929330504395,1.0701342941729,1.07109081623147,1.07275546648672,
1.07996804917874,1.09499104306598,1.13290083688255,1.13885008560609,1.14117885649958,
1.14259585033082,1.1441164503858,1.14616449979271,1.15081115516655,1.1705500189747,
1.195821202368,1.19825117016901,1.20134648902897,1.21232065881903,1.21410668320771,
1.21518647274568,1.21602736955049,1.21698391217889,1.2186488865979,1.22586738079979,
1.24091111672634,1.27892362046886,1.28477171132582,1.28708490083993,1.28849888763765,
1.2900212475605,1.2920804506833,1.29679103739043,1.33300383179863,1.35607978761377,
1.35948236172438,1.36079641428702,1.36158799010225,1.36244976945527,1.36367889757174,
1.36678763657845,1.39641612445705,1.42578529984481,1.43094638411129,1.43314494150014,
1.4346773998433,1.4362411789582,1.43851904872315,1.44460008363608,1.47098728591634,
1.50229890416152,1.50546721600175,1.50674255959211,1.5075268164188,1.50839565409672,
1.50966062213922,1.51300325793552,1.53138701768706,1.5436707350812,1.57426990749613,
1.57745531446596,1.57938937668403,1.58089750971279,1.58254104393215,1.5851894259368,
1.59434841896075,1.61015540781746,1.64187006155175,1.65026317490606,1.65191508158618,
1.65296600885864,1.65380274865187,1.65479181097718,1.6566060277151,1.66633014598367,
1.69203812347397,1.72010097718476,1.72331179390172,1.72525330143445,1.72676249593133,
1.72816194572898,1.73041863275592,1.73677961569699,1.74635009680969,1.76338637087314,
1.79398356736075,1.79719820347499,1.79848131010894,1.79926700081203,1.80013428333466,
1.80139158082396,1.80468316854952,1.82250352462013,1.84334958263878),
 .UNSPECIFIED.);
#1444=B_SPLINE_CURVE_WITH_KNOTS('',3,(#86980,#86981,#86982,#86983),
 .UNSPECIFIED.,.F.,.F.,(4,4),(8.78772022666079E-5,0.000214697203212984),
 .UNSPECIFIED.);
#1445=B_SPLINE_CURVE_WITH_KNOTS('',3,(#86985,#86986,#86987,#86988),
 .UNSPECIFIED.,.F.,.F.,(4,4),(1.84303969707496,1.84316407965133),
 .UNSPECIFIED.);
#1446=B_SPLINE_CURVE_WITH_KNOTS('',3,(#86989,#86990,#86991,#86992,#86993,
#86994,#86995,#86996,#86997,#86998,#86999,#87000,#87001,#87002,#87003,#87004,
#87005,#87006,#87007,#87008,#87009,#87010,#87011,#87012,#87013,#87014,#87015,
#87016,#87017,#87018,#87019,#87020,#87021,#87022,#87023,#87024,#87025,#87026,
#87027,#87028,#87029,#87030,#87031,#87032,#87033,#87034,#87035,#87036,#87037,
#87038,#87039,#87040,#87041,#87042,#87043,#87044,#87045,#87046,#87047,#87048,
#87049,#87050,#87051,#87052,#87053,#87054,#87055,#87056,#87057,#87058,#87059,
#87060,#87061,#87062,#87063,#87064,#87065,#87066,#87067,#87068,#87069,#87070,
#87071,#87072,#87073,#87074,#87075,#87076,#87077,#87078,#87079,#87080,#87081,
#87082,#87083,#87084,#87085,#87086,#87087,#87088,#87089,#87090,#87091,#87092,
#87093,#87094,#87095,#87096,#87097,#87098,#87099,#87100,#87101,#87102,#87103,
#87104,#87105,#87106,#87107,#87108,#87109,#87110,#87111,#87112,#87113,#87114,
#87115,#87116,#87117,#87118,#87119,#87120,#87121,#87122,#87123,#87124,#87125,
#87126,#87127,#87128,#87129,#87130,#87131,#87132,#87133,#87134,#87135,#87136,
#87137,#87138,#87139,#87140,#87141,#87142,#87143,#87144,#87145,#87146,#87147,
#87148,#87149,#87150,#87151,#87152,#87153,#87154,#87155,#87156,#87157,#87158,
#87159,#87160,#87161,#87162,#87163,#87164,#87165,#87166,#87167,#87168,#87169,
#87170,#87171,#87172,#87173,#87174,#87175,#87176,#87177,#87178,#87179,#87180,
#87181,#87182,#87183,#87184,#87185,#87186,#87187,#87188,#87189,#87190,#87191,
#87192,#87193,#87194,#87195,#87196,#87197,#87198,#87199,#87200,#87201,#87202,
#87203,#87204,#87205,#87206,#87207,#87208,#87209,#87210,#87211,#87212,#87213,
#87214),.UNSPECIFIED.,.F.,.F.,(4,2,2,2,2,2,2,2,2,2,2,2,2,2,2,2,2,2,2,2,
2,2,2,2,2,2,2,2,2,2,2,2,2,2,2,2,2,2,2,2,2,2,2,2,2,2,2,2,2,2,2,2,2,2,2,2,
2,2,2,2,2,2,2,2,2,2,2,2,2,2,2,2,2,2,2,2,2,2,2,2,2,2,2,2,2,2,2,2,2,2,2,2,
2,2,2,2,2,2,2,2,2,2,2,2,2,2,2,2,2,2,2,2,4),(0.000470462646023128,0.0204922171035094,
0.0370988817818748,0.0402772102298867,0.0415173749253083,0.0423814292663502,
0.0431708564645063,0.0444730420352634,0.0478015357351266,0.0757274614132303,
0.0893807207704344,0.10267208687341,0.11076690917383,0.11324041277449,0.114880368170131,
0.116390052885393,0.118332831842172,0.121547132606634,0.149085445589273,
0.175197506194649,0.184994531675472,0.186812592023987,0.187802622633527,
0.188639510290839,0.189689798286327,0.191339207447399,0.199686462941816,
0.234798670915509,0.253357209902113,0.257856429728947,0.259878262423531,
0.261394773566892,0.262819126115341,0.265186139976812,0.271377543846967,
0.308997034944195,0.323961046158831,0.331156460148119,0.332819980688512,
0.33377632313522,0.334617468782666,0.335698151298732,0.337486847122686,
0.348517862090443,0.351878685779993,0.376163572466532,0.400891499282885,
0.404329534038799,0.406144629339743,0.407638314561696,0.409377977551032,
0.412380910472977,0.424549830877153,0.428668744361367,0.468081357076615,
0.476859626329267,0.478624173040981,0.479602680976926,0.480440644346913,
0.481506166891304,0.483689129389093,0.504980698994866,0.534325484471477,
0.547582551545762,0.550563270894803,0.552280375998838,0.553775735554607,
0.555619637621047,0.55843789193154,0.571848538021873,0.613779639160073,
0.622752158449686,0.62452763778718,0.625508565615243,0.626346357012073,
0.627408783422206,0.629575889756567,0.647381669012106,0.683023674088682,
0.690162597246958,0.695279564426719,0.697408478077412,0.698943578004517,
0.700342686913735,0.702572751506658,0.707922497214126,0.746463142660987,
0.761610871730347,0.768861159300485,0.770528798321554,0.771486147849491,
0.772327273494162,0.773406772434223,0.775191127926812,0.786069031016917,
0.789906217462343,0.815990244085093,0.83117387298874,0.840085558060999,
0.842709618298333,0.844348231087091,0.845858713681023,0.847805358567995,
0.851032222503032,0.878548247163884,0.912515951173339,0.915643813755194,
0.916876263137658,0.917738951430209,0.918530260935449,0.919626819211096,
0.921853710912926,0.921871960720837),.UNSPECIFIED.);
#1447=B_SPLINE_CURVE_WITH_KNOTS('',3,(#87220,#87221,#87222,#87223),
 .UNSPECIFIED.,.F.,.F.,(4,4),(1.84335924581655,1.84346799293763),
 .UNSPECIFIED.);
#1448=B_SPLINE_CURVE_WITH_KNOTS('',3,(#87224,#87225,#87226,#87227,#87228,
#87229,#87230,#87231,#87232,#87233,#87234,#87235,#87236,#87237,#87238,#87239,
#87240,#87241,#87242,#87243,#87244,#87245,#87246,#87247,#87248,#87249,#87250,
#87251,#87252,#87253,#87254,#87255,#87256,#87257,#87258,#87259,#87260,#87261,
#87262,#87263,#87264,#87265,#87266,#87267,#87268,#87269,#87270,#87271,#87272,
#87273,#87274,#87275,#87276,#87277,#87278,#87279,#87280,#87281,#87282,#87283,
#87284,#87285,#87286,#87287,#87288,#87289,#87290,#87291,#87292,#87293,#87294,
#87295,#87296,#87297,#87298,#87299,#87300,#87301,#87302,#87303,#87304,#87305,
#87306,#87307,#87308,#87309,#87310,#87311,#87312,#87313,#87314,#87315,#87316,
#87317,#87318,#87319,#87320,#87321,#87322,#87323,#87324,#87325,#87326,#87327,
#87328,#87329,#87330,#87331,#87332,#87333,#87334,#87335,#87336,#87337,#87338,
#87339,#87340,#87341,#87342,#87343,#87344,#87345,#87346,#87347,#87348,#87349,
#87350,#87351,#87352,#87353,#87354,#87355,#87356,#87357,#87358,#87359,#87360,
#87361,#87362,#87363,#87364,#87365,#87366,#87367,#87368,#87369,#87370,#87371,
#87372,#87373,#87374,#87375,#87376,#87377,#87378,#87379,#87380,#87381,#87382,
#87383,#87384,#87385,#87386,#87387,#87388,#87389,#87390,#87391,#87392,#87393,
#87394,#87395,#87396,#87397,#87398,#87399,#87400,#87401,#87402,#87403,#87404,
#87405,#87406,#87407,#87408,#87409,#87410,#87411,#87412,#87413,#87414,#87415,
#87416,#87417,#87418,#87419,#87420,#87421,#87422,#87423,#87424,#87425,#87426,
#87427,#87428,#87429,#87430,#87431,#87432,#87433,#87434,#87435,#87436,#87437,
#87438,#87439,#87440,#87441),.UNSPECIFIED.,.F.,.F.,(4,2,2,2,2,2,2,2,2,2,
2,2,2,2,2,2,2,2,2,2,2,2,2,2,2,2,2,2,2,2,2,2,2,2,2,2,2,2,2,2,2,2,2,2,2,2,
2,2,2,2,2,2,2,2,2,2,2,2,2,2,2,2,2,2,2,2,2,2,2,2,2,2,2,2,2,2,2,2,2,2,2,2,
2,2,2,2,2,2,2,2,2,2,2,2,2,2,2,2,2,2,2,2,2,2,2,2,2,2,4),(0.000501094062160151,
0.020376313225356,0.0377674182519577,0.0456454330718914,0.0473550889202536,
0.0483213823981442,0.0491605029236977,0.050242657749981,0.0519979328477672,
0.0623297296595978,0.0924281345294714,0.107896468141753,0.113871172024639,
0.118286036310736,0.120253520557417,0.121776926225932,0.123189123313575,
0.125119067206428,0.1299811675561,0.171020918051707,0.184829815969152,0.191672049711161,
0.193309194057752,0.194259561477828,0.195101668241075,0.196191588880556,
0.19801227919406,0.209853275385144,0.240238608264144,0.259566931752169,
0.264162484858407,0.266201349363525,0.267720332761023,0.269139562432046,
0.271480685232317,0.27751393626361,0.315309858531276,0.330310639796793,
0.337516802809565,0.339180862070359,0.340137196844317,0.340978117791995,
0.342058213536103,0.343845315306817,0.354844194203893,0.358356964904617,
0.384456646491752,0.405205415292156,0.409973673381514,0.41204302346883,
0.413567176170371,0.414978782742025,0.416905932910184,0.42175060921958,
0.458455869168049,0.475538961250223,0.483334938168772,0.485039458283113,
0.4860047231396,0.486844161090152,0.487928313168206,0.489689949193669,0.500147319720073,
0.530125159039801,0.551073509620668,0.555865492522148,0.55793899498697,
0.559463891338942,0.56087455297108,0.562797889452789,0.567619720314074,
0.604576424633933,0.621494178976928,0.629245445338757,0.630947065048312,
0.631911710767307,0.632751273135275,0.633836456256942,0.635601482843632,
0.646127313574301,0.676036838083129,0.691497983676949,0.700519949852961,
0.703154720605649,0.704795347685613,0.706304535108436,0.708245117099112,
0.71145239864302,0.740886310212513,0.765166140901391,0.774931614962136,
0.776747964858226,0.777737544172118,0.778574332254882,0.779624832536468,
0.781275183543627,0.78964021433028,0.821619046844376,0.842828702128301,
0.847651473401638,0.849730310823131,0.851256137888875,0.852665554840647,
0.8545839515487,0.85937647157219,0.896641722775173,0.902130835318364,0.918790577694836,
0.92195427717175),.UNSPECIFIED.);
#1449=B_SPLINE_CURVE_WITH_KNOTS('',3,(#87443,#87444,#87445,#87446,#87447,
#87448,#87449,#87450,#87451,#87452,#87453,#87454,#87455,#87456,#87457,#87458,
#87459,#87460,#87461,#87462,#87463,#87464,#87465,#87466,#87467,#87468,#87469,
#87470,#87471,#87472,#87473,#87474,#87475,#87476,#87477,#87478,#87479,#87480,
#87481,#87482,#87483,#87484,#87485,#87486,#87487,#87488,#87489,#87490,#87491,
#87492,#87493,#87494,#87495,#87496,#87497,#87498,#87499,#87500,#87501,#87502,
#87503,#87504,#87505,#87506,#87507,#87508,#87509,#87510,#87511,#87512,#87513,
#87514,#87515,#87516,#87517,#87518,#87519,#87520,#87521,#87522,#87523,#87524,
#87525,#87526,#87527,#87528,#87529,#87530,#87531,#87532,#87533,#87534,#87535,
#87536,#87537,#87538,#87539,#87540,#87541,#87542,#87543,#87544,#87545,#87546,
#87547,#87548,#87549,#87550,#87551,#87552,#87553,#87554,#87555,#87556,#87557,
#87558,#87559,#87560,#87561,#87562,#87563,#87564,#87565,#87566,#87567,#87568,
#87569,#87570,#87571,#87572,#87573,#87574,#87575,#87576,#87577,#87578,#87579,
#87580,#87581,#87582,#87583,#87584,#87585,#87586,#87587,#87588,#87589,#87590,
#87591,#87592,#87593,#87594,#87595,#87596,#87597,#87598,#87599,#87600,#87601,
#87602,#87603,#87604,#87605,#87606,#87607,#87608,#87609,#87610,#87611,#87612,
#87613,#87614,#87615,#87616,#87617,#87618,#87619,#87620,#87621,#87622,#87623,
#87624,#87625,#87626,#87627,#87628,#87629,#87630,#87631,#87632,#87633,#87634,
#87635,#87636,#87637,#87638,#87639,#87640,#87641,#87642,#87643,#87644,#87645,
#87646,#87647,#87648,#87649,#87650,#87651,#87652,#87653,#87654,#87655,#87656,
#87657,#87658,#87659,#87660,#87661,#87662,#87663,#87664,#87665,#87666,#87667,
#87668,#87669,#87670,#87671,#87672,#87673,#87674,#87675,#87676,#87677,#87678,
#87679,#87680,#87681,#87682,#87683,#87684,#87685,#87686,#87687,#87688,#87689,
#87690,#87691,#87692,#87693,#87694),.UNSPECIFIED.,.F.,.F.,(4,2,2,2,2,2,
2,2,2,2,2,2,2,2,2,2,2,2,2,2,2,2,2,2,2,2,2,2,2,2,2,2,2,2,2,2,2,2,2,2,2,2,
2,2,2,2,2,2,2,2,2,2,2,2,2,2,2,2,2,2,2,2,2,2,2,2,2,2,2,2,2,2,2,2,2,2,2,2,
2,2,2,2,2,2,2,2,2,2,2,2,2,2,2,2,2,2,2,2,2,2,2,2,2,2,2,2,2,2,2,2,2,2,2,2,
2,2,2,2,2,2,2,2,2,2,2,4),(0.921871960720837,0.949440270215207,0.981844760548665,
0.986952506252835,0.988923574561786,0.990346843202346,0.991864447701091,
0.99389161486827,0.998419030815228,1.0171946820494,1.04409920487034,1.0598501517797,
1.0619912342064,1.06304845733733,1.06388587399885,1.06487069916664,1.06666424384185,
1.07597318287055,1.12350908662567,1.13186598618005,1.13452943703573,1.13617647319092,
1.13768392914491,1.13964435589459,1.14381186007085,1.14930204889285,1.1629327539329,
1.18867677082547,1.19390841509642,1.20593926726569,1.20776703180699,1.20885910858364,
1.20970160953145,1.21065099282944,1.21228327831922,1.2190596204163,1.23266092093696,
1.25258459123235,1.27609284374246,1.2792930387934,1.28123159514816,1.2827405666013,
1.28438233156231,1.28702195934497,1.29609127492545,1.31167038566065,1.34326420112935,
1.35205414982,1.35372962784688,1.3547878219802,1.35562513678774,1.35660882851573,
1.35839773028544,1.36762397273887,1.41358743585898,1.4232923439455,1.42610590256454,
1.42778589124642,1.42913556913536,1.43096070576421,1.43444835877218,1.46197712635463,
1.49247184353942,1.49836368556698,1.49999114651512,1.50093938084243,1.50169750912244,
1.50276260327295,1.50494440575319,1.50781261548173,1.51723526435086,1.53831388440014,
1.56783276627006,1.57102968516615,1.57296712753593,1.57447575041889,1.57611765854942,
1.57875866690053,1.58784430150739,1.60346583626812,1.63530263667441,1.64380952792065,
1.64546820210787,1.64652119473949,1.64735805998754,1.64834551100934,1.65015224444485,
1.65972700100909,1.68463737325803,1.71364856568915,1.71685250923932,1.71879199860814,
1.72030090068092,1.72036734817925,1.72041439853904,1.72044803799979,1.72047225569849,
1.72050602193721,1.72053758851671,1.72056713939904,1.72059483925627,1.72062083588314,
1.72064526226447,1.72066823833742,1.72068987253635,1.72071026311724,1.72072949932219,
1.72074766235311,1.72076482625617,1.72078105871009,1.72079642165799,1.72081097189782,
1.72260456772777,1.7259599289535,1.73020406300406,1.73960705086323,1.75614464028749,
1.78758271474888,1.79073419597156,1.79200670526168,1.79279043246386,1.79365984490964,
1.7949276802637,1.79828966621556,1.81689221546138,1.84313766613365),
 .UNSPECIFIED.);
#1450=B_SPLINE_CURVE_WITH_KNOTS('',3,(#87695,#87696,#87697,#87698),
 .UNSPECIFIED.,.F.,.F.,(4,4),(0.000510341810198537,0.000621055971545034),
 .UNSPECIFIED.);
#1451=B_SPLINE_CURVE_WITH_KNOTS('',3,(#87703,#87704,#87705,#87706,#87707,
#87708,#87709,#87710,#87711,#87712,#87713,#87714,#87715,#87716,#87717,#87718,
#87719,#87720,#87721,#87722,#87723,#87724,#87725,#87726,#87727,#87728,#87729,
#87730,#87731,#87732,#87733,#87734,#87735,#87736,#87737,#87738,#87739,#87740,
#87741,#87742,#87743,#87744,#87745,#87746,#87747,#87748,#87749,#87750,#87751,
#87752,#87753,#87754,#87755,#87756,#87757,#87758,#87759,#87760,#87761,#87762,
#87763,#87764,#87765,#87766,#87767,#87768,#87769,#87770,#87771,#87772,#87773,
#87774,#87775,#87776,#87777,#87778,#87779,#87780,#87781,#87782,#87783,#87784,
#87785,#87786,#87787,#87788,#87789,#87790,#87791,#87792,#87793,#87794,#87795,
#87796,#87797,#87798,#87799,#87800,#87801,#87802,#87803,#87804,#87805,#87806,
#87807,#87808,#87809,#87810,#87811,#87812,#87813,#87814,#87815,#87816,#87817,
#87818,#87819,#87820,#87821,#87822,#87823,#87824,#87825,#87826,#87827,#87828,
#87829,#87830,#87831,#87832,#87833,#87834,#87835,#87836,#87837,#87838,#87839,
#87840,#87841,#87842,#87843,#87844,#87845,#87846,#87847,#87848,#87849,#87850,
#87851,#87852,#87853,#87854,#87855,#87856,#87857,#87858,#87859,#87860,#87861,
#87862,#87863,#87864,#87865,#87866,#87867,#87868,#87869,#87870,#87871,#87872,
#87873,#87874,#87875,#87876,#87877,#87878,#87879,#87880,#87881,#87882,#87883,
#87884,#87885,#87886,#87887,#87888,#87889,#87890,#87891,#87892,#87893,#87894,
#87895,#87896,#87897,#87898,#87899,#87900,#87901,#87902,#87903,#87904,#87905,
#87906,#87907,#87908,#87909,#87910,#87911,#87912,#87913,#87914,#87915,#87916,
#87917,#87918,#87919,#87920,#87921,#87922,#87923,#87924,#87925,#87926),
 .UNSPECIFIED.,.F.,.F.,(4,2,2,2,2,2,2,2,2,2,2,2,2,2,2,2,2,2,2,2,2,2,2,2,
2,2,2,2,2,2,2,2,2,2,2,2,2,2,2,2,2,2,2,2,2,2,2,2,2,2,2,2,2,2,2,2,2,2,2,2,
2,2,2,2,2,2,2,2,2,2,2,2,2,2,2,2,2,2,2,2,2,2,2,2,2,2,2,2,2,2,2,2,2,2,2,2,
2,2,2,2,2,2,2,2,2,2,2,2,2,2,2,4),(0.922109850357463,0.926364499330458,0.938252071945183,
0.941232922345019,0.942967199885786,0.944460690111436,0.946281080107383,
0.949746090750819,0.975891065241991,1.00038381370429,1.00451588356627,1.01329126410738,
1.01496793366453,1.01602636640117,1.01686352074859,1.01784659973918,1.01963329440533,
1.02882316078698,1.0741321101012,1.08442447138741,1.08729761044652,1.08899050727524,
1.09033800296037,1.09214398295239,1.09554109250375,1.11858613723642,1.14790794619228,
1.15898242127555,1.16077230856695,1.16185307932804,1.1626938941529,1.16364937824045,
1.16531029777561,1.17247680882564,1.18734837429602,1.22455924321813,1.23116209350491,
1.23359177536206,1.2350276994089,1.2365373818014,1.23851791453039,1.24279532185581,
1.25965907199514,1.28736898559233,1.30454171988466,1.30670444512319,1.30776555292121,
1.30860270835493,1.30958333616694,1.3113593851968,1.32035799399458,1.36267955028518,
1.37571905933657,1.37878488047906,1.38053817785746,1.38188102092444,1.38361697088017,
1.38668774526506,1.4014515929009,1.43929878506412,1.45067941081909,1.45248164966096,
1.45356595729397,1.45440708781459,1.45536016104177,1.45701058580612,1.464035749906,
1.47844050833185,1.50814651004822,1.52150880430896,1.52432265127615,1.52616449079028,
1.5276587262965,1.52937514250395,1.53235619951655,1.5456414545098,1.57512959381509,
1.59619729556426,1.59837898581387,1.59944379248093,1.60028114570728,1.60125886290403,
1.60302178303157,1.6117869241105,1.65106156349731,1.65523784576473,1.66748879079407,
1.67049639363684,1.67223631714902,1.67372877006225,1.67550444632073,1.67880087165689,
1.6829393562013,1.71244647747798,1.74029634877152,1.74362522015739,1.74492690475812,
1.74571583350044,1.74657915177492,1.74781792265938,1.75099081611581,1.76755352926108,
1.79100855696042,1.80084762855678,1.81326033949228,1.8162813771251,1.81802442210205,
1.81950250627412,1.8209278109473,1.82269097878976,1.82534575354189,1.84335924581655),
 .UNSPECIFIED.);
#1452=B_SPLINE_CURVE_WITH_KNOTS('',3,(#87927,#87928,#87929,#87930,#87931,
#87932,#87933,#87934,#87935,#87936,#87937,#87938,#87939,#87940,#87941,#87942,
#87943,#87944,#87945,#87946,#87947,#87948,#87949,#87950,#87951,#87952,#87953,
#87954,#87955,#87956,#87957,#87958,#87959,#87960,#87961,#87962,#87963,#87964,
#87965,#87966,#87967,#87968,#87969,#87970,#87971,#87972,#87973,#87974,#87975,
#87976,#87977,#87978,#87979,#87980,#87981,#87982,#87983,#87984,#87985,#87986,
#87987,#87988,#87989,#87990,#87991,#87992,#87993,#87994,#87995,#87996,#87997,
#87998,#87999,#88000,#88001,#88002,#88003,#88004,#88005,#88006,#88007,#88008,
#88009,#88010,#88011,#88012,#88013,#88014,#88015,#88016,#88017,#88018,#88019,
#88020,#88021,#88022,#88023,#88024,#88025,#88026,#88027,#88028,#88029,#88030,
#88031,#88032,#88033,#88034,#88035,#88036,#88037,#88038,#88039,#88040,#88041,
#88042,#88043,#88044,#88045,#88046,#88047,#88048,#88049,#88050,#88051,#88052,
#88053,#88054,#88055,#88056,#88057,#88058,#88059,#88060,#88061,#88062,#88063,
#88064,#88065,#88066,#88067,#88068,#88069,#88070,#88071,#88072,#88073,#88074,
#88075,#88076,#88077,#88078,#88079,#88080,#88081,#88082,#88083,#88084,#88085,
#88086,#88087,#88088,#88089,#88090,#88091,#88092,#88093,#88094,#88095,#88096,
#88097,#88098,#88099,#88100,#88101,#88102,#88103,#88104,#88105,#88106,#88107,
#88108,#88109,#88110,#88111,#88112,#88113,#88114,#88115,#88116,#88117,#88118,
#88119,#88120,#88121,#88122,#88123,#88124,#88125,#88126,#88127,#88128,#88129,
#88130,#88131,#88132,#88133,#88134,#88135,#88136,#88137,#88138,#88139,#88140,
#88141,#88142,#88143,#88144,#88145,#88146,#88147,#88148,#88149,#88150,#88151,
#88152,#88153,#88154,#88155,#88156,#88157,#88158,#88159,#88160,#88161,#88162),
 .UNSPECIFIED.,.F.,.F.,(4,2,2,2,2,2,2,2,2,2,2,2,2,2,2,2,2,2,2,2,2,2,2,2,
2,2,2,2,2,2,2,2,2,2,2,2,2,2,2,2,2,2,2,2,2,2,2,2,2,2,2,2,2,2,2,2,2,2,2,2,
2,2,2,2,2,2,2,2,2,2,2,2,2,2,2,2,2,2,2,2,2,2,2,2,2,2,2,2,2,2,2,2,2,2,2,2,
2,2,2,2,2,2,2,2,2,2,2,2,2,2,2,2,2,2,2,2,2,4),(0.000621055971545034,0.0164926796293739,
0.0191424794876196,0.0209040757166634,0.0223297365801582,0.0236773254295353,
0.0253762575001516,0.028274252475158,0.0388233649085059,0.0485458344049959,
0.0682550157821357,0.0852865890181955,0.0930686791312674,0.0947724834768994,
0.0957376949138948,0.0965773200645051,0.0976620404053763,0.0994252519311364,
0.109911090360743,0.114550976110018,0.126268455762736,0.148564967824195,
0.158404387555766,0.162786493138197,0.166240426924207,0.168049692651747,
0.169545187720327,0.17126067029907,0.174158237475727,0.18506807987538,0.191760653128429,
0.220146080575321,0.236670583682186,0.239841072468563,0.241080045847406,
0.241943888771945,0.242733603456548,0.244037204297219,0.247374245808302,
0.275159674935999,0.308505692472417,0.31208412791158,0.313928290823128,
0.315423554641253,0.317140210663372,0.320043200985554,0.331013388873103,
0.337597127611375,0.376013997553858,0.384707558979374,0.386467235801051,
0.387444661494943,0.388282703239985,0.389349619916852,0.391053647525328,
0.400357966284453,0.403997720132482,0.440250011500114,0.455242174118239,
0.45832721935937,0.46006698553238,0.461410802087836,0.463162567746466,0.466218578314965,
0.479100405068117,0.521582509197995,0.530593251180539,0.532370726160038,
0.533352040023926,0.534189720984912,0.535251443584593,0.536938258905477,
0.545927337685542,0.577357008136213,0.592922943615645,0.601986644574306,
0.604625954600122,0.606267793831014,0.607777015550761,0.609716145240351,
0.612917808843082,0.636497281597006,0.641289614579291,0.666172962314351,
0.676350172627506,0.678186413933024,0.679180370145092,0.680017039023202,
0.681062599921189,0.683080837211674,0.6954891002435,0.720222841308283,0.737839819218355,
0.747684069007246,0.750398810713735,0.752057305106886,0.753561999645563,
0.75550012606168,0.758627908359886,0.779009524883296,0.786951119708183,
0.806264450903208,0.820500464269846,0.82344031351037,0.824642442175337,
0.825499329162049,0.8262976042475,0.827420764790109,0.830416803026016,0.863430040095334,
0.882915239736762,0.893418385440269,0.896191831735704,0.897863197372455,
0.899364872648781,0.901278793526907,0.904326494053748,0.921990538769251),
 .UNSPECIFIED.);
#1453=B_SPLINE_CURVE_WITH_KNOTS('',3,(#88167,#88168,#88169,#88170,#88171,
#88172,#88173,#88174,#88175,#88176,#88177,#88178,#88179,#88180,#88181,#88182,
#88183,#88184,#88185,#88186,#88187,#88188,#88189,#88190,#88191,#88192,#88193,
#88194,#88195,#88196,#88197,#88198,#88199,#88200,#88201,#88202,#88203,#88204,
#88205,#88206,#88207,#88208,#88209,#88210,#88211,#88212,#88213,#88214,#88215,
#88216,#88217,#88218,#88219,#88220,#88221,#88222,#88223,#88224,#88225,#88226,
#88227,#88228,#88229,#88230,#88231,#88232,#88233,#88234,#88235,#88236,#88237,
#88238,#88239,#88240,#88241,#88242,#88243,#88244,#88245,#88246,#88247,#88248,
#88249,#88250,#88251,#88252,#88253,#88254,#88255,#88256,#88257,#88258,#88259,
#88260,#88261,#88262,#88263,#88264,#88265,#88266,#88267,#88268,#88269,#88270,
#88271,#88272,#88273,#88274,#88275,#88276,#88277,#88278,#88279,#88280,#88281,
#88282,#88283,#88284,#88285,#88286,#88287,#88288,#88289,#88290,#88291,#88292,
#88293,#88294,#88295,#88296,#88297,#88298,#88299,#88300,#88301,#88302,#88303,
#88304,#88305,#88306,#88307,#88308,#88309,#88310,#88311,#88312,#88313,#88314,
#88315,#88316,#88317,#88318,#88319,#88320,#88321,#88322,#88323,#88324,#88325,
#88326,#88327,#88328,#88329,#88330,#88331,#88332,#88333,#88334,#88335,#88336,
#88337,#88338,#88339,#88340,#88341,#88342,#88343,#88344,#88345,#88346,#88347,
#88348,#88349,#88350,#88351,#88352,#88353,#88354,#88355,#88356,#88357,#88358,
#88359,#88360,#88361,#88362,#88363,#88364,#88365,#88366,#88367,#88368,#88369,
#88370,#88371,#88372,#88373,#88374,#88375,#88376,#88377,#88378,#88379,#88380,
#88381,#88382,#88383,#88384,#88385,#88386,#88387,#88388,#88389,#88390,#88391,
#88392,#88393,#88394,#88395,#88396,#88397,#88398,#88399,#88400,#88401,#88402,
#88403,#88404,#88405,#88406,#88407,#88408,#88409,#88410,#88411,#88412,#88413,
#88414,#88415,#88416,#88417,#88418,#88419,#88420,#88421,#88422,#88423,#88424),
 .UNSPECIFIED.,.F.,.F.,(4,2,2,2,2,2,2,2,2,2,2,2,2,2,2,2,2,2,2,2,2,2,2,2,
2,2,2,2,2,2,2,2,2,2,2,2,2,2,2,2,2,2,2,2,2,2,2,2,2,2,2,2,2,2,2,2,2,2,2,2,
2,2,2,2,2,2,2,2,2,2,2,2,2,2,2,2,2,2,2,2,2,2,2,2,2,2,2,2,2,2,2,2,2,2,2,2,
2,2,2,2,2,2,2,2,2,2,2,2,2,2,2,2,2,2,2,2,2,2,2,2,2,2,2,2,2,2,2,2,4),(0.000580235344661419,
0.0225432725559789,0.0395195756805615,0.0547395813179001,0.0636647592289831,
0.0662893339773771,0.0679275068706122,0.0694370656605665,0.071381791396974,
0.0746038758623836,0.100692516496477,0.134022921254523,0.137186221434361,
0.138831619142547,0.139881618525447,0.140854475675506,0.14085845504871,
0.140862475382216,0.14086653747776,0.140870642194567,0.140874790346985,
0.140878982754138,0.140883220351244,0.140887504057328,0.140891834753636,
0.140896213392345,0.140900640982074,0.140905118533105,0.140909647062502,
0.140914227611597,0.140918861284402,0.140923549246386,0.14092829263095,
0.140933092597562,0.140937950393802,0.140942867296467,0.14094784458359,
0.141762958628665,0.142847246558218,0.144609616366993,0.155049145550168,
0.196770974110713,0.209027001387201,0.211938011948635,0.213639297782944,
0.21513550833927,0.216999514246637,0.219884630711234,0.234360152636289,
0.275172747046177,0.284061267213561,0.285831476204802,0.286810960669843,
0.287648418956745,0.288711557736351,0.290403810357839,0.299499540448613,
0.330229923266626,0.351800758571081,0.356665191279316,0.358750943959766,
0.360277740098149,0.361685174891756,0.363596460974486,0.368348380697992,
0.406003952948499,0.422457822563985,0.430081001629044,0.431773878741676,
0.432736493932439,0.433576193984735,0.434664063183912,0.436438424621314,
0.447137735160929,0.447666166110834,0.488570899497871,0.500829523502527,
0.503740726563205,0.505442057516021,0.506938267048643,0.508802218339132,
0.511687148474593,0.526159803908707,0.56697554561199,0.575864321203696,
0.577634547798976,0.578614037668986,0.579451497902992,0.580514635722414,
0.582686914796312,0.60106129134795,0.627512104316833,0.644443987980966,
0.648730689246205,0.650713189823178,0.652223398067841,0.653659090162944,
0.656086602020193,0.662672843991754,0.699893670327183,0.714764785291494,
0.721932128303132,0.723593308505528,0.724548963585063,0.725389937841757,
0.72647093567088,0.728261248933046,0.739338752603396,0.741691332518053,
0.768807938975371,0.791741189702345,0.795136080787728,0.796941804215888,
0.798420636620535,0.800161852764312,0.80317294626838,0.815457920507041,
0.819529757589767,0.849700462084764,0.865568663206356,0.868674777175894,
0.869903430230972,0.870765069343073,0.871556665839067,0.872871051160187,
0.876276076178247,0.899766057275845,0.922002574267844,0.922109850357463),
 .UNSPECIFIED.);
#1454=B_SPLINE_CURVE_WITH_KNOTS('',3,(#88425,#88426,#88427,#88428,#88429,
#88430,#88431,#88432,#88433,#88434,#88435,#88436,#88437,#88438,#88439,#88440,
#88441,#88442,#88443,#88444,#88445,#88446,#88447,#88448,#88449,#88450,#88451,
#88452,#88453,#88454,#88455,#88456,#88457,#88458,#88459,#88460,#88461,#88462,
#88463,#88464,#88465,#88466,#88467,#88468,#88469,#88470,#88471,#88472,#88473,
#88474,#88475,#88476,#88477,#88478,#88479,#88480,#88481,#88482,#88483,#88484,
#88485,#88486,#88487,#88488,#88489,#88490,#88491,#88492,#88493,#88494,#88495,
#88496,#88497,#88498,#88499,#88500,#88501,#88502,#88503,#88504,#88505,#88506,
#88507,#88508,#88509,#88510,#88511,#88512,#88513,#88514,#88515,#88516,#88517,
#88518,#88519,#88520,#88521,#88522,#88523,#88524,#88525,#88526,#88527,#88528,
#88529,#88530,#88531,#88532,#88533,#88534,#88535,#88536,#88537,#88538,#88539,
#88540,#88541,#88542,#88543,#88544,#88545,#88546,#88547,#88548,#88549,#88550,
#88551,#88552,#88553,#88554,#88555,#88556,#88557,#88558,#88559,#88560,#88561,
#88562,#88563,#88564,#88565,#88566,#88567,#88568,#88569,#88570,#88571,#88572,
#88573,#88574,#88575,#88576,#88577,#88578,#88579,#88580,#88581,#88582,#88583,
#88584,#88585,#88586,#88587,#88588,#88589,#88590,#88591,#88592,#88593,#88594,
#88595,#88596,#88597,#88598,#88599,#88600,#88601,#88602,#88603,#88604,#88605,
#88606,#88607,#88608,#88609,#88610,#88611,#88612,#88613,#88614,#88615,#88616,
#88617,#88618,#88619,#88620,#88621,#88622,#88623,#88624,#88625,#88626,#88627,
#88628,#88629,#88630,#88631,#88632,#88633,#88634,#88635,#88636),
 .UNSPECIFIED.,.F.,.F.,(4,2,2,2,2,2,2,2,2,2,2,2,2,2,2,2,2,2,2,2,2,2,2,2,
2,2,2,2,2,2,2,2,2,2,2,2,2,2,2,2,2,2,2,2,2,2,2,2,2,2,2,2,2,2,2,2,2,2,2,2,
2,2,2,2,2,2,2,2,2,2,2,2,2,2,2,2,2,2,2,2,2,2,2,2,2,2,2,2,2,2,2,2,2,2,2,2,
2,2,2,2,2,2,2,2,2,4),(0.921990538769251,0.922095714747312,0.954066959065241,
0.956951359949483,0.967811963590554,0.969592959807857,0.970671362648303,
0.971512220070758,0.972469925098997,0.974139718874511,0.981423336962385,
0.996687786089568,1.03626819204048,1.04089393363255,1.04273409733647,1.04426345407392,
1.04583149900183,1.0481293137838,1.05434765110521,1.08523431900078,1.11156122215719,
1.11493993802917,1.11625022294177,1.11704114865964,1.1179037117141,1.11913647685773,
1.12226774003668,1.138391386666,1.16660570962418,1.18407355713843,1.1871119728053,
1.18902303553471,1.19052433179077,1.19219720289691,1.1949776762486,1.20556384066999,
1.23969399347116,1.25922201751933,1.26140358689794,1.26246874595402,1.26330657907497,
1.26428510865692,1.2660501378811,1.2748395746389,1.31438580228374,1.31890257055696,
1.33060486333009,1.33357315738072,1.3353046884915,1.33679855930986,1.33862286541939,
1.34210601138453,1.36931958415441,1.39901068159224,1.40586936074096,1.40756671848025,
1.40854049621983,1.4093787857176,1.41045038567129,1.4126648696164,1.41558769301656,
1.42279167537777,1.45471099869009,1.4756146086433,1.47875571621069,1.48067677673975,
1.48218315387718,1.48383331875828,1.48651146728239,1.49597306370812,1.51256421488705,
1.53646255770429,1.55103584297068,1.55311760970949,1.55417665570773,1.55501393149779,
1.55599674841249,1.55778195653453,1.56694195061446,1.61175814102968,1.62248041990789,
1.62535976877521,1.62707059765008,1.62856583555445,1.63041648189668,1.63402848051207,
1.66610736196892,1.6951366279121,1.69840673501729,1.69970258802717,1.70056077746854,
1.70141992685552,1.70268965000434,1.70416224813143,1.7233984861634,1.74484585204786,
1.76723107794458,1.77040721009391,1.77233844050999,1.77384604614888,1.77549071054097,
1.77814469949125,1.78736208417325,1.80332027201119,1.83991647277704,1.84332409142739),
 .UNSPECIFIED.);
#1455=B_SPLINE_CURVE_WITH_KNOTS('',3,(#88642,#88643,#88644,#88645,#88646,
#88647,#88648,#88649,#88650,#88651,#88652,#88653,#88654,#88655,#88656,#88657,
#88658,#88659,#88660,#88661,#88662,#88663,#88664,#88665,#88666,#88667,#88668,
#88669,#88670,#88671,#88672,#88673,#88674,#88675,#88676,#88677,#88678,#88679,
#88680,#88681,#88682,#88683,#88684,#88685,#88686,#88687,#88688,#88689,#88690,
#88691,#88692,#88693,#88694,#88695,#88696,#88697,#88698,#88699,#88700,#88701,
#88702,#88703,#88704,#88705,#88706,#88707,#88708,#88709,#88710,#88711,#88712,
#88713,#88714,#88715,#88716,#88717,#88718,#88719,#88720,#88721,#88722,#88723,
#88724,#88725,#88726,#88727,#88728,#88729,#88730,#88731,#88732,#88733,#88734,
#88735,#88736,#88737,#88738,#88739,#88740,#88741,#88742,#88743,#88744,#88745,
#88746,#88747,#88748,#88749,#88750,#88751,#88752,#88753,#88754,#88755,#88756,
#88757,#88758,#88759,#88760,#88761,#88762,#88763,#88764,#88765,#88766,#88767,
#88768,#88769,#88770,#88771,#88772,#88773,#88774,#88775,#88776,#88777,#88778,
#88779,#88780,#88781,#88782,#88783,#88784,#88785,#88786,#88787,#88788,#88789,
#88790,#88791,#88792,#88793,#88794,#88795,#88796,#88797,#88798,#88799,#88800,
#88801,#88802,#88803,#88804,#88805,#88806,#88807,#88808,#88809,#88810,#88811,
#88812,#88813,#88814,#88815,#88816,#88817,#88818,#88819,#88820,#88821,#88822,
#88823,#88824,#88825,#88826,#88827,#88828,#88829,#88830,#88831,#88832,#88833,
#88834,#88835,#88836,#88837,#88838,#88839,#88840,#88841,#88842,#88843,#88844,
#88845,#88846,#88847,#88848,#88849,#88850,#88851,#88852,#88853,#88854,#88855,
#88856,#88857,#88858,#88859,#88860,#88861,#88862,#88863,#88864,#88865,#88866,
#88867,#88868,#88869),.UNSPECIFIED.,.F.,.F.,(4,2,2,2,2,2,2,2,2,2,2,2,2,
2,2,2,2,2,2,2,2,2,2,2,2,2,2,2,2,2,2,2,2,2,2,2,2,2,2,2,2,2,2,2,2,2,2,2,2,
2,2,2,2,2,2,2,2,2,2,2,2,2,2,2,2,2,2,2,2,2,2,2,2,2,2,2,2,2,2,2,2,2,2,2,2,
2,2,2,2,2,2,2,2,2,2,2,2,2,2,2,2,2,2,2,2,2,2,2,2,2,2,2,2,4),(0.922179861339329,
0.922305856265592,0.948358510328141,0.952471061589414,0.960057621900698,
0.961812599274569,0.962799615103655,0.963636667678953,0.964690587806809,
0.966815796791742,0.990242684552143,1.02785755058805,1.03261781327026,1.03453079875911,
1.03593889508962,1.03746584191979,1.03955078738963,1.04440870119828,1.06591590573847,
1.08588201402429,1.10529634706939,1.10747729341786,1.10854227211977,1.10938001991263,
1.11035849728518,1.11212353476405,1.12091481754642,1.16047210605452,1.16499180419956,
1.17669761125749,1.17966535219894,1.18139666135297,1.18289039691978,1.18471460416134,
1.18819774795401,1.21541593730762,1.2451114789543,1.25197835099754,1.2536763194092,
1.25465018452638,1.25548837095895,1.2565595886586,1.25877241890841,1.26169250881564,
1.26880617547408,1.30007185789791,1.32170910461652,1.32486827489585,1.32679458168917,
1.32830157689105,1.32994885606631,1.33261435486327,1.3419470979786,1.35820130365542,
1.38587320479266,1.39735432297528,1.39916106055838,1.40024688647809,1.40108845891231,
1.40204119731707,1.40368914947989,1.41067542785987,1.42495008116317,1.42943758368689,
1.46528075985601,1.47019886469861,1.47213831365025,1.47355296170009,1.4750747485341,
1.47713091099572,1.48182454587331,1.5019514764184,1.53197077249725,1.53459822760856,
1.54346465885915,1.54514421681024,1.5462035211316,1.54704072643429,1.54802312341557,
1.54980669905122,1.55893855784719,1.60327143654874,1.61444340938124,1.61736501374219,
1.61908547640894,1.62057964540784,1.62241681993276,1.62596378018616,1.6599767204213,
1.68708910933584,1.69044493580093,1.69175123085083,1.69254119999579,1.69338662910514,
1.69458300141436,1.69595131864392,1.69838545976789,1.71975572404526,1.75729822192961,
1.76206257494683,1.76397584026046,1.76538365933871,1.76690984135475,1.7689929087563,
1.77384262506732,1.79528699039251,1.83071308178169,1.83583772328696,1.8373827581069,
1.83831255036784,1.83912037044699,1.83995194488624,1.8410514131662,1.84370654451412),
 .UNSPECIFIED.);
#1456=B_SPLINE_CURVE_WITH_KNOTS('',3,(#88870,#88871,#88872,#88873),
 .UNSPECIFIED.,.F.,.F.,(4,4),(0.000555968474940145,0.000580235344661419),
 .UNSPECIFIED.);
#1457=B_SPLINE_CURVE_WITH_KNOTS('',3,(#88875,#88876,#88877,#88878),
 .UNSPECIFIED.,.F.,.F.,(4,4),(1.84332409142739,1.84334992990566),
 .UNSPECIFIED.);
#1458=B_SPLINE_CURVE_WITH_KNOTS('',3,(#88879,#88880,#88881,#88882,#88883,
#88884,#88885,#88886,#88887,#88888,#88889,#88890,#88891,#88892,#88893,#88894,
#88895,#88896,#88897,#88898,#88899,#88900,#88901,#88902,#88903,#88904,#88905,
#88906,#88907,#88908,#88909,#88910,#88911,#88912,#88913,#88914,#88915,#88916,
#88917,#88918,#88919,#88920,#88921,#88922,#88923,#88924,#88925,#88926,#88927,
#88928,#88929,#88930,#88931,#88932,#88933,#88934,#88935,#88936,#88937,#88938,
#88939,#88940,#88941,#88942,#88943,#88944,#88945,#88946,#88947,#88948,#88949,
#88950,#88951,#88952,#88953,#88954,#88955,#88956,#88957,#88958,#88959,#88960,
#88961,#88962,#88963,#88964,#88965,#88966,#88967,#88968,#88969,#88970,#88971,
#88972,#88973,#88974,#88975,#88976,#88977,#88978,#88979,#88980,#88981,#88982,
#88983,#88984,#88985,#88986,#88987,#88988,#88989,#88990,#88991,#88992,#88993,
#88994,#88995,#88996,#88997,#88998,#88999,#89000,#89001,#89002,#89003,#89004,
#89005,#89006,#89007,#89008,#89009,#89010,#89011,#89012,#89013,#89014,#89015,
#89016,#89017,#89018,#89019,#89020,#89021,#89022,#89023,#89024,#89025,#89026,
#89027,#89028,#89029,#89030,#89031,#89032,#89033,#89034,#89035,#89036,#89037,
#89038,#89039,#89040,#89041,#89042,#89043,#89044,#89045,#89046,#89047,#89048,
#89049,#89050,#89051,#89052,#89053,#89054,#89055,#89056,#89057,#89058,#89059,
#89060,#89061,#89062,#89063,#89064,#89065,#89066,#89067,#89068,#89069,#89070,
#89071,#89072,#89073,#89074,#89075,#89076,#89077,#89078,#89079,#89080,#89081,
#89082,#89083,#89084,#89085,#89086,#89087,#89088,#89089,#89090,#89091,#89092,
#89093,#89094,#89095,#89096,#89097,#89098,#89099,#89100,#89101,#89102,#89103,
#89104),.UNSPECIFIED.,.F.,.F.,(4,2,2,2,2,2,2,2,2,2,2,2,2,2,2,2,2,2,2,2,
2,2,2,2,2,2,2,2,2,2,2,2,2,2,2,2,2,2,2,2,2,2,2,2,2,2,2,2,2,2,2,2,2,2,2,2,
2,2,2,2,2,2,2,2,2,2,2,2,2,2,2,2,2,2,2,2,2,2,2,2,2,2,2,2,2,2,2,2,2,2,2,2,
2,2,2,2,2,2,2,2,2,2,2,2,2,2,2,2,2,2,2,2,4),(0.000558997173511017,0.00118482932324078,
0.00213421037112796,0.00296734761077362,0.00377422552920924,0.00458612664028208,
0.00600328572722705,0.0101047151419729,0.0499071472742641,0.0687509441811788,
0.0732860597346557,0.0753142545984871,0.0768316688740968,0.0782540592719929,
0.0802227984831767,0.0853180886060037,0.117978450357613,0.135225524452579,
0.142596710507808,0.145590045548383,0.147172427392033,0.148196450562901,
0.149149832051276,0.149957577827412,0.151012024863666,0.152675300869839,
0.161257720930523,0.192808992350366,0.216360670874264,0.219771331470604,
0.221580502378189,0.222928673605137,0.224620195985398,0.227485572994004,
0.237699113643811,0.28307311271274,0.292265224587159,0.294052346625034,
0.295035683625365,0.29587307375244,0.296931850412204,0.299011849248387,
0.313228411725894,0.32192560895474,0.339700225554792,0.360195866723772,
0.364934239562936,0.366998639521996,0.368522200395972,0.369935427239762,
0.371868157818852,0.376744432904364,0.413080927379175,0.430403285379708,
0.438263649441004,0.439972597159422,0.440938956990164,0.44177844179225,
0.44286148795803,0.444619045202413,0.454988911676274,0.468911596175963,
0.506079850619068,0.510828502862542,0.512894703262471,0.514418575931632,
0.515831371050421,0.517762392583832,0.522628581453398,0.559083053245657,
0.576326495362742,0.581545280923769,0.5850076798281,0.586290481428787,0.587163146112699,
0.587944538923776,0.589203378250332,0.592272158372798,0.624596620718649,
0.653883098486395,0.657394639692195,0.659225003737515,0.660575529111487,
0.662252712200261,0.665052391168854,0.674622328163887,0.720733300802602,
0.729967378695579,0.731756932043072,0.732740887696176,0.733578366533266,
0.734636696281846,0.736783353185639,0.752769023714274,0.779480604171151,
0.798235249906596,0.802759705631013,0.804786311058138,0.806303795753107,
0.807727167355917,0.80969872078133,0.814809762884154,0.847079575981986,
0.867316992227833,0.875907090064295,0.877660935188146,0.878637156507913,
0.879475434636893,0.880544289616095,0.882254529009274,0.891673459689964,
0.921986581853743,0.922114039327125),.UNSPECIFIED.);
#1459=B_SPLINE_CURVE_WITH_KNOTS('',3,(#89109,#89110,#89111,#89112,#89113,
#89114,#89115,#89116,#89117,#89118,#89119,#89120,#89121,#89122,#89123,#89124,
#89125,#89126,#89127,#89128,#89129,#89130,#89131,#89132,#89133,#89134,#89135,
#89136,#89137,#89138,#89139,#89140,#89141,#89142,#89143,#89144,#89145,#89146,
#89147,#89148,#89149,#89150,#89151,#89152,#89153,#89154,#89155,#89156,#89157,
#89158,#89159,#89160,#89161,#89162,#89163,#89164,#89165,#89166,#89167,#89168,
#89169,#89170,#89171,#89172,#89173,#89174,#89175,#89176,#89177,#89178,#89179,
#89180,#89181,#89182,#89183,#89184,#89185,#89186,#89187,#89188,#89189,#89190,
#89191,#89192,#89193,#89194,#89195,#89196,#89197,#89198,#89199,#89200,#89201,
#89202,#89203,#89204,#89205,#89206,#89207,#89208,#89209,#89210,#89211,#89212,
#89213,#89214,#89215,#89216,#89217,#89218,#89219,#89220,#89221,#89222,#89223,
#89224,#89225,#89226,#89227,#89228,#89229,#89230,#89231,#89232,#89233,#89234,
#89235,#89236,#89237,#89238,#89239,#89240,#89241,#89242,#89243,#89244,#89245,
#89246,#89247,#89248,#89249,#89250,#89251,#89252,#89253,#89254,#89255,#89256,
#89257,#89258,#89259,#89260,#89261,#89262,#89263,#89264,#89265,#89266,#89267,
#89268,#89269,#89270,#89271,#89272,#89273,#89274,#89275,#89276,#89277,#89278,
#89279,#89280,#89281,#89282,#89283,#89284,#89285,#89286,#89287,#89288,#89289,
#89290,#89291,#89292,#89293,#89294,#89295,#89296,#89297,#89298,#89299,#89300,
#89301,#89302,#89303,#89304,#89305,#89306,#89307,#89308,#89309,#89310,#89311,
#89312,#89313,#89314,#89315,#89316,#89317,#89318,#89319,#89320,#89321,#89322,
#89323,#89324,#89325,#89326,#89327,#89328,#89329,#89330,#89331,#89332,#89333,
#89334,#89335,#89336,#89337,#89338),.UNSPECIFIED.,.F.,.F.,(4,2,2,2,2,2,
2,2,2,2,2,2,2,2,2,2,2,2,2,2,2,2,2,2,2,2,2,2,2,2,2,2,2,2,2,2,2,2,2,2,2,2,
2,2,2,2,2,2,2,2,2,2,2,2,2,2,2,2,2,2,2,2,2,2,2,2,2,2,2,2,2,2,2,2,2,2,2,2,
2,2,2,2,2,2,2,2,2,2,2,2,2,2,2,2,2,2,2,2,2,2,2,2,2,2,2,2,2,2,2,2,2,2,2,2,
4),(0.000619400602369933,0.00919608380241888,0.0114757258341164,0.0130852337262251,
0.0144846605649322,0.0159937718795114,0.0179350564357408,0.022114236926196,
0.032031337510015,0.0624021120980362,0.0775989411366287,0.0848628546610285,
0.0865309563306177,0.0874881414695774,0.0883288305791964,0.0894073768571555,
0.0911893428924231,0.10206266955029,0.104991085741233,0.14435892336912,
0.151829607439505,0.155434572654819,0.157591370624042,0.159540601878171,
0.161024931277541,0.162451405275953,0.164831134417604,0.171102925614037,
0.208640876783377,0.223586868379027,0.230776472957122,0.232439230065579,
0.233395219437834,0.2342361054806,0.235316500447613,0.237104806172868,0.248135269445715,
0.251504598009287,0.277703873985716,0.300587409916543,0.303980957542119,
0.305786379850709,0.307265175533071,0.309006593252569,0.312018646113224,
0.324316932097665,0.328354201485825,0.367710139799065,0.376483397917154,
0.378247276673065,0.379225450016874,0.380063143578499,0.381128324899813,
0.383310579784424,0.404976144596082,0.434025501880801,0.447215797656127,
0.450191516252336,0.451907188438811,0.453402150641002,0.455246650255673,
0.458067838523388,0.471532547064675,0.513410537352359,0.522378940464121,
0.524153805453075,0.5251344104456,0.525971930927403,0.527034000333089,0.52920031942802,
0.546975894543856,0.572144314686801,0.590668106169812,0.595162823306987,
0.597183726938314,0.598699971185129,0.600124383781581,0.602100892286698,
0.607245577550293,0.638161720593932,0.647374159833474,0.661533690456628,
0.668485319846315,0.670130821667723,0.671083096507633,0.671924898523636,
0.673011854756539,0.674822217352027,0.686389561780758,0.713977024023634,
0.738224311746537,0.741651456337512,0.743464088741333,0.744812599207838,
0.746501622000406,0.749355633228877,0.759450426431562,0.764306768158382,
0.805280098387922,0.814182389041639,0.815953707955983,0.816933594006844,
0.817771264592479,0.818834504714592,0.821006448222701,0.839293883884213,
0.861414731154785,0.876657580204402,0.885592712470732,0.888218790759248,
0.889857595021026,0.891367528195395,0.893312446747319,0.896534221967008,
0.922179861339329),.UNSPECIFIED.);
#1460=B_SPLINE_CURVE_WITH_KNOTS('',3,(#89339,#89340,#89341,#89342,#89343,
#89344,#89345,#89346,#89347,#89348,#89349,#89350,#89351,#89352,#89353,#89354,
#89355,#89356,#89357,#89358,#89359,#89360,#89361,#89362,#89363,#89364,#89365,
#89366,#89367,#89368,#89369,#89370,#89371,#89372,#89373,#89374,#89375,#89376,
#89377,#89378,#89379,#89380,#89381,#89382,#89383,#89384,#89385,#89386,#89387,
#89388,#89389,#89390,#89391,#89392,#89393,#89394,#89395,#89396,#89397,#89398,
#89399,#89400,#89401,#89402,#89403,#89404,#89405,#89406,#89407,#89408,#89409,
#89410,#89411,#89412,#89413,#89414,#89415,#89416,#89417,#89418,#89419,#89420,
#89421,#89422,#89423,#89424,#89425,#89426,#89427,#89428,#89429,#89430,#89431,
#89432,#89433,#89434,#89435,#89436,#89437,#89438,#89439,#89440,#89441,#89442,
#89443,#89444,#89445,#89446,#89447,#89448,#89449,#89450,#89451,#89452,#89453,
#89454,#89455,#89456,#89457,#89458,#89459,#89460,#89461,#89462,#89463,#89464,
#89465,#89466,#89467,#89468,#89469,#89470,#89471,#89472,#89473,#89474,#89475,
#89476,#89477,#89478,#89479,#89480,#89481,#89482,#89483,#89484,#89485,#89486,
#89487,#89488,#89489,#89490,#89491,#89492,#89493,#89494,#89495,#89496,#89497,
#89498,#89499,#89500,#89501,#89502,#89503,#89504,#89505,#89506,#89507,#89508,
#89509,#89510,#89511,#89512,#89513,#89514,#89515,#89516,#89517,#89518,#89519,
#89520,#89521,#89522,#89523,#89524,#89525,#89526,#89527,#89528,#89529,#89530,
#89531,#89532,#89533,#89534,#89535,#89536,#89537,#89538,#89539,#89540,#89541,
#89542,#89543,#89544,#89545,#89546,#89547,#89548,#89549,#89550,#89551,#89552,
#89553,#89554,#89555,#89556,#89557,#89558,#89559,#89560,#89561,#89562),
 .UNSPECIFIED.,.F.,.F.,(4,2,2,2,2,2,2,2,2,2,2,2,2,2,2,2,2,2,2,2,2,2,2,2,
2,2,2,2,2,2,2,2,2,2,2,2,2,2,2,2,2,2,2,2,2,2,2,2,2,2,2,2,2,2,2,2,2,2,2,2,
2,2,2,2,2,2,2,2,2,2,2,2,2,2,2,2,2,2,2,2,2,2,2,2,2,2,2,2,2,2,2,2,2,2,2,2,
2,2,2,2,2,2,2,2,2,2,2,2,2,2,2,4),(0.922114039327125,0.945624226091696,0.948827213167595,
0.950766787910697,0.95227615166331,0.953917940417018,0.956556719896715,
0.965614224239166,0.98116202678807,1.01246585172647,1.02157084447469,1.02326409805016,
1.02432779940373,1.02516565711389,1.02614557025996,1.02791648355293,1.03680686138869,
1.07761456210416,1.09211817122803,1.09500593533567,1.09687116432286,1.09836805222302,
1.10006978317618,1.10298076015325,1.11522531876594,1.16043282024345,1.16774194722377,
1.16947654246819,1.17045901437327,1.17129662955524,1.17235692037406,1.17451339722148,
1.20075664048657,1.23511087100066,1.24012967632635,1.24208630216522,1.24350574076812,
1.24502542543749,1.24706607401043,1.25166932296381,1.2710526267236,1.30131640882227,
1.31318239624137,1.31500435576094,1.31609483207024,1.31693724471554,1.31788782455129,
1.31952506759398,1.32636376376929,1.34016140203455,1.35787370072324,1.38330156871137,
1.38652234062216,1.38846710080209,1.38997718922515,1.3916164452091,1.39424387758119,
1.4031901839883,1.41845886950231,1.43190817195468,1.45693337690098,1.46033498341433,
1.46164908933463,1.46244082570776,1.46330290638594,1.46453269474231,1.46764433395997,
1.49732463428851,1.52663891927665,1.5317955332396,1.53399368124589,1.53552637060039,
1.53709081954051,1.53937046727338,1.5454611581662,1.57234146806514,1.60308991959664,
1.60629536538627,1.60757714090552,1.60836274426424,1.60923062516734,1.61049000287245,
1.61379392792179,1.63174562065282,1.636085479537,1.67300778850469,1.67783363694066,
1.67975784583906,1.68116889339814,1.68266345697938,1.68466973481214,1.68690709750569,
1.69070946107611,1.71941683777152,1.74891025369856,1.75216760867964,1.7534581787459,
1.75424541769429,1.75511159462619,1.75636249846862,1.75961058599429,1.77695656433478,
1.80811934078148,1.81789037217457,1.82341798093191,1.82567704400571,1.82708129752298,
1.82850450734555,1.82999540875606,1.83196472933021,1.83647854077429,1.84364195192957),
 .UNSPECIFIED.);
#1461=B_SPLINE_CURVE_WITH_KNOTS('',3,(#89568,#89569,#89570,#89571,#89572,
#89573,#89574,#89575,#89576,#89577,#89578,#89579,#89580,#89581,#89582,#89583,
#89584,#89585,#89586,#89587,#89588,#89589,#89590,#89591,#89592,#89593,#89594,
#89595,#89596,#89597,#89598,#89599,#89600,#89601,#89602,#89603,#89604,#89605,
#89606,#89607,#89608,#89609,#89610,#89611,#89612,#89613,#89614,#89615,#89616,
#89617,#89618,#89619,#89620,#89621,#89622,#89623,#89624,#89625,#89626,#89627,
#89628,#89629,#89630,#89631,#89632,#89633,#89634,#89635,#89636,#89637,#89638,
#89639,#89640,#89641,#89642,#89643,#89644,#89645,#89646,#89647,#89648,#89649,
#89650,#89651,#89652,#89653,#89654,#89655,#89656,#89657,#89658,#89659,#89660,
#89661,#89662,#89663,#89664,#89665,#89666,#89667,#89668,#89669,#89670,#89671,
#89672,#89673,#89674,#89675,#89676,#89677,#89678,#89679,#89680,#89681,#89682,
#89683,#89684,#89685,#89686,#89687,#89688,#89689,#89690,#89691,#89692,#89693,
#89694,#89695,#89696,#89697,#89698,#89699,#89700,#89701,#89702,#89703,#89704,
#89705,#89706,#89707,#89708,#89709,#89710,#89711,#89712,#89713,#89714,#89715,
#89716,#89717,#89718,#89719,#89720,#89721,#89722,#89723,#89724,#89725,#89726,
#89727,#89728,#89729,#89730,#89731,#89732,#89733,#89734,#89735,#89736,#89737,
#89738,#89739,#89740,#89741,#89742,#89743,#89744,#89745,#89746,#89747,#89748,
#89749,#89750,#89751,#89752,#89753,#89754,#89755,#89756,#89757,#89758,#89759,
#89760,#89761,#89762,#89763,#89764,#89765,#89766,#89767,#89768,#89769,#89770,
#89771,#89772,#89773,#89774,#89775,#89776,#89777,#89778,#89779,#89780,#89781,
#89782,#89783),.UNSPECIFIED.,.F.,.F.,(4,2,2,2,2,2,2,2,2,2,2,2,2,2,2,2,2,
2,2,2,2,2,2,2,2,2,2,2,2,2,2,2,2,2,2,2,2,2,2,2,2,2,2,2,2,2,2,2,2,2,2,2,2,
2,2,2,2,2,2,2,2,2,2,2,2,2,2,2,2,2,2,2,2,2,2,2,2,2,2,2,2,2,2,2,2,2,2,2,2,
2,2,2,2,2,2,2,2,2,2,2,2,2,2,2,2,2,2,4),(0.921789712209714,0.969516972442617,
0.977663339138593,0.98030092688334,0.981941991943733,0.983450697723574,
0.985422434348305,0.989651431407274,1.00615278638608,1.03785913539119,1.04089646410054,
1.04775715836731,1.05261563440904,1.05412981322882,1.05505282476476,1.05590305395752,
1.0570678273355,1.05978746378977,1.07203033675686,1.10037080861799,1.12195989480259,
1.12511780720191,1.12704370160843,1.12855058745357,1.13019796401356,1.13286410403104,
1.14220414903906,1.15847764038684,1.18594699705429,1.19758809187558,1.19940103590949,
1.20048865537482,1.2013304224424,1.20228202611142,1.20392495737164,1.21084464147499,
1.22490386165016,1.23738994994271,1.26775655083843,1.27094342005437,1.27287782464316,
1.27438589890923,1.27602904006446,1.27867606162792,1.28782295291143,1.30359975283607,
1.33543111750219,1.34375461335686,1.34540221447486,1.34645177873384,1.34728837377195,
1.34827836932085,1.35009716687256,1.35991693227439,1.38447052606481,1.41357562985581,
1.41678799606442,1.41872987235136,1.42023901628632,1.42187854239438,1.42450923567496,
1.43349440273658,1.44886245267503,1.47682714120374,1.48925133127379,1.49126955204612,
1.49231487256587,1.49315122052713,1.49414462176963,1.49597937228689,1.50613467520886,
1.5343491410549,1.55943177379842,1.5626412378287,1.56458222624065,1.56609119464961,
1.56773104676413,1.57036339632274,1.57936548273834,1.59477627473829,1.62381683074958,
1.63517331849145,1.63697493135469,1.63805919866253,1.63890050656631,1.63985401801396,
1.64150574026862,1.64854454731483,1.66299183048334,1.69836402112731,1.70686349647,
1.70954327597369,1.7111935317762,1.71264536435632,1.71452935021861,1.71659050619125,
1.71996237934712,1.72676402910598,1.74567363976231,1.77712948827864,1.78191009300749,
1.78341478036209,1.78433560656666,1.78518656065515,1.78635622180276,1.78910466453662,
1.80160047464782,1.84316778997506),.UNSPECIFIED.);
#1462=B_SPLINE_CURVE_WITH_KNOTS('',3,(#89784,#89785,#89786,#89787),
 .UNSPECIFIED.,.F.,.F.,(4,4),(0.000539904033087321,0.000619400602369933),
 .UNSPECIFIED.);
#1463=B_SPLINE_CURVE_WITH_KNOTS('',3,(#89789,#89790,#89791,#89792),
 .UNSPECIFIED.,.F.,.F.,(4,4),(1.84364195192957,1.84371903373639),
 .UNSPECIFIED.);
#1464=B_SPLINE_CURVE_WITH_KNOTS('',3,(#89793,#89794,#89795,#89796,#89797,
#89798,#89799,#89800,#89801,#89802,#89803,#89804,#89805,#89806,#89807,#89808,
#89809,#89810,#89811,#89812,#89813,#89814,#89815,#89816,#89817,#89818,#89819,
#89820,#89821,#89822,#89823,#89824,#89825,#89826,#89827,#89828,#89829,#89830,
#89831,#89832,#89833,#89834,#89835,#89836,#89837,#89838,#89839,#89840,#89841,
#89842,#89843,#89844,#89845,#89846,#89847,#89848,#89849,#89850,#89851,#89852,
#89853,#89854,#89855,#89856,#89857,#89858,#89859,#89860,#89861,#89862,#89863,
#89864,#89865,#89866,#89867,#89868,#89869,#89870,#89871,#89872,#89873,#89874,
#89875,#89876,#89877,#89878,#89879,#89880,#89881,#89882,#89883,#89884,#89885,
#89886,#89887,#89888,#89889,#89890,#89891,#89892,#89893,#89894,#89895,#89896,
#89897,#89898,#89899,#89900,#89901,#89902,#89903,#89904,#89905,#89906,#89907,
#89908,#89909,#89910,#89911,#89912,#89913,#89914,#89915,#89916,#89917,#89918,
#89919,#89920,#89921,#89922,#89923,#89924,#89925,#89926,#89927,#89928,#89929,
#89930,#89931,#89932,#89933,#89934,#89935,#89936,#89937,#89938,#89939,#89940,
#89941,#89942,#89943,#89944,#89945,#89946,#89947,#89948,#89949,#89950,#89951,
#89952,#89953,#89954,#89955,#89956,#89957,#89958,#89959,#89960,#89961,#89962,
#89963,#89964,#89965,#89966,#89967,#89968,#89969,#89970,#89971,#89972,#89973,
#89974,#89975,#89976,#89977,#89978,#89979,#89980,#89981,#89982,#89983,#89984,
#89985,#89986,#89987,#89988,#89989,#89990,#89991,#89992,#89993,#89994,#89995,
#89996,#89997,#89998,#89999,#90000,#90001,#90002,#90003,#90004),
 .UNSPECIFIED.,.F.,.F.,(4,2,2,2,2,2,2,2,2,2,2,2,2,2,2,2,2,2,2,2,2,2,2,2,
2,2,2,2,2,2,2,2,2,2,2,2,2,2,2,2,2,2,2,2,2,2,2,2,2,2,2,2,2,2,2,2,2,2,2,2,
2,2,2,2,2,2,2,2,2,2,2,2,2,2,2,2,2,2,2,2,2,2,2,2,2,2,2,2,2,2,2,2,2,2,2,2,
2,2,2,2,2,2,2,2,2,4),(0.000533489402586898,0.00397323680534875,0.0450333008082084,
0.0539418411053825,0.0557137595300517,0.056693902620216,0.0575317523610931,
0.0585951874530287,0.0607674367854684,0.0830439982009745,0.111619081738958,
0.120239360693202,0.124230807004118,0.127429296934491,0.129169560833597,
0.130525137239771,0.132226947218926,0.135137666476426,0.145819993136191,
0.19068803890273,0.199852633535366,0.20163865270645,0.202621919678572,0.203459577841137,
0.204519111964732,0.206198411437829,0.215048351287394,0.24661592413807,
0.262200294062169,0.271271785411787,0.273912177051211,0.275554436616223,
0.277063875151419,0.27900304801765,0.282204274750429,0.311416513620761,
0.335887361997227,0.345692028790184,0.347510771624519,0.348501087103721,
0.34933816373541,0.350388623340007,0.352038181978138,0.360383549382576,
0.363199267196655,0.363475251828812,0.393650528935288,0.413775552405436,
0.418469745328183,0.420526662715693,0.422049208562541,0.423464704578996,
0.425783436093726,0.431662420042453,0.469630780813025,0.484662715424888,
0.491879054254956,0.493544390366178,0.494501294783121,0.49534261352143,
0.496423107518798,0.4982106451861,0.509205696583877,0.511730426493795,0.540834664335965,
0.559884502852041,0.564446383613359,0.566479881656849,0.567998637114707,
0.569420382840689,0.57177202267251,0.577868671527939,0.628203211064114,
0.637634008862099,0.639434289901172,0.640420768144195,0.641258348674152,
0.642314204333238,0.643981027453988,0.652612140878818,0.696826390533408,
0.708672631895328,0.711554932428218,0.713250689886008,0.714748899817381,
0.716624459510588,0.719544900341177,0.734616558799752,0.7748370878581,0.783682368437372,
0.785451084588931,0.786430684444065,0.787268828320787,0.788333610964954,
0.790511839375826,0.809397958946926,0.844119637683016,0.851167052438432,
0.856233481611442,0.858354303975419,0.859888198561486,0.861289382925383,
0.863172869886759,0.86775866705016,0.906923387391549,0.922374656735376),
 .UNSPECIFIED.);
#1465=B_SPLINE_CURVE_WITH_KNOTS('',3,(#90010,#90011,#90012,#90013),
 .UNSPECIFIED.,.F.,.F.,(4,4),(1.84368667532253,1.8438184773998),
 .UNSPECIFIED.);
#1466=B_SPLINE_CURVE_WITH_KNOTS('',3,(#90014,#90015,#90016,#90017,#90018,
#90019,#90020,#90021,#90022,#90023,#90024,#90025,#90026,#90027,#90028,#90029,
#90030,#90031,#90032,#90033,#90034,#90035,#90036,#90037,#90038,#90039,#90040,
#90041,#90042,#90043,#90044,#90045,#90046,#90047,#90048,#90049,#90050,#90051,
#90052,#90053,#90054,#90055,#90056,#90057,#90058,#90059,#90060,#90061,#90062,
#90063,#90064,#90065,#90066,#90067,#90068,#90069,#90070,#90071,#90072,#90073,
#90074,#90075,#90076,#90077,#90078,#90079,#90080,#90081,#90082,#90083,#90084,
#90085,#90086,#90087,#90088,#90089,#90090,#90091,#90092,#90093,#90094,#90095,
#90096,#90097,#90098,#90099,#90100,#90101,#90102,#90103,#90104,#90105,#90106,
#90107,#90108,#90109,#90110,#90111,#90112,#90113,#90114,#90115,#90116,#90117,
#90118,#90119,#90120,#90121,#90122,#90123,#90124,#90125,#90126,#90127,#90128,
#90129,#90130,#90131,#90132,#90133,#90134,#90135,#90136,#90137,#90138,#90139,
#90140,#90141,#90142,#90143,#90144,#90145,#90146,#90147,#90148,#90149,#90150,
#90151,#90152,#90153,#90154,#90155,#90156,#90157,#90158,#90159,#90160,#90161,
#90162,#90163,#90164,#90165,#90166,#90167,#90168,#90169,#90170,#90171,#90172,
#90173,#90174,#90175,#90176,#90177,#90178,#90179,#90180,#90181,#90182,#90183,
#90184,#90185,#90186,#90187,#90188,#90189,#90190,#90191,#90192,#90193,#90194,
#90195,#90196,#90197,#90198,#90199,#90200,#90201,#90202,#90203,#90204,#90205,
#90206,#90207,#90208,#90209,#90210,#90211,#90212,#90213,#90214,#90215,#90216,
#90217,#90218,#90219,#90220,#90221,#90222,#90223,#90224,#90225,#90226,#90227,
#90228,#90229,#90230,#90231,#90232,#90233,#90234,#90235,#90236,#90237,#90238,
#90239,#90240,#90241,#90242,#90243,#90244,#90245,#90246,#90247,#90248,#90249),
 .UNSPECIFIED.,.F.,.F.,(4,2,2,2,2,2,2,2,2,2,2,2,2,2,2,2,2,2,2,2,2,2,2,2,
2,2,2,2,2,2,2,2,2,2,2,2,2,2,2,2,2,2,2,2,2,2,2,2,2,2,2,2,2,2,2,2,2,2,2,2,
2,2,2,2,2,2,2,2,2,2,2,2,2,2,2,2,2,2,2,2,2,2,2,2,2,2,2,2,2,2,2,2,2,2,2,2,
2,2,2,2,2,2,2,2,2,2,2,2,2,2,2,2,2,2,2,2,2,4),(0.000428601095637824,0.0290350720482551,
0.0310841819515501,0.0327551988883566,0.0337130083902071,0.0345535502786231,
0.035631019808094,0.0374093868099898,0.0481615772158818,0.052273716103244,
0.0633512603638037,0.0779198501948231,0.0939925952084204,0.102368644220221,
0.104285408891655,0.10609096576465,0.107569831301646,0.109311284196931,
0.112323280422703,0.124619526983771,0.128663680243591,0.151709828378808,
0.168993846101592,0.176832292301315,0.178505195061469,0.179484114210167,
0.180321684728525,0.181385730962344,0.183562411614655,0.202405249323511,
0.237148968204392,0.244197114676824,0.249263233919308,0.251383143293465,
0.252916089687658,0.254316207588198,0.256197956259698,0.260777985643243,
0.299949942379356,0.315453627400328,0.322807234262837,0.324481682479458,
0.325440275484734,0.32628072187121,0.327357070578448,0.329131545820094,
0.339831722679084,0.370663704004278,0.390652070736079,0.395328681362214,
0.397381885791505,0.398903211540054,0.400318661621551,0.402261132942787,
0.407197060087205,0.44278754201314,0.46062088966577,0.468615690863605,0.470332910568821,
0.471300903210197,0.472139846870594,0.473219614828353,0.47496680066878,
0.485129051628043,0.515401408395332,0.5363681559274,0.541162094246406,0.543235818247271,
0.544760642467246,0.54617107159134,0.548093835201716,0.552912888917977,
0.589890950744903,0.606790729815376,0.614536808700958,0.616237974443752,
0.617202464867521,0.618041958229898,0.619127139038517,0.620892333209406,
0.631423872921794,0.634149845871044,0.662979035413663,0.682509765140976,
0.687130445788821,0.689173827656646,0.690693595391687,0.692111701775473,
0.694064267219357,0.699060487314966,0.733771606940388,0.752221611976676,
0.760375272421964,0.762102516929666,0.76307273267756,0.763911419005878,
0.764988011738607,0.76672453738627,0.776666919767031,0.782267392838599,
0.805552082362621,0.830236133881733,0.833672823773881,0.835487424329227,
0.836836098482247,0.838523634673806,0.841371031067518,0.851398146492318,
0.857491623107137,0.897392444028762,0.906210872114216,0.907977458172426,
0.908956294707278,0.909794037565089,0.910858615021977,0.91255519161423,
0.921724077110065,0.921789712209714),.UNSPECIFIED.);
#1467=B_SPLINE_CURVE_WITH_KNOTS('',3,(#90251,#90252,#90253,#90254,#90255,
#90256,#90257,#90258,#90259,#90260,#90261,#90262,#90263,#90264,#90265,#90266,
#90267,#90268,#90269,#90270,#90271,#90272,#90273,#90274,#90275,#90276,#90277,
#90278,#90279,#90280,#90281,#90282,#90283,#90284,#90285,#90286,#90287,#90288,
#90289,#90290,#90291,#90292,#90293,#90294,#90295,#90296,#90297,#90298,#90299,
#90300,#90301,#90302,#90303,#90304,#90305,#90306,#90307,#90308,#90309,#90310,
#90311,#90312,#90313,#90314,#90315,#90316,#90317,#90318,#90319,#90320,#90321,
#90322,#90323,#90324,#90325,#90326,#90327,#90328,#90329,#90330,#90331,#90332,
#90333,#90334,#90335,#90336,#90337,#90338,#90339,#90340,#90341,#90342,#90343,
#90344,#90345,#90346,#90347,#90348,#90349,#90350,#90351,#90352,#90353,#90354,
#90355,#90356,#90357,#90358,#90359,#90360,#90361,#90362,#90363,#90364,#90365,
#90366,#90367,#90368,#90369,#90370,#90371,#90372,#90373,#90374,#90375,#90376,
#90377,#90378,#90379,#90380,#90381,#90382,#90383,#90384,#90385,#90386,#90387,
#90388,#90389,#90390,#90391,#90392,#90393,#90394,#90395,#90396,#90397,#90398,
#90399,#90400,#90401,#90402,#90403,#90404,#90405,#90406,#90407,#90408,#90409,
#90410,#90411,#90412,#90413,#90414,#90415,#90416,#90417,#90418,#90419,#90420,
#90421,#90422,#90423,#90424,#90425,#90426,#90427,#90428,#90429,#90430,#90431,
#90432,#90433,#90434,#90435,#90436,#90437,#90438,#90439,#90440,#90441,#90442,
#90443,#90444,#90445,#90446,#90447,#90448,#90449,#90450,#90451,#90452,#90453,
#90454,#90455,#90456,#90457,#90458,#90459,#90460,#90461,#90462,#90463,#90464,
#90465,#90466,#90467,#90468,#90469,#90470,#90471,#90472,#90473,#90474,#90475,
#90476),.UNSPECIFIED.,.F.,.F.,(4,2,2,2,2,2,2,2,2,2,2,2,2,2,2,2,2,2,2,2,
2,2,2,2,2,2,2,2,2,2,2,2,2,2,2,2,2,2,2,2,2,2,2,2,2,2,2,2,2,2,2,2,2,2,2,2,
2,2,2,2,2,2,2,2,2,2,2,2,2,2,2,2,2,2,2,2,2,2,2,2,2,2,2,2,2,2,2,2,2,2,2,2,
2,2,2,2,2,2,2,2,2,2,2,2,2,2,2,2,2,2,2,2,4),(0.922374656735376,0.922441678336817,
0.929669563352342,0.931398013497983,0.932379245701514,0.933133327485008,
0.934154377021716,0.936117662869169,0.949668511573435,0.978599913803431,
0.99950309319788,1.00264567689765,1.00456774062369,1.00607496506275,1.007726120093,
1.01040601455546,1.01987525904208,1.03648178654763,1.05246817701862,1.07486147229562,
1.07703546006387,1.07809937797505,1.07893743104844,1.07991760135824,1.08168905123686,
1.09058365373482,1.13142881373052,1.14590925157162,1.14879591706687,1.15066103985426,
1.15215823534679,1.15386074058017,1.15677409968098,1.1690450573802,1.2066866730778,
1.21011190129153,1.22111804185858,1.22290600999143,1.22398663716322,1.22482797849294,
1.2257848066074,1.22744978901483,1.23466086729284,1.24967651901599,1.28754670880767,
1.29353421236312,1.29586917817801,1.29728772594104,1.298808304525,1.30085337778138,
1.30548053531504,1.32505477851414,1.35276125107147,1.35599530990382,1.36702217182252,
1.36881091548896,1.36989172870319,1.37073303810518,1.37168962811205,1.37335373326487,
1.3805537965296,1.39553306347069,1.43323279119158,1.43937922786553,1.44173875298288,
1.44316187486993,1.44467953756059,1.44670715268892,1.45123713180544,1.47003328032966,
1.49710674954745,1.51266765250984,1.51480640888025,1.51586315992757,1.51670053763647,
1.51768570748545,1.51948087626994,1.52882112663116,1.57702007751937,1.58482029049405,
1.58741496865909,1.58904682755785,1.590559000198,1.5925527638141,1.59689857919281,
1.61427073157841,1.6503870241433,1.65907731127102,1.66074876059535,1.66180574475427,
1.66264300101881,1.66362767121947,1.66542101950393,1.67462109717352,1.69767869170011,
1.72320023579086,1.73074654846158,1.73330840509739,1.7349330898852,1.73644793990468,
1.73845911607361,1.742703335404,1.76176944885827,1.77710430862767,1.80254111148967,
1.80594173691123,1.80725558217838,1.80804719634072,1.80890917573716,1.81013887279834,
1.81153304103024,1.81688352078661,1.84386758684803),.UNSPECIFIED.);
#1468=B_SPLINE_CURVE_WITH_KNOTS('',3,(#90477,#90478,#90479,#90480),
 .UNSPECIFIED.,.F.,.F.,(4,4),(0.000437250149454394,0.000569891382468709),
 .UNSPECIFIED.);
#1469=B_SPLINE_CURVE_WITH_KNOTS('',3,(#90485,#90486,#90487,#90488,#90489,
#90490,#90491,#90492,#90493,#90494,#90495,#90496,#90497,#90498,#90499,#90500,
#90501,#90502,#90503,#90504,#90505,#90506,#90507,#90508,#90509,#90510,#90511,
#90512,#90513,#90514,#90515,#90516,#90517,#90518,#90519,#90520,#90521,#90522,
#90523,#90524,#90525,#90526,#90527,#90528,#90529,#90530,#90531,#90532,#90533,
#90534,#90535,#90536,#90537,#90538,#90539,#90540,#90541,#90542,#90543,#90544,
#90545,#90546,#90547,#90548,#90549,#90550,#90551,#90552,#90553,#90554,#90555,
#90556,#90557,#90558,#90559,#90560,#90561,#90562,#90563,#90564,#90565,#90566,
#90567,#90568,#90569,#90570,#90571,#90572,#90573,#90574,#90575,#90576,#90577,
#90578,#90579,#90580,#90581,#90582,#90583,#90584,#90585,#90586,#90587,#90588,
#90589,#90590,#90591,#90592,#90593,#90594,#90595,#90596,#90597,#90598,#90599,
#90600,#90601,#90602,#90603,#90604,#90605,#90606,#90607,#90608,#90609,#90610,
#90611,#90612,#90613,#90614,#90615,#90616,#90617,#90618,#90619,#90620,#90621,
#90622,#90623,#90624,#90625,#90626,#90627,#90628,#90629,#90630,#90631,#90632,
#90633,#90634,#90635,#90636,#90637,#90638,#90639,#90640,#90641,#90642,#90643,
#90644,#90645,#90646,#90647,#90648,#90649,#90650,#90651,#90652,#90653,#90654,
#90655,#90656,#90657,#90658,#90659,#90660,#90661,#90662,#90663,#90664,#90665,
#90666,#90667,#90668,#90669,#90670,#90671,#90672,#90673,#90674,#90675,#90676,
#90677,#90678,#90679,#90680,#90681,#90682,#90683,#90684,#90685,#90686,#90687,
#90688,#90689,#90690,#90691,#90692,#90693,#90694,#90695,#90696,#90697,#90698,
#90699,#90700,#90701,#90702,#90703,#90704,#90705,#90706,#90707,#90708,#90709,
#90710,#90711,#90712),.UNSPECIFIED.,.F.,.F.,(4,2,2,2,2,2,2,2,2,2,2,2,2,
2,2,2,2,2,2,2,2,2,2,2,2,2,2,2,2,2,2,2,2,2,2,2,2,2,2,2,2,2,2,2,2,2,2,2,2,
2,2,2,2,2,2,2,2,2,2,2,2,2,2,2,2,2,2,2,2,2,2,2,2,2,2,2,2,2,2,2,2,2,2,2,2,
2,2,2,2,2,2,2,2,2,2,2,2,2,2,2,2,2,2,2,2,2,2,2,2,2,2,2,2,4),(0.922237918268933,
0.926191380517241,0.928119136273235,0.929622265718532,0.931285630671642,
0.934023493063675,0.944125402861637,0.962454933641687,0.991889074968301,
0.999075909855535,1.00080040965521,1.00178039749423,1.00261796873746,1.00368084370519,
1.0058512515426,1.03270699473906,1.06637721632002,1.07143241105219,1.07339463166143,
1.07481525079866,1.0763335103127,1.07836757148888,1.08293592137179,1.10204291116039,
1.1315854070021,1.13445517732235,1.14463158888902,1.14638195575269,1.14746269654295,
1.1483017540574,1.14926914126989,1.15098353319044,1.15893311426642,1.17659485078496,
1.21246334268913,1.21737983272704,1.21931906276357,1.22073369826865,1.22225561069733,
1.22431218795711,1.22900784980099,1.24915062863753,1.27901742982362,1.29041927107787,
1.2922228579389,1.29330776575634,1.29414923112743,1.29510253520903,1.29675302271267,
1.30377338419188,1.31815923966033,1.34839826012403,1.3613316449532,1.36439084658745,
1.36614305909745,1.36748649037184,1.36922488470512,1.37230492781941,1.38721768321407,
1.42297123686884,1.42539232928606,1.43633239314308,1.43811689464082,1.43919620642788,
1.44003700860903,1.44099376058001,1.44265982786119,1.449894473333,1.46499328388894,
1.50325668840128,1.50886886276059,1.51114173453244,1.51254819335221,1.51407588306873,
1.5161663824848,1.52105817626358,1.54286212948439,1.57254396029178,1.58232286539809,
1.58405106567852,1.58512508976432,1.58596345918923,1.5869352271435,1.58866990840903,
1.59694670305082,1.61589018058861,1.64993240861968,1.65496655955894,1.65692521533157,
1.6583447912648,1.6598633719341,1.66190035739807,1.66633367998342,1.67235653071594,
1.68801302370398,1.71216513777381,1.72781247307564,1.72995298528613,1.73100976777579,
1.73184675312409,1.73283095715545,1.73387720794681,1.73794425893755,1.75494459842043,
1.77044323174245,1.77166507438393,1.7981109293864,1.80133484956356,1.80328007860033,
1.80478967806922,1.80642754540642,1.80905086815995,1.81212690020928,1.84368667532253),
 .UNSPECIFIED.);
#1470=B_SPLINE_CURVE_WITH_KNOTS('',3,(#90713,#90714,#90715,#90716,#90717,
#90718,#90719,#90720,#90721,#90722,#90723,#90724,#90725,#90726,#90727,#90728,
#90729,#90730,#90731,#90732,#90733,#90734,#90735,#90736,#90737,#90738,#90739,
#90740,#90741,#90742,#90743,#90744,#90745,#90746,#90747,#90748,#90749,#90750,
#90751,#90752,#90753,#90754,#90755,#90756,#90757,#90758,#90759,#90760,#90761,
#90762,#90763,#90764,#90765,#90766,#90767,#90768,#90769,#90770,#90771,#90772,
#90773,#90774,#90775,#90776,#90777,#90778,#90779,#90780,#90781,#90782,#90783,
#90784,#90785,#90786,#90787,#90788,#90789,#90790,#90791,#90792,#90793,#90794,
#90795,#90796,#90797,#90798,#90799,#90800,#90801,#90802,#90803,#90804,#90805,
#90806,#90807,#90808,#90809,#90810,#90811,#90812,#90813,#90814,#90815,#90816,
#90817,#90818,#90819,#90820,#90821,#90822,#90823,#90824,#90825,#90826,#90827,
#90828,#90829,#90830,#90831,#90832,#90833,#90834,#90835,#90836,#90837,#90838,
#90839,#90840,#90841,#90842,#90843,#90844,#90845,#90846,#90847,#90848,#90849,
#90850,#90851,#90852,#90853,#90854,#90855,#90856,#90857,#90858,#90859,#90860,
#90861,#90862,#90863,#90864,#90865,#90866,#90867,#90868,#90869,#90870,#90871,
#90872,#90873,#90874,#90875,#90876,#90877,#90878,#90879,#90880,#90881,#90882,
#90883,#90884,#90885,#90886,#90887,#90888,#90889,#90890,#90891,#90892,#90893,
#90894,#90895,#90896,#90897,#90898,#90899,#90900,#90901,#90902,#90903,#90904,
#90905,#90906,#90907,#90908,#90909,#90910,#90911,#90912,#90913,#90914,#90915,
#90916,#90917,#90918,#90919,#90920,#90921,#90922,#90923,#90924,#90925,#90926,
#90927,#90928,#90929,#90930,#90931,#90932,#90933,#90934,#90935,#90936,#90937,
#90938,#90939,#90940,#90941,#90942,#90943,#90944),.UNSPECIFIED.,.F.,.F.,
(4,2,2,2,2,2,2,2,2,2,2,2,2,2,2,2,2,2,2,2,2,2,2,2,2,2,2,2,2,2,2,2,2,2,2,
2,2,2,2,2,2,2,2,2,2,2,2,2,2,2,2,2,2,2,2,2,2,2,2,2,2,2,2,2,2,2,2,2,2,2,2,
2,2,2,2,2,2,2,2,2,2,2,2,2,2,2,2,2,2,2,2,2,2,2,2,2,2,2,2,2,2,2,2,2,2,2,2,
2,2,2,2,2,2,2,2,4),(0.000569891382468709,0.0234211215008631,0.0315171806116301,
0.0339709507313322,0.0356514811228152,0.0372904855016129,0.0388005311631058,
0.0407454991466058,0.043967164020376,0.0697359704180957,0.0844820296529836,
0.0988428121560535,0.107481436198876,0.109244982890933,0.110223230805987,
0.11106115406743,0.112126860457267,0.114310981263468,0.134638951409163,
0.164053319859173,0.177676762169647,0.18081673796223,0.182638142610473,
0.184132090598205,0.185866480323286,0.188846498971669,0.200717047092492,
0.233131063805651,0.246781920501471,0.253574678304614,0.255208327210515,
0.256158076276057,0.257000604441232,0.25809234348391,0.259918760145209,
0.271906743243061,0.297193090713906,0.314735376428027,0.324552159824207,
0.32726429947459,0.328922186055001,0.330426968953316,0.332366108330506,
0.335497373125117,0.356011549494214,0.390892671955947,0.399248465929993,
0.400988356283973,0.401961488635483,0.402800056497892,0.403873093279465,
0.405597333071729,0.415288666826581,0.421307420759307,0.448587327955876,
0.46741073454005,0.471943738532229,0.473971810494902,0.475489457928112,
0.476912302909234,0.479270763592592,0.485411497540558,0.523098540317878,
0.538070497887251,0.545268612143073,0.546932467540542,0.547888956264438,
0.54873019972848,0.549810968446364,0.551599725619324,0.562628340190154,
0.566012356347143,0.592202465961849,0.615086289528182,0.618480922763481,
0.620287048494713,0.621766488939377,0.623508750029304,0.62652248439948,
0.638831970114233,0.642841142841366,0.673063236989276,0.688919668413057,
0.692025151299668,0.693254012674242,0.69411595522706,0.694907964105746,
0.696223316119934,0.699632375081228,0.723790847739265,0.745670453589918,
0.75606487262287,0.760619041201492,0.764212010330671,0.766059312856068,
0.767554986933282,0.769269763017668,0.772163961525809,0.783036015483478,
0.786952820842268,0.827943342067928,0.83684703368413,0.838618769265589,
0.839598912949456,0.840436825921643,0.841500421755409,0.843673265471758,
0.862012533910661,0.897195178130637,0.904288691818974,0.909380527776448,
0.911505336825534,0.913039741168961,0.91443976540244,0.916674648209001,
0.922012310475654),.UNSPECIFIED.);
#1471=B_SPLINE_CURVE_WITH_KNOTS('',3,(#90949,#90950,#90951,#90952,#90953,
#90954,#90955,#90956,#90957,#90958,#90959,#90960,#90961,#90962,#90963,#90964,
#90965,#90966,#90967,#90968,#90969,#90970,#90971,#90972,#90973,#90974,#90975,
#90976,#90977,#90978,#90979,#90980,#90981,#90982,#90983,#90984,#90985,#90986,
#90987,#90988,#90989,#90990,#90991,#90992,#90993,#90994,#90995,#90996,#90997,
#90998,#90999,#91000,#91001,#91002,#91003,#91004,#91005,#91006,#91007,#91008,
#91009,#91010,#91011,#91012,#91013,#91014,#91015,#91016,#91017,#91018,#91019,
#91020,#91021,#91022,#91023,#91024,#91025,#91026,#91027,#91028,#91029,#91030,
#91031,#91032,#91033,#91034,#91035,#91036,#91037,#91038,#91039,#91040,#91041,
#91042,#91043,#91044,#91045,#91046,#91047,#91048,#91049,#91050,#91051,#91052,
#91053,#91054,#91055,#91056,#91057,#91058,#91059,#91060,#91061,#91062,#91063,
#91064,#91065,#91066,#91067,#91068,#91069,#91070,#91071,#91072,#91073,#91074,
#91075,#91076,#91077,#91078,#91079,#91080,#91081,#91082,#91083,#91084,#91085,
#91086,#91087,#91088,#91089,#91090,#91091,#91092,#91093,#91094,#91095,#91096,
#91097,#91098,#91099,#91100,#91101,#91102,#91103,#91104,#91105,#91106,#91107,
#91108,#91109,#91110,#91111,#91112,#91113,#91114,#91115,#91116,#91117,#91118,
#91119,#91120,#91121,#91122,#91123,#91124,#91125,#91126,#91127,#91128,#91129,
#91130,#91131,#91132,#91133,#91134,#91135,#91136,#91137,#91138,#91139,#91140,
#91141,#91142,#91143,#91144,#91145,#91146,#91147,#91148,#91149,#91150,#91151,
#91152,#91153,#91154,#91155,#91156,#91157,#91158,#91159,#91160,#91161,#91162,
#91163,#91164,#91165,#91166,#91167,#91168,#91169,#91170,#91171,#91172,#91173,
#91174,#91175,#91176),.UNSPECIFIED.,.F.,.F.,(4,2,2,2,2,2,2,2,2,2,2,2,2,
2,2,2,2,2,2,2,2,2,2,2,2,2,2,2,2,2,2,2,2,2,2,2,2,2,2,2,2,2,2,2,2,2,2,2,2,
2,2,2,2,2,2,2,2,2,2,2,2,2,2,2,2,2,2,2,2,2,2,2,2,2,2,2,2,2,2,2,2,2,2,2,2,
2,2,2,2,2,2,2,2,2,2,2,2,2,2,2,2,2,2,2,2,2,2,2,2,2,2,2,2,4),(0.000603157058436499,
0.0242728015901372,0.0455242222249288,0.0503514875987475,0.0524308860125723,
0.0539566101115037,0.0553655701855657,0.0572827886299263,0.0620694707013623,
0.099379775291639,0.102545358965389,0.116838533857367,0.121490824014618,
0.123655519389192,0.125362449551318,0.126333778083171,0.126337691211615,
0.126341651433116,0.126345659551442,0.126349716391369,0.126353822850078,
0.127190990917063,0.128249684223656,0.1299272293033,0.138757312345306,0.17100292461915,
0.191533483353917,0.196275389841045,0.198339976075251,0.199863153369347,
0.201275652089698,0.203206804707063,0.20807605831657,0.244489499537873,
0.261761562072419,0.269607877709756,0.271315508305104,0.27228137131579,
0.273120578558098,0.274203448618717,0.275961068058469,0.286340350187178,
0.295183586668706,0.319507365454128,0.337806469474444,0.342272235850673,
0.344287741411451,0.345802988305927,0.347228696031453,0.349603969183966,
0.355847514036339,0.393426364216901,0.408374808841762,0.41556538462058,
0.417228312338521,0.418184391169677,0.419025350140752,0.42010583143647,
0.421894264863799,0.432924996460801,0.436108066989557,0.462487116587213,
0.485382382099437,0.488776478899617,0.49058211151842,0.492061037907891,
0.493802561074966,0.496814675384872,0.509111350805791,0.513155866981549,
0.552511676599832,0.56128540280106,0.563049418113686,0.564027672791934,
0.564865439480634,0.565930718254876,0.568113187653535,0.589866027533524,
0.606707473900117,0.631220901665064,0.634654020888471,0.63646792445505,
0.63796134282706,0.639701503609759,0.642707298657573,0.654917462954403,
0.659006768372456,0.698416368541185,0.707194991925221,0.708959386853598,
0.709937772186992,0.710775601288849,0.711840895797125,0.713539763905891,
0.722749965942763,0.76637228426485,0.778163385065766,0.781040511201531,
0.782734564429488,0.784232083904403,0.786107854793001,0.789030688848387,
0.804167326361854,0.844313480092512,0.853151338136041,0.854918979493543,
0.855898028664477,0.85673572349562,0.857799944438683,0.859495394901204,
0.868644171644638,0.899312640430864,0.92219364149957,0.922237918268933),
 .UNSPECIFIED.);
#1472=B_SPLINE_CURVE_WITH_KNOTS('',3,(#91177,#91178,#91179,#91180,#91181,
#91182,#91183,#91184,#91185,#91186,#91187,#91188,#91189,#91190,#91191,#91192,
#91193,#91194,#91195,#91196,#91197,#91198,#91199,#91200,#91201,#91202,#91203,
#91204,#91205,#91206,#91207,#91208,#91209,#91210,#91211,#91212,#91213,#91214,
#91215,#91216,#91217,#91218,#91219,#91220,#91221,#91222,#91223,#91224,#91225,
#91226,#91227,#91228,#91229,#91230,#91231,#91232,#91233,#91234,#91235,#91236,
#91237,#91238,#91239,#91240,#91241,#91242,#91243,#91244,#91245,#91246,#91247,
#91248,#91249,#91250,#91251,#91252,#91253,#91254,#91255,#91256,#91257,#91258,
#91259,#91260,#91261,#91262,#91263,#91264,#91265,#91266,#91267,#91268,#91269,
#91270,#91271,#91272,#91273,#91274,#91275,#91276,#91277,#91278,#91279,#91280,
#91281,#91282,#91283,#91284,#91285,#91286,#91287,#91288,#91289,#91290,#91291,
#91292,#91293,#91294,#91295,#91296,#91297,#91298,#91299,#91300,#91301,#91302,
#91303,#91304,#91305,#91306,#91307,#91308,#91309,#91310,#91311,#91312,#91313,
#91314,#91315,#91316,#91317,#91318,#91319,#91320,#91321,#91322,#91323,#91324,
#91325,#91326,#91327,#91328,#91329,#91330,#91331,#91332,#91333,#91334,#91335,
#91336,#91337,#91338,#91339,#91340,#91341,#91342,#91343,#91344,#91345,#91346,
#91347,#91348,#91349,#91350,#91351,#91352,#91353,#91354,#91355,#91356,#91357,
#91358,#91359,#91360,#91361,#91362,#91363,#91364,#91365,#91366,#91367,#91368,
#91369,#91370,#91371,#91372,#91373,#91374,#91375,#91376,#91377,#91378,#91379,
#91380,#91381,#91382,#91383,#91384,#91385,#91386,#91387,#91388),
 .UNSPECIFIED.,.F.,.F.,(4,2,2,2,2,2,2,2,2,2,2,2,2,2,2,2,2,2,2,2,2,2,2,2,
2,2,2,2,2,2,2,2,2,2,2,2,2,2,2,2,2,2,2,2,2,2,2,2,2,2,2,2,2,2,2,2,2,2,2,2,
2,2,2,2,2,2,2,2,2,2,2,2,2,2,2,2,2,2,2,2,2,2,2,2,2,2,2,2,2,2,2,2,2,2,2,2,
2,2,2,2,2,2,2,2,2,4),(0.922012310475654,0.922053808326363,0.949455824714825,
0.980528444692292,0.983719999894429,0.984999548071363,0.985784813757977,
0.986653290540001,0.987915201678888,0.991235277550237,1.00936229902265,
1.02659807552285,1.05246100582919,1.05568386392365,1.05762934388777,1.05913967148792,
1.06077886681035,1.06340550166928,1.07234219378278,1.08758610019145,1.10790122412403,
1.12793654730576,1.13012047774734,1.13118624408529,1.13202429074506,1.13300276475955,
1.13476693373777,1.14353620666142,1.18282372255295,1.18701135371279,1.19926325525754,
1.20227256744914,1.20401374016723,1.2055074236171,1.20732090411564,1.21075098030214,
1.23511516870443,1.26178250415154,1.27406222930179,1.27589897747276,1.27699375435078,
1.277836710955,1.27878477472938,1.28041071672016,1.2871030386372,1.30043974824966,
1.32188474872857,1.34428388675028,1.34746139161366,1.34939342081783,1.35090162854341,
1.35254692800404,1.35520189353604,1.3644221744581,1.3803847460207,1.41098684208453,
1.42016999933871,1.4218674950582,1.42293244928709,1.42377035632849,1.42474924379045,
1.42651559610713,1.4353258366773,1.47511925967412,1.48066672649061,1.49126351871709,
1.49416583012754,1.49586560599262,1.49721294531379,1.49901153509807,1.50237131992824,
1.52402543071296,1.54909326115857,1.56560408614993,1.56775704018537,1.56881650574999,
1.5696539166194,1.57063666359216,1.57242116588277,1.5815646331395,1.62609006279349,
1.63708222855347,1.63998684703158,1.64170365505979,1.64319855322547,1.64504162642632,
1.64861591268507,1.68205919800277,1.7097092430882,1.71304962887461,1.71435359723089,
1.71514325641996,1.71593506806637,1.71709792995239,1.71978491699447,1.72358547575521,
1.73404962440439,1.77554765578889,1.78356984827116,1.78619213296712,1.78782984969521,
1.78933965012658,1.79131888859957,1.79558781985974,1.8123854668724,1.84347475602747),
 .UNSPECIFIED.);
#1473=B_SPLINE_CURVE_WITH_KNOTS('',3,(#91394,#91395,#91396,#91397,#91398,
#91399,#91400,#91401,#91402,#91403,#91404,#91405,#91406,#91407,#91408,#91409,
#91410,#91411,#91412,#91413,#91414,#91415,#91416,#91417,#91418,#91419,#91420,
#91421,#91422,#91423,#91424,#91425,#91426,#91427,#91428,#91429,#91430,#91431,
#91432,#91433,#91434,#91435,#91436,#91437,#91438,#91439,#91440,#91441,#91442,
#91443,#91444,#91445,#91446,#91447,#91448,#91449,#91450,#91451,#91452,#91453,
#91454,#91455,#91456,#91457,#91458,#91459,#91460,#91461,#91462,#91463,#91464,
#91465,#91466,#91467,#91468,#91469,#91470,#91471,#91472,#91473,#91474,#91475,
#91476,#91477,#91478,#91479,#91480,#91481,#91482,#91483,#91484,#91485,#91486,
#91487,#91488,#91489,#91490,#91491,#91492,#91493,#91494,#91495,#91496,#91497,
#91498,#91499,#91500,#91501,#91502,#91503,#91504,#91505,#91506,#91507,#91508,
#91509,#91510,#91511,#91512,#91513,#91514,#91515,#91516,#91517,#91518,#91519,
#91520,#91521,#91522,#91523,#91524,#91525,#91526,#91527,#91528,#91529,#91530,
#91531,#91532,#91533,#91534,#91535,#91536,#91537,#91538,#91539,#91540,#91541,
#91542,#91543,#91544,#91545,#91546,#91547,#91548,#91549,#91550,#91551,#91552,
#91553,#91554,#91555,#91556,#91557,#91558,#91559,#91560,#91561,#91562,#91563,
#91564,#91565,#91566,#91567,#91568,#91569,#91570,#91571,#91572,#91573,#91574,
#91575,#91576,#91577,#91578,#91579,#91580,#91581,#91582,#91583,#91584,#91585,
#91586,#91587,#91588,#91589,#91590,#91591,#91592,#91593,#91594,#91595,#91596,
#91597,#91598,#91599,#91600,#91601,#91602,#91603,#91604,#91605,#91606,#91607,
#91608,#91609,#91610,#91611,#91612,#91613,#91614,#91615,#91616,#91617,#91618,
#91619,#91620,#91621,#91622,#91623,#91624,#91625),.UNSPECIFIED.,.F.,.F.,
(4,2,2,2,2,2,2,2,2,2,2,2,2,2,2,2,2,2,2,2,2,2,2,2,2,2,2,2,2,2,2,2,2,2,2,
2,2,2,2,2,2,2,2,2,2,2,2,2,2,2,2,2,2,2,2,2,2,2,2,2,2,2,2,2,2,2,2,2,2,2,2,
2,2,2,2,2,2,2,2,2,2,2,2,2,2,2,2,2,2,2,2,2,2,2,2,2,2,2,2,2,2,2,2,2,2,2,2,
2,2,2,2,2,2,2,2,4),(0.92220090061974,0.922325888116382,0.929171380658707,
0.944910417814658,0.947051038261568,0.948108072843558,0.9489453561298,0.949930025013108,
0.951723270745192,0.961029923508041,1.00850138698254,1.01692383708755,1.01959486903211,
1.02124341671153,1.02275014578737,1.02470660615659,1.02885412891554,1.06167680520233,
1.08454191506249,1.09155920700789,1.09326982510087,1.09424661867011,1.09508450525561,
1.09615170321977,1.09834400459525,1.12278401280386,1.15909034657558,1.16397128534812,
1.16590452490943,1.16731764096164,1.16884062117056,1.17090341854495,1.17563445618998,
1.19607034499369,1.22334825821511,1.22615479033711,1.23702743095864,1.23881000275399,
1.23988873981184,1.2407294656659,1.24168655535469,1.2433541876858,1.25061099521239,
1.2657850321197,1.30444229493087,1.30969707579691,1.31191120450844,1.31330702704867,
1.31484397478946,1.31698560842737,1.32218328021569,1.32946848222614,1.35061032612254,
1.38098904106956,1.38421493273134,1.38549987882817,1.38628586935009,1.3871527072722,
1.38840803044897,1.39168695864234,1.40937080414152,1.43029035384477,1.45302481649981,
1.45620900610413,1.45814262711265,1.45965059411416,1.46129412730463,1.46394290542258,
1.47310732126338,1.48892877731242,1.52056293615756,1.52900419925148,1.53065889680903,
1.53171063039138,1.53254735199949,1.53353561931391,1.53534637627702,1.54500308550315,
1.56875537706158,1.59886558841991,1.60206399916757,1.60400178310818,1.60551033163413,
1.60715181224644,1.60979136027428,1.61886395583434,1.63445222451569,1.66213694960228,
1.67451803689323,1.67653467489069,1.67757965379503,1.67841598574851,1.67938969775886,
1.68114884599781,1.68336741545605,1.68818380798208,1.70329560238921,1.74164518418991,
1.7471787445908,1.74943825888756,1.75084218494262,1.75237167034521,1.75447287499963,
1.75942825667814,1.78179040117797,1.80000504732398,1.80787176689765,1.81270722073954,
1.82075949869818,1.82239019564568,1.82343451635495,1.82427074015814,1.82506598874869,
1.8260479410353,1.82752872464318,1.84359018605298),.UNSPECIFIED.);
#1474=B_SPLINE_CURVE_WITH_KNOTS('',3,(#91626,#91627,#91628,#91629),
 .UNSPECIFIED.,.F.,.F.,(4,4),(0.000504233101903366,0.000603157058436499),
 .UNSPECIFIED.);
#1475=B_SPLINE_CURVE_WITH_KNOTS('',3,(#91631,#91632,#91633,#91634),
 .UNSPECIFIED.,.F.,.F.,(4,4),(1.84347475602747,1.84357418596773),
 .UNSPECIFIED.);
#1476=B_SPLINE_CURVE_WITH_KNOTS('',3,(#91635,#91636,#91637,#91638,#91639,
#91640,#91641,#91642,#91643,#91644,#91645,#91646,#91647,#91648,#91649,#91650,
#91651,#91652,#91653,#91654,#91655,#91656,#91657,#91658,#91659,#91660,#91661,
#91662,#91663,#91664,#91665,#91666,#91667,#91668,#91669,#91670,#91671,#91672,
#91673,#91674,#91675,#91676,#91677,#91678,#91679,#91680,#91681,#91682,#91683,
#91684,#91685,#91686,#91687,#91688,#91689,#91690,#91691,#91692,#91693,#91694,
#91695,#91696,#91697,#91698,#91699,#91700,#91701,#91702,#91703,#91704,#91705,
#91706,#91707,#91708,#91709,#91710,#91711,#91712,#91713,#91714,#91715,#91716,
#91717,#91718,#91719,#91720,#91721,#91722,#91723,#91724,#91725,#91726,#91727,
#91728,#91729,#91730,#91731,#91732,#91733,#91734,#91735,#91736,#91737,#91738,
#91739,#91740,#91741,#91742,#91743,#91744,#91745,#91746,#91747,#91748,#91749,
#91750,#91751,#91752,#91753,#91754,#91755,#91756,#91757,#91758,#91759,#91760,
#91761,#91762,#91763,#91764,#91765,#91766,#91767,#91768,#91769,#91770,#91771,
#91772,#91773,#91774,#91775,#91776,#91777,#91778,#91779,#91780,#91781,#91782,
#91783,#91784,#91785,#91786,#91787,#91788,#91789,#91790,#91791,#91792,#91793,
#91794,#91795,#91796,#91797,#91798,#91799,#91800,#91801,#91802,#91803,#91804,
#91805,#91806,#91807,#91808,#91809,#91810,#91811,#91812,#91813,#91814,#91815,
#91816,#91817,#91818,#91819,#91820,#91821,#91822,#91823,#91824,#91825,#91826,
#91827,#91828,#91829,#91830,#91831,#91832,#91833,#91834,#91835,#91836,#91837,
#91838,#91839,#91840,#91841,#91842,#91843,#91844,#91845,#91846,#91847,#91848,
#91849,#91850,#91851,#91852,#91853,#91854,#91855,#91856,#91857,#91858,#91859,
#91860,#91861,#91862,#91863,#91864),.UNSPECIFIED.,.F.,.F.,(4,2,2,2,2,2,
2,2,2,2,2,2,2,2,2,2,2,2,2,2,2,2,2,2,2,2,2,2,2,2,2,2,2,2,2,2,2,2,2,2,2,2,
2,2,2,2,2,2,2,2,2,2,2,2,2,2,2,2,2,2,2,2,2,2,2,2,2,2,2,2,2,2,2,2,2,2,2,2,
2,2,2,2,2,2,2,2,2,2,2,2,2,2,2,2,2,2,2,2,2,2,2,2,2,2,2,2,2,2,2,2,2,2,2,2,
4),(0.000514367078856413,0.0145491834342173,0.0159723333821196,0.0169307456053303,
0.0177208162106002,0.0185598473094828,0.0196386025654595,0.0213819679780018,
0.0314599034020634,0.0384405059200993,0.0640065293208735,0.0831024169649428,
0.0876694908409809,0.0897036020698978,0.0912221463529332,0.0926432104126621,
0.0946063324042943,0.0996655295224006,0.133196328624006,0.139827735978584,
0.154048280886289,0.158686042382176,0.160846107346323,0.162569295973232,
0.163534594088163,0.164371878264975,0.165428474660188,0.167566792227759,
0.192354390306657,0.211287190609083,0.229185364956923,0.233599982327971,
0.235606533211473,0.237120772034357,0.238747545335732,0.241318523352881,
0.248933555089244,0.290869300131118,0.3049240147517,0.307844798036407,0.309043863488256,
0.309900263008358,0.310699438675858,0.311825761227252,0.314843824875668,
0.347587392027096,0.367248803133798,0.377812096025181,0.380590910569084,
0.382263573116883,0.383765182632549,0.385677330502464,0.388718823848285,
0.406280457836509,0.434283339279588,0.450490326151363,0.453630094275619,
0.454864289627471,0.455727214292652,0.456517971226011,0.457826992779143,
0.461197307826611,0.487877340014091,0.518431063279376,0.524668383519615,
0.526969068294142,0.528537832201057,0.530066934633274,0.531905633552078,
0.536521459514119,0.576165623906971,0.591380580461383,0.598650417277672,
0.600319344936863,0.601276926423549,0.602117918338552,0.603196814428242,
0.604979287975413,0.615852269783709,0.61877549619381,0.621522709073118,
0.650263236054138,0.662498474932574,0.667598427435381,0.671529708301216,
0.673444797452557,0.674946765474791,0.676617813094535,0.679389225609711,
0.688693882009756,0.735114611881829,0.74436597440058,0.74615658066323,0.747140827492345,
0.747978378994018,0.749036577115915,0.751182240392891,0.767116820935144,
0.796235179698225,0.813027418718856,0.81729643654,0.819276302815579,0.820786825935832,
0.822425564493073,0.825050006188704,0.83308285832759,0.881000615253691,
0.890327880790218,0.892122683501165,0.893107931706556,0.893945542452374,
0.895002805086352,0.897143294078358,0.921919804481415,0.922044868712354),
 .UNSPECIFIED.);
#1477=B_SPLINE_CURVE_WITH_KNOTS('',3,(#91869,#91870,#91871,#91872,#91873,
#91874,#91875,#91876,#91877,#91878,#91879,#91880,#91881,#91882,#91883,#91884,
#91885,#91886,#91887,#91888,#91889,#91890,#91891,#91892,#91893,#91894,#91895,
#91896,#91897,#91898,#91899,#91900,#91901,#91902,#91903,#91904,#91905,#91906,
#91907,#91908,#91909,#91910,#91911,#91912,#91913,#91914,#91915,#91916,#91917,
#91918,#91919,#91920,#91921,#91922,#91923,#91924,#91925,#91926,#91927,#91928,
#91929,#91930,#91931,#91932,#91933,#91934,#91935,#91936,#91937,#91938,#91939,
#91940,#91941,#91942,#91943,#91944,#91945,#91946,#91947,#91948,#91949,#91950,
#91951,#91952,#91953,#91954,#91955,#91956,#91957,#91958,#91959,#91960,#91961,
#91962,#91963,#91964,#91965,#91966,#91967,#91968,#91969,#91970,#91971,#91972,
#91973,#91974,#91975,#91976,#91977,#91978,#91979,#91980,#91981,#91982,#91983,
#91984,#91985,#91986,#91987,#91988,#91989,#91990,#91991,#91992,#91993,#91994,
#91995,#91996,#91997,#91998,#91999,#92000,#92001,#92002,#92003,#92004,#92005,
#92006,#92007,#92008,#92009,#92010,#92011,#92012,#92013,#92014,#92015,#92016,
#92017,#92018,#92019,#92020,#92021,#92022,#92023,#92024,#92025,#92026,#92027,
#92028,#92029,#92030,#92031,#92032,#92033,#92034,#92035,#92036,#92037,#92038,
#92039,#92040,#92041,#92042,#92043,#92044,#92045,#92046,#92047,#92048,#92049,
#92050,#92051,#92052,#92053,#92054,#92055,#92056,#92057,#92058,#92059,#92060,
#92061,#92062,#92063,#92064,#92065,#92066,#92067,#92068,#92069,#92070,#92071,
#92072,#92073,#92074,#92075,#92076,#92077,#92078,#92079,#92080,#92081,#92082,
#92083,#92084,#92085,#92086,#92087,#92088),.UNSPECIFIED.,.F.,.F.,(4,2,2,
2,2,2,2,2,2,2,2,2,2,2,2,2,2,2,2,2,2,2,2,2,2,2,2,2,2,2,2,2,2,2,2,2,2,2,2,
2,2,2,2,2,2,2,2,2,2,2,2,2,2,2,2,2,2,2,2,2,2,2,2,2,2,2,2,2,2,2,2,2,2,2,2,
2,2,2,2,2,2,2,2,2,2,2,2,2,2,2,2,2,2,2,2,2,2,2,2,2,2,2,2,2,2,2,2,2,2,4),
(0.000560841254929146,0.00122756953817873,0.00267783709836508,0.00567972886798112,
0.0181404681574918,0.0482412476540577,0.0631058226340338,0.0702712299010112,
0.0719322779124441,0.0728879076863163,0.073728893577787,0.074809949783987,
0.0766004493265835,0.0876821930869903,0.0934836507060726,0.118466356148674,
0.132922348118984,0.14153694467225,0.144129266545428,0.14553501432938,0.146922238349318,
0.148684188609048,0.151883422859173,0.16719752434947,0.207148620060003,
0.215970682958397,0.217737382556324,0.218716201272492,0.219553878953511,
0.220618309432577,0.222796599214438,0.241812416348709,0.27641312480095,
0.287075251525013,0.289861973754058,0.291536071740568,0.293036860785837,
0.294945072957918,0.297974518986067,0.315238399591854,0.343693836168037,
0.359788736556918,0.362917222689147,0.364149435902665,0.36501179462008,
0.365802663216913,0.367113095539219,0.370493437868455,0.396815555788648,
0.427749043793531,0.43396315179399,0.436260129516705,0.437827806985887,
0.43935695795578,0.441197049068491,0.445823569974353,0.485390019406719,
0.500655046706769,0.507939190168633,0.509608807644229,0.510566368139009,
0.511407058598387,0.51248518732404,0.514265603325819,0.525039635340057,
0.529105156428922,0.530736963300407,0.557265998364079,0.575997299907815,
0.580518225428479,0.58254380013687,0.584060725004862,0.585679346535489,
0.58821425323658,0.595559647273401,0.644307115618753,0.653671182364416,
0.65546738505493,0.656452688764453,0.657289909113878,0.658346102245061,
0.660014916233895,0.668662787504782,0.700017285642924,0.715901171077016,
0.725090015718347,0.727741707522573,0.729386168383326,0.730894397707321,
0.732827540488198,0.736009171757536,0.758600313644145,0.779718294718379,
0.793139809137975,0.799859817340565,0.801487782092057,0.802436227597114,
0.803278963837292,0.804372721475638,0.80620620218633,0.818393093773607,
0.844663171343837,0.867198441868272,0.872173952201972,0.87427899915139,
0.875809569388275,0.877213302395477,0.879108651497984,0.88376550628148,
0.92220090061974),.UNSPECIFIED.);
#1478=B_SPLINE_CURVE_WITH_KNOTS('',3,(#92089,#92090,#92091,#92092,#92093,
#92094,#92095,#92096,#92097,#92098,#92099,#92100,#92101,#92102,#92103,#92104,
#92105,#92106,#92107,#92108,#92109,#92110,#92111,#92112,#92113,#92114,#92115,
#92116,#92117,#92118,#92119,#92120,#92121,#92122,#92123,#92124,#92125,#92126,
#92127,#92128,#92129,#92130,#92131,#92132,#92133,#92134,#92135,#92136,#92137,
#92138,#92139,#92140,#92141,#92142,#92143,#92144,#92145,#92146,#92147,#92148,
#92149,#92150,#92151,#92152,#92153,#92154,#92155,#92156,#92157,#92158,#92159,
#92160,#92161,#92162,#92163,#92164,#92165,#92166,#92167,#92168,#92169,#92170,
#92171,#92172,#92173,#92174,#92175,#92176,#92177,#92178,#92179,#92180,#92181,
#92182,#92183,#92184,#92185,#92186,#92187,#92188,#92189,#92190,#92191,#92192,
#92193,#92194,#92195,#92196,#92197,#92198,#92199,#92200,#92201,#92202,#92203,
#92204,#92205,#92206,#92207,#92208,#92209,#92210,#92211,#92212,#92213,#92214,
#92215,#92216,#92217,#92218,#92219,#92220,#92221,#92222,#92223,#92224,#92225,
#92226,#92227,#92228,#92229,#92230,#92231,#92232,#92233,#92234,#92235,#92236,
#92237,#92238,#92239,#92240,#92241,#92242,#92243,#92244,#92245,#92246,#92247,
#92248,#92249,#92250,#92251,#92252,#92253,#92254,#92255,#92256,#92257,#92258,
#92259,#92260,#92261,#92262,#92263,#92264,#92265,#92266,#92267,#92268,#92269,
#92270,#92271,#92272,#92273,#92274,#92275,#92276,#92277,#92278,#92279,#92280,
#92281,#92282,#92283,#92284,#92285,#92286,#92287,#92288,#92289,#92290,#92291,
#92292,#92293,#92294,#92295,#92296,#92297,#92298,#92299,#92300,#92301,#92302,
#92303,#92304,#92305,#92306,#92307,#92308),.UNSPECIFIED.,.F.,.F.,(4,2,2,
2,2,2,2,2,2,2,2,2,2,2,2,2,2,2,2,2,2,2,2,2,2,2,2,2,2,2,2,2,2,2,2,2,2,2,2,
2,2,2,2,2,2,2,2,2,2,2,2,2,2,2,2,2,2,2,2,2,2,2,2,2,2,2,2,2,2,2,2,2,2,2,2,
2,2,2,2,2,2,2,2,2,2,2,2,2,2,2,2,2,2,2,2,2,2,2,2,2,2,2,2,2,2,2,2,2,2,4),
(0.922044868712354,0.957951216955999,0.962857132189006,0.964795243308246,
0.966210145180478,0.9677333716962,0.969793542894975,0.974505481536299,1.01033907250438,
1.0338039155043,1.03720987579679,1.03852492584848,1.03931701440143,1.04017928093119,
1.04140900386122,1.04451874111044,1.07372111205207,1.10353715082914,1.1086946534071,
1.11089337087447,1.1124265223922,1.11399149734849,1.11627201105666,1.12236561508084,
1.14930613726452,1.18000634886144,1.18321643011407,1.18449922076051,1.18528518696247,
1.18615322471591,1.18741241065632,1.19071345506026,1.20862773288827,1.22811240673908,
1.25200343314321,1.25521115203296,1.25715237260071,1.2586622920841,1.2603039561618,
1.26294093295913,1.2719762186749,1.28746609780656,1.31797414836967,1.32789531037431,
1.3296314252471,1.33070821458202,1.33154734756932,1.33251842554787,1.3342480693396,
1.34242910861663,1.36098295462764,1.39558537584312,1.40059166365024,1.40254652978157,
1.40396575209104,1.40548619857169,1.40752960195658,1.41214653280481,1.43163573793088,
1.46109093775326,1.46575197942915,1.47398752796917,1.4756304750864,1.47667897077869,
1.47751601842559,1.47850810236714,1.48033480490755,1.49030057773163,1.50465655267378,
1.54179382211166,1.54660189492035,1.5485234289827,1.54993406629443,1.55146017990374,
1.55353756966455,1.55834869626468,1.57944921565393,1.61104710500875,1.61984885719269,
1.6215254494019,1.6225841891728,1.62342182948617,1.62440578001485,1.62619483841352,
1.63541480323601,1.68121846539728,1.69108264970303,1.69385733035515,1.69555583432989,
1.69702341744196,1.69846303747577,1.70150822980826,1.71580014007246,1.75047936255721,
1.75524581448804,1.76564446812615,1.76740352464161,1.76848707458016,1.76932667796977,
1.77029285853423,1.7720007494468,1.77984282979742,1.7970971166788,1.8275937815837,
1.83252639647331,1.83812231186191,1.84034742488907,1.84176042468243,1.84300117335869,
1.84382673505472),.UNSPECIFIED.);
#1479=B_SPLINE_CURVE_WITH_KNOTS('',3,(#92313,#92314,#92315,#92316,#92317,
#92318,#92319,#92320,#92321,#92322,#92323,#92324,#92325,#92326,#92327,#92328,
#92329,#92330,#92331,#92332,#92333,#92334,#92335,#92336,#92337,#92338,#92339,
#92340,#92341,#92342,#92343,#92344,#92345,#92346,#92347,#92348,#92349,#92350,
#92351,#92352,#92353,#92354,#92355,#92356,#92357,#92358,#92359,#92360,#92361,
#92362,#92363,#92364,#92365,#92366,#92367,#92368,#92369,#92370,#92371,#92372,
#92373,#92374,#92375,#92376,#92377,#92378,#92379,#92380,#92381,#92382,#92383,
#92384,#92385,#92386,#92387,#92388,#92389,#92390,#92391,#92392,#92393,#92394,
#92395,#92396,#92397,#92398,#92399,#92400,#92401,#92402,#92403,#92404,#92405,
#92406,#92407,#92408,#92409,#92410,#92411,#92412,#92413,#92414,#92415,#92416,
#92417,#92418,#92419,#92420,#92421,#92422,#92423,#92424,#92425,#92426,#92427,
#92428,#92429,#92430,#92431,#92432,#92433,#92434,#92435,#92436,#92437,#92438,
#92439,#92440,#92441,#92442,#92443,#92444,#92445,#92446,#92447,#92448,#92449,
#92450,#92451,#92452,#92453,#92454,#92455,#92456,#92457,#92458,#92459,#92460,
#92461,#92462,#92463,#92464,#92465,#92466,#92467,#92468,#92469,#92470,#92471,
#92472,#92473,#92474,#92475,#92476,#92477,#92478,#92479,#92480,#92481,#92482,
#92483,#92484,#92485,#92486,#92487,#92488,#92489,#92490,#92491,#92492,#92493,
#92494,#92495,#92496,#92497,#92498,#92499,#92500,#92501,#92502,#92503,#92504,
#92505,#92506,#92507,#92508,#92509,#92510,#92511,#92512,#92513,#92514,#92515,
#92516,#92517,#92518,#92519,#92520,#92521,#92522,#92523,#92524,#92525,#92526,
#92527,#92528,#92529,#92530,#92531,#92532,#92533,#92534),.UNSPECIFIED.,
 .F.,.F.,(4,2,2,2,2,2,2,2,2,2,2,2,2,2,2,2,2,2,2,2,2,2,2,2,2,2,2,2,2,2,2,
2,2,2,2,2,2,2,2,2,2,2,2,2,2,2,2,2,2,2,2,2,2,2,2,2,2,2,2,2,2,2,2,2,2,2,2,
2,2,2,2,2,2,2,2,2,2,2,2,2,2,2,2,2,2,2,2,2,2,2,2,2,2,2,2,2,2,2,2,2,2,2,2,
2,2,2,2,2,2,2,4),(0.92184713791035,0.959502202714741,0.964248452591541,
0.966156811049808,0.967563602013588,0.969091156156367,0.971180574837927,
0.976065701690815,0.997810886587701,1.02713685176618,1.03730234613504,1.03905214723152,
1.04013269185765,1.04097169562458,1.0419391328413,1.04365388153892,1.05160994584751,
1.06929694504387,1.10512553887402,1.11004478453439,1.11198442586174,1.11339912362621,
1.11492087830805,1.11697684646725,1.12166937331292,1.14178715244534,1.17188928515539,
1.17273432237921,1.18316199506977,1.18492196537473,1.18600553516131,1.18684480276664,
1.18781018172543,1.18951565207609,1.1973287366786,1.21447855352106,1.25110000003608,
1.25595276669724,1.25788110008379,1.25929286085876,1.2608165019727,1.26288395880259,
1.2676424961359,1.28831042375301,1.30862340201075,1.32865266040931,1.33083561439304,
1.33190083574309,1.33273841724212,1.33371628803733,1.33547920376982,1.34423845665217,
1.38342544851417,1.38781514310891,1.3999761416561,1.40297752093518,1.4047162932078,
1.40620921539986,1.40802338134246,1.41145963549553,1.43617313975216,1.4603718058285,
1.46384144304377,1.47483184582374,1.47661814597033,1.47769784321836,1.47853850608394,
1.47949459753753,1.48115836177949,1.48836497250983,1.50337154463875,1.54121631636813,
1.54721110253447,1.549546013434,1.55096377325012,1.55248292851237,1.55452507219774,
1.55914117317309,1.57863886211985,1.60781127175613,1.61105675297003,1.62078703102191,
1.62251245465064,1.62358549676229,1.62442358458636,1.6253955811703,1.62713202352675,
1.63544317725256,1.66991338570153,1.69086710689583,1.69428921568218,1.69610054202612,
1.69755590889034,1.69895896290358,1.70150520065044,1.70970187225048,1.72316486819267,
1.74781792230383,1.76618561505148,1.7683570221211,1.76941977827453,1.77025696197296,
1.77123615053114,1.77300589804385,1.78189313395678,1.8226996992311,1.83718485204772,
1.84032456194338,1.8419602229474,1.84280903719847,1.84319664678967),
 .UNSPECIFIED.);
#1480=B_SPLINE_CURVE_WITH_KNOTS('',3,(#92535,#92536,#92537,#92538,#92539,
#92540,#92541,#92542,#92543,#92544,#92545,#92546,#92547,#92548,#92549,#92550,
#92551,#92552,#92553,#92554,#92555,#92556,#92557,#92558,#92559,#92560,#92561,
#92562,#92563,#92564,#92565,#92566,#92567,#92568,#92569,#92570,#92571,#92572,
#92573,#92574,#92575,#92576,#92577,#92578,#92579,#92580,#92581,#92582,#92583,
#92584,#92585,#92586,#92587,#92588,#92589,#92590,#92591,#92592,#92593,#92594,
#92595,#92596,#92597,#92598,#92599,#92600,#92601,#92602,#92603,#92604,#92605,
#92606,#92607,#92608,#92609,#92610,#92611,#92612,#92613,#92614,#92615,#92616,
#92617,#92618,#92619,#92620,#92621,#92622,#92623,#92624,#92625,#92626,#92627,
#92628,#92629,#92630,#92631,#92632,#92633,#92634,#92635,#92636,#92637,#92638,
#92639,#92640,#92641,#92642,#92643,#92644,#92645,#92646,#92647,#92648,#92649,
#92650,#92651,#92652,#92653,#92654,#92655,#92656,#92657,#92658,#92659,#92660,
#92661,#92662,#92663,#92664,#92665,#92666,#92667,#92668,#92669,#92670,#92671,
#92672,#92673,#92674,#92675,#92676,#92677,#92678,#92679,#92680,#92681,#92682,
#92683,#92684,#92685,#92686,#92687,#92688,#92689,#92690,#92691,#92692,#92693,
#92694,#92695,#92696,#92697,#92698,#92699,#92700,#92701,#92702,#92703,#92704,
#92705,#92706,#92707,#92708,#92709,#92710,#92711,#92712,#92713,#92714,#92715,
#92716,#92717,#92718,#92719,#92720,#92721,#92722,#92723,#92724,#92725,#92726,
#92727,#92728,#92729,#92730,#92731,#92732,#92733,#92734,#92735,#92736,#92737,
#92738,#92739,#92740,#92741,#92742,#92743,#92744,#92745,#92746,#92747,#92748,
#92749,#92750,#92751,#92752,#92753,#92754,#92755,#92756,#92757,#92758,#92759,
#92760,#92761,#92762,#92763,#92764,#92765,#92766,#92767,#92768,#92769,#92770,
#92771,#92772,#92773,#92774,#92775,#92776,#92777,#92778,#92779,#92780,#92781,
#92782),.UNSPECIFIED.,.F.,.F.,(4,2,2,2,2,2,2,2,2,2,2,2,2,2,2,2,2,2,2,2,
2,2,2,2,2,2,2,2,2,2,2,2,2,2,2,2,2,2,2,2,2,2,2,2,2,2,2,2,2,2,2,2,2,2,2,2,
2,2,2,2,2,2,2,2,2,2,2,2,2,2,2,2,2,2,2,2,2,2,2,2,2,2,2,2,2,2,2,2,2,2,2,2,
2,2,2,2,2,2,2,2,2,2,2,2,2,2,2,2,2,2,2,2,2,2,2,2,2,2,2,2,2,2,2,4),(0.00012595403202429,
0.00218637696266717,0.00554721496821566,0.0239701111963791,0.0549555024570598,
0.0636516104352712,0.0670061422371314,0.0694733219362498,0.0705931884102283,
0.0714369703945452,0.0723816528101506,0.0739923205577916,0.0797162191741279,
0.110377873674624,0.136998805598095,0.141103587059436,0.142994152621875,
0.143020098183966,0.143046065870231,0.143072140017256,0.143098410197693,
0.143124972852337,0.143151933243671,0.143179407914987,0.143207527730223,
0.143236441781002,0.14326632246758,0.143297372223598,0.143329832604141,
0.143363996858905,0.143400227678008,0.143438983102546,0.143480855440994,
0.143526632169561,0.143577395805891,0.144957057462043,0.146705001471571,
0.14984124782424,0.164210301934727,0.205133245307085,0.214031167616271,
0.21580243835845,0.21678241386525,0.217620237933776,0.218683791331271,0.220856781157315,
0.239233502956004,0.257374347094855,0.275282649333089,0.285233094207398,
0.287957727233648,0.289618476098257,0.291122756979793,0.29305690630218,
0.296171217751287,0.316033489673126,0.35153527606005,0.35995526673488,0.361699123477876,
0.362673179710778,0.363511729196881,0.364583687709302,0.366304170682459,
0.375919616626686,0.382066480279564,0.409311086696754,0.4281318055117,0.432664686170611,
0.434692856912888,0.436210639211135,0.437633654884878,0.439603705195045,
0.444704969762174,0.47725879114568,0.504375707510041,0.507053723176792,
0.50821158373033,0.509061025093207,0.509872153033562,0.511284864792439,
0.515352271524616,0.547470932545512,0.575660180833196,0.579158623129055,
0.580986428030765,0.582336837988072,0.58401614983331,0.586824785491797,
0.596476726083428,0.602933215397876,0.642909884322407,0.651734677152069,
0.653501996700771,0.654481177582231,0.655319182211822,0.656384069648828,
0.658563447040849,0.677644759745462,0.712189363349494,0.722843238208159,
0.725629948181284,0.727304448801835,0.728805862426927,0.730715234046021,
0.733747263033456,0.751009086425224,0.789012703406279,0.797670777485914,
0.799428638215717,0.800405773101758,0.801244012328779,0.802311756290388,
0.804018199210054,0.813363859088499,0.816967421623116,0.846250287691673,
0.865755008074216,0.870373298635367,0.872416782579536,0.873937083934142,
0.87554994869635,0.878056510194058,0.88518976221749,0.921744011977849),
 .UNSPECIFIED.);
#1481=B_SPLINE_CURVE_WITH_KNOTS('',3,(#92788,#92789,#92790,#92791),
 .UNSPECIFIED.,.F.,.F.,(4,4),(1.84328751696407,1.84339250911099),
 .UNSPECIFIED.);
#1482=B_SPLINE_CURVE_WITH_KNOTS('',3,(#92792,#92793,#92794,#92795,#92796,
#92797,#92798,#92799,#92800,#92801,#92802,#92803,#92804,#92805,#92806,#92807,
#92808,#92809,#92810,#92811,#92812,#92813,#92814,#92815,#92816,#92817,#92818,
#92819,#92820,#92821,#92822,#92823,#92824,#92825,#92826,#92827,#92828,#92829,
#92830,#92831,#92832,#92833,#92834,#92835,#92836,#92837,#92838,#92839,#92840,
#92841,#92842,#92843,#92844,#92845,#92846,#92847,#92848,#92849,#92850,#92851,
#92852,#92853,#92854,#92855,#92856,#92857,#92858,#92859,#92860,#92861,#92862,
#92863,#92864,#92865,#92866,#92867,#92868,#92869,#92870,#92871,#92872,#92873,
#92874,#92875,#92876,#92877,#92878,#92879,#92880,#92881,#92882,#92883,#92884,
#92885,#92886,#92887,#92888,#92889,#92890,#92891,#92892,#92893,#92894,#92895,
#92896,#92897,#92898,#92899,#92900,#92901,#92902,#92903,#92904,#92905,#92906,
#92907,#92908,#92909,#92910,#92911,#92912,#92913,#92914,#92915,#92916,#92917,
#92918,#92919,#92920,#92921,#92922,#92923,#92924,#92925,#92926,#92927,#92928,
#92929,#92930,#92931,#92932,#92933,#92934,#92935,#92936,#92937,#92938,#92939,
#92940,#92941,#92942,#92943,#92944,#92945,#92946,#92947,#92948,#92949,#92950,
#92951,#92952,#92953,#92954,#92955,#92956,#92957,#92958,#92959,#92960,#92961,
#92962,#92963,#92964,#92965,#92966,#92967,#92968,#92969,#92970,#92971,#92972,
#92973,#92974,#92975,#92976,#92977,#92978,#92979,#92980,#92981,#92982,#92983,
#92984,#92985,#92986,#92987,#92988,#92989,#92990,#92991,#92992,#92993,#92994,
#92995,#92996,#92997,#92998,#92999,#93000,#93001,#93002,#93003,#93004,#93005,
#93006,#93007,#93008,#93009,#93010,#93011,#93012,#93013,#93014,#93015,#93016,
#93017,#93018,#93019,#93020,#93021,#93022,#93023,#93024,#93025,#93026,#93027,
#93028,#93029,#93030,#93031,#93032,#93033,#93034,#93035,#93036,#93037,#93038,
#93039,#93040,#93041,#93042,#93043),.UNSPECIFIED.,.F.,.F.,(4,2,2,2,2,2,
2,2,2,2,2,2,2,2,2,2,2,2,2,2,2,2,2,2,2,2,2,2,2,2,2,2,2,2,2,2,2,2,2,2,2,2,
2,2,2,2,2,2,2,2,2,2,2,2,2,2,2,2,2,2,2,2,2,2,2,2,2,2,2,2,2,2,2,2,2,2,2,2,
2,2,2,2,2,2,2,2,2,2,2,2,2,2,2,2,2,2,2,2,2,2,2,2,2,2,2,2,2,2,2,2,2,2,2,2,
2,2,2,2,2,2,2,2,2,2,2,4),(0.000507238272519671,0.0115418756662477,0.0161571515980744,
0.0175387459960026,0.0184800213009734,0.0192665950615534,0.0201084096248052,
0.0211965733620706,0.0230114391999691,0.0347020160235591,0.0421510699498056,
0.0629843018573606,0.0786783707889196,0.087791964193193,0.0904356812284005,
0.0920781025212334,0.0935864074751727,0.0955223417032235,0.0987143659005448,
0.121823158328269,0.142229744673646,0.155766161873468,0.16026128371635,
0.162373702648284,0.164065047205974,0.165023582816099,0.165026289481035,
0.16502900841385,0.165031739646659,0.165034483317566,0.165037239494238,
0.165040008196784,0.165042789523719,0.165045583614506,0.165884248018116,
0.166961579432677,0.168700784394348,0.178700731597012,0.184200587396513,
0.211105093774062,0.232350788405546,0.235697760840822,0.237493357017398,
0.238971777810241,0.240721778058453,0.24377141410812,0.256571256187601,
0.299144704642571,0.308161566058544,0.30993901754339,0.310920150949101,
0.311757569683489,0.312818801779902,0.314504531697237,0.323479859128245,
0.354926694790919,0.370495029651168,0.379559213562087,0.38219808772191,
0.383839518327,0.385348268110146,0.387286652872957,0.390486772602777,0.414010639504558,
0.433903873874492,0.447505272164639,0.454282058326798,0.455914194091047,
0.456863450066428,0.457705798384517,0.458797618410472,0.460624823668758,
0.472643209202041,0.501037126350278,0.516429831595371,0.525424242536336,
0.528056017980191,0.529695862242627,0.531205058415621,0.533146666039113,
0.536357838593584,0.56499738458374,0.589917764242636,0.599810258968735,
0.601632640613339,0.60262344653153,0.603460044239458,0.604508754759125,
0.606153459330318,0.614427710277649,0.646412431380139,0.667697184496171,
0.672528479771231,0.674608640766409,0.676134560611962,0.677543445880114,
0.679460169640051,0.684243574775772,0.721592007256339,0.738248490911493,
0.745927941863251,0.74762467943057,0.748588190957836,0.749427827593889,
0.750514502575196,0.752284714430037,0.762912850310487,0.776606589220784,
0.813728503794617,0.818475755710185,0.820541362201342,0.82206479592093,
0.82347718065036,0.825407631681245,0.830272301428554,0.866745356671935,
0.883980439204212,0.891817078929897,0.893524166361651,0.894489952440844,
0.895329241447557,0.896412411779411,0.898170901120078,0.908566028100056,
0.921725293771825,0.92184713791035),.UNSPECIFIED.);
#1483=B_SPLINE_CURVE_WITH_KNOTS('',3,(#93045,#93046,#93047,#93048,#93049,
#93050,#93051,#93052,#93053,#93054,#93055,#93056,#93057,#93058,#93059,#93060,
#93061,#93062,#93063,#93064,#93065,#93066,#93067,#93068,#93069,#93070,#93071,
#93072,#93073,#93074,#93075,#93076,#93077,#93078,#93079,#93080,#93081,#93082,
#93083,#93084,#93085,#93086,#93087,#93088,#93089,#93090,#93091,#93092,#93093,
#93094,#93095,#93096,#93097,#93098,#93099,#93100,#93101,#93102,#93103,#93104,
#93105,#93106,#93107,#93108,#93109,#93110,#93111,#93112,#93113,#93114,#93115,
#93116,#93117,#93118,#93119,#93120,#93121,#93122,#93123,#93124,#93125,#93126,
#93127,#93128,#93129,#93130,#93131,#93132,#93133,#93134,#93135,#93136,#93137,
#93138,#93139,#93140,#93141,#93142,#93143,#93144,#93145,#93146,#93147,#93148,
#93149,#93150,#93151,#93152,#93153,#93154,#93155,#93156,#93157,#93158,#93159,
#93160,#93161,#93162,#93163,#93164,#93165,#93166,#93167,#93168,#93169,#93170,
#93171,#93172,#93173,#93174,#93175,#93176,#93177,#93178,#93179,#93180,#93181,
#93182,#93183,#93184,#93185,#93186,#93187,#93188,#93189,#93190,#93191,#93192,
#93193,#93194,#93195,#93196,#93197,#93198,#93199,#93200,#93201,#93202,#93203,
#93204,#93205,#93206,#93207,#93208,#93209,#93210,#93211,#93212,#93213,#93214,
#93215,#93216,#93217,#93218,#93219,#93220,#93221,#93222,#93223,#93224,#93225,
#93226,#93227,#93228,#93229,#93230,#93231,#93232,#93233,#93234,#93235,#93236,
#93237,#93238,#93239,#93240,#93241,#93242,#93243,#93244,#93245,#93246,#93247,
#93248,#93249,#93250,#93251,#93252,#93253,#93254,#93255,#93256,#93257,#93258,
#93259,#93260,#93261,#93262,#93263,#93264,#93265,#93266,#93267,#93268,#93269,
#93270,#93271,#93272,#93273,#93274,#93275,#93276,#93277,#93278,#93279,#93280,
#93281,#93282,#93283,#93284),.UNSPECIFIED.,.F.,.F.,(4,2,2,2,2,2,2,2,2,2,
2,2,2,2,2,2,2,2,2,2,2,2,2,2,2,2,2,2,2,2,2,2,2,2,2,2,2,2,2,2,2,2,2,2,2,2,
2,2,2,2,2,2,2,2,2,2,2,2,2,2,2,2,2,2,2,2,2,2,2,2,2,2,2,2,2,2,2,2,2,2,2,2,
2,2,2,2,2,2,2,2,2,2,2,2,2,2,2,2,2,2,2,2,2,2,2,2,2,2,2,2,2,2,2,2,2,2,2,2,
2,4),(0.921744011977849,0.921865738458927,0.942875463146245,0.945058987704988,
0.946124727844946,0.946962837126453,0.947941480348613,0.949706193849952,
0.958483171269677,0.997857769285124,1.00187835052179,1.01419853273591,1.01721313057314,
1.01895560251344,1.0204350532745,1.02224098303035,1.02563462099119,1.04848407546454,
1.07493123890233,1.07808623450929,1.08909791407495,1.09088591753303,1.09196647160793,
1.09280769694936,1.09376432570356,1.09542880642761,1.10263529751694,1.11763689221872,
1.15544509611991,1.16148560244784,1.1638283010648,1.16524816107476,1.16676757045501,
1.16880658534114,1.17340071769271,1.19271066898546,1.22306651610329,1.23492716994851,
1.23674892120692,1.23783933268164,1.2386817319795,1.23963233829674,1.24126972005375,
1.24811034418236,1.2619141802092,1.27953506561225,1.30504490179358,1.30826601596226,
1.31021086919364,1.31172096257071,1.31336015649653,1.31598734191935,1.32493135350266,
1.3401943565466,1.35554782663822,1.3786729325822,1.38207577983284,1.38339007796561,
1.38418184574252,1.38504388360563,1.38627348205163,1.3893839636763,1.40529378766577,
1.43527994794866,1.4396329781728,1.45181249929639,1.4548163387311,1.45655624372948,
1.45804996887263,1.45986490392343,1.46330200352542,1.48798919102565,1.51148591021547,
1.51647211320548,1.52674685887107,1.52849974082616,1.52958137564175,1.53042070745019,
1.53138795173193,1.53310100821026,1.54102522776882,1.55858967427563,1.59459275642693,
1.5994982202846,1.60143586669545,1.60285032804622,1.6043729844576,1.60643221539607,
1.61114125540389,1.64630990005493,1.67041592703416,1.67382310313879,1.67513807747604,
1.67592996080104,1.67679185839171,1.67799608307912,1.68096790791604,1.6852713676201,
1.69791597508939,1.70532821100474,1.74038201230939,1.74535752409139,1.74730693232044,
1.74872444459137,1.7502451746662,1.75229265811921,1.75693484534131,1.77663505762934,
1.78935914088988,1.80298014927108,1.80863787201225,1.81852255491565,1.82025634996804,
1.82133221316388,1.82217095734787,1.82296140675861,1.82392165848958,1.825349327827,
1.83023071831389,1.84305473654517),.UNSPECIFIED.);
#1484=B_SPLINE_CURVE_WITH_KNOTS('',3,(#93285,#93286,#93287,#93288),
 .UNSPECIFIED.,.F.,.F.,(4,4),(6.06069286854334E-5,0.000165048526771096),
 .UNSPECIFIED.);
#1485=B_SPLINE_CURVE_WITH_KNOTS('',3,(#93293,#93294,#93295,#93296,#93297,
#93298,#93299,#93300,#93301,#93302,#93303,#93304,#93305,#93306,#93307,#93308,
#93309,#93310,#93311,#93312,#93313,#93314,#93315,#93316,#93317,#93318,#93319,
#93320,#93321,#93322,#93323,#93324,#93325,#93326,#93327,#93328,#93329,#93330,
#93331,#93332,#93333,#93334,#93335,#93336,#93337,#93338,#93339,#93340,#93341,
#93342,#93343,#93344,#93345,#93346,#93347,#93348,#93349,#93350,#93351,#93352,
#93353,#93354,#93355,#93356,#93357,#93358,#93359,#93360,#93361,#93362,#93363,
#93364,#93365,#93366,#93367,#93368,#93369,#93370,#93371,#93372,#93373,#93374,
#93375,#93376,#93377,#93378,#93379,#93380,#93381,#93382,#93383,#93384,#93385,
#93386,#93387,#93388,#93389,#93390,#93391,#93392,#93393,#93394,#93395,#93396,
#93397,#93398,#93399,#93400,#93401,#93402,#93403,#93404,#93405,#93406,#93407,
#93408,#93409,#93410,#93411,#93412,#93413,#93414,#93415,#93416,#93417,#93418,
#93419,#93420,#93421,#93422,#93423,#93424,#93425,#93426,#93427,#93428,#93429,
#93430,#93431,#93432,#93433,#93434,#93435,#93436,#93437,#93438,#93439,#93440,
#93441,#93442,#93443,#93444,#93445,#93446,#93447,#93448,#93449,#93450,#93451,
#93452,#93453,#93454,#93455,#93456,#93457,#93458,#93459,#93460,#93461,#93462,
#93463,#93464,#93465,#93466,#93467,#93468,#93469,#93470,#93471,#93472,#93473,
#93474,#93475,#93476,#93477,#93478,#93479,#93480,#93481,#93482,#93483,#93484,
#93485,#93486,#93487,#93488,#93489,#93490,#93491,#93492,#93493,#93494,#93495,
#93496,#93497,#93498,#93499,#93500,#93501,#93502,#93503,#93504,#93505,#93506,
#93507,#93508,#93509,#93510,#93511,#93512,#93513,#93514,#93515,#93516,#93517,
#93518,#93519,#93520,#93521,#93522,#93523,#93524,#93525,#93526,#93527,#93528,
#93529,#93530,#93531,#93532,#93533,#93534,#93535,#93536,#93537,#93538,#93539,
#93540,#93541,#93542,#93543,#93544,#93545,#93546,#93547,#93548),
 .UNSPECIFIED.,.F.,.F.,(4,2,2,2,2,2,2,2,2,2,2,2,2,2,2,2,2,2,2,2,2,2,2,2,
2,2,2,2,2,2,2,2,2,2,2,2,2,2,2,2,2,2,2,2,2,2,2,2,2,2,2,2,2,2,2,2,2,2,2,2,
2,2,2,2,2,2,2,2,2,2,2,2,2,2,2,2,2,2,2,2,2,2,2,2,2,2,2,2,2,2,2,2,2,2,2,2,
2,2,2,2,2,2,2,2,2,2,2,2,2,2,2,2,2,2,2,2,2,2,2,2,2,2,2,2,2,2,2,4),(0.922053660167366,
0.922087260060697,0.940040360019168,0.958910709984947,0.983671445610604,
0.985810267030443,0.986866773817845,0.987703816919092,0.988688410408651,
0.990482049751448,0.999802918261662,1.04760833158185,1.05573564435285,1.05837060642386,
1.06001090511697,1.06151948947206,1.06349191178263,1.06772567124173,1.08426476345355,
1.11574005942909,1.11885233189373,1.12983902779931,1.13162520391438,1.13270487849394,
1.1335455565126,1.13450170272864,1.13616564787603,1.14337437849144,1.15838785883843,
1.19626480252467,1.20222978917324,1.2045603323842,1.20597729398325,1.20749701025564,
1.20954238349892,1.21417651122442,1.2338200852316,1.25922972009727,1.26100214864451,
1.26482076322953,1.27568689324359,1.27746791799819,1.27854602954697,1.2793864628986,
1.28034344268722,1.28201139689418,1.28927770565495,1.30448693936983,1.34414883568525,
1.3487613483557,1.35059880301895,1.35212688710593,1.35369462407545,1.35599383057863,
1.36222726691849,1.39276552672758,1.41942133833821,1.42278982840368,1.42409804027155,
1.42488827484649,1.42575058815126,1.42698382421619,1.43012066012992,1.44630887783009,
1.47432585394347,1.49190032765189,1.49494096782665,1.49685216649045,1.49835277641904,
1.500024058684,1.50279994461129,1.51334407414068,1.53295260484837,1.56573419028011,
1.56874343108313,1.56986798384359,1.57066632193375,1.57152226232998,1.57272138558515,
1.57564567927515,1.58974377943675,1.60915394397955,1.61679756787017,1.63753339326822,
1.64066930848961,1.64258843731963,1.64409404646603,1.64574412966254,1.64842384050773,
1.65790877083962,1.67456349461645,1.69821351357824,1.70255103019716,1.71317250854167,
1.71494190029434,1.71602812568589,1.71686744654269,1.71687216082131,1.7168768143746,
1.71688140830469,1.71688594376328,1.71689042178191,1.71689484343876,1.71689920972128,
1.71690352167988,1.71690778028904,1.71691198646676,1.71691614111979,1.71692024519425,
1.7169242996355,1.71692830523611,1.71693226285809,1.71693617336732,1.71790696852665,
1.719614421643,1.72177880850698,1.72643098462764,1.74072683873456,1.74383712668433,
1.78121434372384,1.78599374279393,1.78790937635078,1.78931763970165,1.79084305803641,
1.79292284985602,1.79775473667297,1.81904968632349,1.84328751696407),
 .UNSPECIFIED.);
#1486=B_SPLINE_CURVE_WITH_KNOTS('',3,(#93549,#93550,#93551,#93552,#93553,
#93554,#93555,#93556,#93557,#93558,#93559,#93560,#93561,#93562,#93563,#93564,
#93565,#93566,#93567,#93568,#93569,#93570,#93571,#93572,#93573,#93574,#93575,
#93576,#93577,#93578,#93579,#93580,#93581,#93582,#93583,#93584,#93585,#93586,
#93587,#93588,#93589,#93590,#93591,#93592,#93593,#93594,#93595,#93596,#93597,
#93598,#93599,#93600,#93601,#93602,#93603,#93604,#93605,#93606,#93607,#93608,
#93609,#93610,#93611,#93612,#93613,#93614,#93615,#93616,#93617,#93618,#93619,
#93620,#93621,#93622,#93623,#93624,#93625,#93626,#93627,#93628,#93629,#93630,
#93631,#93632,#93633,#93634,#93635,#93636,#93637,#93638,#93639,#93640,#93641,
#93642,#93643,#93644,#93645,#93646,#93647,#93648,#93649,#93650,#93651,#93652,
#93653,#93654,#93655,#93656,#93657,#93658,#93659,#93660,#93661,#93662,#93663,
#93664,#93665,#93666,#93667,#93668,#93669,#93670,#93671,#93672,#93673,#93674,
#93675,#93676,#93677,#93678,#93679,#93680,#93681,#93682,#93683,#93684,#93685,
#93686,#93687,#93688,#93689,#93690,#93691,#93692,#93693,#93694,#93695,#93696,
#93697,#93698,#93699,#93700,#93701,#93702,#93703,#93704,#93705,#93706,#93707,
#93708,#93709,#93710,#93711,#93712,#93713,#93714,#93715,#93716,#93717,#93718,
#93719,#93720,#93721,#93722,#93723,#93724,#93725,#93726,#93727,#93728,#93729,
#93730,#93731,#93732,#93733,#93734,#93735,#93736,#93737,#93738,#93739,#93740,
#93741,#93742,#93743,#93744,#93745,#93746,#93747,#93748,#93749,#93750,#93751,
#93752,#93753,#93754,#93755,#93756,#93757,#93758),.UNSPECIFIED.,.F.,.F.,
(4,2,2,2,2,2,2,2,2,2,2,2,2,2,2,2,2,2,2,2,2,2,2,2,2,2,2,2,2,2,2,2,2,2,2,
2,2,2,2,2,2,2,2,2,2,2,2,2,2,2,2,2,2,2,2,2,2,2,2,2,2,2,2,2,2,2,2,2,2,2,2,
2,2,2,2,2,2,2,2,2,2,2,2,2,2,2,2,2,2,2,2,2,2,2,2,2,2,2,2,2,2,2,2,2,4),(0.000165048526771096,
0.0253293883020531,0.0440233312379338,0.0485398414473035,0.0505648628561064,
0.0520819455305609,0.0535055102898666,0.055478239491361,0.0605976600882879,
0.0925806594593137,0.10915816826352,0.117396232764874,0.120628643687784,
0.122986886223187,0.12409383075386,0.124938905444333,0.12587847551582,0.127466259173235,
0.132972937720969,0.16925234368963,0.191681696135606,0.195063574176281,
0.196866782701579,0.198214489825009,0.199910658158823,0.202796750168318,
0.213220029316128,0.251687139151591,0.265761457742648,0.268684113545649,
0.269883381047268,0.270739721685867,0.271538680130797,0.272664469367232,
0.275679517991829,0.308422014850004,0.336476115064903,0.340539390079268,
0.342479881201168,0.343984674175026,0.345641523504167,0.348349582542018,
0.357088150645222,0.404153698408706,0.413437102129098,0.415229164613122,
0.416213619409496,0.417050987617156,0.418108494810463,0.420251265221457,
0.436076610926745,0.458751781769642,0.48340680028559,0.486843423628163,
0.488658281846636,0.490152031996057,0.491892066490804,0.494896377870751,
0.507082102985869,0.511188035506528,0.550597961678869,0.559376301281374,
0.561140919085653,0.562119473964424,0.562957482177003,0.564023067720846,
0.566206179224661,0.588183613402241,0.596117734484779,0.625354867098855,
0.631497351123744,0.63378463826994,0.63535077359174,0.636882353070066,0.638730141208508,
0.643402166041564,0.682627912157238,0.698100337801896,0.705445750016467,
0.707120145580897,0.708078999657966,0.708919873807517,0.709997043152338,
0.711773438040698,0.722493362893514,0.753298414168122,0.77329564601873,
0.777974224727522,0.780028339488228,0.781550364211679,0.782966484875099,
0.784909912426693,0.789848493038749,0.825420735390588,0.84326989705901,
0.851269806027336,0.85298789305913,0.853956349300999,0.854795684524097,
0.855875962836496,0.857623996064188,0.86779260362386,0.895513888013049,
0.92109500354705,0.921781199990569),.UNSPECIFIED.);
#1487=B_SPLINE_CURVE_WITH_KNOTS('',3,(#93763,#93764,#93765,#93766,#93767,
#93768,#93769,#93770,#93771,#93772,#93773,#93774,#93775,#93776,#93777,#93778,
#93779,#93780,#93781,#93782,#93783,#93784,#93785,#93786,#93787,#93788,#93789,
#93790,#93791,#93792,#93793,#93794,#93795,#93796,#93797,#93798,#93799,#93800,
#93801,#93802,#93803,#93804,#93805,#93806,#93807,#93808,#93809,#93810,#93811,
#93812,#93813,#93814,#93815,#93816,#93817,#93818,#93819,#93820,#93821,#93822,
#93823,#93824,#93825,#93826,#93827,#93828,#93829,#93830,#93831,#93832,#93833,
#93834,#93835,#93836,#93837,#93838,#93839,#93840,#93841,#93842,#93843,#93844,
#93845,#93846,#93847,#93848,#93849,#93850,#93851,#93852,#93853,#93854,#93855,
#93856,#93857,#93858,#93859,#93860,#93861,#93862,#93863,#93864,#93865,#93866,
#93867,#93868,#93869,#93870,#93871,#93872,#93873,#93874,#93875,#93876,#93877,
#93878,#93879,#93880,#93881,#93882,#93883,#93884,#93885,#93886,#93887,#93888,
#93889,#93890,#93891,#93892,#93893,#93894,#93895,#93896,#93897,#93898,#93899,
#93900,#93901,#93902,#93903,#93904,#93905,#93906,#93907,#93908,#93909,#93910,
#93911,#93912,#93913,#93914,#93915,#93916,#93917,#93918,#93919,#93920,#93921,
#93922,#93923,#93924,#93925,#93926,#93927,#93928,#93929,#93930,#93931,#93932,
#93933,#93934,#93935,#93936,#93937,#93938,#93939,#93940,#93941,#93942,#93943,
#93944,#93945,#93946,#93947,#93948,#93949,#93950,#93951,#93952,#93953,#93954,
#93955,#93956,#93957,#93958,#93959,#93960,#93961,#93962,#93963,#93964,#93965,
#93966,#93967,#93968,#93969,#93970,#93971,#93972,#93973,#93974,#93975,#93976,
#93977,#93978,#93979,#93980,#93981,#93982,#93983,#93984,#93985,#93986,#93987,
#93988,#93989,#93990),.UNSPECIFIED.,.F.,.F.,(4,2,2,2,2,2,2,2,2,2,2,2,2,
2,2,2,2,2,2,2,2,2,2,2,2,2,2,2,2,2,2,2,2,2,2,2,2,2,2,2,2,2,2,2,2,2,2,2,2,
2,2,2,2,2,2,2,2,2,2,2,2,2,2,2,2,2,2,2,2,2,2,2,2,2,2,2,2,2,2,2,2,2,2,2,2,
2,2,2,2,2,2,2,2,2,2,2,2,2,2,2,2,2,2,2,2,2,2,2,2,2,2,2,2,4),(0.00056079372868648,
0.0314868325224866,0.0345598635795401,0.0371810842167673,0.0388185847011278,
0.0403284860626301,0.0422749990790293,0.0455029771596276,0.0724134642533599,
0.0872259664856132,0.101947138251465,0.109164320163466,0.110836809300504,
0.111794974413502,0.112635462014109,0.11371242912883,0.115489139215583,
0.126221107362654,0.128816795710397,0.132081318273396,0.156173772407901,
0.171434016811604,0.177355359165885,0.181728724373122,0.183754843511515,
0.185271694282524,0.186694272331117,0.188664405386996,0.193769847522993,
0.226162967187165,0.246306035750068,0.254872941407773,0.256624855220193,
0.257600370626565,0.258438267959618,0.259506906218576,0.261217299757883,
0.27064950507009,0.302044032362892,0.317302963090176,0.326243708766339,
0.328869849463748,0.330508349749237,0.332017771100936,0.333961706768687,
0.337181150505317,0.3662284688738,0.390796876715171,0.400619329131009,0.402438186940812,
0.403428179111341,0.404264756774781,0.405314281688441,0.406961781844157,
0.415283332591889,0.447278012038036,0.468504645774497,0.473328970080421,
0.475407843006287,0.476933459153305,0.47834251479773,0.480260163788278,
0.48504948533156,0.522330013438216,0.53902709121155,0.546717468734998,0.548414854612492,
0.549378469746305,0.550218018268044,0.551304349595943,0.553073556687684,
0.56368495909994,0.564269942653249,0.570558938821339,0.594857189204174,
0.616637607065162,0.620000669124977,0.621799680235413,0.62327823891301,
0.625025257715295,0.628061764484938,0.640677113568726,0.683446680757099,
0.692477058164472,0.694255267817985,0.695236574889481,0.696073992199009,
0.697135030279977,0.698820090335841,0.707783081089864,0.75164721128199,
0.763459359468865,0.766337819828426,0.76803203133338,0.769529307174784,
0.771404264713819,0.774324850434573,0.789423958958945,0.829601299629364,
0.838440914800426,0.840208492969272,0.841187452754502,0.842025038781892,
0.843089079352831,0.84526566082161,0.864091502318696,0.888440640740583,
0.901833252358031,0.909999925860023,0.912543469636756,0.914163927687913,
0.915679995621691,0.917665771636198,0.922053660167366),.UNSPECIFIED.);
#1488=B_SPLINE_CURVE_WITH_KNOTS('',3,(#93991,#93992,#93993,#93994,#93995,
#93996,#93997,#93998,#93999,#94000,#94001,#94002,#94003,#94004,#94005,#94006,
#94007,#94008,#94009,#94010,#94011,#94012,#94013,#94014,#94015,#94016,#94017,
#94018,#94019,#94020,#94021,#94022,#94023,#94024,#94025,#94026,#94027,#94028,
#94029,#94030,#94031,#94032,#94033,#94034,#94035,#94036,#94037,#94038,#94039,
#94040,#94041,#94042,#94043,#94044,#94045,#94046,#94047,#94048,#94049,#94050,
#94051,#94052,#94053,#94054,#94055,#94056,#94057,#94058,#94059,#94060,#94061,
#94062,#94063,#94064,#94065,#94066,#94067,#94068,#94069,#94070,#94071,#94072,
#94073,#94074,#94075,#94076,#94077,#94078,#94079,#94080,#94081,#94082,#94083,
#94084,#94085,#94086,#94087,#94088,#94089,#94090,#94091,#94092,#94093,#94094,
#94095,#94096,#94097,#94098,#94099,#94100,#94101,#94102,#94103,#94104,#94105,
#94106,#94107,#94108,#94109,#94110,#94111,#94112,#94113,#94114,#94115,#94116,
#94117,#94118,#94119,#94120,#94121,#94122,#94123,#94124,#94125,#94126,#94127,
#94128,#94129,#94130,#94131,#94132,#94133,#94134,#94135,#94136,#94137,#94138,
#94139,#94140,#94141,#94142,#94143,#94144,#94145,#94146,#94147,#94148,#94149,
#94150,#94151,#94152,#94153,#94154,#94155,#94156,#94157,#94158,#94159,#94160,
#94161,#94162,#94163,#94164,#94165,#94166,#94167,#94168,#94169,#94170,#94171,
#94172,#94173,#94174,#94175,#94176,#94177,#94178,#94179,#94180,#94181,#94182,
#94183,#94184,#94185,#94186,#94187,#94188,#94189,#94190,#94191,#94192,#94193,
#94194,#94195,#94196,#94197,#94198,#94199,#94200,#94201,#94202,#94203,#94204,
#94205,#94206,#94207,#94208,#94209,#94210,#94211,#94212,#94213,#94214,#94215,
#94216,#94217,#94218,#94219,#94220,#94221,#94222),.UNSPECIFIED.,.F.,.F.,
(4,2,2,2,2,2,2,2,2,2,2,2,2,2,2,2,2,2,2,2,2,2,2,2,2,2,2,2,2,2,2,2,2,2,2,
2,2,2,2,2,2,2,2,2,2,2,2,2,2,2,2,2,2,2,2,2,2,2,2,2,2,2,2,2,2,2,2,2,2,2,2,
2,2,2,2,2,2,2,2,2,2,2,2,2,2,2,2,2,2,2,2,2,2,2,2,2,2,2,2,2,2,2,2,2,2,2,2,
2,2,2,2,2,2,2,2,4),(0.921781199990569,0.92455095130394,0.926369992845057,
0.927864117165824,0.929601106002656,0.932591516343193,0.944590865243596,
0.949293899696131,0.979093267103647,0.995024654573263,0.998137633628146,
0.999367725088923,1.00022994456683,1.00102174896383,1.00233585262656,1.00573684592158,
1.03077341063013,1.06505526322163,1.06976355062009,1.07182283997351,1.07334568558818,
1.07476042344764,1.07669860552441,1.08160625616145,1.11757494442375,1.13515119104018,
1.14307936949195,1.14479283679915,1.14576025985897,1.14659970808534,1.14768145085986,
1.14943443285809,1.15970666592777,1.18987032639148,1.20534364386987,1.21437093478311,
1.21700674299596,1.21864792017993,1.22015755308706,1.22209862854499,1.22530656891669,
1.25473863107226,1.2757464528823,1.28440318015446,1.28774742812013,1.29020875530951,
1.29132760484008,1.2921713194975,1.29311669242011,1.2947302137988,1.3004808435593,
1.30626871977407,1.30930471325302,1.33737951701725,1.35694385064697,1.36156935968951,
1.36361405187422,1.36513448008221,1.36655297988812,1.36850574083191,1.37350061478156,
1.40824376170405,1.43406245578207,1.4362509610709,1.43731764330944,1.43815577309033,
1.4391336086655,1.4408478370578,1.44790386429858,1.44979800263793,1.4814650796046,
1.4970622927606,1.50613861089842,1.50877933953405,1.51042158155929,1.51193085145158,
1.5138695959426,1.51706965847292,1.54054429365722,1.56050029693511,1.57409281112921,
1.58086737186545,1.58249974582887,1.58344927734843,1.5842919696053,1.58538438367816,
1.587212905422,1.59925479608142,1.62565749930631,1.65055185824534,1.65399373811137,
1.65580975672256,1.65730363596076,1.65904288161403,1.66204349298362,1.67417871372211,
1.67859734755346,1.70855105229235,1.72445648647901,1.72756679366189,1.72879641004152,
1.72965849363162,1.73045033591453,1.73176480791234,1.73516837594106,1.75829974816944,
1.7776790180723,1.79499523856027,1.79933387057718,1.80132656348101,1.80283883844358,
1.80447169141039,1.80706983679546,1.81573374903721,1.83030588459926,1.8432544735135),
 .UNSPECIFIED.);
#1489=B_SPLINE_CURVE_WITH_KNOTS('',3,(#94228,#94229,#94230,#94231,#94232,
#94233,#94234,#94235,#94236,#94237,#94238,#94239,#94240,#94241,#94242,#94243,
#94244,#94245,#94246,#94247,#94248,#94249,#94250,#94251,#94252,#94253,#94254,
#94255,#94256,#94257,#94258,#94259,#94260,#94261,#94262,#94263,#94264,#94265,
#94266,#94267,#94268,#94269,#94270,#94271,#94272,#94273,#94274,#94275,#94276,
#94277,#94278,#94279,#94280,#94281,#94282,#94283,#94284,#94285,#94286,#94287,
#94288,#94289,#94290,#94291,#94292,#94293,#94294,#94295,#94296,#94297,#94298,
#94299,#94300,#94301,#94302,#94303,#94304,#94305,#94306,#94307,#94308,#94309,
#94310,#94311,#94312,#94313,#94314,#94315,#94316,#94317,#94318,#94319,#94320,
#94321,#94322,#94323,#94324,#94325,#94326,#94327,#94328,#94329,#94330,#94331,
#94332,#94333,#94334,#94335,#94336,#94337,#94338,#94339,#94340,#94341,#94342,
#94343,#94344,#94345,#94346,#94347,#94348,#94349,#94350,#94351,#94352,#94353,
#94354,#94355,#94356,#94357,#94358,#94359,#94360,#94361,#94362,#94363,#94364,
#94365,#94366,#94367,#94368,#94369,#94370,#94371,#94372,#94373,#94374,#94375,
#94376,#94377,#94378,#94379,#94380,#94381,#94382,#94383,#94384,#94385,#94386,
#94387,#94388,#94389,#94390,#94391,#94392,#94393,#94394,#94395,#94396,#94397,
#94398,#94399,#94400,#94401,#94402,#94403,#94404,#94405,#94406,#94407,#94408,
#94409,#94410,#94411,#94412,#94413,#94414,#94415,#94416,#94417,#94418,#94419,
#94420,#94421,#94422,#94423,#94424,#94425,#94426,#94427,#94428,#94429,#94430,
#94431,#94432,#94433,#94434,#94435,#94436,#94437,#94438,#94439,#94440,#94441,
#94442,#94443,#94444,#94445,#94446,#94447,#94448,#94449,#94450,#94451,#94452,
#94453),.UNSPECIFIED.,.F.,.F.,(4,2,2,2,2,2,2,2,2,2,2,2,2,2,2,2,2,2,2,2,
2,2,2,2,2,2,2,2,2,2,2,2,2,2,2,2,2,2,2,2,2,2,2,2,2,2,2,2,2,2,2,2,2,2,2,2,
2,2,2,2,2,2,2,2,2,2,2,2,2,2,2,2,2,2,2,2,2,2,2,2,2,2,2,2,2,2,2,2,2,2,2,2,
2,2,2,2,2,2,2,2,2,2,2,2,2,2,2,2,2,2,2,2,4),(0.717606620371918,0.724937303735731,
0.72771389595266,0.72888278799588,0.729730165448876,0.730647726823811,0.732136308992316,
0.73678160719935,0.768402239729924,0.796423821392427,0.799925976396239,
0.80175695640325,0.803254677655556,0.804988896032012,0.807957585117534,
0.819622552326261,0.864542031817913,0.872241162803488,0.874009203477053,
0.875001700919868,0.875832872735957,0.876882871898634,0.878984749072429,
0.89957509783129,0.929771591109237,0.942756162588134,0.945819933785195,
0.947573744537744,0.948917873732766,0.950656544863179,0.95373524925088,
0.968601891243069,1.0040053419056,1.00701040447089,1.01785002831095,1.01963014616438,
1.02070808014087,1.02154842329556,1.02250507618966,1.02417287734539,1.03144459367853,
1.04667321819947,1.0863368694704,1.09095248756988,1.09278982277997,1.09431726656705,
1.09588378280359,1.09818012924158,1.10439888502929,1.13531603198701,1.16165487700035,
1.16503396067604,1.16634340607445,1.16713352886259,1.16799583108429,1.16922778679252,
1.17235396922868,1.18842502050758,1.21720898018135,1.2243668936313,1.23501452377013,
1.23792210383151,1.23962329924067,1.24110633894059,1.24296628002408,1.24662074531124,
1.27806483870237,1.30767612503891,1.3109392755739,1.31223116949292,1.31301889491692,
1.31388493343726,1.31513511845046,1.31837872927036,1.33567699042397,1.34803104693547,
1.37716376910126,1.38233104206709,1.38453078151396,1.38606357113137,1.38762727790221,
1.38990429049629,1.39597850367512,1.42192912837342,1.42776626852438,1.45338219518245,
1.45677440129569,1.45808673156896,1.45887794155059,1.45973989963584,1.46097028512708,
1.46395167097746,1.46830742711889,1.48119288853573,1.50699447052287,1.5258449547263,
1.5289267787661,1.53085073164652,1.53235323409534,1.53401829323474,1.53573667617848,
1.54145490323515,1.55968522198252,1.57484523843323,1.59922670856218,1.6026316006263,
1.60394594253714,1.60473751311349,1.6055992434061,1.60682804040949,1.6082209491119,
1.61365131628245,1.63904789497656),.UNSPECIFIED.);
#1490=B_SPLINE_CURVE_WITH_KNOTS('',3,(#94454,#94455,#94456,#94457),
 .UNSPECIFIED.,.F.,.F.,(4,4),(0.000428749880585189,0.00056079372868648),
 .UNSPECIFIED.);
#1491=B_SPLINE_CURVE_WITH_KNOTS('',3,(#94458,#94459,#94460,#94461,#94462,
#94463,#94464,#94465,#94466,#94467,#94468,#94469,#94470,#94471,#94472,#94473,
#94474,#94475,#94476,#94477,#94478,#94479,#94480,#94481,#94482,#94483,#94484,
#94485,#94486,#94487,#94488,#94489,#94490,#94491,#94492,#94493,#94494,#94495,
#94496,#94497,#94498,#94499,#94500,#94501,#94502,#94503,#94504,#94505,#94506,
#94507,#94508,#94509,#94510,#94511,#94512,#94513,#94514,#94515,#94516,#94517,
#94518,#94519,#94520,#94521,#94522,#94523,#94524,#94525,#94526,#94527,#94528,
#94529,#94530,#94531,#94532,#94533,#94534,#94535,#94536,#94537,#94538,#94539,
#94540,#94541,#94542,#94543,#94544,#94545,#94546,#94547,#94548,#94549,#94550,
#94551,#94552,#94553,#94554,#94555,#94556,#94557,#94558,#94559,#94560,#94561,
#94562,#94563,#94564,#94565,#94566,#94567,#94568,#94569,#94570,#94571,#94572,
#94573,#94574,#94575,#94576,#94577,#94578,#94579,#94580,#94581,#94582,#94583,
#94584,#94585,#94586,#94587,#94588,#94589,#94590,#94591,#94592,#94593,#94594,
#94595,#94596,#94597,#94598,#94599,#94600,#94601,#94602,#94603,#94604,#94605,
#94606,#94607,#94608,#94609,#94610,#94611,#94612,#94613,#94614,#94615,#94616,
#94617,#94618,#94619,#94620,#94621,#94622,#94623,#94624,#94625,#94626,#94627,
#94628,#94629,#94630,#94631,#94632,#94633,#94634,#94635,#94636,#94637,#94638,
#94639,#94640,#94641,#94642,#94643,#94644,#94645,#94646,#94647,#94648,#94649,
#94650,#94651,#94652,#94653,#94654,#94655,#94656,#94657,#94658,#94659,#94660,
#94661,#94662,#94663,#94664,#94665,#94666,#94667,#94668,#94669,#94670,#94671,
#94672,#94673,#94674,#94675,#94676,#94677,#94678,#94679,#94680,#94681,#94682,
#94683),.UNSPECIFIED.,.F.,.F.,(4,2,2,2,2,2,2,2,2,2,2,2,2,2,2,2,2,2,2,2,
2,2,2,2,2,2,2,2,2,2,2,2,2,2,2,2,2,2,2,2,2,2,2,2,2,2,2,2,2,2,2,2,2,2,2,2,
2,2,2,2,2,2,2,2,2,2,2,2,2,2,2,2,2,2,2,2,2,2,2,2,2,2,2,2,2,2,2,2,2,2,2,2,
2,2,2,2,2,2,2,2,2,2,2,2,2,2,2,2,2,2,2,2,4),(1.8432544735135,1.8581363739033,
1.86112220837997,1.87199099534198,1.87377297983242,1.87485174794923,1.87569273833946,
1.87665041392195,1.87831976961295,1.88559534826818,1.90083125139594,1.94046777125858,
1.94508724735617,1.9469265328112,1.94845578117905,1.95002434981121,1.95232410921401,
1.95855499105206,1.98926037353949,2.01576739741428,2.01914140474939,2.0204510073231,
2.02124186120728,2.02210465525392,2.02333827005434,2.02647444683507,2.04264654034132,
2.07066897754576,2.08827570540849,2.09131882588206,2.09323143629484,2.09473306762275,
2.09640540121951,2.09918284141753,2.10973086876282,2.12934522951758,2.16212278622311,
2.16514227758109,2.16626877159969,2.16706797513093,2.16792435908762,2.16912325548418,
2.17204283790939,2.18608753455905,2.22793132200851,2.23563790852107,2.23822074099923,
2.23985010818368,2.2413633813349,2.24336364012969,2.24774402244608,2.26537775381782,
2.28448711846242,2.3093890232548,2.3115227903059,2.31257843230654,2.31341554963876,
2.3144011018584,2.31619896006248,2.32559914920328,2.37521258159991,2.38185828637151,
2.38429442281185,2.38573169728544,2.38724101307681,2.38921809666859,2.39347639338184,
2.41019678982574,2.44004992322427,2.44578951561498,2.45563738933412,2.45736886604957,
2.45844380758605,2.45928217985398,2.4602531541547,2.461984427979,2.47020720730987,
2.48893603076886,2.52326417040624,2.52828263426371,2.53023875068998,2.53165769187546,
2.53317672403976,2.53521628682881,2.53981618777728,2.55918022556685,2.58945059709051,
2.60129966026234,2.60312060653294,2.60421064523502,2.60505295477509,2.60600390272237,
2.60764216152916,2.6144911394687,2.62832325001618,2.64523808840187,2.67134918821194,
2.67457170201162,2.67651697086531,2.67802714538887,2.67966619221896,2.68229264239869,
2.69122951398775,2.70647487972667,2.72536440763726,2.74679920447638,2.74898103650369,
2.75004613345169,2.75088344515566,2.75186049662732,2.75362245727572,2.76238681864969,
2.76458849571582),.UNSPECIFIED.);
#1492=B_SPLINE_CURVE_WITH_KNOTS('',3,(#94689,#94690,#94691,#94692,#94693,
#94694,#94695,#94696,#94697,#94698,#94699,#94700,#94701,#94702,#94703,#94704,
#94705,#94706,#94707,#94708,#94709,#94710,#94711,#94712,#94713,#94714,#94715,
#94716,#94717,#94718,#94719,#94720,#94721,#94722,#94723,#94724,#94725,#94726,
#94727,#94728,#94729,#94730,#94731,#94732,#94733,#94734,#94735,#94736,#94737,
#94738,#94739,#94740,#94741,#94742,#94743,#94744,#94745,#94746,#94747,#94748,
#94749,#94750,#94751,#94752,#94753,#94754,#94755,#94756,#94757,#94758,#94759,
#94760,#94761,#94762,#94763,#94764,#94765,#94766,#94767,#94768,#94769,#94770,
#94771,#94772,#94773,#94774,#94775,#94776,#94777,#94778,#94779,#94780,#94781,
#94782,#94783,#94784,#94785,#94786,#94787,#94788,#94789,#94790,#94791,#94792,
#94793,#94794,#94795,#94796,#94797,#94798,#94799,#94800,#94801,#94802),
 .UNSPECIFIED.,.F.,.F.,(4,2,2,2,2,2,2,2,2,2,2,2,2,2,2,2,2,2,2,2,2,2,2,2,
2,2,2,2,2,2,2,2,2,2,2,2,2,2,2,2,2,2,2,2,2,2,2,2,2,2,2,2,2,2,2,2,4),(-0.423911080838966,
-0.405908211040072,-0.402945684174472,-0.401057530385946,-0.399554399235692,
-0.397855357586041,-0.394963617425683,-0.382532843334228,-0.350771365776667,
-0.344155903874234,-0.342492928273389,-0.341527363314198,-0.340772431801499,
-0.339720645055032,-0.337575447171142,-0.318902188176821,-0.289632196839236,
-0.285408451687143,-0.283470616792185,-0.281969865296512,-0.2803418803254,
-0.277727928237807,-0.268593217070172,-0.23944422163428,-0.226992082995754,
-0.225204556914693,-0.224128704593718,-0.223289083878224,-0.222318390100464,
-0.220589885175706,-0.212188939951695,-0.19030078397516,-0.170407573432568,
-0.167425713515098,-0.165529010270916,-0.164021556253698,-0.162320256413333,
-0.159431029504583,-0.147102952224871,-0.115896794955732,-0.108940542391568,
-0.10724034705368,-0.106260105942312,-0.10541646138879,-0.104312932188852,
-0.103083802959583,-0.101020854601744,-0.0966688858107392,-0.0659538254154411,
-0.0539488960812429,-0.0509875805156346,-0.0492411068141357,-0.0477186667861302,
-0.0458353018362169,-0.042144008099143,-0.0181099242452841,-9.99999997863821E-7),
 .UNSPECIFIED.);
#1493=B_SPLINE_CURVE_WITH_KNOTS('',3,(#94805,#94806,#94807,#94808,#94809,
#94810,#94811,#94812,#94813,#94814,#94815,#94816,#94817,#94818,#94819,#94820,
#94821,#94822,#94823,#94824,#94825,#94826,#94827,#94828,#94829,#94830,#94831,
#94832,#94833,#94834,#94835,#94836,#94837,#94838,#94839,#94840,#94841,#94842,
#94843,#94844,#94845,#94846,#94847,#94848,#94849,#94850,#94851,#94852,#94853,
#94854,#94855,#94856,#94857,#94858,#94859,#94860,#94861,#94862,#94863,#94864,
#94865,#94866,#94867,#94868,#94869,#94870,#94871,#94872,#94873,#94874,#94875,
#94876,#94877,#94878,#94879,#94880,#94881,#94882,#94883,#94884,#94885,#94886),
 .UNSPECIFIED.,.F.,.F.,(4,3,3,3,3,3,3,3,3,3,3,3,3,3,3,3,3,3,3,3,3,3,3,3,
3,3,3,4),(11.6159397475004,11.7279534302045,11.7402765323561,11.8627684357717,
11.9852329360532,12.1077126178578,12.2334429699799,12.3561779531201,12.4834059897331,
12.5952366943264,12.6106340263461,12.6106792268383,12.718077365594,12.7349708112018,
12.8532987602863,12.9714916814451,13.0896045359157,13.2076921393023,13.3258929009561,
13.4441598868657,13.5566380093714,13.5626466500754,13.6053283051919,13.6053817568075,
13.7129385955191,13.725252783422,13.8508263858764,13.9763998223961),
 .UNSPECIFIED.);
#1494=B_SPLINE_CURVE_WITH_KNOTS('',3,(#94891,#94892,#94893,#94894,#94895,
#94896,#94897,#94898,#94899,#94900,#94901,#94902,#94903,#94904,#94905,#94906,
#94907,#94908,#94909,#94910,#94911,#94912,#94913,#94914,#94915,#94916,#94917,
#94918,#94919,#94920,#94921,#94922,#94923,#94924,#94925,#94926,#94927,#94928,
#94929,#94930,#94931,#94932,#94933,#94934,#94935,#94936,#94937,#94938,#94939,
#94940,#94941,#94942,#94943,#94944,#94945,#94946,#94947,#94948,#94949,#94950,
#94951,#94952,#94953,#94954,#94955,#94956,#94957,#94958,#94959,#94960,#94961,
#94962,#94963,#94964,#94965,#94966,#94967,#94968,#94969,#94970,#94971,#94972,
#94973,#94974,#94975,#94976,#94977,#94978,#94979,#94980,#94981,#94982,#94983,
#94984,#94985,#94986,#94987,#94988,#94989,#94990,#94991,#94992,#94993,#94994,
#94995,#94996,#94997,#94998,#94999,#95000,#95001,#95002,#95003,#95004,#95005,
#95006,#95007,#95008,#95009,#95010,#95011,#95012,#95013,#95014,#95015,#95016,
#95017,#95018,#95019,#95020,#95021,#95022,#95023,#95024,#95025,#95026,#95027,
#95028,#95029,#95030,#95031,#95032,#95033,#95034,#95035,#95036,#95037,#95038,
#95039,#95040,#95041,#95042,#95043,#95044,#95045,#95046,#95047,#95048,#95049,
#95050,#95051,#95052,#95053,#95054,#95055,#95056,#95057,#95058,#95059,#95060,
#95061,#95062,#95063,#95064,#95065,#95066,#95067,#95068,#95069,#95070,#95071,
#95072,#95073,#95074,#95075,#95076,#95077,#95078,#95079,#95080,#95081,#95082,
#95083,#95084,#95085,#95086,#95087,#95088,#95089,#95090,#95091,#95092,#95093,
#95094,#95095,#95096,#95097,#95098,#95099,#95100,#95101,#95102,#95103,#95104,
#95105,#95106,#95107,#95108),.UNSPECIFIED.,.F.,.F.,(4,2,2,2,2,2,2,2,2,2,
2,2,2,2,2,2,2,2,2,2,2,2,2,2,2,2,2,2,2,2,2,2,2,2,2,2,2,2,2,2,2,2,2,2,2,2,
2,2,2,2,2,2,2,2,2,2,2,2,2,2,2,2,2,2,2,2,2,2,2,2,2,2,2,2,2,2,2,2,2,2,2,2,
2,2,2,2,2,2,2,2,2,2,2,2,2,2,2,2,2,2,2,2,2,2,2,2,2,2,4),(-1.16578625258722,
-1.16495654187368,-1.16387501348904,-1.16303297303707,-1.1620629866672,
-1.16033394485289,-1.15188727820847,-1.12963412033475,-1.1104469835436,
-1.10748738777761,-1.10560281206173,-1.10410373135837,-1.10241061282265,
-1.09953244228331,-1.0872267352026,-1.05637041394269,-1.04889684686108,
-1.04716995475504,-1.0461901107729,-1.04534952929034,-1.04426464835453,
-1.04197498292351,-1.03889883285415,-1.03104273656382,-1.0063481291354,
-0.992640476299625,-0.9895944166997,-0.987846825113856,-0.98636714294917,
-0.984562623157298,-0.981162977683459,-0.976890565698702,-0.967198668382222,
-0.951556633460711,-0.933393821295391,-0.930455067393325,-0.929341844000728,
-0.928546592610655,-0.927681699048231,-0.926436143859374,-0.92320457470987,
-0.918368552294689,-0.902034378221544,-0.877501261995395,-0.872984035893418,
-0.870985689089877,-0.869467053799717,-0.867847658102225,-0.865306839995702,
-0.85700970951092,-0.827093006994181,-0.820444421276279,-0.813894183147314,
-0.812237116229529,-0.811273136987149,-0.810514063718278,-0.809450436543141,
-0.807272889010454,-0.789683323536542,-0.759416520850773,-0.755328828738471,
-0.753386932804677,-0.75188091242938,-0.750219519245063,-0.747488586636999,
-0.73717713213949,-0.71748982862789,-0.698511044436333,-0.695567413783529,
-0.694453463778226,-0.693657870737538,-0.692793767140101,-0.691549919168422,
-0.688325103285038,-0.683501581693507,-0.667239799232136,-0.642592123635406,
-0.638078649210613,-0.636082078756564,-0.634564871758043,-0.632947093886349,
-0.630409058292278,-0.62212431160859,-0.592230577070229,-0.585590872619476,
-0.578989339942265,-0.577329024853092,-0.576364892165802,-0.575606739190672,
-0.574545905558548,-0.572379782936935,-0.552910823499936,-0.524785970609621,
-0.520458360306892,-0.518493129209306,-0.516979169580948,-0.51534463755178,
-0.512736781622201,-0.503789355310463,-0.47429073229228,-0.462011770044367,
-0.460223268836459,-0.459143190738879,-0.458299202617069,-0.457322322059325,
-0.45557387726905,-0.446865573376514,-0.429016188564468,-0.423911080838966),
 .UNSPECIFIED.);
#1495=B_SPLINE_CURVE_WITH_KNOTS('',3,(#95109,#95110,#95111,#95112,#95113,
#95114,#95115,#95116,#95117,#95118,#95119,#95120,#95121,#95122,#95123,#95124,
#95125,#95126,#95127,#95128,#95129,#95130,#95131,#95132,#95133,#95134,#95135,
#95136,#95137,#95138,#95139,#95140,#95141,#95142,#95143,#95144,#95145,#95146,
#95147,#95148,#95149,#95150,#95151,#95152,#95153,#95154,#95155,#95156,#95157,
#95158,#95159,#95160,#95161,#95162,#95163,#95164,#95165,#95166,#95167,#95168,
#95169,#95170,#95171,#95172,#95173,#95174,#95175,#95176,#95177,#95178,#95179,
#95180,#95181,#95182,#95183,#95184,#95185,#95186,#95187,#95188,#95189,#95190,
#95191,#95192,#95193,#95194,#95195,#95196,#95197,#95198,#95199,#95200,#95201,
#95202,#95203,#95204,#95205,#95206,#95207,#95208,#95209,#95210,#95211,#95212,
#95213,#95214,#95215,#95216,#95217,#95218,#95219,#95220,#95221,#95222,#95223,
#95224,#95225,#95226,#95227,#95228,#95229,#95230,#95231,#95232,#95233,#95234,
#95235,#95236,#95237,#95238,#95239,#95240,#95241,#95242,#95243,#95244,#95245,
#95246,#95247,#95248,#95249,#95250,#95251,#95252,#95253,#95254,#95255,#95256,
#95257,#95258,#95259,#95260,#95261,#95262,#95263,#95264,#95265,#95266,#95267,
#95268,#95269,#95270,#95271,#95272,#95273,#95274,#95275,#95276,#95277,#95278,
#95279,#95280,#95281,#95282,#95283,#95284,#95285,#95286,#95287,#95288,#95289,
#95290,#95291,#95292,#95293,#95294,#95295,#95296,#95297,#95298,#95299,#95300,
#95301,#95302,#95303,#95304,#95305,#95306,#95307,#95308,#95309,#95310,#95311,
#95312,#95313,#95314,#95315,#95316,#95317,#95318,#95319,#95320,#95321,#95322,
#95323,#95324,#95325,#95326,#95327,#95328,#95329,#95330,#95331,#95332,#95333,
#95334,#95335,#95336,#95337,#95338,#95339,#95340,#95341,#95342,#95343,#95344,
#95345,#95346,#95347,#95348,#95349,#95350,#95351,#95352,#95353,#95354,#95355,
#95356,#95357,#95358,#95359,#95360),.UNSPECIFIED.,.F.,.F.,(4,2,2,2,2,2,
2,2,2,2,2,2,2,2,2,2,2,2,2,2,2,2,2,2,2,2,2,2,2,2,2,2,2,2,2,2,2,2,2,2,2,2,
2,2,2,2,2,2,2,2,2,2,2,2,2,2,2,2,2,2,2,2,2,2,2,2,2,2,2,2,2,2,2,2,2,2,2,2,
2,2,2,2,2,2,2,2,2,2,2,2,2,2,2,2,2,2,2,2,2,2,2,2,2,2,2,2,2,2,2,2,2,2,2,2,
2,2,2,2,2,2,2,2,2,2,2,4),(-3.17187947594733,-3.16473921561708,-3.16044316022415,
-3.15846517394355,-3.15695858374128,-3.15550482049477,-3.15406538677774,
-3.15208883016073,-3.14702675590512,-3.13661888044744,-3.11307841034839,
-3.10170138613847,-3.09980716171223,-3.09878428835165,-3.09801338455359,
-3.09697594603795,-3.09501861920091,-3.08313200236917,-3.06093000735926,
-3.05061394924129,-3.04615428213288,-3.04266380028948,-3.04084529016682,
-3.04082970367069,-3.04081308834817,-3.04079537316206,-3.04077648185846,
-3.04075633252447,-3.04073483719827,-3.04071190137564,-3.0406874234969,
-3.04066129445413,-3.04063339698503,-3.04060360512891,-3.04057178360287,
-3.04053778717087,-3.04051430308288,-3.04048217521517,-3.04043825415266,
-3.04037827706347,-3.04021217474066,-3.03868567534402,-3.03667384093241,
-3.03211184985238,-3.0077630940736,-2.99109257182972,-2.98619608800655,
-2.98293338566112,-2.98168248022944,-2.98081636090251,-2.98002687645685,
-2.97892473992055,-2.97604294642776,-2.95505059765632,-2.92818487901805,
-2.92479986426057,-2.92300643314673,-2.92166802083699,-2.91998339613827,
-2.91710777801048,-2.90622305090127,-2.88241214551628,-2.86803096211046,
-2.86515617296928,-2.86397305226884,-2.86312331737095,-2.86231496670698,
-2.86091410110994,-2.85689131048492,-2.82232135423191,-2.80962358938941,
-2.80671604439528,-2.80501425651505,-2.80351265896253,-2.80163169890575,
-2.79869077066792,-2.78059942225208,-2.75753930416373,-2.74896173234075,
-2.74722111813196,-2.74624631948059,-2.74540265460367,-2.74432113162423,
-2.74252649138957,-2.73005240772113,-2.70030937760648,-2.69176898761776,
-2.68920302699147,-2.68757829101405,-2.6860620585469,-2.6840775962008,-2.67963839706581,
-2.65309963755078,-2.63219491261709,-2.63003427031576,-2.62897490286081,
-2.62821730997577,-2.6272532254352,-2.62559159585125,-2.61896608146239,
-2.61234247874397,-2.58246684431845,-2.57420731415295,-2.57167292818137,
-2.57005657166638,-2.56854006816777,-2.56654351167923,-2.5620261450634,
-2.53753545536722,-2.52114250077137,-2.51629823951272,-2.51306381837714,
-2.51181894868876,-2.51095501667289,-2.51016029464169,-2.50904853637329,
-2.50611857824521,-2.48765980805246,-2.46759729142429,-2.457178204582,-2.45443942572901,
-2.45277690884135,-2.45127222392516,-2.44933536282734,-2.44527082756646,
-2.43011734130913),.UNSPECIFIED.);
#1496=B_SPLINE_CURVE_WITH_KNOTS('',3,(#95365,#95366,#95367,#95368,#95369,
#95370,#95371,#95372,#95373,#95374,#95375,#95376,#95377,#95378,#95379,#95380,
#95381,#95382,#95383,#95384,#95385,#95386,#95387,#95388,#95389,#95390,#95391,
#95392,#95393,#95394,#95395,#95396,#95397,#95398,#95399,#95400,#95401,#95402,
#95403,#95404,#95405,#95406,#95407,#95408,#95409,#95410,#95411,#95412,#95413,
#95414,#95415,#95416,#95417,#95418,#95419,#95420,#95421,#95422,#95423,#95424,
#95425,#95426,#95427,#95428,#95429,#95430,#95431,#95432,#95433,#95434,#95435,
#95436,#95437,#95438,#95439,#95440,#95441,#95442,#95443,#95444,#95445,#95446,
#95447,#95448,#95449,#95450,#95451,#95452,#95453,#95454,#95455,#95456,#95457,
#95458,#95459,#95460,#95461,#95462,#95463,#95464,#95465,#95466,#95467,#95468,
#95469,#95470,#95471,#95472,#95473,#95474,#95475,#95476,#95477,#95478,#95479,
#95480,#95481,#95482,#95483,#95484,#95485,#95486,#95487,#95488,#95489,#95490,
#95491,#95492,#95493,#95494,#95495,#95496,#95497,#95498,#95499,#95500,#95501,
#95502,#95503,#95504,#95505,#95506,#95507,#95508,#95509,#95510,#95511,#95512,
#95513,#95514,#95515,#95516,#95517,#95518,#95519,#95520,#95521,#95522,#95523,
#95524,#95525,#95526,#95527,#95528,#95529,#95530,#95531,#95532,#95533,#95534,
#95535,#95536,#95537,#95538,#95539,#95540,#95541,#95542,#95543,#95544,#95545,
#95546,#95547,#95548,#95549,#95550,#95551,#95552,#95553,#95554,#95555,#95556,
#95557,#95558,#95559,#95560,#95561,#95562,#95563,#95564,#95565,#95566,#95567,
#95568),.UNSPECIFIED.,.F.,.F.,(4,2,2,2,2,2,2,2,2,2,2,2,2,2,2,2,2,2,2,2,
2,2,2,2,2,2,2,2,2,2,2,2,2,2,2,2,2,2,2,2,2,2,2,2,2,2,2,2,2,2,2,2,2,2,2,2,
2,2,2,2,2,2,2,2,2,2,2,2,2,2,2,2,2,2,2,2,2,2,2,2,2,2,2,2,2,2,2,2,2,2,2,2,
2,2,2,2,2,2,2,2,2,4),(-1.90752595100115,-1.88362007859244,-1.87112823595947,
-1.86923240311331,-1.86822682861868,-1.86738863321829,-1.86633766927285,
-1.86468173537945,-1.8557597745918,-1.83061280324773,-1.82000118008745,
-1.81545898028867,-1.81189055818152,-1.81005141379379,-1.80855615675114,
-1.80683182606532,-1.80388768999709,-1.79176290704775,-1.76603521218253,
-1.75475694109299,-1.75219701800133,-1.75106212471271,-1.75021593980457,
-1.74926644958552,-1.74763045583421,-1.74153093645605,-1.70930448767715,
-1.69684311878572,-1.69395531811923,-1.69226035765088,-1.69076196957358,
-1.68888136103131,-1.68593406072472,-1.66747583626637,-1.64456837248137,
-1.63601254258091,-1.63427770759079,-1.63330661495954,-1.63246496521011,
-1.63138569179719,-1.62959662607504,-1.61723848958478,-1.58779912984415,
-1.57887860735567,-1.57627473302151,-1.57464193181266,-1.57312906146327,
-1.57116451827422,-1.56786265759568,-1.54203959778174,-1.52568792496754,
-1.52084946018167,-1.51761716182718,-1.51637162997539,-1.51550684957953,
-1.51471173461568,-1.51359879543186,-1.51066130463228,-1.49252208165286,
-1.47691089020177,-1.46721161593233,-1.46085672556273,-1.45855022034882,
-1.45698086817229,-1.45545090116724,-1.45360756069512,-1.449118910736,-1.42706666905852,
-1.40284243785337,-1.40011138653267,-1.3990297660391,-1.39824275966789,
-1.39736994698105,-1.39608427528726,-1.39257836425615,-1.37040107937369,
-1.34728885334641,-1.34274930355675,-1.34074733930023,-1.33922838715297,
-1.3376109883521,-1.33507819770006,-1.32685280826892,-1.29689557226867,
-1.29025670941099,-1.28366196973957,-1.28200159105016,-1.28103707627179,
-1.28027871311056,-1.27921745288886,-1.27704907926542,-1.2560123952169,
-1.22970667905637,-1.22526151599802,-1.22327608557229,-1.22175977128464,
-1.22013558524442,-1.21757185672893,-1.20905283779287,-1.179309962143,-1.16675301095494,
-1.16578625258722),.UNSPECIFIED.);
#1497=B_SPLINE_CURVE_WITH_KNOTS('',3,(#95569,#95570,#95571,#95572,#95573,
#95574,#95575,#95576,#95577,#95578,#95579,#95580,#95581,#95582,#95583,#95584,
#95585,#95586,#95587,#95588,#95589,#95590,#95591,#95592,#95593,#95594,#95595,
#95596,#95597,#95598,#95599,#95600,#95601,#95602,#95603,#95604,#95605,#95606,
#95607,#95608,#95609,#95610,#95611,#95612,#95613,#95614,#95615,#95616,#95617,
#95618,#95619,#95620,#95621,#95622,#95623,#95624,#95625,#95626,#95627,#95628,
#95629,#95630,#95631,#95632,#95633,#95634,#95635,#95636,#95637,#95638,#95639,
#95640,#95641,#95642,#95643,#95644,#95645,#95646,#95647,#95648,#95649,#95650,
#95651,#95652,#95653,#95654,#95655,#95656,#95657,#95658,#95659,#95660,#95661,
#95662,#95663,#95664,#95665,#95666,#95667,#95668,#95669,#95670,#95671,#95672,
#95673,#95674,#95675,#95676,#95677,#95678,#95679,#95680,#95681,#95682,#95683,
#95684,#95685,#95686,#95687,#95688,#95689,#95690,#95691,#95692,#95693,#95694,
#95695,#95696,#95697,#95698,#95699,#95700,#95701,#95702,#95703,#95704,#95705,
#95706,#95707,#95708,#95709,#95710,#95711,#95712,#95713,#95714,#95715,#95716,
#95717,#95718,#95719,#95720,#95721,#95722,#95723,#95724,#95725,#95726,#95727,
#95728,#95729,#95730,#95731,#95732,#95733,#95734,#95735,#95736,#95737,#95738,
#95739,#95740,#95741,#95742,#95743,#95744,#95745,#95746,#95747,#95748,#95749,
#95750,#95751,#95752,#95753,#95754,#95755,#95756,#95757,#95758,#95759,#95760,
#95761,#95762,#95763,#95764,#95765,#95766,#95767,#95768,#95769,#95770,#95771,
#95772,#95773,#95774,#95775,#95776,#95777,#95778,#95779,#95780,#95781,#95782,
#95783,#95784,#95785,#95786,#95787,#95788,#95789,#95790),.UNSPECIFIED.,
 .F.,.F.,(4,2,2,2,2,2,2,2,2,2,2,2,2,2,2,2,2,2,2,2,2,2,2,2,2,2,2,2,2,2,2,
2,2,2,2,2,2,2,2,2,2,2,2,2,2,2,2,2,2,2,2,2,2,2,2,2,2,2,2,2,2,2,2,2,2,2,2,
2,2,2,2,2,2,2,2,2,2,2,2,2,2,2,2,2,2,2,2,2,2,2,2,2,2,2,2,2,2,2,2,2,2,2,2,
2,2,2,2,2,2,2,4),(-2.43011734130913,-2.41481597979633,-2.39735880329152,
-2.3951857239436,-2.39412332080614,-2.39336474106553,-2.39240087403877,
-2.39074293165702,-2.38417507960966,-2.37754099977846,-2.34765118013879,
-2.33936461579502,-2.33682578563583,-2.33520738364571,-2.33368949355389,
-2.33169186189631,-2.32717517701453,-2.30262989511402,-2.28628960318989,
-2.2814530635049,-2.27822188698461,-2.27697677552855,-2.27611229495503,
-2.27531751752274,-2.27420510798581,-2.27126957426423,-2.25308987489998,
-2.23741153811376,-2.22777208390113,-2.22144585230775,-2.21914379736487,
-2.21757578345002,-2.21604583130719,-2.21385756719043,-2.2098303906548,
-2.18405653985788,-2.16250179614377,-2.16033255818783,-2.15927139526951,
-2.15851328196107,-2.15754930103005,-2.15589057139364,-2.14931192937181,
-2.14267957413884,-2.11279472797624,-2.10450682264593,-2.10196773305272,
-2.10034919926566,-2.09883120778007,-2.09683347215035,-2.09231665468224,
-2.06780511780435,-2.0514485793426,-2.04660938853951,-2.04337679968161,
-2.04213131911732,-2.04126663773164,-2.0404717332308,-2.0393591730667,-2.0364234808381,
-2.01824308175593,-2.00256287380938,-1.99292551321565,-1.98660010744146,
-1.98429796104629,-1.98272976567177,-1.9811995425484,-1.97901072271622,
-1.97498207079746,-1.94923880548864,-1.92765532393432,-1.9254858153486,
-1.92442451582824,-1.92366634347788,-1.92270237944221,-1.92104366308279,
-1.91446490803787,-1.90783238510119,-1.87794963104795,-1.86965969423404,
-1.86712048027951,-1.86550198325893,-1.86398410929363,-1.86198665203645,
-1.85747102856351,-1.83290660094356,-1.81658592119984,-1.81175256170352,
-1.8085229096544,-1.80727793881097,-1.80641340280718,-1.80561840504782,
-1.80450551193352,-1.80156717702645,-1.78343911347554,-1.76785126220425,
-1.75812539288814,-1.75384296291085,-1.75043697141373,-1.74863147700218,
-1.74715220089815,-1.74540650430903,-1.74236735281841,-1.72878470509405,
-1.70397250207422,-1.69608978396245,-1.69300705029047,-1.69071388327278,
-1.68962851881294,-1.68879575725663,-1.68837727951077),.UNSPECIFIED.);
#1498=B_SPLINE_CURVE_WITH_KNOTS('',3,(#95795,#95796,#95797,#95798,#95799,
#95800,#95801,#95802,#95803,#95804,#95805,#95806,#95807,#95808,#95809,#95810,
#95811,#95812,#95813,#95814,#95815,#95816,#95817,#95818,#95819,#95820,#95821,
#95822,#95823,#95824,#95825,#95826,#95827,#95828,#95829,#95830,#95831,#95832,
#95833,#95834,#95835,#95836,#95837,#95838,#95839,#95840,#95841,#95842,#95843,
#95844,#95845,#95846,#95847,#95848,#95849,#95850,#95851,#95852,#95853,#95854,
#95855,#95856,#95857,#95858,#95859,#95860,#95861,#95862,#95863,#95864,#95865,
#95866,#95867,#95868,#95869,#95870,#95871,#95872,#95873,#95874,#95875,#95876,
#95877,#95878,#95879,#95880,#95881,#95882,#95883,#95884,#95885,#95886,#95887,
#95888,#95889,#95890,#95891,#95892,#95893,#95894,#95895,#95896,#95897,#95898,
#95899,#95900,#95901,#95902,#95903,#95904,#95905,#95906,#95907,#95908,#95909,
#95910,#95911,#95912,#95913,#95914,#95915,#95916,#95917,#95918,#95919,#95920,
#95921,#95922,#95923,#95924,#95925,#95926,#95927,#95928,#95929,#95930,#95931,
#95932,#95933,#95934,#95935,#95936,#95937,#95938,#95939,#95940,#95941,#95942,
#95943,#95944,#95945,#95946,#95947,#95948,#95949,#95950,#95951,#95952,#95953,
#95954,#95955,#95956,#95957,#95958,#95959,#95960,#95961,#95962,#95963,#95964,
#95965,#95966,#95967,#95968,#95969,#95970,#95971,#95972,#95973,#95974,#95975,
#95976,#95977,#95978,#95979,#95980,#95981,#95982,#95983,#95984,#95985,#95986,
#95987,#95988,#95989,#95990,#95991,#95992,#95993,#95994,#95995,#95996,#95997,
#95998,#95999,#96000,#96001,#96002,#96003,#96004,#96005,#96006,#96007,#96008,
#96009,#96010),.UNSPECIFIED.,.F.,.F.,(4,2,2,2,2,2,2,2,2,2,2,2,2,2,2,2,2,
2,2,2,2,2,2,2,2,2,2,2,2,2,2,2,2,2,2,2,2,2,2,2,2,2,2,2,2,2,2,2,2,2,2,2,2,
2,2,2,2,2,2,2,2,2,2,2,2,2,2,2,2,2,2,2,2,2,2,2,2,2,2,2,2,2,2,2,2,2,2,2,2,
2,2,2,2,2,2,2,2,2,2,2,2,2,2,2,2,2,2,4),(-2.64925299467486,-2.64439351024018,
-2.63565889459159,-2.63307331472224,-2.63144440576356,-2.62992995093017,
-2.62795594218273,-2.62357474183728,-2.59619746795857,-2.57586934090486,
-2.57385329507439,-2.57282268699081,-2.57206719318075,-2.57107948403193,
-2.56931753007274,-2.56131765817323,-2.53100239768952,-2.51876962769625,
-2.51589668789644,-2.51420488438948,-2.51270589196559,-2.51081999124654,
-2.50785545885685,-2.48503067071668,-2.46864116774041,-2.46155619862553,
-2.45868673852026,-2.45651796612064,-2.45545665759374,-2.45469832475683,
-2.45373392202227,-2.45207391558962,-2.44548261860415,-2.43885340813565,
-2.40892171742417,-2.40068743612303,-2.39815377975433,-2.39653623048402,
-2.3950174179726,-2.39301604707854,-2.38847968822856,-2.36676311390131,
-2.34820482573476,-2.34302860948065,-2.33963065150869,-2.33836052006936,
-2.3374908864139,-2.33670096754575,-2.33560785923745,-2.33280833504335,
-2.30996599499759,-2.28482659429243,-2.2814493210076,-2.27964963938307,
-2.27817035326332,-2.27641902530293,-2.27335569285477,-2.25930627414214,
-2.22659252383275,-2.22377608093784,-2.22163863865929,-2.22058351565617,
-2.21982582960366,-2.21885704792273,-2.21717808546918,-2.21035518688709,
-2.17887351667309,-2.16649564916164,-2.163613189024,-2.16191934049744,-2.16042070496863,
-2.15853814660727,-2.15558456668745,-2.13680309970434,-2.1141775387529,
-2.10847936773302,-2.10483354671467,-2.1035283383505,-2.1026514869268,-2.10186792572786,
-2.1008000089707,-2.09814943393302,-2.0730549085317,-2.05289726207563,-2.04756503052882,
-2.0454086436735,-2.04386887570229,-2.0424735113764,-2.04026180869694,-2.03614825122908,
-2.01376601227614,-2.00366217768058,-1.98994878542966,-1.98713101531951,
-1.98595149737698,-1.98509858985585,-1.98417003067989,-1.98262854204101,
-1.97746256902453,-1.9543775990238,-1.93298772212286,-1.92934500580595,
-1.92749086290136,-1.92599465069147,-1.92428157668236,-1.92138652203456,
-1.90998773984318,-1.90752595100115),.UNSPECIFIED.);
#1499=B_SPLINE_CURVE_WITH_KNOTS('',3,(#96011,#96012,#96013,#96014,#96015,
#96016,#96017,#96018,#96019,#96020,#96021,#96022,#96023,#96024,#96025,#96026,
#96027,#96028,#96029,#96030,#96031,#96032,#96033,#96034,#96035,#96036,#96037,
#96038,#96039,#96040,#96041,#96042,#96043,#96044,#96045,#96046,#96047,#96048,
#96049,#96050,#96051,#96052,#96053,#96054,#96055,#96056,#96057,#96058,#96059,
#96060,#96061,#96062,#96063,#96064,#96065,#96066,#96067,#96068,#96069,#96070,
#96071,#96072,#96073,#96074,#96075,#96076,#96077,#96078,#96079,#96080,#96081,
#96082,#96083,#96084,#96085,#96086,#96087,#96088,#96089,#96090,#96091,#96092,
#96093,#96094,#96095,#96096,#96097,#96098,#96099,#96100,#96101,#96102,#96103,
#96104,#96105,#96106,#96107,#96108,#96109,#96110,#96111,#96112,#96113,#96114,
#96115,#96116,#96117,#96118,#96119,#96120,#96121,#96122,#96123,#96124,#96125,
#96126,#96127,#96128,#96129,#96130,#96131,#96132,#96133,#96134,#96135,#96136,
#96137,#96138,#96139,#96140,#96141,#96142,#96143,#96144,#96145,#96146,#96147,
#96148,#96149,#96150,#96151,#96152,#96153,#96154,#96155,#96156,#96157,#96158,
#96159,#96160,#96161,#96162,#96163,#96164,#96165,#96166,#96167,#96168,#96169,
#96170,#96171,#96172,#96173,#96174,#96175,#96176,#96177,#96178,#96179,#96180,
#96181,#96182,#96183,#96184,#96185,#96186,#96187,#96188,#96189,#96190,#96191,
#96192,#96193,#96194,#96195,#96196,#96197,#96198,#96199,#96200,#96201,#96202,
#96203,#96204,#96205,#96206,#96207,#96208,#96209,#96210,#96211,#96212,#96213,
#96214,#96215,#96216,#96217,#96218),.UNSPECIFIED.,.F.,.F.,(4,2,2,2,2,2,
2,2,2,2,2,2,2,2,2,2,2,2,2,2,2,2,2,2,2,2,2,2,2,2,2,2,2,2,2,2,2,2,2,2,2,2,
2,2,2,2,2,2,2,2,2,2,2,2,2,2,2,2,2,2,2,2,2,2,2,2,2,2,2,2,2,2,2,2,2,2,2,2,
2,2,2,2,2,2,2,2,2,2,2,2,2,2,2,2,2,2,2,2,2,2,2,2,2,4),(-1.68837727951077,
-1.68781998827758,-1.68610979525433,-1.67886635089715,-1.64780264548136,
-1.63547486615305,-1.63259618872471,-1.63090345529188,-1.62940513817301,
-1.62752209583028,-1.62456603543931,-1.60208463247758,-1.58604837104348,
-1.58328776244323,-1.57479403079398,-1.57300287084039,-1.57200878358889,
-1.57117010413174,-1.57010575287063,-1.56792058347704,-1.54999750431417,
-1.5201389670866,-1.51600081545764,-1.5140714746315,-1.51256409693759,-1.51091542116062,
-1.50823770536098,-1.49852389736165,-1.48002805574701,-1.45910579318059,
-1.45621523972934,-1.45510858376549,-1.45431526753437,-1.45344932519703,
-1.45219699867077,-1.44891827769304,-1.44398634083731,-1.42704748350368,
-1.40332169062381,-1.39878941643496,-1.39678907942413,-1.39527075619288,
-1.39365345110996,-1.39111961347584,-1.38288005792432,-1.35294259185594,
-1.34630432348075,-1.33970486856746,-1.3380444022016,-1.3370800401523,-1.33632193093201,
-1.33526121958634,-1.33309467692154,-1.3127563740379,-1.28568157624691,
-1.28128131800398,-1.27930424410242,-1.27778965052923,-1.27616276355083,
-1.27358506945204,-1.26492447566055,-1.23529328123922,-1.22278897324005,
-1.22099485422695,-1.21991420100556,-1.21907253005077,-1.2181026569478,
-1.21637298908872,-1.20790641209283,-1.18553319150925,-1.1664777146516,
-1.16352049009428,-1.16163701279139,-1.16013855537909,-1.15844588210301,
-1.15556785209376,-1.14325333290793,-1.11232117755965,-1.10492188802842,
-1.10320050946234,-1.10222212669995,-1.10138161656133,-1.10029535559583,
-1.09799783477396,-1.09490794205804,-1.0869986496557,-1.06205865171597,
-1.04864715763952,-1.04561679310036,-1.04387296233757,-1.04239341535756,
-1.04058530574585,-1.03716735423768,-1.0121242096119,-0.989206628751375,
-0.986409617298101,-0.98531692822558,-0.984527124500201,-0.983657402301642,
-0.982386808912438,-0.978985619553725,-0.973803504429689,-0.955204122596725,
-0.946563016930913),.UNSPECIFIED.);
#1500=B_SPLINE_CURVE_WITH_KNOTS('',3,(#96224,#96225,#96226,#96227,#96228,
#96229,#96230,#96231,#96232,#96233,#96234,#96235,#96236,#96237,#96238,#96239,
#96240,#96241,#96242,#96243,#96244,#96245,#96246,#96247,#96248,#96249,#96250,
#96251,#96252,#96253,#96254,#96255,#96256,#96257,#96258,#96259,#96260,#96261,
#96262,#96263,#96264,#96265,#96266,#96267,#96268,#96269,#96270,#96271,#96272,
#96273,#96274,#96275,#96276,#96277,#96278,#96279,#96280,#96281,#96282,#96283,
#96284,#96285,#96286,#96287,#96288,#96289,#96290,#96291,#96292,#96293,#96294,
#96295,#96296,#96297,#96298,#96299,#96300,#96301,#96302,#96303,#96304,#96305,
#96306,#96307,#96308,#96309,#96310,#96311,#96312,#96313,#96314,#96315,#96316,
#96317,#96318,#96319,#96320,#96321,#96322,#96323,#96324,#96325,#96326,#96327,
#96328,#96329,#96330,#96331,#96332,#96333,#96334,#96335,#96336,#96337,#96338,
#96339,#96340,#96341,#96342,#96343,#96344,#96345,#96346,#96347,#96348,#96349,
#96350,#96351,#96352,#96353,#96354,#96355,#96356,#96357,#96358,#96359,#96360,
#96361,#96362,#96363,#96364,#96365,#96366,#96367,#96368,#96369,#96370,#96371,
#96372,#96373,#96374,#96375,#96376,#96377,#96378,#96379,#96380,#96381,#96382,
#96383,#96384,#96385,#96386,#96387,#96388,#96389),.UNSPECIFIED.,.F.,.F.,
(4,2,2,2,2,2,2,2,2,2,2,2,2,2,2,2,2,2,2,2,2,2,2,2,2,2,2,2,2,2,2,2,2,2,2,
2,2,2,2,2,2,2,2,2,2,2,2,2,2,2,2,2,2,2,2,2,2,2,2,2,2,2,2,2,2,2,2,2,2,2,2,
2,2,2,2,2,2,2,2,2,2,2,4),(-0.537654944100775,-0.535789434415299,-0.530947381133612,
-0.514580167551101,-0.490084584660939,-0.485565321528231,-0.483566236081426,
-0.482047101143448,-0.480427231448254,-0.477885793525669,-0.469587853842892,
-0.439665187161532,-0.433016535679776,-0.426451903678453,-0.424793424927305,
-0.423829021551239,-0.423070125063847,-0.422007310375762,-0.419832860044324,
-0.402343849447898,-0.371897899064157,-0.367826861984351,-0.365888215743501,
-0.364382717444537,-0.362719887114946,-0.35998196007451,-0.349584623386473,
-0.32960290970421,-0.310991294368649,-0.308059469310665,-0.306946758269144,
-0.306151391360009,-0.305285841775843,-0.304038405518085,-0.300796693331405,
-0.29594092366606,-0.279489546469263,-0.255103847963886,-0.250581519354464,
-0.248581854820801,-0.247062582934163,-0.245442858781237,-0.242902261654239,
-0.234612787780911,-0.204682516993568,-0.198034421772961,-0.191465316403598,
-0.189806424106082,-0.188841905400883,-0.188082996306437,-0.187020265440863,
-0.184846351190446,-0.167378181365044,-0.136903367542583,-0.132835647464107,
-0.130897590697415,-0.129445614808312,-0.129398584673514,-0.129342416684613,
-0.129302777728965,-0.129274889351391,-0.129240549353893,-0.12756818050583,
-0.124705725681973,-0.12122400083898,-0.114021254191121,-0.0911078939858096,
-0.0745667805052817,-0.0725599365381608,-0.0715177521615853,-0.0706793631632185,
-0.0696648629221745,-0.0677282820327141,-0.0537098029930007,-0.0275392113435695,
-0.0171711065967806,-0.0144304378264026,-0.0127669742247786,-0.0113088240864444,
-0.0098533766463521,-0.00798939879024556,-0.00478412906894591,-9.99999999917733E-7),
 .UNSPECIFIED.);
#1501=B_SPLINE_CURVE_WITH_KNOTS('',3,(#96390,#96391,#96392,#96393,#96394,
#96395,#96396,#96397,#96398,#96399,#96400,#96401,#96402,#96403,#96404,#96405,
#96406,#96407,#96408,#96409,#96410,#96411,#96412,#96413,#96414,#96415,#96416,
#96417,#96418,#96419,#96420,#96421,#96422,#96423,#96424,#96425,#96426,#96427,
#96428,#96429,#96430,#96431,#96432,#96433,#96434,#96435,#96436,#96437,#96438,
#96439,#96440,#96441,#96442,#96443),.UNSPECIFIED.,.F.,.F.,(4,2,2,2,2,2,
2,2,2,2,2,2,2,2,2,2,2,2,2,2,2,2,2,2,2,2,4),(-2.85368559544924,-2.81938608199108,
-2.81030961351792,-2.80854721642627,-2.80757009001122,-2.80672923804291,
-2.80564065848723,-2.80385950953547,-2.79173942507301,-2.7625979824271,
-2.75637958199243,-2.75323833338059,-2.75061443207407,-2.74900757992761,
-2.74758466130194,-2.74570140373577,-2.74274564548966,-2.7239293707165,
-2.70133497900864,-2.69283039418367,-2.69109827123299,-2.69012771407087,
-2.68928588651286,-2.68820557349282,-2.68641312434399,-2.67396368254774,
-2.64925299467486),.UNSPECIFIED.);
#1502=B_SPLINE_CURVE_WITH_KNOTS('',3,(#96444,#96445,#96446,#96447,#96448,
#96449,#96450,#96451,#96452,#96453,#96454,#96455,#96456,#96457,#96458,#96459,
#96460,#96461,#96462,#96463,#96464,#96465,#96466,#96467,#96468,#96469,#96470,
#96471,#96472,#96473,#96474,#96475,#96476,#96477,#96478,#96479,#96480,#96481,
#96482,#96483,#96484,#96485,#96486,#96487,#96488,#96489,#96490,#96491,#96492,
#96493,#96494,#96495,#96496,#96497,#96498,#96499,#96500,#96501,#96502,#96503,
#96504,#96505,#96506,#96507,#96508,#96509,#96510,#96511,#96512,#96513,#96514,
#96515,#96516,#96517,#96518,#96519,#96520,#96521,#96522,#96523,#96524,#96525,
#96526,#96527,#96528,#96529,#96530,#96531,#96532,#96533,#96534,#96535,#96536,
#96537,#96538,#96539,#96540,#96541,#96542,#96543,#96544,#96545,#96546,#96547,
#96548,#96549,#96550,#96551,#96552,#96553,#96554,#96555,#96556,#96557,#96558,
#96559,#96560,#96561,#96562,#96563,#96564,#96565,#96566,#96567,#96568,#96569,
#96570,#96571,#96572,#96573,#96574,#96575,#96576,#96577,#96578,#96579,#96580,
#96581,#96582,#96583,#96584,#96585,#96586,#96587,#96588,#96589,#96590,#96591,
#96592,#96593,#96594,#96595,#96596,#96597,#96598,#96599,#96600,#96601,#96602,
#96603,#96604,#96605,#96606,#96607,#96608,#96609,#96610,#96611,#96612,#96613,
#96614,#96615,#96616,#96617,#96618,#96619,#96620,#96621,#96622,#96623,#96624,
#96625,#96626,#96627,#96628,#96629,#96630,#96631,#96632,#96633,#96634,#96635,
#96636,#96637,#96638,#96639,#96640,#96641,#96642,#96643,#96644,#96645,#96646,
#96647,#96648,#96649,#96650,#96651,#96652,#96653,#96654,#96655,#96656,#96657,
#96658,#96659,#96660,#96661),.UNSPECIFIED.,.F.,.F.,(4,2,2,2,2,2,2,2,2,2,
2,2,2,2,2,2,2,2,2,2,2,2,2,2,2,2,2,2,2,2,2,2,2,2,2,2,2,2,2,2,2,2,2,2,2,2,
2,2,2,2,2,2,2,2,2,2,2,2,2,2,2,2,2,2,2,2,2,2,2,2,2,2,2,2,2,2,2,2,2,2,2,2,
2,2,2,2,2,2,2,2,2,2,2,2,2,2,2,2,2,2,2,2,2,2,2,2,2,2,4),(-0.946563016930913,
-0.933543375261107,-0.929009140367105,-0.927008139137741,-0.925489390025472,
-0.923871706480782,-0.921337433505994,-0.913097924492891,-0.883150834223557,
-0.876511016857133,-0.869908544931653,-0.868247532108279,-0.867282889721922,
-0.86652458230784,-0.865463623065431,-0.863296681852881,-0.843047106167405,
-0.815859994076131,-0.811465573806204,-0.809489222871741,-0.807974422528057,
-0.806346569401789,-0.803765748407679,-0.795078739523885,-0.765456565894513,
-0.752960370416633,-0.751166189901932,-0.750085369736987,-0.749243486889604,
-0.748273273917912,-0.746542772802078,-0.738067268495438,-0.71564853254054,
-0.69663361684836,-0.69367624316458,-0.691792456537885,-0.690293617109017,
-0.688600367667036,-0.685721000716398,-0.673394577760545,-0.642384729066529,
-0.635053489863898,-0.633336554734155,-0.632359027962573,-0.631526147626519,
-0.630442426595042,-0.628159064392551,-0.625093902727327,-0.617280252282636,
-0.592803719098889,-0.578825766515184,-0.57576553179727,-0.574014653615267,
-0.572534992457822,-0.570733936579166,-0.56735132820757,-0.563106045903372,
-0.553505071266121,-0.537759260907421,-0.519534548142031,-0.516597706164644,
-0.515484669052243,-0.514689428041729,-0.513824441598386,-0.512578544540572,
-0.509344914334808,-0.50450484478626,-0.48814701270472,-0.463638893578981,
-0.459120691590664,-0.457122255418734,-0.455603693883614,-0.453984518406383,
-0.451444357169866,-0.443152646648182,-0.413237651196606,-0.406592022840417,
-0.40001261636984,-0.398353305966229,-0.397388938362001,-0.396630401853502,
-0.395568544255559,-0.393397696789795,-0.376015086200967,-0.345430838764617,
-0.341378160289219,-0.339443452728329,-0.337938936622103,-0.336275088590443,
-0.333530621562447,-0.323045066780609,-0.302752436624759,-0.284564297864742,
-0.281625701240686,-0.280512417965607,-0.279717095485449,-0.278852129075036,
-0.277606440116836,-0.274374345786027,-0.269537420335027,-0.253199354551679,
-0.228663201841218,-0.224145795664896,-0.222147460249137,-0.220628877206173,
-0.219009584431811,-0.21646904090926,-0.208174229584812,-0.204517382372539),
 .UNSPECIFIED.);
#1503=B_SPLINE_CURVE_WITH_KNOTS('',3,(#96666,#96667,#96668,#96669,#96670,
#96671,#96672,#96673,#96674,#96675,#96676,#96677,#96678,#96679,#96680,#96681,
#96682,#96683,#96684,#96685,#96686,#96687,#96688,#96689,#96690,#96691,#96692,
#96693,#96694,#96695,#96696,#96697,#96698,#96699,#96700,#96701,#96702,#96703,
#96704,#96705,#96706,#96707,#96708,#96709,#96710,#96711,#96712,#96713,#96714,
#96715,#96716,#96717,#96718,#96719,#96720,#96721,#96722,#96723,#96724,#96725,
#96726,#96727,#96728,#96729,#96730,#96731,#96732,#96733,#96734,#96735,#96736,
#96737,#96738,#96739,#96740,#96741,#96742,#96743,#96744,#96745,#96746,#96747,
#96748,#96749,#96750,#96751,#96752,#96753,#96754,#96755,#96756,#96757,#96758,
#96759,#96760,#96761,#96762,#96763,#96764,#96765,#96766,#96767,#96768,#96769,
#96770,#96771,#96772,#96773,#96774,#96775,#96776,#96777,#96778,#96779,#96780,
#96781,#96782,#96783,#96784,#96785,#96786,#96787,#96788,#96789,#96790,#96791,
#96792,#96793,#96794,#96795,#96796,#96797,#96798,#96799,#96800,#96801,#96802,
#96803,#96804,#96805,#96806,#96807,#96808,#96809,#96810,#96811,#96812,#96813,
#96814,#96815,#96816,#96817,#96818,#96819,#96820,#96821,#96822,#96823,#96824,
#96825,#96826,#96827,#96828,#96829,#96830,#96831,#96832,#96833,#96834,#96835,
#96836,#96837,#96838,#96839,#96840,#96841,#96842,#96843,#96844,#96845,#96846,
#96847,#96848,#96849,#96850,#96851,#96852,#96853,#96854,#96855,#96856,#96857,
#96858,#96859,#96860,#96861,#96862,#96863,#96864,#96865,#96866,#96867,#96868,
#96869,#96870,#96871,#96872,#96873,#96874,#96875,#96876,#96877,#96878,#96879,
#96880,#96881,#96882,#96883,#96884,#96885),.UNSPECIFIED.,.F.,.F.,(4,2,2,
2,2,2,2,2,2,2,2,2,2,2,2,2,2,2,2,2,2,2,2,2,2,2,2,2,2,2,2,2,2,2,2,2,2,2,2,
2,2,2,2,2,2,2,2,2,2,2,2,2,2,2,2,2,2,2,2,2,2,2,2,2,2,2,2,2,2,2,2,2,2,2,2,
2,2,2,2,2,2,2,2,2,2,2,2,2,2,2,2,2,2,2,2,2,2,2,2,2,2,2,2,2,2,2,2,2,2,4),
(-1.27975427727725,-1.25199137047719,-1.2493861684092,-1.24795605413082,
-1.24670473500885,-1.24583850733499,-1.24504412631629,-1.24393492438005,
-1.24102936833812,-1.22046684545241,-1.20604336971845,-1.19705571217952,
-1.19107438868889,-1.18890711482678,-1.18750659945926,-1.18598938184144,
-1.1840015550619,-1.1795458133282,-1.15278914018882,-1.13808430320792,-1.13352500983649,
-1.13048617808367,-1.1292388225823,-1.12837334061542,-1.1275780416231,-1.12646544340642,
-1.12353385323737,-1.10513420448383,-1.08501620582852,-1.07457982324743,
-1.0718388463062,-1.07017541104046,-1.06867016562359,-1.06673296820058,
-1.06266921959483,-1.03214972768199,-1.01469977961972,-1.01252640859014,
-1.0114638338231,-1.01070499668163,-1.00974050140096,-1.00808152619519,
-1.00151007460853,-0.994872770029299,-0.964961008133719,-0.956673173050825,
-0.95413287521227,-0.952513280162439,-0.950994084821972,-0.948994454910477,
-0.944471949744033,-0.920058519159929,-0.903610202969209,-0.898754773236036,
-0.895513561965845,-0.894266237093875,-0.893400744325761,-0.892605409700215,
-0.891492727669283,-0.888560634559187,-0.869868832058371,-0.849969375697545,
-0.839595815676233,-0.836859956359817,-0.835197614040961,-0.833692061380742,
-0.831752648806168,-0.827677395399033,-0.797246780094766,-0.779727540466477,
-0.777552150100562,-0.776489160180354,-0.77573025909539,-0.774766001104869,
-0.773108124239889,-0.766550115246269,-0.759910112492467,-0.730018557154092,
-0.721702483369917,-0.719159148492118,-0.717538865773099,-0.716019899224641,
-0.714021844164187,-0.709508502666446,-0.684765956089572,-0.676101493216078,
-0.661861018297902,-0.659919396433078,-0.658903881336649,-0.658065571402876,
-0.65702462922252,-0.655023386087201,-0.639862526826004,-0.633171124375001,
-0.607483957067017,-0.603451721784349,-0.601261030727202,-0.599729540785908,
-0.598160074139939,-0.595856103905065,-0.589525912707429,-0.579879704757375,
-0.564181223881447,-0.545983606284509,-0.543045109004461,-0.541931575654508,
-0.541136007376822,-0.540270683575712,-0.539024306948506,-0.537654944100775),
 .UNSPECIFIED.);
#1504=B_SPLINE_CURVE_WITH_KNOTS('',3,(#96887,#96888,#96889,#96890,#96891,
#96892,#96893,#96894,#96895,#96896,#96897,#96898,#96899,#96900,#96901,#96902,
#96903,#96904,#96905,#96906,#96907,#96908,#96909,#96910,#96911,#96912,#96913,
#96914,#96915,#96916,#96917,#96918,#96919,#96920,#96921,#96922,#96923,#96924,
#96925,#96926,#96927,#96928,#96929,#96930,#96931,#96932,#96933,#96934,#96935,
#96936,#96937,#96938,#96939,#96940,#96941,#96942),.UNSPECIFIED.,.F.,.F.,
(4,2,2,2,2,2,2,2,2,2,2,2,2,2,2,2,2,2,2,2,2,2,2,2,2,2,2,4),(-0.204517382372539,
-0.178260528710531,-0.171614465939901,-0.165036253785904,-0.163377013093062,
-0.162412645657632,-0.161654084114003,-0.160592158797679,-0.158421055664157,
-0.141031124508097,-0.110454985546614,-0.106401055436445,-0.104466078025292,
-0.102961494387479,-0.101362134321586,-0.0987650910074259,-0.0956616331105435,
-0.0895499348259312,-0.0726251376513031,-0.0493628884496759,-0.0465823321335659,
-0.0454922521321131,-0.0447029763573064,-0.0438322353545825,-0.0425574477223321,
-0.0391288503697206,-0.018101941217382,-9.99999999334866E-7),
 .UNSPECIFIED.);
#1505=B_SPLINE_CURVE_WITH_KNOTS('',3,(#96943,#96944,#96945,#96946,#96947,
#96948,#96949,#96950,#96951,#96952,#96953,#96954,#96955,#96956,#96957,#96958,
#96959,#96960,#96961,#96962,#96963,#96964,#96965,#96966,#96967,#96968,#96969,
#96970,#96971,#96972,#96973,#96974,#96975,#96976,#96977,#96978,#96979,#96980,
#96981,#96982,#96983,#96984,#96985,#96986,#96987,#96988,#96989,#96990,#96991,
#96992,#96993,#96994,#96995,#96996,#96997,#96998,#96999,#97000,#97001,#97002,
#97003,#97004,#97005,#97006,#97007,#97008,#97009,#97010,#97011,#97012,#97013,
#97014,#97015,#97016,#97017,#97018,#97019,#97020,#97021,#97022,#97023,#97024,
#97025,#97026,#97027,#97028,#97029,#97030,#97031,#97032,#97033,#97034,#97035,
#97036,#97037,#97038,#97039,#97040,#97041,#97042,#97043,#97044,#97045,#97046,
#97047,#97048,#97049,#97050,#97051,#97052,#97053,#97054,#97055,#97056,#97057,
#97058,#97059,#97060,#97061,#97062,#97063,#97064,#97065,#97066,#97067,#97068,
#97069,#97070,#97071,#97072,#97073,#97074,#97075,#97076,#97077,#97078,#97079,
#97080,#97081,#97082,#97083,#97084,#97085,#97086,#97087,#97088,#97089,#97090,
#97091,#97092,#97093,#97094,#97095,#97096,#97097,#97098,#97099,#97100,#97101,
#97102),.UNSPECIFIED.,.F.,.F.,(4,2,2,2,2,2,2,2,2,2,2,2,2,2,2,2,2,2,2,2,
2,2,2,2,2,2,2,2,2,2,2,2,2,2,2,2,2,2,2,2,2,2,2,2,2,2,2,2,2,2,2,2,2,2,2,2,
2,2,2,2,2,2,2,2,2,2,2,2,2,2,2,2,2,2,2,2,2,2,2,4),(-3.48624385780003,-3.47968930691364,
-3.47573880689191,-3.4740821909817,-3.47267806908479,-3.47117870449806,
-3.46928641528836,-3.46557720932842,-3.45535784924294,-3.4246234335228,
-3.41638808331368,-3.41467132645148,-3.41370418633071,-3.41286191236619,
-3.41177672076385,-3.40996730853489,-3.39662162732591,-3.37656970251867,
-3.36570710000715,-3.36109315356723,-3.35854379436467,-3.35631853704546,
-3.35478161598719,-3.35325072097044,-3.35105967957976,-3.34702365578681,
-3.32127602239909,-3.29969866281412,-3.29752868554427,-3.29646714030711,
-3.29570878577414,-3.29474457929997,-3.29308541795997,-3.28650451149845,
-3.27987065043401,-3.24997831033339,-3.24168967859122,-3.23915020974154,
-3.23753140328845,-3.23601313587224,-3.23401500982554,-3.22949720661632,
-3.20496895368156,-3.18861347599592,-3.18377395732304,-3.18054105197065,
-3.17929540993799,-3.17843059850735,-3.17763551326552,-3.176522697548,-3.17358625468488,
-3.15540160246922,-3.13971816419939,-3.13007749621605,-3.12375007188259,
-3.12144729179094,-3.119878693829,-3.11834810009179,-3.11615878867429,-3.11212932872914,
-3.08637810083257,-3.0647923385948,-3.06262229172352,-3.06156071783781,
-3.06080234503758,-3.05983811835208,-3.05817892877509,-3.05159799690581,
-3.04496395578766,-3.01507111257892,-3.00678201838198,-3.00424246137772,
-3.00262361065234,-3.00110531006374,-2.99910715253951,-2.99458933177557,
-2.9700572810668,-2.95370384307095,-2.94886460473741,-2.94874919963959),
 .UNSPECIFIED.);
#1506=B_SPLINE_CURVE_WITH_KNOTS('',3,(#97107,#97108,#97109,#97110,#97111,
#97112,#97113,#97114,#97115,#97116,#97117,#97118,#97119,#97120,#97121,#97122,
#97123,#97124,#97125,#97126,#97127,#97128,#97129,#97130,#97131,#97132,#97133,
#97134,#97135,#97136,#97137,#97138,#97139,#97140,#97141,#97142,#97143,#97144,
#97145,#97146,#97147,#97148,#97149,#97150,#97151,#97152,#97153,#97154,#97155,
#97156,#97157,#97158,#97159,#97160,#97161,#97162,#97163,#97164,#97165,#97166,
#97167,#97168,#97169,#97170,#97171,#97172,#97173,#97174,#97175,#97176,#97177,
#97178,#97179,#97180,#97181,#97182,#97183,#97184,#97185,#97186,#97187,#97188,
#97189,#97190,#97191,#97192,#97193,#97194,#97195,#97196,#97197,#97198,#97199,
#97200,#97201,#97202,#97203,#97204,#97205,#97206,#97207,#97208,#97209,#97210,
#97211,#97212,#97213,#97214,#97215,#97216,#97217,#97218,#97219,#97220,#97221,
#97222,#97223,#97224,#97225,#97226,#97227,#97228,#97229,#97230,#97231,#97232,
#97233,#97234,#97235,#97236,#97237,#97238,#97239,#97240,#97241,#97242,#97243,
#97244,#97245,#97246,#97247,#97248,#97249,#97250,#97251,#97252,#97253,#97254,
#97255,#97256,#97257,#97258,#97259,#97260,#97261,#97262,#97263,#97264,#97265,
#97266,#97267,#97268,#97269,#97270,#97271,#97272,#97273,#97274,#97275,#97276,
#97277,#97278,#97279,#97280,#97281,#97282,#97283,#97284,#97285,#97286,#97287,
#97288,#97289,#97290,#97291,#97292,#97293,#97294,#97295,#97296,#97297,#97298,
#97299,#97300,#97301,#97302,#97303,#97304,#97305,#97306,#97307,#97308,#97309,
#97310,#97311,#97312,#97313,#97314,#97315,#97316,#97317,#97318,#97319,#97320,
#97321,#97322,#97323,#97324,#97325,#97326),.UNSPECIFIED.,.F.,.F.,(4,2,2,
2,2,2,2,2,2,2,2,2,2,2,2,2,2,2,2,2,2,2,2,2,2,2,2,2,2,2,2,2,2,2,2,2,2,2,2,
2,2,2,2,2,2,2,2,2,2,2,2,2,2,2,2,2,2,2,2,2,2,2,2,2,2,2,2,2,2,2,2,2,2,2,2,
2,2,2,2,2,2,2,2,2,2,2,2,2,2,2,2,2,2,2,2,2,2,2,2,2,2,2,2,2,2,2,2,2,2,4),
(-0.742062510194801,-0.736873225342865,-0.732806069602463,-0.730868275943952,
-0.729363008565338,-0.727699996180712,-0.72496075667552,-0.714545192383826,
-0.694498614772829,-0.675978223068981,-0.67304653797817,-0.671933918317771,
-0.671138625410848,-0.6702731663647,-0.669025877113159,-0.665784639025209,
-0.660929657847286,-0.644481805877878,-0.620096036935879,-0.615574221659552,
-0.613574767187254,-0.612055648296152,-0.610436080905066,-0.607895716329152,
-0.599606876740267,-0.569679726799791,-0.563032275923686,-0.556463916494297,
-0.554805196987647,-0.553840776026411,-0.553081942139507,-0.552019314382996,
-0.549845603126137,-0.532378705361215,-0.501907393605616,-0.497840090088558,
-0.495902228388823,-0.494396909181205,-0.492733840575492,-0.489994510873881,
-0.479578635159875,-0.459531529393454,-0.441010289384183,-0.438078503971869,
-0.436965846175701,-0.436170525995552,-0.435305037253762,-0.434057705178371,
-0.430816355657519,-0.425961207439399,-0.409512788179206,-0.385126186769233,
-0.380604216274537,-0.378604693195326,-0.37708552218971,-0.37546589924846,
-0.372925447561444,-0.364636323943848,-0.334708147158132,-0.32806046827743,
-0.321491883378753,-0.319833106959273,-0.318868652911839,-0.318109792994398,
-0.317047128789903,-0.314873342988328,-0.297405846798249,-0.266933488780481,
-0.262866045864875,-0.260928117713057,-0.25942274687041,-0.257759621202867,
-0.255020197475023,-0.244603963763567,-0.224556167892638,-0.206034295759932,
-0.203102409772794,-0.201989713807829,-0.201194366344894,-0.200328847913545,
-0.199081473050705,-0.195840012343133,-0.190984697582693,-0.174535714125226,
-0.150164769065553,-0.145631444051202,-0.143629891320126,-0.142110342886935,
-0.140709614980209,-0.138492924912212,-0.132397383291039,-0.123186729675139,
-0.100865008703675,-0.0870939715360433,-0.0852858201090558,-0.0842006554811097,
-0.0833579376182,-0.0823897113833211,-0.0806696712496977,-0.072470763153566,
-0.0593359563225871,-0.045059337371504,-0.030476726664995,-0.027659988660972,
-0.0258184925403211,-0.0243222753918401,-0.0229115649271589,-0.0212193354767052,
-0.0187333837042564,-1.00000008385059E-6),.UNSPECIFIED.);
#1507=B_SPLINE_CURVE_WITH_KNOTS('',3,(#97327,#97328,#97329,#97330,#97331,
#97332,#97333,#97334,#97335,#97336,#97337,#97338,#97339,#97340,#97341,#97342,
#97343,#97344,#97345,#97346,#97347,#97348,#97349,#97350,#97351,#97352,#97353,
#97354,#97355,#97356,#97357,#97358,#97359,#97360,#97361,#97362,#97363,#97364,
#97365,#97366,#97367,#97368,#97369,#97370,#97371,#97372,#97373,#97374,#97375,
#97376,#97377,#97378,#97379,#97380,#97381,#97382,#97383,#97384,#97385,#97386,
#97387,#97388,#97389,#97390,#97391,#97392,#97393,#97394,#97395,#97396,#97397,
#97398,#97399,#97400,#97401,#97402,#97403,#97404,#97405,#97406,#97407,#97408,
#97409,#97410,#97411,#97412,#97413,#97414,#97415,#97416,#97417,#97418,#97419,
#97420,#97421,#97422,#97423,#97424,#97425,#97426,#97427,#97428,#97429,#97430,
#97431,#97432,#97433,#97434,#97435,#97436,#97437,#97438,#97439,#97440,#97441,
#97442,#97443,#97444,#97445,#97446,#97447,#97448,#97449,#97450,#97451,#97452,
#97453,#97454,#97455,#97456,#97457,#97458,#97459,#97460,#97461,#97462,#97463,
#97464,#97465,#97466,#97467,#97468,#97469,#97470,#97471,#97472,#97473,#97474,
#97475,#97476,#97477,#97478,#97479,#97480,#97481,#97482,#97483,#97484,#97485,
#97486,#97487,#97488,#97489,#97490,#97491,#97492,#97493,#97494,#97495,#97496,
#97497,#97498,#97499,#97500,#97501,#97502,#97503,#97504,#97505,#97506,#97507,
#97508,#97509,#97510,#97511,#97512,#97513,#97514,#97515,#97516,#97517,#97518,
#97519,#97520,#97521,#97522,#97523,#97524,#97525,#97526,#97527,#97528,#97529,
#97530,#97531,#97532,#97533,#97534,#97535,#97536,#97537,#97538,#97539,#97540,
#97541,#97542,#97543,#97544),.UNSPECIFIED.,.F.,.F.,(4,2,2,2,2,2,2,2,2,2,
2,2,2,2,2,2,2,2,2,2,2,2,2,2,2,2,2,2,2,2,2,2,2,2,2,2,2,2,2,2,2,2,2,2,2,2,
2,2,2,2,2,2,2,2,2,2,2,2,2,2,2,2,2,2,2,2,2,2,2,2,2,2,2,2,2,2,2,2,2,2,2,2,
2,2,2,2,2,2,2,2,2,2,2,2,2,2,2,2,2,2,2,2,2,2,2,2,2,2,4),(-2.94874919963959,
-2.94563181336272,-2.94438616932686,-2.94352134164249,-2.9427262295307,
-2.94161336042909,-2.93867664477627,-2.92049594125669,-2.90481990378337,
-2.8951716182036,-2.88884054412347,-2.88653722719753,-2.88496849127357,
-2.8834379379217,-2.88124899019365,-2.8772209945663,-2.85142959079008,-2.82988005621161,
-2.82771003991804,-2.82664845594012,-2.82589006572939,-2.82492580292341,
-2.82326652084327,-2.81668482031881,-2.81005072088468,-2.78015618473745,
-2.77186811969537,-2.76932862961244,-2.76770976621996,-2.76619141500019,
-2.76419313432092,-2.75967478626329,-2.7351571068768,-2.71879195802694,
-2.71395076033784,-2.71071698023472,-2.70947116876784,-2.70860629404098,
-2.70781119420487,-2.70669841572578,-2.70376255310536,-2.68556030021428,
-2.66984655242859,-2.66023340089687,-2.65391892335074,-2.65161784995547,
-2.65004954813491,-2.64851857685317,-2.64632755916661,-2.64229192481368,
-2.61669401127094,-2.60337869593432,-2.59429832090056,-2.59253570780119,
-2.59155854160376,-2.59071771446621,-2.58962926936559,-2.58784855611947,
-2.57574356815116,-2.54663867354052,-2.53719187527053,-2.53453776874591,
-2.53289389135039,-2.53138442810734,-2.5294434367491,-2.52524438228764,
-2.49587639680752,-2.4775309312382,-2.47533358817698,-2.47426661449917,
-2.47342748751495,-2.47243476984707,-2.47065065363171,-2.46228457510869,
-2.43230743330612,-2.42011777321775,-2.41724763451464,-2.41555643801239,
-2.41405735272636,-2.41217049850482,-2.40920283352659,-2.3891901890282,
-2.38724898164711,-2.36747259894213,-2.35926444946408,-2.35754914363084,
-2.35658225927113,-2.35573983681129,-2.35465398220687,-2.35284248740325,
-2.33878654230967,-2.31807641461105,-2.30807480991439,-2.30371001763489,
-2.30025208759365,-2.29843551985566,-2.29708617175595,-2.29539590635686,
-2.29253021073826,-2.28195198318271,-2.2580260494147,-2.24363463152286,
-2.24075042566623,-2.23955979022528,-2.23870495394633,-2.2377807981689,
-2.23625942108317,-2.23127379633466,-2.20677820015193),.UNSPECIFIED.);
#1508=B_SPLINE_CURVE_WITH_KNOTS('',3,(#97549,#97550,#97551,#97552,#97553,
#97554,#97555,#97556,#97557,#97558,#97559,#97560,#97561,#97562,#97563,#97564,
#97565,#97566,#97567,#97568,#97569,#97570,#97571,#97572,#97573,#97574,#97575,
#97576,#97577,#97578,#97579,#97580,#97581,#97582,#97583,#97584,#97585,#97586,
#97587,#97588,#97589,#97590,#97591,#97592,#97593,#97594,#97595,#97596,#97597,
#97598,#97599,#97600,#97601,#97602,#97603,#97604,#97605,#97606,#97607,#97608,
#97609,#97610,#97611,#97612,#97613,#97614,#97615,#97616,#97617,#97618,#97619,
#97620,#97621,#97622,#97623,#97624,#97625,#97626,#97627,#97628,#97629,#97630,
#97631,#97632,#97633,#97634,#97635,#97636,#97637,#97638,#97639,#97640,#97641,
#97642,#97643,#97644,#97645,#97646,#97647,#97648,#97649,#97650,#97651,#97652,
#97653,#97654,#97655,#97656,#97657,#97658,#97659,#97660,#97661,#97662,#97663,
#97664,#97665,#97666,#97667,#97668,#97669,#97670,#97671,#97672,#97673,#97674,
#97675,#97676,#97677,#97678,#97679,#97680,#97681,#97682,#97683,#97684,#97685,
#97686,#97687,#97688,#97689,#97690,#97691,#97692,#97693,#97694,#97695,#97696,
#97697,#97698,#97699,#97700,#97701,#97702,#97703,#97704,#97705,#97706,#97707,
#97708,#97709,#97710,#97711,#97712,#97713,#97714,#97715,#97716,#97717,#97718,
#97719,#97720,#97721,#97722,#97723,#97724,#97725,#97726,#97727,#97728,#97729,
#97730,#97731,#97732,#97733,#97734,#97735,#97736,#97737,#97738,#97739,#97740,
#97741,#97742,#97743,#97744,#97745,#97746,#97747,#97748,#97749,#97750,#97751,
#97752,#97753,#97754,#97755,#97756),.UNSPECIFIED.,.F.,.F.,(4,2,2,2,2,2,
2,2,2,2,2,2,2,2,2,2,2,2,2,2,2,2,2,2,2,2,2,2,2,2,2,2,2,2,2,2,2,2,2,2,2,2,
2,2,2,2,2,2,2,2,2,2,2,2,2,2,2,2,2,2,2,2,2,2,2,2,2,2,2,2,2,2,2,2,2,2,2,2,
2,2,2,2,2,2,2,2,2,2,2,2,2,2,2,2,2,2,2,2,2,2,2,2,2,4),(-1.48411343733603,
-1.48391937310299,-1.46979791345893,-1.44217094315329,-1.43824144942646,
-1.43629458071536,-1.43487784313069,-1.43335459476186,-1.43129367620594,
-1.42654436271121,-1.41998565202743,-1.40083602324541,-1.38081805978295,
-1.37789894277997,-1.37678800916947,-1.37599321408102,-1.37512748052567,
-1.37387844619672,-1.37062513018299,-1.36574562215395,-1.34914406759509,
-1.32496541931158,-1.32043920508221,-1.31843910199311,-1.31691999566555,
-1.31530092751719,-1.31276236584729,-1.30448891516698,-1.27455384889865,
-1.26790837164263,-1.26133363315694,-1.25967449115301,-1.25871003186337,
-1.25795129722163,-1.25688897645381,-1.25471649648369,-1.23728677584488,
-1.20677233317044,-1.2027113325222,-1.20077478610655,-1.19926975686926,
-1.19760626616624,-1.19486451918617,-1.18441684133425,-1.16425711219195,
-1.14589196910587,-1.14295934986015,-1.14184666105141,-1.14105138342591,
-1.14018601556656,-1.13893898082861,-1.13569908990507,-1.13084670990019,
-1.11441402372758,-1.09001130270313,-1.08549026710628,-1.08349103051009,
-1.08197202765248,-1.08035253635164,-1.0778121911182,-1.06952248093534,
-1.03959841782298,-1.03295128618048,-1.0263840613134,-1.02472551151036,
-1.02376116882008,-1.02300238378214,-1.02193980789052,-1.01976614330796,
-1.00229692844627,-0.97183222092432,-0.96776461244867,-0.965826771272516,
-0.96432153981366,-0.96265864095223,-0.959919759536341,-0.94950779657122,
-0.929473205906618,-0.910938302271087,-0.908006730024431,-0.906894149096673,
-0.906098882946798,-0.905233451947954,-0.903986201350591,-0.900745053860764,
-0.895890200008261,-0.879442688064493,-0.855057989796824,-0.850536316746511,
-0.848536926975115,-0.847017857948266,-0.845398344398416,-0.842858065702801,
-0.834569519654809,-0.804643340629272,-0.797996110643673,-0.791427957786785,
-0.789769292113311,-0.788804902743149,-0.788046093894874,-0.786983501437117,
-0.784809863235326,-0.767343590916143,-0.742062510194801),.UNSPECIFIED.);
#1509=B_SPLINE_CURVE_WITH_KNOTS('',3,(#97757,#97758,#97759,#97760,#97761,
#97762,#97763,#97764,#97765,#97766,#97767,#97768,#97769,#97770,#97771,#97772,
#97773,#97774,#97775,#97776,#97777,#97778,#97779,#97780,#97781,#97782,#97783,
#97784,#97785,#97786,#97787,#97788,#97789,#97790,#97791,#97792,#97793,#97794,
#97795,#97796,#97797,#97798,#97799,#97800,#97801,#97802,#97803,#97804,#97805,
#97806,#97807,#97808,#97809,#97810,#97811,#97812,#97813,#97814,#97815,#97816,
#97817,#97818,#97819,#97820,#97821,#97822,#97823,#97824,#97825,#97826,#97827,
#97828,#97829,#97830,#97831,#97832,#97833,#97834,#97835,#97836,#97837,#97838,
#97839,#97840,#97841,#97842,#97843,#97844,#97845,#97846,#97847,#97848,#97849,
#97850,#97851,#97852,#97853,#97854,#97855,#97856,#97857,#97858,#97859,#97860,
#97861,#97862,#97863,#97864,#97865,#97866,#97867,#97868,#97869,#97870,#97871,
#97872,#97873,#97874,#97875,#97876,#97877,#97878,#97879,#97880,#97881,#97882,
#97883,#97884,#97885,#97886,#97887,#97888,#97889,#97890,#97891,#97892,#97893,
#97894,#97895,#97896,#97897,#97898,#97899,#97900,#97901,#97902,#97903,#97904,
#97905,#97906,#97907,#97908,#97909,#97910,#97911,#97912,#97913,#97914,#97915,
#97916,#97917,#97918,#97919,#97920,#97921,#97922,#97923,#97924,#97925,#97926,
#97927,#97928,#97929,#97930,#97931,#97932,#97933,#97934,#97935,#97936,#97937,
#97938,#97939,#97940,#97941,#97942,#97943,#97944,#97945,#97946,#97947,#97948,
#97949,#97950,#97951,#97952,#97953,#97954,#97955,#97956,#97957,#97958,#97959,
#97960,#97961,#97962,#97963,#97964,#97965,#97966,#97967,#97968),
 .UNSPECIFIED.,.F.,.F.,(4,2,2,2,2,2,2,2,2,2,2,2,2,2,2,2,2,2,2,2,2,2,2,2,
2,2,2,2,2,2,2,2,2,2,2,2,2,2,2,2,2,2,2,2,2,2,2,2,2,2,2,2,2,2,2,2,2,2,2,2,
2,2,2,2,2,2,2,2,2,2,2,2,2,2,2,2,2,2,2,2,2,2,2,2,2,2,2,2,2,2,2,2,2,2,2,2,
2,2,2,2,2,2,2,2,2,4),(-2.20677820015193,-2.19782960546998,-2.18524257551801,
-2.18234651604768,-2.18064970785602,-2.17915151037252,-2.1772735701919,
-2.17433523092769,-2.15626959839353,-2.13299626968107,-2.12437999180744,
-2.12264176548573,-2.12166990949715,-2.12082834350583,-2.11975014283919,
-2.11796483893494,-2.10571925429444,-2.07644693946391,-2.06726843738073,
-2.06463952170548,-2.06300120198874,-2.06149009575149,-2.05953753985984,
-2.05527495910282,-2.02651360467143,-2.0076813778414,-2.00547137576711,
-2.00440195344056,-2.00356269726017,-2.00257193829803,-2.0007963755545,
-1.99256516272289,-1.96245945135483,-1.95025275853269,-1.94738158187449,
-1.94569021112711,-1.94419123868638,-1.94230488414745,-1.93933871169091,
-1.91671034502803,-1.9003870691124,-1.8896125997876,-1.88777499095322,-1.88678176369205,
-1.88594276825481,-1.88487668670315,-1.88317070003192,-1.87323412624796,
-1.84907194678992,-1.83852824763725,-1.83400544482355,-1.83044903042786,
-1.82861233948987,-1.82711724836727,-1.82539107742984,-1.82243883097819,
-1.81019451494527,-1.78444278643403,-1.77328369346748,-1.7707372182407,
-1.76960473894355,-1.76875888820371,-1.7678081649945,-1.76616655703857,
-1.7600062831576,-1.73329216150789,-1.71601076727462,-1.71309609345232,
-1.71122532129363,-1.70972775310294,-1.70802618401248,-1.70510829538191,
-1.69217465206501,-1.67521802115282,-1.65647819344893,-1.65354327201266,
-1.6524306079394,-1.65163555335253,-1.65077067747817,-1.64952478748937,
-1.64629032950031,-1.64144830223028,-1.62507606895734,-1.60059514261638,
-1.59607710796654,-1.59407891202565,-1.59256059790068,-1.59094174862975,
-1.58840223023976,-1.58011384269552,-1.55020267036847,-1.54355837122753,
-1.53697920676373,-1.53532011047188,-1.5343558939778,-1.5335974929654,-1.53253584664277,
-1.53036550857978,-1.51299046027206,-1.48240563647643,-1.47835443034983,
-1.47642020637837,-1.47491597105228,-1.47325233670926,-1.47050799711252,
-1.46482421780974),.UNSPECIFIED.);
#1510=B_SPLINE_CURVE_WITH_KNOTS('',3,(#97973,#97974,#97975,#97976,#97977,
#97978,#97979,#97980,#97981,#97982,#97983,#97984,#97985,#97986,#97987,#97988,
#97989,#97990,#97991,#97992,#97993,#97994,#97995,#97996,#97997,#97998,#97999,
#98000,#98001,#98002,#98003,#98004,#98005,#98006,#98007,#98008,#98009,#98010,
#98011,#98012,#98013,#98014,#98015,#98016,#98017,#98018,#98019,#98020,#98021,
#98022,#98023,#98024,#98025,#98026,#98027,#98028,#98029,#98030,#98031,#98032,
#98033,#98034,#98035,#98036,#98037,#98038,#98039,#98040,#98041,#98042,#98043,
#98044,#98045,#98046,#98047,#98048,#98049,#98050,#98051,#98052,#98053,#98054,
#98055,#98056,#98057,#98058,#98059,#98060,#98061,#98062,#98063,#98064,#98065,
#98066,#98067,#98068,#98069,#98070,#98071,#98072,#98073,#98074,#98075,#98076,
#98077,#98078,#98079,#98080,#98081,#98082,#98083,#98084,#98085,#98086,#98087,
#98088,#98089,#98090,#98091,#98092,#98093,#98094,#98095,#98096,#98097,#98098,
#98099,#98100,#98101,#98102,#98103,#98104,#98105,#98106,#98107,#98108,#98109,
#98110,#98111,#98112,#98113,#98114,#98115,#98116,#98117,#98118,#98119,#98120,
#98121,#98122,#98123,#98124,#98125,#98126,#98127,#98128,#98129,#98130,#98131,
#98132,#98133,#98134,#98135,#98136,#98137,#98138,#98139,#98140,#98141,#98142,
#98143,#98144,#98145,#98146,#98147,#98148,#98149,#98150,#98151,#98152,#98153,
#98154,#98155,#98156,#98157,#98158,#98159,#98160,#98161,#98162,#98163,#98164,
#98165,#98166,#98167,#98168,#98169,#98170,#98171,#98172,#98173,#98174,#98175,
#98176,#98177,#98178,#98179,#98180,#98181,#98182,#98183,#98184,#98185,#98186,
#98187,#98188),.UNSPECIFIED.,.F.,.F.,(4,2,2,2,2,2,2,2,2,2,2,2,2,2,2,2,2,
2,2,2,2,2,2,2,2,2,2,2,2,2,2,2,2,2,2,2,2,2,2,2,2,2,2,2,2,2,2,2,2,2,2,2,2,
2,2,2,2,2,2,2,2,2,2,2,2,2,2,2,2,2,2,2,2,2,2,2,2,2,2,2,2,2,2,2,2,2,2,2,2,
2,2,2,2,2,2,2,2,2,2,2,2,2,2,2,2,2,2,4),(-2.22607311897124,-2.21929097350467,
-2.20184663678831,-2.1996738642096,-2.19861157330789,-2.19785293534124,
-2.19688868835388,-2.19523012968417,-2.18866018895975,-2.18202465914146,
-2.1521203992696,-2.14383516185461,-2.14129557415982,-2.13967641268918,
-2.13815761061215,-2.13615847872499,-2.13163701355976,-2.10723555996063,
-2.09078731868563,-2.08593247508836,-2.08269177223932,-2.08144472237794,
-2.08057944611062,-2.07978433102873,-2.07867198334757,-2.07574099727257,
-2.05735400750317,-2.03723455461772,-2.02679885505298,-2.02405837689652,
-2.02239530050497,-2.02089041594831,-2.01895373356547,-2.01489125575152,
-1.98437637370039,-1.96693249704206,-1.96475969277226,-1.96369737864859,
-1.96293872095436,-1.96197444458483,-1.96031582603649,-1.95374552485027,
-1.94710985140665,-1.91720450455584,-1.90891942598523,-1.90637981070113,
-1.90476061464001,-1.90324176820599,-1.90124256055587,-1.89672084748269,
-1.87232371251244,-1.85587126976998,-1.85101568780574,-1.84777459627112,
-1.84652746740652,-1.84566215915344,-1.84486703298962,-1.84375469399392,
-1.84082393163144,-1.82239978557885,-1.80230702524183,-1.79187884229759,
-1.78913892990292,-1.78747594903847,-1.78597099157341,-1.78403399194874,
-1.77997000837532,-1.74946525645529,-1.73201252422919,-1.72983942216229,
-1.72877703233859,-1.72801834901254,-1.72705407902309,-1.72539555590722,
-1.71882674723765,-1.71219058801633,-1.68228702651055,-1.6739982848203,
-1.67145823626562,-1.66983891760047,-1.66832006378673,-1.66632100343427,
-1.66180031506509,-1.63735816753994,-1.62093881526335,-1.616088531535,-1.61285004753217,
-1.61160329242204,-1.61073803966324,-1.60994280098531,-1.60883008851428,
-1.60589654520782,-1.58711761841533,-1.5672924211645,-1.55694138896825,
-1.55420778264581,-1.55254615509739,-1.5510408280934,-1.5491011136097,-1.54502298822946,
-1.51462822507784,-1.49708992145263,-1.49491433881309,-1.49385144290656,
-1.49309268530451,-1.4921287142232,-1.49047155714957,-1.48411343733603),
 .UNSPECIFIED.);
#1511=B_SPLINE_CURVE_WITH_KNOTS('',3,(#98189,#98190,#98191,#98192,#98193,
#98194,#98195,#98196,#98197,#98198,#98199,#98200,#98201,#98202,#98203,#98204,
#98205,#98206,#98207,#98208,#98209,#98210,#98211,#98212,#98213,#98214,#98215,
#98216,#98217,#98218,#98219,#98220,#98221,#98222,#98223,#98224,#98225,#98226,
#98227,#98228,#98229,#98230,#98231,#98232,#98233,#98234,#98235,#98236,#98237,
#98238,#98239,#98240,#98241,#98242,#98243,#98244,#98245,#98246,#98247,#98248,
#98249,#98250,#98251,#98252,#98253,#98254,#98255,#98256,#98257,#98258,#98259,
#98260,#98261,#98262,#98263,#98264,#98265,#98266,#98267,#98268,#98269,#98270,
#98271,#98272,#98273,#98274,#98275,#98276,#98277,#98278,#98279,#98280,#98281,
#98282,#98283,#98284,#98285,#98286,#98287,#98288,#98289,#98290,#98291,#98292,
#98293,#98294,#98295,#98296,#98297,#98298,#98299,#98300,#98301,#98302,#98303,
#98304,#98305,#98306,#98307,#98308,#98309,#98310,#98311,#98312,#98313,#98314,
#98315,#98316,#98317,#98318,#98319,#98320,#98321,#98322,#98323,#98324,#98325,
#98326,#98327,#98328,#98329,#98330,#98331,#98332,#98333,#98334,#98335,#98336,
#98337,#98338,#98339,#98340,#98341,#98342,#98343,#98344,#98345,#98346,#98347,
#98348,#98349,#98350,#98351,#98352,#98353,#98354,#98355,#98356,#98357,#98358,
#98359,#98360,#98361,#98362,#98363,#98364,#98365,#98366,#98367,#98368,#98369,
#98370,#98371,#98372,#98373,#98374,#98375,#98376,#98377,#98378,#98379,#98380,
#98381,#98382,#98383,#98384,#98385,#98386,#98387,#98388,#98389,#98390,#98391,
#98392,#98393,#98394),.UNSPECIFIED.,.F.,.F.,(4,2,2,2,2,2,2,2,2,2,2,2,2,
2,2,2,2,2,2,2,2,2,2,2,2,2,2,2,2,2,2,2,2,2,2,2,2,2,2,2,2,2,2,2,2,2,2,2,2,
2,2,2,2,2,2,2,2,2,2,2,2,2,2,2,2,2,2,2,2,2,2,2,2,2,2,2,2,2,2,2,2,2,2,2,2,
2,2,2,2,2,2,2,2,2,2,2,2,2,2,2,2,2,4),(-1.46482421780974,-1.46001994932202,
-1.43971559363077,-1.42155231735944,-1.41861317870521,-1.41749995646963,
-1.41670473759329,-1.41583995287812,-1.41459463946323,-1.41136415181476,
-1.40653016733953,-1.39020783042935,-1.36565915175576,-1.36114281590523,
-1.35914487918438,-1.35762656992739,-1.35600754100542,-1.3534673524203,
-1.3451731481688,-1.31526518534176,-1.30862017719824,-1.30204349333684,
-1.30038456908071,-1.29942037352597,-1.29866193967416,-1.2976001833691,
-1.2954293908031,-1.27804037321172,-1.24747212951246,-1.2434185308706,-1.24148381441753,
-1.2399794783136,-1.23831601924344,-1.23557263500235,-1.22509705304821,
-1.20483720260103,-1.18660948706426,-1.18367317733575,-1.18256028950037,
-1.18176514331254,-1.18090024639802,-1.17965445581982,-1.17642097704914,
-1.1715810280829,-1.15522245515856,-1.13072042524661,-1.12620262984951,
-1.12420439819367,-1.12268600169625,-1.12106701145758,-1.11852716029011,
-1.11023664378171,-1.08032474361402,-1.07367987417458,-1.06710105922155,
-1.0654419207791,-1.0644776570861,-1.06371920478855,-1.06265746829177,-1.06048687993743,
-1.04310686284157,-1.01252511141035,-1.0084729942557,-1.00653852202217,
-1.00503417473672,-1.00337049899509,-1.00062628266808,-0.990141242459935,
-0.969848582487102,-0.951665671743487,-0.948727246683078,-0.947614067007472,
-0.946818827236084,-0.945953960780812,-0.944708432285455,-0.941476846000052,
-0.936640758685802,-0.920306364980012,-0.895770732472425,-0.891253696576016,
-0.889255559335028,-0.887737140308702,-0.886118035340222,-0.883577813600781,
-0.875284306475449,-0.845373490488388,-0.83872816404903,-0.832150458556475,
-0.830491377321681,-0.82952710808295,-0.828768627223265,-0.827706819327287,
-0.825535972292219,-0.808148813821095,-0.777574698039789,-0.773521340243112,
-0.77158659457866,-0.770082173149268,-0.768418556118181,-0.765674763579876,
-0.755195668359902,-0.734924512360489,-0.722776382337732),.UNSPECIFIED.);
#1512=B_SPLINE_CURVE_WITH_KNOTS('',3,(#98399,#98400,#98401,#98402,#98403,
#98404,#98405,#98406,#98407,#98408,#98409,#98410,#98411,#98412,#98413,#98414,
#98415,#98416,#98417,#98418,#98419,#98420,#98421,#98422,#98423,#98424,#98425,
#98426,#98427,#98428,#98429,#98430,#98431,#98432,#98433,#98434,#98435,#98436,
#98437,#98438,#98439,#98440,#98441,#98442,#98443,#98444,#98445,#98446,#98447,
#98448,#98449,#98450,#98451,#98452,#98453,#98454,#98455,#98456,#98457,#98458,
#98459,#98460,#98461,#98462,#98463,#98464,#98465,#98466,#98467,#98468,#98469,
#98470,#98471,#98472,#98473,#98474,#98475,#98476,#98477,#98478,#98479,#98480,
#98481,#98482,#98483,#98484,#98485,#98486,#98487,#98488,#98489,#98490,#98491,
#98492,#98493,#98494,#98495,#98496,#98497,#98498,#98499,#98500,#98501,#98502,
#98503,#98504,#98505,#98506,#98507,#98508,#98509,#98510,#98511,#98512,#98513,
#98514,#98515,#98516,#98517,#98518,#98519,#98520,#98521,#98522,#98523,#98524,
#98525,#98526,#98527,#98528,#98529,#98530,#98531,#98532,#98533,#98534,#98535,
#98536,#98537,#98538,#98539,#98540,#98541,#98542,#98543,#98544,#98545,#98546,
#98547,#98548,#98549,#98550,#98551,#98552,#98553,#98554,#98555,#98556,#98557,
#98558,#98559,#98560,#98561,#98562,#98563,#98564,#98565,#98566,#98567,#98568,
#98569,#98570,#98571,#98572,#98573,#98574,#98575,#98576,#98577,#98578,#98579,
#98580,#98581,#98582,#98583,#98584,#98585,#98586,#98587,#98588,#98589,#98590,
#98591,#98592,#98593,#98594,#98595,#98596,#98597,#98598,#98599,#98600,#98601,
#98602,#98603,#98604,#98605,#98606,#98607,#98608,#98609,#98610,#98611,#98612,
#98613,#98614,#98615,#98616,#98617,#98618),.UNSPECIFIED.,.F.,.F.,(4,2,2,
2,2,2,2,2,2,2,2,2,2,2,2,2,2,2,2,2,2,2,2,2,2,2,2,2,2,2,2,2,2,2,2,2,2,2,2,
2,2,2,2,2,2,2,2,2,2,2,2,2,2,2,2,2,2,2,2,2,2,2,2,2,2,2,2,2,2,2,2,2,2,2,2,
2,2,2,2,2,2,2,2,2,2,2,2,2,2,2,2,2,2,2,2,2,2,2,2,2,2,2,2,2,2,2,2,2,2,4),
(-2.96795039865844,-2.96582312178668,-2.96411238401058,-2.96264615200535,
-2.96120232953042,-2.95976648285695,-2.95733638411068,-2.95061343729543,
-2.91678081521481,-2.90596739345903,-2.90412810799626,-2.90313443010285,
-2.90229532205603,-2.90122941424266,-2.899524286847,-2.88961158757631,-2.88031750535324,
-2.86580509013092,-2.85503624381333,-2.85044878485478,-2.84790946403175,
-2.84568861099755,-2.84415331235272,-2.84262041423798,-2.8407665656986,
-2.83632531186626,-2.81194750279753,-2.79550013957811,-2.79064561722568,
-2.78740514170684,-2.78615818805693,-2.78529298137241,-2.78449793249726,
-2.78338568043151,-2.78045497116021,-2.7620659038308,-2.74195074538013,
-2.73151665661648,-2.7287764644494,-2.72711353751422,-2.72560877270466,
-2.72367222270958,-2.71960994093126,-2.68909861461352,-2.67165534807906,
-2.66948269800173,-2.66842046605485,-2.66766186980976,-2.66669767532902,
-2.66503920584079,-2.65846960343412,-2.6518344420474,-2.62193178925201,
-2.61364705288247,-2.61110760951643,-2.60948853800343,-2.60796981886377,
-2.60597079403584,-2.60144956172376,-2.57705004995336,-2.56060225625885,
-2.55574760552114,-2.55250704402705,-2.55126005710661,-2.55039482727659,
-2.5495997570843,-2.54848747513251,-2.5455566865813,-2.52716720531476,-2.50705145006173,
-2.49661706525348,-2.49387679834531,-2.49221382658099,-2.49070902154583,
-2.4887724202592,-2.48471003267899,-2.45419786599084,-2.43675415023053,
-2.43458144248419,-2.43351918219339,-2.43276056564562,-2.43179634527647,
-2.43013783107876,-2.4235680491917,-2.41693271078169,-2.38702925172266,
-2.37874430083671,-2.37620479024701,-2.37458567554674,-2.37306691566721,
-2.37106783688021,-2.36654648105286,-2.34214641160455,-2.32569810507832,
-2.32084331263122,-2.31760265854901,-2.31635563735819,-2.31549038418914,
-2.3146952929029,-2.31358298190684,-2.31065212069231,-2.29226157465932,
-2.27214570480497,-2.26171116191006,-2.25897083156582,-2.25730781744919,
-2.25580297161136,-2.25386631433926,-2.24980379625315,-2.22607311897124),
 .UNSPECIFIED.);
#1513=B_SPLINE_CURVE_WITH_KNOTS('',3,(#98619,#98620,#98621,#98622,#98623,
#98624,#98625,#98626,#98627,#98628,#98629,#98630,#98631,#98632,#98633,#98634,
#98635,#98636,#98637,#98638,#98639,#98640,#98641,#98642,#98643,#98644,#98645,
#98646,#98647,#98648,#98649,#98650,#98651,#98652,#98653,#98654,#98655,#98656,
#98657,#98658,#98659,#98660,#98661,#98662,#98663,#98664,#98665,#98666,#98667,
#98668,#98669,#98670,#98671,#98672,#98673,#98674,#98675,#98676,#98677,#98678,
#98679,#98680,#98681,#98682,#98683,#98684,#98685,#98686,#98687,#98688,#98689,
#98690,#98691,#98692,#98693,#98694,#98695,#98696,#98697,#98698,#98699,#98700,
#98701,#98702,#98703,#98704,#98705,#98706,#98707,#98708,#98709,#98710,#98711,
#98712,#98713,#98714,#98715,#98716,#98717,#98718,#98719,#98720,#98721,#98722,
#98723,#98724,#98725,#98726,#98727,#98728,#98729,#98730,#98731,#98732,#98733,
#98734,#98735,#98736,#98737,#98738,#98739,#98740,#98741,#98742,#98743,#98744,
#98745,#98746,#98747,#98748,#98749,#98750,#98751,#98752,#98753,#98754,#98755,
#98756,#98757,#98758,#98759,#98760,#98761,#98762,#98763,#98764,#98765,#98766,
#98767,#98768,#98769,#98770,#98771,#98772,#98773,#98774,#98775,#98776,#98777,
#98778,#98779,#98780,#98781,#98782,#98783,#98784,#98785,#98786,#98787,#98788,
#98789,#98790,#98791,#98792,#98793,#98794,#98795,#98796,#98797,#98798,#98799,
#98800,#98801,#98802,#98803,#98804,#98805,#98806,#98807,#98808,#98809,#98810,
#98811,#98812,#98813,#98814,#98815,#98816,#98817,#98818,#98819,#98820,#98821,
#98822,#98823,#98824,#98825,#98826,#98827,#98828,#98829,#98830,#98831,#98832,
#98833,#98834,#98835,#98836,#98837,#98838,#98839,#98840,#98841,#98842),
 .UNSPECIFIED.,.F.,.F.,(4,2,2,2,2,2,2,2,2,2,2,2,2,2,2,2,2,2,2,2,2,2,2,2,
2,2,2,2,2,2,2,2,2,2,2,2,2,2,2,2,2,2,2,2,2,2,2,2,2,2,2,2,2,2,2,2,2,2,2,2,
2,2,2,2,2,2,2,2,2,2,2,2,2,2,2,2,2,2,2,2,2,2,2,2,2,2,2,2,2,2,2,2,2,2,2,2,
2,2,2,2,2,2,2,2,2,2,2,2,2,2,2,4),(-0.722776382337732,-0.71670969380575,
-0.713772601598928,-0.712659566861819,-0.711864349472997,-0.710999413964259,
-0.709753631907668,-0.706520531551523,-0.701681451522177,-0.685329089473591,
-0.660815835596637,-0.65629801331289,-0.654299699248656,-0.652781212609362,
-0.651162099776851,-0.648622000653125,-0.640330154988522,-0.610416925061539,
-0.603771556543183,-0.59719270324614,-0.595533490176064,-0.594569171791328,
-0.593810669414327,-0.592748853646526,-0.590578070347913,-0.573195013440525,
-0.542613806318726,-0.538561104060447,-0.536626445552064,-0.535121993832293,
-0.533458243669305,-0.530714000034983,-0.520230118854494,-0.499942624720985,
-0.481749372222675,-0.478811190096316,-0.477697993422082,-0.476902716937715,
-0.476037782284897,-0.474792108930055,-0.471559887721116,-0.466722630334772,
-0.450381907936951,-0.425851704769859,-0.42133418297843,-0.419335882791448,
-0.417817360234243,-0.416198164397421,-0.41365784112425,-0.405364385979259,
-0.37545120158245,-0.368805499226406,-0.362227085257113,-0.360567873271435,
-0.359603536395724,-0.358845007546557,-0.357783139236549,-0.355612192965832,
-0.33822533204436,-0.307647388778757,-0.303594008818171,-0.301659183930078,
-0.300154671082593,-0.298490922667605,-0.295746843055298,-0.28526572048483,
-0.264988492305487,-0.246779220897407,-0.243841645118142,-0.242728501367635,
-0.241933222833659,-0.241068240084413,-0.23982242177642,-0.236589403977412,
-0.231750597476462,-0.215400782040919,-0.190881167420983,-0.18636318553894,
-0.184364765777982,-0.182846185120308,-0.181226958856382,-0.178686654082288,
-0.170393878298478,-0.140479018320842,-0.133833186267082,-0.127254101028983,
-0.125594797115679,-0.12463042029666,-0.123871868440924,-0.122809978843987,
-0.120794313396195,-0.118085898298531,-0.11157921046003,-0.0847788066827937,
-0.0710930379762348,-0.0680476788053426,-0.0663000920922622,-0.0648201876150918,
-0.0630151221594017,-0.059840848056003,-0.0424085710450419,-0.0284568101529183,
-0.0241031573718179,-0.0103445925008922,-0.00853705100009869,-0.00745225982743724,
-0.00660984167598957,-0.00564199331628065,-0.00461671524486754,-0.0030282692782334,
0.,0.0193343403549321),.UNSPECIFIED.);
#1514=B_SPLINE_CURVE_WITH_KNOTS('',3,(#98847,#98848,#98849,#98850,#98851,
#98852,#98853,#98854,#98855,#98856,#98857,#98858,#98859,#98860,#98861,#98862,
#98863,#98864,#98865,#98866,#98867,#98868,#98869,#98870,#98871,#98872,#98873,
#98874,#98875,#98876,#98877,#98878,#98879,#98880,#98881,#98882,#98883,#98884,
#98885,#98886,#98887,#98888,#98889,#98890,#98891,#98892,#98893,#98894,#98895,
#98896,#98897,#98898,#98899,#98900,#98901,#98902,#98903,#98904,#98905,#98906,
#98907,#98908,#98909,#98910,#98911,#98912,#98913,#98914,#98915,#98916,#98917,
#98918,#98919,#98920,#98921,#98922,#98923,#98924,#98925,#98926,#98927,#98928,
#98929,#98930,#98931,#98932,#98933,#98934,#98935,#98936,#98937,#98938,#98939,
#98940,#98941,#98942,#98943,#98944,#98945,#98946,#98947,#98948,#98949,#98950,
#98951,#98952,#98953,#98954,#98955,#98956,#98957,#98958,#98959,#98960,#98961,
#98962,#98963,#98964,#98965,#98966,#98967,#98968,#98969,#98970,#98971,#98972,
#98973,#98974,#98975,#98976,#98977,#98978,#98979,#98980,#98981,#98982,#98983,
#98984,#98985,#98986,#98987,#98988,#98989,#98990,#98991,#98992,#98993,#98994,
#98995,#98996,#98997,#98998,#98999,#99000,#99001,#99002,#99003,#99004,#99005,
#99006,#99007,#99008,#99009,#99010,#99011,#99012,#99013,#99014,#99015,#99016,
#99017,#99018,#99019,#99020,#99021,#99022,#99023,#99024,#99025,#99026,#99027,
#99028,#99029,#99030,#99031,#99032,#99033,#99034,#99035,#99036,#99037,#99038,
#99039,#99040,#99041,#99042,#99043,#99044,#99045,#99046,#99047,#99048,#99049,
#99050,#99051,#99052,#99053,#99054,#99055,#99056,#99057,#99058,#99059,#99060,
#99061,#99062,#99063,#99064,#99065,#99066,#99067,#99068,#99069,#99070,#99071,
#99072,#99073,#99074,#99075,#99076,#99077,#99078,#99079,#99080,#99081,#99082,
#99083,#99084),.UNSPECIFIED.,.F.,.F.,(4,2,2,2,2,2,2,2,2,2,2,2,2,2,2,2,2,
2,2,2,2,2,2,2,2,2,2,2,2,2,2,2,2,2,2,2,2,2,2,2,2,2,2,2,2,2,2,2,2,2,2,2,2,
2,2,2,2,2,2,2,2,2,2,2,2,2,2,2,2,2,2,2,2,2,2,2,2,2,2,2,2,2,2,2,2,2,2,2,2,
2,2,2,2,2,2,2,2,2,2,2,2,2,2,2,2,2,2,2,2,2,2,2,2,2,2,2,2,2,4),(-0.742146480711913,
-0.730686365730827,-0.706301136079038,-0.701779365981078,-0.699779933249417,
-0.698260831564137,-0.69664128317838,-0.6941009498033,-0.685812224992619,
-0.655885402884276,-0.649238029918415,-0.642669736091088,-0.641011034774147,
-0.640046624672213,-0.63928779950678,-0.638225184193244,-0.636051499215259,
-0.618584850007295,-0.588113823977103,-0.584046575082922,-0.582108737104111,
-0.580603435324913,-0.578940384962293,-0.576201082965369,-0.565785281894072,
-0.545738250448365,-0.527217429904185,-0.524285677830778,-0.523173032747767,
-0.522377721668476,-0.521512242846235,-0.520264925092833,-0.517023612934832,
-0.512168520805433,-0.495720292912289,-0.471333966863692,-0.46681204825984,
-0.464812548098975,-0.463293394495491,-0.461673790097061,-0.459133367474245,
-0.450844338492267,-0.420916504703379,-0.414268901932379,-0.407700392410164,
-0.406041635001019,-0.405077192002399,-0.404318340776084,-0.403255688738652,
-0.401081927813235,-0.383614630955482,-0.353142622895265,-0.34907522644454,
-0.347137320465424,-0.345631966861323,-0.34396886025404,-0.341229467956718,
-0.330813354215518,-0.310765790287895,-0.292244127181168,-0.289312274777373,
-0.2881995915571,-0.287404253203741,-0.28653874468529,-0.28529138410809,
-0.282049960521632,-0.277194701361948,-0.260745906248171,-0.236358747608618,
-0.23183667378618,-0.229837105017573,-0.228317899298664,-0.226698239348884,
-0.224157729612459,-0.215868416588593,-0.185939555941578,-0.179291725161071,
-0.172722990169445,-0.171064175846755,-0.170099699761621,-0.169340822504424,
-0.168278134018156,-0.166104298545297,-0.148636403226273,-0.118163502966416,
-0.11417942824114,-0.112232673618163,-0.110758944782324,-0.110533163732709,
-0.1104708700406,-0.110417800358241,-0.110372121652461,-0.110332466450366,
-0.110297790673932,-0.110267281365393,-0.110240294786231,-0.110216313703445,
-0.110194917173601,-0.110175758736259,-0.110158550351455,-0.110123961628251,
-0.110090036369164,-0.110056716115043,-0.110023946513459,-0.109991676869477,
-0.108068324725186,-0.105966805335979,-0.102485666467731,-0.0769792213491306,
-0.0572382317910659,-0.0543144065797727,-0.053202700784251,-0.0524075883548014,
-0.0515417804150689,-0.0502930872286179,-0.0470431689749201,-0.0421708969525724,
-0.0256175127124944,-9.99999999140577E-7),.UNSPECIFIED.);
#1515=B_SPLINE_CURVE_WITH_KNOTS('',3,(#99085,#99086,#99087,#99088,#99089,
#99090,#99091,#99092,#99093,#99094,#99095,#99096,#99097,#99098,#99099,#99100,
#99101,#99102,#99103,#99104,#99105,#99106,#99107,#99108,#99109,#99110,#99111,
#99112,#99113,#99114,#99115,#99116,#99117,#99118,#99119,#99120,#99121,#99122,
#99123,#99124,#99125,#99126,#99127,#99128,#99129,#99130,#99131,#99132,#99133,
#99134,#99135,#99136,#99137,#99138,#99139,#99140,#99141,#99142,#99143,#99144,
#99145,#99146,#99147,#99148,#99149,#99150,#99151,#99152,#99153,#99154,#99155,
#99156,#99157,#99158,#99159,#99160,#99161,#99162,#99163,#99164,#99165,#99166,
#99167,#99168,#99169,#99170,#99171,#99172,#99173,#99174,#99175,#99176,#99177,
#99178,#99179,#99180,#99181,#99182,#99183,#99184,#99185,#99186,#99187,#99188,
#99189,#99190,#99191,#99192,#99193,#99194,#99195,#99196,#99197,#99198,#99199,
#99200,#99201,#99202,#99203,#99204,#99205,#99206,#99207,#99208,#99209,#99210,
#99211,#99212,#99213,#99214,#99215,#99216,#99217,#99218,#99219,#99220,#99221,
#99222,#99223,#99224,#99225,#99226,#99227,#99228,#99229,#99230,#99231,#99232,
#99233,#99234,#99235,#99236,#99237,#99238,#99239,#99240,#99241,#99242,#99243,
#99244,#99245,#99246,#99247,#99248,#99249,#99250,#99251,#99252,#99253,#99254,
#99255,#99256,#99257,#99258,#99259,#99260,#99261,#99262,#99263,#99264,#99265,
#99266,#99267,#99268,#99269,#99270,#99271,#99272,#99273,#99274,#99275,#99276,
#99277,#99278,#99279,#99280,#99281,#99282,#99283,#99284,#99285,#99286,#99287,
#99288,#99289,#99290,#99291,#99292,#99293,#99294,#99295,#99296,#99297,#99298,
#99299,#99300),.UNSPECIFIED.,.F.,.F.,(4,2,2,2,2,2,2,2,2,2,2,2,2,2,2,2,2,
2,2,2,2,2,2,2,2,2,2,2,2,2,2,2,2,2,2,2,2,2,2,2,2,2,2,2,2,2,2,2,2,2,2,2,2,
2,2,2,2,2,2,2,2,2,2,2,2,2,2,2,2,2,2,2,2,2,2,2,2,2,2,2,2,2,2,2,2,2,2,2,2,
2,2,2,2,2,2,2,2,2,2,2,2,2,2,2,2,2,2,4),(-2.9676701370104,-2.94175666738961,
-2.93911264794775,-2.93735604142886,-2.93566511119323,-2.93416660720203,
-2.93228094658283,-2.92931607151012,-2.90954221254287,-2.89532384694272,
-2.88024403955377,-2.87805100644773,-2.87696642087232,-2.87613383411841,
-2.87515776976436,-2.87344594860904,-2.86617758918803,-2.86127925981406,
-2.83190743163019,-2.82242996351109,-2.81982952527453,-2.81816661510919,
-2.81666296236614,-2.81472938693359,-2.81067918087877,-2.78009126943132,
-2.76271514019006,-2.76054530273761,-2.75948399659913,-2.75872588236757,
-2.75776207667931,-2.7561038116788,-2.74952919486424,-2.74289679569286,
-2.71302077081229,-2.70472647192174,-2.70218695668462,-2.70056849673392,
-2.69905081760935,-2.69705384973015,-2.69254035461096,-2.66792153002845,
-2.65164575931562,-2.64681995367273,-2.64359414087782,-2.64234982538102,
-2.64148547827381,-2.64069045329864,-2.63957723660059,-2.63663566807151,
-2.61857598497361,-2.59823043969221,-2.5877324070383,-2.58498800070745,
-2.58332474453713,-2.58182111807604,-2.57988805090804,-2.5758406874834,
-2.54522911815593,-2.5278698895905,-2.52570049068269,-2.52463925327488,
-2.52388112878865,-2.52291722870322,-2.52125862474109,-2.51468032824387,
-2.50804838616223,-2.47816611384685,-2.46987878503141,-2.46733996214793,
-2.46572162242803,-2.4642038312463,-2.4622063880866,-2.45769037600957,-2.43315483291176,
-2.41681549354176,-2.41197926626567,-2.40874824962633,-2.40750312476058,
-2.40663860409561,-2.40584373137623,-2.40473114061371,-2.40179468494817,
-2.38363538680355,-2.3679916574597,-2.35832091319345,-2.35405512121286,
-2.35065967814731,-2.34885648076452,-2.34737742590961,-2.34563004371517,
-2.34258300517303,-2.32884344524328,-2.30416459414037,-2.29255548730127,
-2.29068799029271,-2.28968857269036,-2.2888502841821,-2.28779261726404,
-2.28611404246069,-2.27671606336304,-2.24772936495183,-2.23568382370033,
-2.23282413022014,-2.23113558923967,-2.2296367125002,-2.22774724283736,
-2.22596222870392),.UNSPECIFIED.);
#1516=B_SPLINE_CURVE_WITH_KNOTS('',3,(#99305,#99306,#99307,#99308,#99309,
#99310,#99311,#99312,#99313,#99314,#99315,#99316,#99317,#99318,#99319,#99320,
#99321,#99322,#99323,#99324,#99325,#99326,#99327,#99328,#99329,#99330,#99331,
#99332,#99333,#99334,#99335,#99336,#99337,#99338,#99339,#99340,#99341,#99342,
#99343,#99344,#99345,#99346,#99347,#99348,#99349,#99350,#99351,#99352,#99353,
#99354,#99355,#99356,#99357,#99358,#99359,#99360,#99361,#99362,#99363,#99364,
#99365,#99366,#99367,#99368,#99369,#99370,#99371,#99372,#99373,#99374,#99375,
#99376,#99377,#99378,#99379,#99380,#99381,#99382,#99383,#99384,#99385,#99386,
#99387,#99388,#99389,#99390,#99391,#99392,#99393,#99394,#99395,#99396,#99397,
#99398,#99399,#99400,#99401,#99402,#99403,#99404,#99405,#99406,#99407,#99408,
#99409,#99410,#99411,#99412,#99413,#99414,#99415,#99416,#99417,#99418,#99419,
#99420,#99421,#99422,#99423,#99424,#99425,#99426,#99427,#99428,#99429,#99430,
#99431,#99432,#99433,#99434,#99435,#99436,#99437,#99438,#99439,#99440,#99441,
#99442,#99443,#99444,#99445,#99446,#99447,#99448,#99449,#99450,#99451,#99452,
#99453,#99454,#99455,#99456,#99457,#99458,#99459,#99460,#99461,#99462,#99463,
#99464,#99465,#99466,#99467,#99468,#99469,#99470,#99471,#99472,#99473,#99474,
#99475,#99476,#99477,#99478,#99479,#99480,#99481,#99482,#99483,#99484,#99485,
#99486,#99487,#99488,#99489,#99490,#99491,#99492,#99493,#99494,#99495,#99496,
#99497,#99498,#99499,#99500,#99501,#99502,#99503,#99504,#99505,#99506,#99507,
#99508,#99509,#99510,#99511,#99512,#99513,#99514,#99515,#99516,#99517,#99518,
#99519,#99520),.UNSPECIFIED.,.F.,.F.,(4,2,2,2,2,2,2,2,2,2,2,2,2,2,2,2,2,
2,2,2,2,2,2,2,2,2,2,2,2,2,2,2,2,2,2,2,2,2,2,2,2,2,2,2,2,2,2,2,2,2,2,2,2,
2,2,2,2,2,2,2,2,2,2,2,2,2,2,2,2,2,2,2,2,2,2,2,2,2,2,2,2,2,2,2,2,2,2,2,2,
2,2,2,2,2,2,2,2,2,2,2,2,2,2,2,2,2,2,4),(-1.48420216693846,-1.48081117371075,
-1.4656063909844,-1.46360488387489,-1.4625640121514,-1.46172587250738,-1.46071069853317,
-1.45877011247224,-1.44455498745966,-1.43632198942973,-1.41113250435355,
-1.40663681474194,-1.40464211160295,-1.40312393804102,-1.40150280890822,
-1.39895458212505,-1.39058917641951,-1.3607240811837,-1.35407046888925,
-1.34754095724135,-1.3458856571652,-1.34492210261443,-1.34416324876302,
-1.34309968101823,-1.34092076364548,-1.32326191197243,-1.29304695297833,
-1.28935604326243,-1.28746819059756,-1.28606624721167,-1.28453163077674,
-1.28240556694461,-1.27726605129387,-1.25534986017643,-1.23187639153396,
-1.22910368924323,-1.22801485561443,-1.22722580644576,-1.22635450400148,
-1.22507749517868,-1.22163445716663,-1.20040089788481,-1.17621916959604,
-1.17169290770253,-1.16969276868369,-1.16817362927291,-1.16655452029471,
-1.16401588291926,-1.15574207666808,-1.12580645197037,-1.11916080804386,
-1.11258599987531,-1.11092682671214,-1.10996234694199,-1.10920359471085,
-1.10814124739732,-1.10596870625297,-1.08853818379277,-1.05802357127363,
-1.05396241044446,-1.05202580697739,-1.0505207417855,-1.0488572198512,-1.04611544113931,
-1.03566790215954,-1.01550903437464,-0.997141670835854,-0.994209015949504,
-0.993096305706441,-0.992301010968272,-0.991435622422391,-0.990188554463272,
-0.986948558230927,-0.98209600434782,-0.965662553418826,-0.941259789740869,
-0.936738637592961,-0.934739352991742,-0.933220315039454,-0.931600787648849,
-0.929060388590836,-0.920770528781568,-0.890845751993523,-0.884198472029847,
-0.87763107779755,-0.875972488476971,-0.875008123378191,-0.874249321063157,
-0.873186721438305,-0.871013009961648,-0.853543493258314,-0.823077962683899,
-0.819010277383013,-0.817072394987168,-0.815567129510281,-0.813904191039501,
-0.811165239685877,-0.800752949348432,-0.780717589997058,-0.762182677960775,
-0.759251038299022,-0.758138431894522,-0.757343147558453,-0.756477696797236,
-0.755230417765071,-0.75198919664362,-0.747134232721038,-0.742146480711913),
 .UNSPECIFIED.);
#1517=B_SPLINE_CURVE_WITH_KNOTS('',3,(#99521,#99522,#99523,#99524,#99525,
#99526,#99527,#99528,#99529,#99530,#99531,#99532,#99533,#99534,#99535,#99536,
#99537,#99538,#99539,#99540,#99541,#99542,#99543,#99544,#99545,#99546,#99547,
#99548,#99549,#99550,#99551,#99552,#99553,#99554,#99555,#99556,#99557,#99558,
#99559,#99560,#99561,#99562,#99563,#99564,#99565,#99566,#99567,#99568,#99569,
#99570,#99571,#99572,#99573,#99574,#99575,#99576,#99577,#99578,#99579,#99580,
#99581,#99582,#99583,#99584,#99585,#99586,#99587,#99588,#99589,#99590,#99591,
#99592,#99593,#99594,#99595,#99596,#99597,#99598,#99599,#99600,#99601,#99602,
#99603,#99604,#99605,#99606,#99607,#99608,#99609,#99610,#99611,#99612,#99613,
#99614,#99615,#99616,#99617,#99618,#99619,#99620,#99621,#99622,#99623,#99624,
#99625,#99626,#99627,#99628,#99629,#99630,#99631,#99632,#99633,#99634,#99635,
#99636,#99637,#99638,#99639,#99640,#99641,#99642,#99643,#99644,#99645,#99646,
#99647,#99648,#99649,#99650,#99651,#99652,#99653,#99654,#99655,#99656,#99657,
#99658,#99659,#99660,#99661,#99662,#99663,#99664,#99665,#99666,#99667,#99668,
#99669,#99670,#99671,#99672,#99673,#99674,#99675,#99676,#99677,#99678,#99679,
#99680,#99681,#99682,#99683,#99684,#99685,#99686,#99687,#99688,#99689,#99690,
#99691,#99692,#99693,#99694,#99695,#99696,#99697,#99698,#99699,#99700,#99701,
#99702,#99703,#99704,#99705,#99706,#99707,#99708,#99709,#99710,#99711,#99712,
#99713,#99714,#99715,#99716,#99717,#99718,#99719,#99720,#99721,#99722,#99723,
#99724,#99725,#99726),.UNSPECIFIED.,.F.,.F.,(4,2,2,2,2,2,2,2,2,2,2,2,2,
2,2,2,2,2,2,2,2,2,2,2,2,2,2,2,2,2,2,2,2,2,2,2,2,2,2,2,2,2,2,2,2,2,2,2,2,
2,2,2,2,2,2,2,2,2,2,2,2,2,2,2,2,2,2,2,2,2,2,2,2,2,2,2,2,2,2,2,2,2,2,2,2,
2,2,2,2,2,2,2,2,2,2,2,2,2,2,2,2,2,4),(-2.22596222870392,-2.22476976080297,
-2.20318940350078,-2.18313477087351,-2.17487161453999,-2.17315354888634,
-2.1721862650835,-2.17134425760098,-2.17025990643865,-2.16845292359828,
-2.15466496615236,-2.13375959174518,-2.11920139599229,-2.11581961256073,
-2.11401922318127,-2.11254022155332,-2.11079025655054,-2.10773195555156,
-2.09377458483878,-2.06669502388854,-2.05754061755594,-2.05577465636391,
-2.05479693456033,-2.05395645742597,-2.05286954309243,-2.05109345642804,
-2.03912127154843,-2.0190612341553,-2.00293452490127,-1.99883339538176,
-1.99688995572536,-1.99538484512809,-1.99372659694651,-1.99100580380971,
-1.98190045207522,-1.97546321472832,-1.95167918798749,-1.94398151414005,
-1.94094735507046,-1.93868230994526,-1.93760234797305,-1.93676246146497,
-1.93577985208639,-1.93403966073558,-1.9263604773608,-1.89572667905436,
-1.88345256978119,-1.88057739515835,-1.87888540394194,-1.8773869402259,
-1.87550264055797,-1.87254249054539,-1.85327417467825,-1.83106504551911,
-1.82262575636492,-1.82089760729077,-1.81992808801895,-1.81908639155126,
-1.81800529781344,-1.81620962043365,-1.80366283492563,-1.77397346609612,
-1.7654200274196,-1.76285331455238,-1.76122883542191,-1.75971335741571,
-1.75773062864765,-1.75329852034088,-1.72672859928168,-1.70591066469657,
-1.70374283550844,-1.70268186617172,-1.70192372954294,-1.70095953476934,
-1.69929981736681,-1.69270906636629,-1.68607889498275,-1.65617594406913,
-1.64791292450111,-1.64537657491691,-1.64375870141099,-1.64224056911165,
-1.64024154086236,-1.6357169367613,-1.61151008596343,-1.59491959370344,
-1.59004263984899,-1.58679136311717,-1.58554312917557,-1.58467796615649,
-1.58388371745364,-1.58277360308433,-1.57985691403693,-1.55979584464193,
-1.54070611286403,-1.53416029517888,-1.52941831444084,-1.52735944504096,
-1.52583729136321,-1.52442127220101,-1.52247492705227,-1.51748447566437,
-1.48417870616889),.UNSPECIFIED.);
#1518=B_SPLINE_CURVE_WITH_KNOTS('',3,(#99731,#99732,#99733,#99734,#99735,
#99736,#99737,#99738,#99739,#99740,#99741,#99742,#99743,#99744,#99745,#99746,
#99747,#99748,#99749,#99750,#99751,#99752,#99753,#99754,#99755,#99756,#99757,
#99758,#99759,#99760,#99761,#99762,#99763,#99764,#99765,#99766,#99767,#99768,
#99769,#99770,#99771,#99772,#99773,#99774,#99775,#99776,#99777,#99778,#99779,
#99780,#99781,#99782,#99783,#99784,#99785,#99786,#99787,#99788,#99789,#99790,
#99791,#99792,#99793,#99794,#99795,#99796,#99797,#99798,#99799,#99800,#99801,
#99802,#99803,#99804,#99805,#99806,#99807,#99808,#99809,#99810,#99811,#99812,
#99813,#99814,#99815,#99816,#99817,#99818,#99819,#99820,#99821,#99822,#99823,
#99824,#99825,#99826,#99827,#99828,#99829,#99830,#99831,#99832,#99833,#99834,
#99835,#99836,#99837,#99838,#99839,#99840,#99841,#99842,#99843,#99844,#99845,
#99846,#99847,#99848,#99849,#99850,#99851,#99852,#99853,#99854,#99855,#99856,
#99857,#99858,#99859,#99860,#99861,#99862,#99863,#99864,#99865,#99866,#99867,
#99868,#99869,#99870,#99871,#99872,#99873,#99874,#99875,#99876,#99877,#99878,
#99879,#99880,#99881,#99882,#99883,#99884,#99885,#99886,#99887,#99888,#99889,
#99890,#99891,#99892,#99893,#99894,#99895,#99896,#99897,#99898,#99899,#99900,
#99901,#99902,#99903,#99904,#99905,#99906,#99907,#99908,#99909,#99910,#99911,
#99912,#99913,#99914,#99915,#99916,#99917,#99918,#99919,#99920,#99921,#99922,
#99923,#99924,#99925,#99926,#99927,#99928,#99929,#99930,#99931,#99932,#99933,
#99934,#99935,#99936,#99937,#99938,#99939,#99940,#99941,#99942),
 .UNSPECIFIED.,.F.,.F.,(4,2,2,2,2,2,2,2,2,2,2,2,2,2,2,2,2,2,2,2,2,2,2,2,
2,2,2,2,2,2,2,2,2,2,2,2,2,2,2,2,2,2,2,2,2,2,2,2,2,2,2,2,2,2,2,2,2,2,2,2,
2,2,2,2,2,2,2,2,2,2,2,2,2,2,2,2,2,2,2,2,2,2,2,2,2,2,2,2,2,2,2,2,2,2,2,2,
2,2,2,2,2,2,2,2,2,4),(-2.22616681243302,-2.22604246147792,-2.22453767372853,
-2.22260111388507,-2.21853888542679,-2.18802607251338,-2.17058324476156,
-2.16841057850465,-2.16734833249655,-2.16658972370756,-2.16562550985455,
-2.16396699961134,-2.15739713765143,-2.15076188957102,-2.12085849610008,
-2.11257392064909,-2.11003446589562,-2.10841537359118,-2.10689662546881,
-2.10489754866071,-2.10037613785273,-2.0759801652396,-2.05952909573883,
-2.05467387749143,-2.05143302010607,-2.05018597549344,-2.04932072380644,
-2.04852564810396,-2.04741337769718,-2.04448277941868,-2.02606385120704,
-2.00596938737891,-1.9955410178392,-1.99280121175038,-1.99113832274565,
-1.98963346599106,-1.98769662063731,-1.98363305345516,-1.95312906116816,
-1.93567838150813,-1.93350544611992,-1.93244313006603,-1.93168449628269,
-1.93072028496013,-1.92906185342671,-1.92249328447566,-1.91585758747718,
-1.88595567028374,-1.87766784313493,-1.87512799877584,-1.87350879334234,
-1.87199003386457,-1.86999108035674,-1.86547055734127,-1.84103481852673,
-1.82461287616393,-1.81976231410155,-1.81652374551662,-1.8152770264833,
-1.814411820986,-1.81361664357233,-1.81250404038425,-1.8095709814,-1.79086169529351,
-1.77098631377317,-1.76413109542401,-1.75921852717353,-1.75713003344748,
-1.7556022073965,-1.75419230180041,-1.75227200996737,-1.74845036941389,
-1.71949921476802,-1.70082456986282,-1.69861823578307,-1.69754934406224,
-1.69670989443295,-1.69571816669359,-1.69393908298723,-1.68565535438361,
-1.65560409078445,-1.64340456818339,-1.64053333214333,-1.63884163392006,
-1.63734218593728,-1.63545497775124,-1.63248693931853,-1.60993090572051,
-1.59366313410074,-1.58631735076348,-1.582027395654,-1.58059066880361,-1.57977514760289,
-1.57892338428559,-1.57775215062521,-1.57498474011419,-1.57104927554577,
-1.55954787230436,-1.53206055775014,-1.5251497725076,-1.52268964888888,
-1.52124777940947,-1.5197379733565,-1.51776359585784,-1.51349965249691,
-1.48420216693846),.UNSPECIFIED.);
#1519=B_SPLINE_CURVE_WITH_KNOTS('',3,(#99943,#99944,#99945,#99946,#99947,
#99948,#99949,#99950,#99951,#99952,#99953,#99954,#99955,#99956,#99957,#99958,
#99959,#99960,#99961,#99962,#99963,#99964,#99965,#99966,#99967,#99968,#99969,
#99970,#99971,#99972,#99973,#99974,#99975,#99976,#99977,#99978,#99979,#99980,
#99981,#99982,#99983,#99984,#99985,#99986,#99987,#99988,#99989,#99990,#99991,
#99992,#99993,#99994,#99995,#99996,#99997,#99998,#99999,#100000,#100001,
#100002,#100003,#100004,#100005,#100006,#100007,#100008,#100009,#100010,
#100011,#100012,#100013,#100014,#100015,#100016,#100017,#100018,#100019,
#100020,#100021,#100022,#100023,#100024,#100025,#100026,#100027,#100028,
#100029,#100030,#100031,#100032,#100033,#100034,#100035,#100036,#100037,
#100038,#100039,#100040,#100041,#100042,#100043,#100044,#100045,#100046,
#100047,#100048,#100049,#100050,#100051,#100052,#100053,#100054,#100055,
#100056,#100057,#100058,#100059,#100060,#100061,#100062,#100063,#100064,
#100065,#100066,#100067,#100068,#100069,#100070,#100071,#100072,#100073,
#100074,#100075,#100076,#100077,#100078,#100079,#100080,#100081,#100082,
#100083,#100084,#100085,#100086,#100087,#100088,#100089,#100090,#100091,
#100092,#100093,#100094,#100095,#100096,#100097,#100098,#100099,#100100,
#100101,#100102,#100103,#100104,#100105,#100106,#100107,#100108,#100109,
#100110,#100111,#100112,#100113,#100114,#100115,#100116,#100117,#100118,
#100119,#100120,#100121,#100122,#100123,#100124,#100125,#100126,#100127,
#100128,#100129,#100130,#100131,#100132,#100133,#100134,#100135,#100136,
#100137,#100138,#100139,#100140,#100141,#100142,#100143,#100144,#100145,
#100146,#100147,#100148,#100149,#100150,#100151,#100152,#100153,#100154,
#100155,#100156,#100157,#100158),.UNSPECIFIED.,.F.,.F.,(4,2,2,2,2,2,2,2,
2,2,2,2,2,2,2,2,2,2,2,2,2,2,2,2,2,2,2,2,2,2,2,2,2,2,2,2,2,2,2,2,2,2,2,2,
2,2,2,2,2,2,2,2,2,2,2,2,2,2,2,2,2,2,2,2,2,2,2,2,2,2,2,2,2,2,2,2,2,2,2,2,
2,2,2,2,2,2,2,2,2,2,2,2,2,2,2,2,2,2,2,2,2,2,2,2,2,2,2,4),(-1.48417870616889,
-1.48393864425358,-1.48218042152621,-1.47828722870527,-1.47039019383324,
-1.46863521841759,-1.46764923408789,-1.46680968537757,-1.46573431696964,
-1.46349314672872,-1.46050035275944,-1.45295920686657,-1.43691964324222,
-1.41444181724997,-1.4114850135209,-1.40960160813851,-1.40810308358595,
-1.40641020214032,-1.40353149130104,-1.39120840242425,-1.36021101942625,
-1.35287536391893,-1.3511583709944,-1.35018095479658,-1.34934826346162,
-1.34826491112707,-1.3459827594878,-1.34291950355474,-1.33511230179353,
-1.31066661567715,-1.29666156507403,-1.29360044170085,-1.2918495861168,
-1.29037025048514,-1.28856996568095,-1.28518994678059,-1.26068986106189,
-1.23712084191432,-1.23435220323809,-1.23326430350343,-1.23247570180016,
-1.23160463622985,-1.23032756234818,-1.22688189678002,-1.20560226588492,
-1.1814736562158,-1.17694705254759,-1.17494733752316,-1.1734287539856,-1.17181046799911,
-1.16927361820722,-1.16101056983662,-1.13107979173519,-1.12443765768997,
-1.11784608999374,-1.11618594100828,-1.11522147365623,-1.11446310033037,
-1.11340178474876,-1.11123316954272,-1.0901872640142,-1.06387483590322,
-1.05942866590538,-1.05744305854541,-1.05592672634565,-1.05430264060515,
-1.05173933814198,-1.04322466931433,-1.0134780200184,-1.00090081220348,
-0.999103587016294,-0.998021852613617,-0.997179837181083,-0.996210148631531,
-0.994482184411101,-0.986053134210115,-0.965158653727647,-0.944593332047074,
-0.941621671328921,-0.93973352069584,-0.938234202905426,-0.936543589225841,
-0.933676522086198,-0.921536132578467,-0.891932755995872,-0.883150201351662,
-0.881500942245093,-0.880451909101975,-0.879613650273504,-0.878606096497797,
-0.87670140467154,-0.863910477887846,-0.836205157950646,-0.826223308464406,
-0.823414449814019,-0.821736523109991,-0.820385150800801,-0.818550241131409,
-0.815003470991717,-0.79046657118555,-0.767218981199978,-0.764437960361355,
-0.763347817290045,-0.762558539105024,-0.761687846440725,-0.760413215882158,
-0.756985559074815,-0.742164101532787),.UNSPECIFIED.);
#1520=B_SPLINE_CURVE_WITH_KNOTS('',3,(#100163,#100164,#100165,#100166,#100167,
#100168,#100169,#100170,#100171,#100172,#100173,#100174,#100175,#100176,
#100177,#100178,#100179,#100180,#100181,#100182,#100183,#100184,#100185,
#100186,#100187,#100188,#100189,#100190,#100191,#100192,#100193,#100194,
#100195,#100196,#100197,#100198,#100199,#100200,#100201,#100202,#100203,
#100204,#100205,#100206,#100207,#100208,#100209,#100210,#100211,#100212,
#100213,#100214,#100215,#100216,#100217,#100218,#100219,#100220,#100221,
#100222,#100223,#100224,#100225,#100226,#100227,#100228,#100229,#100230,
#100231,#100232,#100233,#100234,#100235,#100236,#100237,#100238,#100239,
#100240,#100241,#100242,#100243,#100244,#100245,#100246,#100247,#100248,
#100249,#100250,#100251,#100252,#100253,#100254,#100255,#100256,#100257,
#100258,#100259,#100260,#100261,#100262,#100263,#100264,#100265,#100266,
#100267,#100268,#100269,#100270,#100271,#100272,#100273,#100274,#100275,
#100276,#100277,#100278,#100279,#100280,#100281,#100282,#100283,#100284,
#100285,#100286,#100287,#100288,#100289,#100290,#100291,#100292,#100293,
#100294,#100295,#100296,#100297,#100298,#100299,#100300,#100301,#100302,
#100303,#100304,#100305,#100306,#100307,#100308,#100309,#100310,#100311,
#100312,#100313,#100314,#100315,#100316,#100317,#100318,#100319,#100320,
#100321,#100322,#100323,#100324,#100325,#100326,#100327,#100328,#100329,
#100330,#100331,#100332,#100333,#100334,#100335,#100336,#100337,#100338,
#100339,#100340,#100341,#100342,#100343,#100344,#100345,#100346,#100347,
#100348,#100349,#100350,#100351,#100352,#100353,#100354,#100355,#100356,
#100357,#100358,#100359,#100360,#100361,#100362,#100363,#100364,#100365,
#100366,#100367,#100368,#100369,#100370,#100371,#100372),.UNSPECIFIED.,
 .F.,.F.,(4,2,2,2,2,2,2,2,2,2,2,2,2,2,2,2,2,2,2,2,2,2,2,2,2,2,2,2,2,2,2,
2,2,2,2,2,2,2,2,2,2,2,2,2,2,2,2,2,2,2,2,2,2,2,2,2,2,2,2,2,2,2,2,2,2,2,2,
2,2,2,2,2,2,2,2,2,2,2,2,2,2,2,2,2,2,2,2,2,2,2,2,2,2,2,2,2,2,2,2,2,2,2,2,
2,4),(-2.96801447478129,-2.96566606301484,-2.94555217476699,-2.93511874503777,
-2.93237872598084,-2.93071590410633,-2.929211234369,-2.92727480673222,-2.92321278164468,
-2.89270338276873,-2.87526121851301,-2.87308870571027,-2.87202654087673,
-2.87126799255996,-2.87030385899625,-2.86864549428685,-2.86207630690686,
-2.85544156473784,-2.82554080113032,-2.81725658827659,-2.8147173053619,
-2.81309833614395,-2.81157971295625,-2.80958081442194,-2.80505986773348,
-2.78066189864089,-2.76421514327792,-2.75936079912144,-2.75612044229885,
-2.75487353415286,-2.75400835898611,-2.7532133390287,-2.75210112735967,
-2.74917052404422,-2.730782197954,-2.71066771856115,-2.70023399441319,-2.69749390075135,
-2.69583103407927,-2.69432632411209,-2.6923898451321,-2.68832771396066,
-2.65781747701803,-2.64037486183409,-2.63820229131619,-2.63714009813048,
-2.63638152951123,-2.63541737006762,-2.63375896068065,-2.62718959417551,
-2.62055467493251,-2.59065310564982,-2.58236867758816,-2.57982932737951,
-2.57821031496099,-2.57669165104294,-2.57469269859435,-2.57017162863388,
-2.54577309267923,-2.52932583149074,-2.52447134676194,-2.52123089791694,
-2.51998395558743,-2.51911875709964,-2.51832371603074,-2.51721147524773,
-2.51428079871268,-2.49589146325859,-2.47577682827127,-2.46534293431623,
-2.462602776261,-2.46093986702863,-2.45943511631044,-2.45749858174765,-2.45343632217927,
-2.4229254219056,-2.40548222190687,-2.40330958984779,-2.4022473675554,-2.40148877854864,
-2.40052459373867,-2.39886614190593,-2.39229662291705,-2.3856615216754,
-2.35575918801667,-2.34747448976598,-2.34493506642525,-2.34331600953875,
-2.34179730542131,-2.33979830226663,-2.3352771273439,-2.31087730753948,
-2.29443008280833,-2.28957554523006,-2.28633504789604,-2.28508807795948,
-2.28422285742077,-2.28342779376688,-2.28231551832051,-2.27938472497521,
-2.26099858451193,-2.24088067951307,-2.23044572474394,-2.22770542927393,
-2.22616681243302),.UNSPECIFIED.);
#1521=B_SPLINE_CURVE_WITH_KNOTS('',3,(#100373,#100374,#100375,#100376,#100377,
#100378,#100379,#100380,#100381,#100382,#100383,#100384,#100385,#100386,
#100387,#100388,#100389,#100390,#100391,#100392,#100393,#100394,#100395,
#100396,#100397,#100398,#100399,#100400,#100401,#100402,#100403,#100404,
#100405,#100406,#100407,#100408,#100409,#100410,#100411,#100412,#100413,
#100414,#100415,#100416,#100417,#100418,#100419,#100420,#100421,#100422,
#100423,#100424,#100425,#100426,#100427,#100428,#100429,#100430,#100431,
#100432,#100433,#100434,#100435,#100436,#100437,#100438,#100439,#100440,
#100441,#100442,#100443,#100444,#100445,#100446,#100447,#100448,#100449,
#100450,#100451,#100452,#100453,#100454,#100455,#100456,#100457,#100458,
#100459,#100460,#100461,#100462,#100463,#100464,#100465,#100466,#100467,
#100468,#100469,#100470,#100471,#100472,#100473,#100474,#100475,#100476,
#100477,#100478,#100479,#100480,#100481,#100482,#100483,#100484,#100485,
#100486,#100487,#100488,#100489,#100490,#100491,#100492,#100493,#100494,
#100495,#100496,#100497,#100498,#100499,#100500,#100501,#100502,#100503,
#100504,#100505,#100506,#100507,#100508,#100509,#100510,#100511,#100512,
#100513,#100514,#100515,#100516,#100517,#100518,#100519,#100520,#100521,
#100522,#100523,#100524,#100525,#100526,#100527,#100528,#100529,#100530,
#100531,#100532,#100533,#100534,#100535,#100536,#100537,#100538,#100539,
#100540,#100541,#100542,#100543,#100544,#100545,#100546,#100547,#100548,
#100549,#100550,#100551,#100552,#100553,#100554,#100555,#100556,#100557,
#100558,#100559,#100560,#100561,#100562,#100563,#100564,#100565,#100566,
#100567,#100568,#100569,#100570,#100571,#100572,#100573,#100574,#100575,
#100576,#100577,#100578,#100579,#100580,#100581,#100582),.UNSPECIFIED.,
 .F.,.F.,(4,2,2,2,2,2,2,2,2,2,2,2,2,2,2,2,2,2,2,2,2,2,2,2,2,2,2,2,2,2,2,
2,2,2,2,2,2,2,2,2,2,2,2,2,2,2,2,2,2,2,2,2,2,2,2,2,2,2,2,2,2,2,2,2,2,2,2,
2,2,2,2,2,2,2,2,2,2,2,2,2,2,2,2,2,2,2,2,2,2,2,2,2,2,2,2,2,2,2,2,2,2,2,2,
2,4),(-0.742164101532787,-0.735971382998655,-0.711532708451572,-0.7070124647953,
-0.705013628555544,-0.703494959260892,-0.701875857657293,-0.69933620881987,
-0.691049873326518,-0.661129576938896,-0.654484222027339,-0.647901840908411,
-0.646242242945901,-0.645277788803992,-0.644519234492205,-0.643457417216243,
-0.641286886214012,-0.623917327195036,-0.593314120394164,-0.589263609088311,
-0.587329273300069,-0.585824758232584,-0.584160618550969,-0.581414989788193,
-0.57091597675433,-0.550576374908781,-0.532453481139082,-0.529511418512946,
-0.528397670971167,-0.527602207833066,-0.526737308123534,-0.525492077579572,
-0.522263183513004,-0.517432752772695,-0.501135022417639,-0.476543905369007,
-0.472027680492035,-0.470029510502894,-0.468510913727838,-0.466891472113768,
-0.4643504130524,-0.456051281306886,-0.426139443141783,-0.419492756867436,
-0.412916242256106,-0.411257099863112,-0.410292732049222,-0.409534134327624,
-0.408472111783265,-0.40630064270998,-0.38890025524091,-0.358335714082141,
-0.354279965561734,-0.352344596292237,-0.350839914659885,-0.34917623812735,
-0.346432877600162,-0.335962437692785,-0.315724167965985,-0.297456476807057,
-0.294520931592771,-0.293407985434298,-0.292612718982639,-0.291747600778781,
-0.290501342131511,-0.287265818221643,-0.28242210279169,-0.266043159182359,
-0.241558469125866,-0.237039116390008,-0.235040358720029,-0.23352162605094,
-0.231902338489127,-0.229362149280418,-0.221071728653136,-0.191152176746599,
-0.184506077462624,-0.177924993493206,-0.176265432678288,-0.175300949619573,
-0.174542341063625,-0.173480406966033,-0.171309490482136,-0.153930255700701,
-0.123336452654517,-0.119367343876605,-0.117441837365444,-0.11596426221111,
-0.114563975867067,-0.112187479462713,-0.105305352214359,-0.0944571800687469,
-0.0745045971603884,-0.0609820264330281,-0.0591776137768069,-0.0580936989468276,
-0.0572513334793649,-0.0562828133379011,-0.0545606323743867,-0.0462372018743076,
-0.0278881277266695,-0.00534326115204203,-0.00210175747461067,-0.000970090757637366,
-1.00000000580192E-6),.UNSPECIFIED.);
#1522=B_SPLINE_CURVE_WITH_KNOTS('',3,(#100588,#100589,#100590,#100591,#100592,
#100593,#100594,#100595,#100596,#100597,#100598,#100599,#100600,#100601,
#100602,#100603,#100604,#100605,#100606,#100607,#100608,#100609,#100610,
#100611,#100612,#100613,#100614,#100615,#100616,#100617,#100618,#100619,
#100620,#100621,#100622,#100623,#100624,#100625,#100626,#100627,#100628,
#100629,#100630,#100631,#100632,#100633,#100634,#100635,#100636,#100637,
#100638,#100639,#100640,#100641,#100642,#100643,#100644,#100645,#100646,
#100647,#100648,#100649,#100650,#100651,#100652,#100653,#100654,#100655,
#100656,#100657,#100658,#100659,#100660,#100661,#100662,#100663,#100664,
#100665,#100666,#100667,#100668,#100669,#100670,#100671,#100672,#100673,
#100674,#100675,#100676,#100677,#100678,#100679,#100680,#100681,#100682,
#100683,#100684,#100685,#100686,#100687,#100688,#100689,#100690,#100691,
#100692,#100693,#100694,#100695,#100696,#100697,#100698,#100699,#100700,
#100701,#100702,#100703,#100704,#100705,#100706,#100707,#100708,#100709,
#100710,#100711,#100712,#100713,#100714,#100715,#100716,#100717,#100718,
#100719,#100720,#100721,#100722,#100723,#100724,#100725,#100726,#100727,
#100728,#100729,#100730,#100731,#100732,#100733,#100734,#100735,#100736,
#100737,#100738,#100739,#100740,#100741,#100742,#100743,#100744,#100745,
#100746,#100747),.UNSPECIFIED.,.F.,.F.,(4,2,2,2,2,2,2,2,2,2,2,2,2,2,2,2,
2,2,2,2,2,2,2,2,2,2,2,2,2,2,2,2,2,2,2,2,2,2,2,2,2,2,2,2,2,2,2,2,2,2,2,2,
2,2,2,2,2,2,2,2,2,2,2,2,2,2,2,2,2,2,2,2,2,2,2,2,2,2,2,4),(-0.537529498082018,
-0.537417443195381,-0.530769639104979,-0.524200930478091,-0.522542122814459,
-0.521577650601132,-0.520818776390598,-0.519756092171006,-0.517582265426865,
-0.50011444027448,-0.469641508250662,-0.465573988730827,-0.463636024079067,
-0.462130624882595,-0.460467467889012,-0.457727992560687,-0.447311562620452,
-0.427263389015693,-0.408741168195958,-0.405809226986125,-0.40469651006346,
-0.403901147620284,-0.403035612886966,-0.401788214529537,-0.398546692768889,
-0.393691286558525,-0.377241993286614,-0.352854095919316,-0.34833188513093,
-0.346332255798364,-0.344813004064781,-0.343193295057419,-0.340652708371575,
-0.332363144269462,-0.302433377118387,-0.295785344982849,-0.289216411034999,
-0.287557546469063,-0.286593041171085,-0.28583414092853,-0.284771420254957,
-0.282597518939526,-0.2651290945308,-0.234655117241117,-0.230587458182983,
-0.228649427050693,-0.227143976213566,-0.225480762168664,-0.222741192870317,
-0.212324405654129,-0.192275544480842,-0.173752688076481,-0.17082064629093,
-0.169707891198068,-0.168912501471051,-0.168046937046673,-0.16679949589876,
-0.163557862941249,-0.158702290171232,-0.142252432620423,-0.117880397832208,
-0.113440807103225,-0.111586800903833,-0.110053412926676,-0.108547727747675,
-0.106475940296733,-0.104043687813602,-0.0997330197806514,-0.0899153030896199,
-0.0743955965550353,-0.0563009987160674,-0.0533569616062631,-0.0522426885144976,
-0.0514468975801223,-0.0505816833750096,-0.0493360448122893,-0.0461063072858154,
-0.0412746707953448,-0.024972170629327,-9.99999999806711E-7),
 .UNSPECIFIED.);
#1523=B_SPLINE_CURVE_WITH_KNOTS('',3,(#100748,#100749,#100750,#100751,#100752,
#100753,#100754,#100755,#100756,#100757,#100758,#100759,#100760,#100761,
#100762,#100763,#100764,#100765,#100766,#100767,#100768,#100769,#100770,
#100771,#100772,#100773,#100774,#100775,#100776,#100777,#100778,#100779,
#100780,#100781,#100782,#100783,#100784,#100785,#100786,#100787,#100788,
#100789,#100790,#100791,#100792,#100793,#100794,#100795,#100796,#100797,
#100798,#100799,#100800,#100801,#100802,#100803,#100804,#100805,#100806,
#100807,#100808,#100809,#100810,#100811,#100812,#100813,#100814,#100815,
#100816,#100817,#100818,#100819),.UNSPECIFIED.,.F.,.F.,(4,2,2,2,2,2,2,2,
2,2,2,2,2,2,2,2,2,2,2,2,2,2,2,2,2,2,2,2,2,2,2,2,2,2,2,4),(-3.17249563591246,
-3.16985267282884,-3.16781533109578,-3.16633184302089,-3.16490281197556,
-3.163297182562,-3.16081860207664,-3.15373960056998,-3.12036675469528,-3.10955754083093,
-3.10771851416671,-3.10672493238573,-3.10588587908643,-3.10482000713047,
-3.10311487383523,-3.09319993144343,-3.08390891414379,-3.06939590956882,
-3.05862925215487,-3.05404252045242,-3.05150353223612,-3.04928310547904,
-3.0477479089204,-3.04621511743451,-3.04436140389674,-3.03992050257416,
-3.01554427711876,-2.99909803353467,-2.99424384163313,-2.99100358669265,
-2.98975671792045,-2.98889157012816,-2.98809657536929,-2.98698439901021,
-2.98405388921461,-2.96801447478129),.UNSPECIFIED.);
#1524=B_SPLINE_CURVE_WITH_KNOTS('',3,(#100820,#100821,#100822,#100823,#100824,
#100825,#100826,#100827,#100828,#100829,#100830,#100831,#100832,#100833,
#100834,#100835,#100836,#100837,#100838,#100839,#100840,#100841,#100842,
#100843,#100844,#100845,#100846,#100847,#100848,#100849,#100850,#100851,
#100852,#100853,#100854,#100855,#100856,#100857,#100858,#100859,#100860,
#100861,#100862,#100863,#100864,#100865,#100866,#100867,#100868,#100869,
#100870,#100871,#100872,#100873,#100874,#100875,#100876,#100877,#100878,
#100879,#100880,#100881,#100882,#100883,#100884,#100885,#100886,#100887,
#100888,#100889,#100890,#100891,#100892,#100893,#100894,#100895,#100896,
#100897,#100898,#100899,#100900,#100901,#100902,#100903,#100904,#100905,
#100906,#100907,#100908,#100909,#100910,#100911,#100912,#100913,#100914,
#100915,#100916,#100917,#100918,#100919,#100920,#100921,#100922,#100923,
#100924,#100925,#100926,#100927,#100928,#100929,#100930,#100931,#100932,
#100933,#100934,#100935,#100936,#100937,#100938,#100939,#100940,#100941,
#100942,#100943,#100944,#100945,#100946,#100947,#100948,#100949,#100950,
#100951,#100952,#100953,#100954,#100955,#100956,#100957,#100958,#100959,
#100960,#100961,#100962,#100963,#100964,#100965,#100966,#100967,#100968,
#100969,#100970,#100971,#100972,#100973,#100974,#100975,#100976,#100977,
#100978,#100979,#100980,#100981,#100982,#100983,#100984,#100985,#100986,
#100987,#100988,#100989,#100990,#100991,#100992,#100993,#100994,#100995,
#100996,#100997,#100998,#100999,#101000,#101001,#101002,#101003,#101004,
#101005,#101006,#101007,#101008,#101009,#101010,#101011,#101012,#101013,
#101014,#101015,#101016,#101017,#101018,#101019,#101020,#101021,#101022,
#101023,#101024,#101025,#101026,#101027,#101028,#101029,#101030,#101031,
#101032,#101033,#101034,#101035,#101036,#101037,#101038,#101039),
 .UNSPECIFIED.,.F.,.F.,(4,2,2,2,2,2,2,2,2,2,2,2,2,2,2,2,2,2,2,2,2,2,2,2,
2,2,2,2,2,2,2,2,2,2,2,2,2,2,2,2,2,2,2,2,2,2,2,2,2,2,2,2,2,2,2,2,2,2,2,2,
2,2,2,2,2,2,2,2,2,2,2,2,2,2,2,2,2,2,2,2,2,2,2,2,2,2,2,2,2,2,2,2,2,2,2,2,
2,2,2,2,2,2,2,2,2,2,2,2,2,4),(-2.96750086879726,-2.96659381553983,-2.96566234470614,
-2.96397271119722,-2.9610817025472,-2.94935671779514,-2.94114237626293,
-2.92562380844789,-2.91095596322626,-2.90900636756406,-2.90798963910852,
-2.90715199860394,-2.90611398543103,-2.90412423733864,-2.88975693764299,
-2.88480095240155,-2.86754019977096,-2.85866994608347,-2.85271443192878,
-2.85046415054895,-2.8490623648705,-2.8475832178978,-2.84556578763806,-2.84112921401378,
-2.8166088453051,-2.80026584222002,-2.79542855840305,-2.79219684172702,
-2.7909514510463,-2.79008674710252,-2.78929170689931,-2.78817888307029,
-2.78524182367117,-2.76707832462089,-2.75143065220629,-2.74175846499277,
-2.73749195156003,-2.73409590434219,-2.73229234937941,-2.73081298269155,
-2.72906521035275,-2.72601743611279,-2.71227319673704,-2.68759061762133,
-2.67973481679985,-2.67665899579946,-2.67436976402665,-2.6732850808675,
-2.67245229921497,-2.67147586509102,-2.6697630765253,-2.66248541161207,
-2.63145086921952,-2.61912557406169,-2.61624679612206,-2.61455390465507,
-2.61305538734124,-2.61117201287294,-2.60821527221347,-2.58922747840533,
-2.56677171569434,-2.55829014517698,-2.55655950286485,-2.55558937762736,
-2.55474767326373,-2.55366722481265,-2.55187396304261,-2.5393966653032,
-2.50981136243578,-2.50110574645628,-2.49852337370193,-2.49689536759146,
-2.49538099081942,-2.49340600184759,-2.48901808423033,-2.46172759139055,
-2.44155559660842,-2.43938879777495,-2.43832796212388,-2.43756976992492,
-2.43660529723624,-2.43494465111538,-2.42834422747228,-2.42171496317697,
-2.39179468298425,-2.38354933231851,-2.3810146825189,-2.37939706004146,
-2.37787857863445,-2.3758782364563,-2.37134688577835,-2.34745426195576,
-2.33061921715309,-2.3257030358317,-2.32243226483154,-2.32118101744791,
-2.32031520016361,-2.31952149715098,-2.31841365449556,-2.31551489261125,
-2.29482873909818,-2.29315787154553,-2.26771780909957,-2.2643076116996,
-2.26250121043244,-2.26102185618847,-2.25927684515296,-2.25624086117816,
-2.24272104725783,-2.22568207937383),.UNSPECIFIED.);
#1525=B_SPLINE_CURVE_WITH_KNOTS('',3,(#101044,#101045,#101046,#101047,#101048,
#101049,#101050,#101051,#101052,#101053,#101054,#101055,#101056,#101057,
#101058,#101059,#101060,#101061,#101062,#101063,#101064,#101065,#101066,
#101067,#101068,#101069,#101070,#101071,#101072,#101073,#101074,#101075,
#101076,#101077,#101078,#101079,#101080,#101081,#101082,#101083,#101084,
#101085,#101086,#101087,#101088,#101089,#101090,#101091,#101092,#101093,
#101094,#101095,#101096,#101097,#101098,#101099,#101100,#101101,#101102,
#101103,#101104,#101105,#101106,#101107,#101108,#101109,#101110,#101111,
#101112,#101113,#101114,#101115,#101116,#101117,#101118,#101119,#101120,
#101121,#101122,#101123,#101124,#101125,#101126,#101127,#101128,#101129,
#101130,#101131,#101132,#101133,#101134,#101135,#101136,#101137,#101138,
#101139,#101140,#101141,#101142,#101143,#101144,#101145,#101146,#101147,
#101148,#101149,#101150,#101151,#101152,#101153,#101154,#101155,#101156,
#101157,#101158,#101159,#101160,#101161,#101162,#101163,#101164,#101165,
#101166,#101167,#101168,#101169,#101170,#101171,#101172,#101173,#101174,
#101175,#101176,#101177,#101178,#101179,#101180,#101181,#101182,#101183,
#101184,#101185,#101186,#101187,#101188,#101189,#101190,#101191,#101192,
#101193,#101194,#101195,#101196,#101197,#101198,#101199,#101200,#101201,
#101202,#101203,#101204,#101205,#101206,#101207,#101208,#101209,#101210,
#101211,#101212,#101213,#101214,#101215,#101216,#101217,#101218,#101219,
#101220,#101221,#101222,#101223,#101224,#101225,#101226,#101227,#101228,
#101229,#101230,#101231,#101232,#101233,#101234,#101235,#101236,#101237,
#101238,#101239,#101240,#101241,#101242,#101243,#101244,#101245,#101246,
#101247),.UNSPECIFIED.,.F.,.F.,(4,2,2,2,2,2,2,2,2,2,2,2,2,2,2,2,2,2,2,2,
2,2,2,2,2,2,2,2,2,2,2,2,2,2,2,2,2,2,2,2,2,2,2,2,2,2,2,2,2,2,2,2,2,2,2,2,
2,2,2,2,2,2,2,2,2,2,2,2,2,2,2,2,2,2,2,2,2,2,2,2,2,2,2,2,2,2,2,2,2,2,2,2,
2,2,2,2,2,2,2,2,2,4),(-1.27966587227297,-1.272229553693,-1.24231524967437,
-1.23566675406253,-1.22910608887625,-1.22744806857877,-1.22648383674135,
-1.22572501586584,-1.22466222995535,-1.22248756132775,-1.20498420611661,
-1.17456296225542,-1.17048969707102,-1.16855076009953,-1.1670453691952,
-1.1653829949818,-1.16264660018661,-1.15226526909598,-1.13233710476868,
-1.11365923393185,-1.11072765119195,-1.10961505462486,-1.10881977465045,
-1.10795432555878,-1.10670704385205,-1.10346578746735,-1.09861074663655,
-1.08216234110127,-1.05777793164239,-1.05325615177723,-1.05125671993242,
-1.04973762095168,-1.0481180774026,-1.04557775571645,-1.03728910733969,
-1.00736230565903,-1.0007149522592,-0.994146644174214,-0.992487944047101,
-0.991523535473559,-0.990764712032883,-0.989702099812687,-0.987528423598759,
-0.970061955180934,-0.939590808048614,-0.935523591644476,-0.9335857623448,
-0.932080464362188,-0.93041741520764,-0.927678108280225,-0.917262197845361,
-0.897214751229519,-0.878694582583011,-0.875762836113375,-0.874650193336952,
-0.873854883947281,-0.872989407010776,-0.871742092052779,-0.868500787591783,
-0.863645707359806,-0.84719752378669,-0.822811238550126,-0.818289329988472,
-0.816289834188434,-0.8147706838671,-0.813151082937947,-0.810610665694105,
-0.80232165367715,-0.772393885050031,-0.765746296522921,-0.759177801588982,
-0.757519047790598,-0.756554606878571,-0.755795757285973,-0.754733107525846,
-0.752559351221373,-0.735092089804921,-0.704620150260785,-0.700552762210098,
-0.698614860337424,-0.697109509968391,-0.695446406980943,-0.692707020752121,
-0.682290931473667,-0.662243417765353,-0.643721785187141,-0.640789939111242,
-0.639677258289613,-0.638881921650265,-0.63801641499628,-0.636769057104699,
-0.633527640490277,-0.628672391768234,-0.612223631952927,-0.587836526034994,
-0.583314461950113,-0.581314897488488,-0.579795695042388,-0.578176038582264,
-0.575635534320366,-0.567346239168023,-0.537529498082018),.UNSPECIFIED.);
#1526=B_SPLINE_CURVE_WITH_KNOTS('',3,(#101248,#101249,#101250,#101251,#101252,
#101253,#101254,#101255,#101256,#101257,#101258,#101259,#101260,#101261,
#101262,#101263,#101264,#101265,#101266,#101267,#101268,#101269,#101270,
#101271,#101272,#101273,#101274,#101275,#101276,#101277,#101278,#101279,
#101280,#101281,#101282,#101283,#101284,#101285,#101286,#101287,#101288,
#101289,#101290,#101291,#101292,#101293,#101294,#101295,#101296,#101297,
#101298,#101299,#101300,#101301,#101302,#101303,#101304,#101305,#101306,
#101307,#101308,#101309,#101310,#101311,#101312,#101313,#101314,#101315,
#101316,#101317,#101318,#101319,#101320,#101321,#101322,#101323,#101324,
#101325,#101326,#101327,#101328,#101329,#101330,#101331,#101332,#101333,
#101334,#101335,#101336,#101337,#101338,#101339,#101340,#101341,#101342,
#101343,#101344,#101345,#101346,#101347,#101348,#101349,#101350,#101351,
#101352,#101353,#101354,#101355,#101356,#101357,#101358,#101359,#101360,
#101361,#101362,#101363,#101364,#101365,#101366,#101367,#101368,#101369,
#101370,#101371,#101372,#101373,#101374,#101375,#101376,#101377,#101378,
#101379,#101380,#101381,#101382,#101383,#101384,#101385,#101386,#101387,
#101388,#101389,#101390,#101391,#101392,#101393,#101394,#101395,#101396,
#101397,#101398,#101399,#101400,#101401,#101402,#101403,#101404,#101405,
#101406,#101407,#101408,#101409,#101410,#101411,#101412,#101413,#101414,
#101415,#101416,#101417,#101418,#101419,#101420,#101421,#101422,#101423,
#101424,#101425,#101426,#101427,#101428,#101429,#101430,#101431,#101432,
#101433,#101434,#101435,#101436,#101437,#101438,#101439,#101440,#101441,
#101442,#101443,#101444,#101445,#101446,#101447,#101448,#101449,#101450,
#101451,#101452,#101453,#101454,#101455,#101456,#101457),.UNSPECIFIED.,
 .F.,.F.,(4,2,2,2,2,2,2,2,2,2,2,2,2,2,2,2,2,2,2,2,2,2,2,2,2,2,2,2,2,2,2,
2,2,2,2,2,2,2,2,2,2,2,2,2,2,2,2,2,2,2,2,2,2,2,2,2,2,2,2,2,2,2,2,2,2,2,2,
2,2,2,2,2,2,2,2,2,2,2,2,2,2,2,2,2,2,2,2,2,2,2,2,2,2,2,2,2,2,2,2,2,2,2,2,
2,4),(-2.22568207937383,-2.2178550763344,-2.20996050804542,-2.20687464687162,
-2.20457965742834,-2.20349392601551,-2.20265351964583,-2.20167489394261,
-2.19995227863786,-2.19253328554911,-2.16164218072051,-2.14933535492842,
-2.14645796637081,-2.14476546629631,-2.14326703600014,-2.14138342463555,
-2.13842562978174,-2.11934775938661,-2.09697329055344,-2.08850581083454,
-2.08677605707526,-2.08580617431666,-2.0849645132728,-2.08388390907997,
-2.08208995556594,-2.06959072642165,-2.03997372232598,-2.03131741890679,
-2.02874017120338,-2.02711337079791,-2.02559872209595,-2.02362138036714,
-2.01921972390955,-1.99213992946854,-1.97178308683545,-1.96961611262615,
-1.96855529545168,-1.96779715900002,-1.96683281557215,-1.96517251881195,
-1.95857516983299,-1.95194600075082,-1.92203219501182,-1.91378229384877,
-1.91124729777793,-1.90962968979649,-1.90811138723478,-1.90611152209622,
-1.90158231869837,-1.87759287000226,-1.85617778127242,-1.8527232992923,
-1.85144513645397,-1.85057399667539,-1.84978584670233,-1.84869924843294,
-1.84593752013967,-1.82224624669334,-1.79796419568912,-1.79454388347424,
-1.79273544702362,-1.79138724829403,-1.78969202299961,-1.78680208324825,
-1.77588587450665,-1.75216290144899,-1.73794614617645,-1.73507924074646,
-1.73389168897721,-1.73303758273514,-1.73211263980119,-1.73058687994514,
-1.72556001326817,-1.69217385932536,-1.67959524900537,-1.67670038753949,
-1.67500417649623,-1.67350644282145,-1.67162899982318,-1.6686912736257,
-1.65061933690581,-1.62736407286598,-1.61875222682429,-1.61701464193775,
-1.61604311267743,-1.61520180888352,-1.61412391797587,-1.61233907363577,
-1.60009429297636,-1.57082737804266,-1.56165770766578,-1.5590301860362,
-1.55739250652819,-1.55588183691212,-1.55392962898009,-1.54966692078736,
-1.5209293389813,-1.50209108184843,-1.49988146952484,-1.49881232445706,
-1.49797332885811,-1.49698292804261,-1.49520812729529,-1.48698281804791,
-1.48384928743498),.UNSPECIFIED.);
#1527=B_SPLINE_CURVE_WITH_KNOTS('',3,(#101462,#101463,#101464,#101465,#101466,
#101467,#101468,#101469,#101470,#101471,#101472,#101473,#101474,#101475,
#101476,#101477,#101478,#101479,#101480,#101481,#101482,#101483,#101484,
#101485,#101486,#101487,#101488,#101489,#101490,#101491,#101492,#101493,
#101494,#101495,#101496,#101497,#101498,#101499,#101500,#101501,#101502,
#101503,#101504,#101505,#101506,#101507,#101508,#101509,#101510,#101511,
#101512,#101513,#101514,#101515,#101516,#101517,#101518,#101519,#101520,
#101521,#101522,#101523,#101524,#101525,#101526,#101527,#101528,#101529,
#101530,#101531,#101532,#101533,#101534,#101535,#101536,#101537,#101538,
#101539,#101540,#101541,#101542,#101543,#101544,#101545,#101546,#101547,
#101548,#101549,#101550,#101551,#101552,#101553,#101554,#101555,#101556,
#101557,#101558,#101559,#101560,#101561,#101562,#101563,#101564,#101565,
#101566,#101567,#101568,#101569,#101570,#101571,#101572,#101573,#101574,
#101575,#101576,#101577,#101578,#101579,#101580,#101581,#101582,#101583,
#101584,#101585,#101586,#101587,#101588,#101589,#101590,#101591,#101592,
#101593,#101594,#101595,#101596,#101597,#101598,#101599,#101600,#101601,
#101602,#101603,#101604,#101605,#101606,#101607,#101608,#101609,#101610,
#101611,#101612,#101613,#101614,#101615,#101616,#101617,#101618,#101619,
#101620,#101621,#101622,#101623,#101624,#101625,#101626,#101627,#101628,
#101629,#101630,#101631,#101632,#101633,#101634,#101635,#101636,#101637,
#101638,#101639,#101640,#101641,#101642,#101643,#101644,#101645,#101646,
#101647,#101648,#101649,#101650,#101651,#101652,#101653,#101654,#101655,
#101656,#101657,#101658,#101659,#101660,#101661,#101662,#101663,#101664,
#101665,#101666,#101667,#101668,#101669,#101670,#101671,#101672,#101673,
#101674,#101675),.UNSPECIFIED.,.F.,.F.,(4,2,2,2,2,2,2,2,2,2,2,2,2,2,2,2,
2,2,2,2,2,2,2,2,2,2,2,2,2,2,2,2,2,2,2,2,2,2,2,2,2,2,2,2,2,2,2,2,2,2,2,2,
2,2,2,2,2,2,2,2,2,2,2,2,2,2,2,2,2,2,2,2,2,2,2,2,2,2,2,2,2,2,2,2,2,2,2,2,
2,2,2,2,2,2,2,2,2,2,2,2,2,2,2,2,2,2,4),(-2.02162775575412,-2.02147662782479,
-1.99579917719131,-1.99236999230877,-1.9905590974704,-1.98920999891803,
-1.98751485866348,-1.98462806222062,-1.97376679701779,-1.94689196501622,
-1.93427540470258,-1.9323753699355,-1.93136869038776,-1.93053022739403,
-1.92947974854527,-1.92782606531596,-1.91895789189624,-1.88946352597479,
-1.87734105365018,-1.87447490275668,-1.87278426784987,-1.87128457903486,
-1.86939548216155,-1.86642133576316,-1.84379852215493,-1.82744916164141,
-1.81670891442864,-1.81487219767349,-1.8138789560533,-1.81303964054625,
-1.81197273424283,-1.81026462778585,-1.80028619653179,-1.77708718181986,
-1.76179829786174,-1.75780489701819,-1.75588134780566,-1.75437796803572,
-1.75270764804842,-1.74993436713586,-1.73909076913937,-1.71748189494616,
-1.71667938370067,-1.69959312984664,-1.69758663409149,-1.69654469670994,
-1.69570654291272,-1.69469237137944,-1.69275654060829,-1.6787508954603,
-1.6565595797421,-1.64285580237271,-1.63980942276381,-1.63806149034949,
-1.63658142537093,-1.63477632006471,-1.63137519601336,-1.60436196535677,
-1.58351503169303,-1.58062033590652,-1.5795126105778,-1.57871865380714,
-1.57785214722016,-1.57659920134281,-1.57331993583358,-1.56838797398566,
-1.55145656216529,-1.52770656023906,-1.52317234659849,-1.52117081895816,
-1.51965145200251,-1.51803289495087,-1.51549678861445,-1.5072467059908,
-1.47729328112608,-1.47064976042364,-1.46406354056792,-1.46240341567264,
-1.46143871841482,-1.46068000451188,-1.45961798269716,-1.45744708249859,
-1.44007364837657,-1.40948450649961,-1.40543294077683,-1.40349816537977,
-1.40199332725761,-1.40032884344286,-1.39758266129586,-1.38708109250646,
-1.36673193862266,-1.34863137185491,-1.34568832245574,-1.34457429740133,
-1.34377865532294,-1.34291357043371,-1.34166806439913,-1.33843837295501,
-1.33360655304634,-1.31730071386141,-1.29272880313439,-1.28821225078702,
-1.28621377740751,-1.28469487836143,-1.28307503958348,-1.280533186487,-1.27966587227297),
 .UNSPECIFIED.);
#1528=B_SPLINE_CURVE_WITH_KNOTS('',3,(#101676,#101677,#101678,#101679,#101680,
#101681,#101682,#101683,#101684,#101685,#101686,#101687,#101688,#101689,
#101690,#101691,#101692,#101693,#101694,#101695,#101696,#101697,#101698,
#101699,#101700,#101701,#101702,#101703,#101704,#101705,#101706,#101707,
#101708,#101709,#101710,#101711,#101712,#101713,#101714,#101715,#101716,
#101717,#101718,#101719,#101720,#101721,#101722,#101723,#101724,#101725,
#101726,#101727,#101728,#101729,#101730,#101731,#101732,#101733,#101734,
#101735,#101736,#101737,#101738,#101739,#101740,#101741,#101742,#101743,
#101744,#101745,#101746,#101747,#101748,#101749,#101750,#101751,#101752,
#101753,#101754,#101755,#101756,#101757,#101758,#101759,#101760,#101761,
#101762,#101763,#101764,#101765,#101766,#101767,#101768,#101769,#101770,
#101771,#101772,#101773,#101774,#101775,#101776,#101777,#101778,#101779,
#101780,#101781,#101782,#101783,#101784,#101785,#101786,#101787,#101788,
#101789,#101790,#101791,#101792,#101793,#101794,#101795,#101796,#101797,
#101798,#101799,#101800,#101801,#101802,#101803,#101804,#101805,#101806,
#101807,#101808,#101809,#101810,#101811,#101812,#101813,#101814,#101815,
#101816,#101817,#101818,#101819,#101820,#101821,#101822,#101823,#101824,
#101825,#101826,#101827,#101828,#101829,#101830,#101831,#101832,#101833,
#101834,#101835,#101836,#101837,#101838,#101839,#101840,#101841,#101842,
#101843,#101844,#101845,#101846,#101847,#101848,#101849,#101850,#101851,
#101852,#101853,#101854,#101855,#101856,#101857,#101858,#101859,#101860,
#101861,#101862,#101863,#101864,#101865,#101866,#101867,#101868,#101869,
#101870,#101871,#101872,#101873,#101874,#101875,#101876,#101877,#101878,
#101879,#101880,#101881),.UNSPECIFIED.,.F.,.F.,(4,2,2,2,2,2,2,2,2,2,2,2,
2,2,2,2,2,2,2,2,2,2,2,2,2,2,2,2,2,2,2,2,2,2,2,2,2,2,2,2,2,2,2,2,2,2,2,2,
2,2,2,2,2,2,2,2,2,2,2,2,2,2,2,2,2,2,2,2,2,2,2,2,2,2,2,2,2,2,2,2,2,2,2,2,
2,2,2,2,2,2,2,2,2,2,2,2,2,2,2,2,2,2,4),(-1.48384928743498,-1.48371487514913,
-1.45992098907207,-1.45316751042258,-1.44435845282337,-1.44166795103817,
-1.44001642210639,-1.43850972897545,-1.4365533128346,-1.43238267017394,
-1.41570153769621,-1.39714765591542,-1.39052852106685,-1.38382530265048,
-1.38215634381116,-1.38119006452188,-1.38043231583846,-1.37937452679372,
-1.37722256323148,-1.3592887795006,-1.32937980589441,-1.32524768930559,
-1.32331947571404,-1.32181226388046,-1.32016304265725,-1.31748280202988,
-1.30774048718393,-1.28914981928658,-1.26836283430222,-1.26546756892906,
-1.26436028286843,-1.26356680453757,-1.26270102249211,-1.2614494843269,
-1.2581759739495,-1.25325457770005,-1.23638245168105,-1.21257079640948,
-1.20803988659005,-1.20603980200214,-1.20452153433703,-1.20290415785877,
-1.20036993480368,-1.19212659200106,-1.1621924355117,-1.15555392058275,
-1.14895623076907,-1.147295924445,-1.1463316061485,-1.14557349983231,-1.14451275228775,
-1.14234599394355,-1.12188557254686,-1.09494687991804,-1.09053795209298,
-1.08855934383968,-1.08704451734614,-1.08541830061073,-1.08284363912912,
-1.07421277475296,-1.04456084817699,-1.03204279963325,-1.03024818877804,
-1.02916739664843,-1.02832571679146,-1.02735594954993,-1.0256267447897,
-1.01716827935652,-0.994842791709283,-0.975732558151765,-0.972774618471869,
-0.970890933631439,-0.969392468262866,-0.967699953168219,-0.96482260489375,
-0.952518134542969,-0.921665753420448,-0.914186137862191,-0.912459226949321,
-0.911479589805214,-0.910639252803292,-0.909554839380846,-0.907266931489033,
-0.904193666742227,-0.896347999719222,-0.871702172569502,-0.857935787844761,
-0.854887079176965,-0.85313910364302,-0.851659758347692,-0.849856465839474,
-0.84646164810969,-0.821458411157971,-0.798454693664855,-0.795663099149229,
-0.794571323303341,-0.793781759808521,-0.79291180806615,-0.791640045586063,
-0.788230762433554,-0.783031897915181,-0.764315199738776,-0.742062386064265),
 .UNSPECIFIED.);
#1529=B_SPLINE_CURVE_WITH_KNOTS('',3,(#101886,#101887,#101888,#101889,#101890,
#101891,#101892,#101893,#101894,#101895,#101896,#101897,#101898,#101899,
#101900,#101901,#101902,#101903,#101904,#101905,#101906,#101907,#101908,
#101909,#101910,#101911,#101912,#101913,#101914,#101915,#101916,#101917,
#101918,#101919,#101920,#101921,#101922,#101923,#101924,#101925,#101926,
#101927,#101928,#101929,#101930,#101931,#101932,#101933,#101934,#101935,
#101936,#101937,#101938,#101939,#101940,#101941,#101942,#101943,#101944,
#101945,#101946,#101947,#101948,#101949,#101950,#101951,#101952,#101953,
#101954,#101955,#101956,#101957,#101958,#101959,#101960,#101961,#101962,
#101963,#101964,#101965,#101966,#101967,#101968,#101969,#101970,#101971,
#101972,#101973,#101974,#101975,#101976,#101977,#101978,#101979,#101980,
#101981,#101982,#101983,#101984,#101985,#101986,#101987,#101988,#101989,
#101990,#101991,#101992,#101993,#101994,#101995,#101996,#101997,#101998,
#101999,#102000,#102001,#102002,#102003,#102004,#102005,#102006,#102007,
#102008,#102009,#102010,#102011,#102012,#102013,#102014,#102015,#102016,
#102017,#102018,#102019,#102020,#102021,#102022,#102023,#102024,#102025,
#102026,#102027,#102028,#102029,#102030,#102031,#102032,#102033,#102034,
#102035,#102036,#102037,#102038,#102039,#102040,#102041,#102042,#102043,
#102044,#102045,#102046,#102047,#102048,#102049,#102050,#102051,#102052,
#102053,#102054,#102055,#102056,#102057,#102058,#102059,#102060,#102061,
#102062,#102063,#102064,#102065,#102066,#102067,#102068,#102069,#102070,
#102071,#102072,#102073,#102074,#102075,#102076,#102077,#102078,#102079,
#102080,#102081,#102082,#102083,#102084,#102085,#102086,#102087,#102088,
#102089,#102090,#102091,#102092,#102093,#102094,#102095,#102096,#102097,
#102098,#102099,#102100,#102101,#102102,#102103,#102104,#102105),
 .UNSPECIFIED.,.F.,.F.,(4,2,2,2,2,2,2,2,2,2,2,2,2,2,2,2,2,2,2,2,2,2,2,2,
2,2,2,2,2,2,2,2,2,2,2,2,2,2,2,2,2,2,2,2,2,2,2,2,2,2,2,2,2,2,2,2,2,2,2,2,
2,2,2,2,2,2,2,2,2,2,2,2,2,2,2,2,2,2,2,2,2,2,2,2,2,2,2,2,2,2,2,2,2,2,2,2,
2,2,2,2,2,2,2,2,2,2,2,2,2,4),(-2.76357650556602,-2.76333910123122,-2.75848438226922,
-2.7552437508587,-2.75399672052331,-2.7531314552273,-2.75233634816034,-2.75122400896148,
-2.74829302256299,-2.72990936421677,-2.70978783425493,-2.69935159453149,
-2.69661109385011,-2.69494802477304,-2.69344316032543,-2.69150652273189,
-2.68744420997499,-2.65692875403012,-2.63948578767287,-2.63731302871906,
-2.63625073083977,-2.63549208234201,-2.63452781436635,-2.6328692031118,
-2.62629883652042,-2.61966326564236,-2.58975804464378,-2.58147335285329,
-2.57893379777217,-2.57731462708841,-2.5757957953463,-2.57379659373902,
-2.56927483576058,-2.54488179704724,-2.52842665780175,-2.52357066505057,
-2.52032937925598,-2.51908222978033,-2.51821692474097,-2.51742181557619,
-2.51630951891588,-2.51337902209132,-2.49486851842749,-2.47484072004081,
-2.46443123965767,-2.46169288462138,-2.46003025727294,-2.4585252390341,
-2.45658762717991,-2.45252034902333,-2.42204219450288,-2.40456953800957,
-2.40239588673835,-2.40133339592048,-2.40057470858364,-2.39961052682485,
-2.39795235774239,-2.39138761855596,-2.38475079760956,-2.35485375792119,
-2.34655688386981,-2.34401599188356,-2.3423965025242,-2.34087774560954,
-2.33887918760444,-2.33436128514433,-2.30981819664569,-2.29347535034401,
-2.28863751470529,-2.28540522316763,-2.28415941353748,-2.2832943504381,
-2.28249891165476,-2.28138542392974,-2.27844569770715,-2.26032216225262,
-2.24001170065774,-2.22952147075715,-2.22677645841289,-2.22511234354426,
-2.22360761911942,-2.22167268271544,-2.21761964708966,-2.18702854666275,
-2.16964125581399,-2.16747000136533,-2.16640796618303,-2.16564931281343,
-2.16468477479765,-2.16302512669482,-2.1564430865538,-2.14980924478117,
-2.11988478137169,-2.11162305708371,-2.10908585485216,-2.10746713711236,
-2.10594799591339,-2.10394731470303,-2.09941748009255,-2.07537102088888,
-2.05865013439352,-2.05375136047925,-2.05048883559966,-2.04923844510154,
-2.04837247838587,-2.0475780312308,-2.04646833460141,-2.04355830397262,
-2.02328296612591,-2.02162775575412),.UNSPECIFIED.);
#1530=B_SPLINE_CURVE_WITH_KNOTS('',3,(#102106,#102107,#102108,#102109,#102110,
#102111,#102112,#102113,#102114,#102115,#102116,#102117,#102118,#102119,
#102120,#102121,#102122,#102123,#102124,#102125,#102126,#102127,#102128,
#102129,#102130,#102131,#102132,#102133,#102134,#102135,#102136,#102137,
#102138,#102139,#102140,#102141,#102142,#102143,#102144,#102145,#102146,
#102147,#102148,#102149,#102150,#102151,#102152,#102153,#102154,#102155,
#102156,#102157,#102158,#102159,#102160,#102161,#102162,#102163,#102164,
#102165,#102166,#102167,#102168,#102169,#102170,#102171,#102172,#102173,
#102174,#102175,#102176,#102177,#102178,#102179,#102180,#102181,#102182,
#102183,#102184,#102185,#102186,#102187,#102188,#102189,#102190,#102191,
#102192,#102193,#102194,#102195,#102196,#102197,#102198,#102199,#102200,
#102201,#102202,#102203,#102204,#102205,#102206,#102207,#102208,#102209,
#102210,#102211,#102212,#102213,#102214,#102215,#102216,#102217,#102218,
#102219,#102220,#102221,#102222,#102223,#102224,#102225,#102226,#102227,
#102228,#102229,#102230,#102231,#102232,#102233,#102234,#102235,#102236,
#102237,#102238,#102239,#102240,#102241,#102242,#102243,#102244,#102245,
#102246,#102247,#102248,#102249,#102250,#102251,#102252,#102253,#102254,
#102255,#102256,#102257,#102258,#102259,#102260,#102261,#102262,#102263,
#102264,#102265,#102266,#102267,#102268,#102269,#102270,#102271,#102272,
#102273,#102274,#102275,#102276,#102277,#102278,#102279,#102280,#102281,
#102282,#102283,#102284,#102285,#102286,#102287,#102288,#102289,#102290,
#102291,#102292,#102293,#102294,#102295,#102296,#102297,#102298,#102299,
#102300,#102301,#102302,#102303,#102304,#102305,#102306,#102307,#102308,
#102309,#102310,#102311,#102312,#102313,#102314,#102315,#102316,#102317),
 .UNSPECIFIED.,.F.,.F.,(4,2,2,2,2,2,2,2,2,2,2,2,2,2,2,2,2,2,2,2,2,2,2,2,
2,2,2,2,2,2,2,2,2,2,2,2,2,2,2,2,2,2,2,2,2,2,2,2,2,2,2,2,2,2,2,2,2,2,2,2,
2,2,2,2,2,2,2,2,2,2,2,2,2,2,2,2,2,2,2,2,2,2,2,2,2,2,2,2,2,2,2,2,2,2,2,2,
2,2,2,2,2,2,2,2,2,4),(-0.742062386064265,-0.74082383376707,-0.737869415397941,
-0.735986639034777,-0.734488050000979,-0.732794494203004,-0.729913149670426,
-0.717552972081476,-0.686257841443905,-0.679215895273211,-0.677520680049237,
-0.676548181575274,-0.675791032555118,-0.67474111797497,-0.672629736978213,
-0.669857428699497,-0.637223542329692,-0.623024817171694,-0.619953812077845,
-0.618200691867482,-0.616856440607815,-0.615114036658552,-0.612007516490281,
-0.595293529230479,-0.57053124605763,-0.561918932363373,-0.560278648945289,
-0.559232438360717,-0.558394418912458,-0.557384729251122,-0.555469375730979,
-0.542277148593382,-0.510745238808649,-0.504200542749606,-0.501792081941628,
-0.50036044778997,-0.498846718000441,-0.496842545239705,-0.492413052451229,
-0.486422502890039,-0.457038989206241,-0.444712997222777,-0.442924941834431,
-0.441845945351214,-0.441004302802943,-0.440032984615947,-0.438297228970429,
-0.429725133269381,-0.406720517678837,-0.38837707567522,-0.385432126285059,
-0.383552160700355,-0.382053758703231,-0.380358226481331,-0.377468095427148,
-0.364974867739976,-0.332504153034069,-0.326601134473886,-0.324983529793714,
-0.324038031820967,-0.323190646977257,-0.322047689270369,-0.319442850933044,
-0.307766043937616,-0.280185911257941,-0.270093871003887,-0.267264959762892,
-0.265582689793245,-0.264232092710329,-0.262403853495407,-0.258889455265981,
-0.235374619354801,-0.210929544415633,-0.208226356486813,-0.207153561441298,
-0.206368704155963,-0.205493153490716,-0.204194672154184,-0.200598482719977,
-0.195007704204448,-0.174508802421658,-0.153473193464271,-0.150494726168837,
-0.148604457188224,-0.147104848829453,-0.145415380194428,-0.142700409556506,
-0.132719799042709,-0.112848589275792,-0.0938092476952492,-0.0908709478082895,
-0.0897577058029344,-0.0889623967724351,-0.0880974265373271,-0.0868517016312246,
-0.0837240513991225,-0.0690248805669019,-0.0544089790042287,-0.0359591647858924,
-0.0330113274865467,-0.0311302678909457,-0.0296314706306193,-0.0279359999577877,
-0.0261731935859782,-0.0235150047612098,-9.99999999584666E-7),
 .UNSPECIFIED.);
#1531=B_SPLINE_CURVE_WITH_KNOTS('',3,(#102322,#102323,#102324,#102325,#102326,
#102327,#102328,#102329,#102330,#102331,#102332,#102333,#102334,#102335,
#102336,#102337,#102338,#102339,#102340,#102341,#102342,#102343,#102344,
#102345,#102346,#102347,#102348,#102349,#102350,#102351,#102352,#102353,
#102354,#102355,#102356,#102357,#102358,#102359,#102360,#102361,#102362,
#102363,#102364,#102365,#102366,#102367,#102368,#102369,#102370,#102371,
#102372,#102373,#102374,#102375,#102376,#102377,#102378,#102379,#102380,
#102381,#102382,#102383,#102384,#102385,#102386,#102387,#102388,#102389,
#102390,#102391,#102392,#102393,#102394,#102395,#102396,#102397,#102398,
#102399,#102400,#102401,#102402,#102403,#102404,#102405,#102406,#102407,
#102408,#102409,#102410,#102411,#102412,#102413,#102414,#102415,#102416,
#102417,#102418,#102419,#102420,#102421,#102422,#102423,#102424,#102425,
#102426,#102427,#102428,#102429,#102430,#102431,#102432,#102433,#102434,
#102435,#102436,#102437,#102438,#102439,#102440,#102441,#102442,#102443,
#102444,#102445,#102446,#102447,#102448,#102449,#102450,#102451,#102452,
#102453,#102454,#102455,#102456,#102457,#102458,#102459,#102460,#102461,
#102462,#102463,#102464,#102465,#102466,#102467,#102468,#102469,#102470,
#102471,#102472,#102473,#102474,#102475,#102476,#102477,#102478,#102479,
#102480,#102481,#102482,#102483,#102484,#102485,#102486,#102487,#102488,
#102489,#102490,#102491,#102492,#102493,#102494,#102495,#102496,#102497,
#102498,#102499,#102500,#102501,#102502,#102503,#102504,#102505,#102506,
#102507,#102508,#102509,#102510,#102511,#102512,#102513,#102514,#102515,
#102516,#102517,#102518,#102519,#102520,#102521,#102522,#102523,#102524,
#102525),.UNSPECIFIED.,.F.,.F.,(4,2,2,2,2,2,2,2,2,2,2,2,2,2,2,2,2,2,2,2,
2,2,2,2,2,2,2,2,2,2,2,2,2,2,2,2,2,2,2,2,2,2,2,2,2,2,2,2,2,2,2,2,2,2,2,2,
2,2,2,2,2,2,2,2,2,2,2,2,2,2,2,2,2,2,2,2,2,2,2,2,2,2,2,2,2,2,2,2,2,2,2,2,
2,2,2,2,2,2,2,2,2,4),(-3.5055211511763,-3.47946494400775,-3.46168294829212,
-3.45950078978816,-3.45843670135296,-3.45767791091164,-3.45671501789293,
-3.45506213297972,-3.4485584203116,-3.44191116699937,-3.41210875999234,
-3.40651548446923,-3.40359891009418,-3.40119027356962,-3.39960405615639,
-3.39815310481854,-3.39621654399659,-3.39215413455514,-3.3616441099215,
-3.34420039502125,-3.34202775143225,-3.34096552807006,-3.34020694015761,
-3.33924275928536,-3.33758431974529,-3.3310149222981,-3.32437981353755,
-3.2944777058399,-3.28619279835907,-3.2836533559628,-3.28203429697311,-3.28051559792107,
-3.27851661170238,-3.27399552031847,-3.24959614891806,-3.23314855281832,
-3.22829395934054,-3.22505343584816,-3.22380646340187,-3.22294124356671,
-3.22214618251995,-3.22103391331147,-3.21810315791383,-3.1997139511651,
-3.17959838154418,-3.16916410379622,-3.16642386739735,-3.16476091456905,
-3.16325612693956,-3.16131954843232,-3.15725721006259,-3.12674537660817,
-3.10930187620266,-3.10712919391382,-3.1060669459508,-3.10530833815878,
-3.10434412885242,-3.10268563353998,-3.09611592456874,-3.0894806631881,
-3.05957754451498,-3.05129269501063,-3.04875321432321,-3.04713411842615,
-3.04561537600109,-3.04361631992141,-3.03909501427405,-3.01469530255772,
-2.99824712789313,-2.99339238207356,-2.99015176071685,-2.98890475320324,
-2.9880395098748,-2.98724442791264,-2.98613213033272,-2.9832013075556,-2.96481051331061,
-2.94469521644095,-2.93426089143454,-2.93152060068324,-2.92985760749354,
-2.92835277859863,-2.92641614033669,-2.92235365161984,-2.8918413266534,
-2.87439710972965,-2.87222436213446,-2.87116208432121,-2.87040345605727,
-2.86943922188932,-2.86778068632549,-2.86121085106628,-2.85457540284204,
-2.82467156040574,-2.81638638663323,-2.8138468270709,-2.81222768545878,
-2.81070890335604,-2.80870979972494,-2.80418840712191,-2.77978670660156,
-2.76357650556602),.UNSPECIFIED.);
#1532=B_SPLINE_CURVE_WITH_KNOTS('',3,(#102526,#102527,#102528,#102529,#102530,
#102531,#102532,#102533,#102534,#102535,#102536,#102537,#102538,#102539,
#102540,#102541,#102542,#102543,#102544,#102545,#102546,#102547,#102548,
#102549,#102550,#102551,#102552,#102553,#102554,#102555,#102556,#102557,
#102558,#102559,#102560,#102561,#102562,#102563,#102564,#102565,#102566,
#102567,#102568,#102569,#102570,#102571,#102572,#102573,#102574,#102575,
#102576,#102577,#102578,#102579,#102580,#102581,#102582,#102583,#102584,
#102585,#102586,#102587,#102588,#102589,#102590,#102591,#102592,#102593,
#102594,#102595,#102596,#102597,#102598,#102599,#102600,#102601,#102602,
#102603,#102604,#102605,#102606,#102607,#102608,#102609,#102610,#102611,
#102612,#102613,#102614,#102615,#102616,#102617,#102618,#102619,#102620,
#102621,#102622,#102623,#102624,#102625,#102626,#102627,#102628,#102629,
#102630,#102631,#102632,#102633,#102634,#102635,#102636,#102637,#102638,
#102639,#102640,#102641,#102642,#102643,#102644,#102645,#102646,#102647,
#102648,#102649,#102650,#102651,#102652,#102653,#102654,#102655,#102656,
#102657,#102658,#102659,#102660,#102661,#102662,#102663,#102664,#102665,
#102666,#102667,#102668,#102669,#102670,#102671,#102672,#102673,#102674,
#102675,#102676,#102677,#102678,#102679,#102680,#102681,#102682,#102683,
#102684,#102685,#102686,#102687,#102688,#102689,#102690,#102691,#102692,
#102693,#102694,#102695,#102696,#102697,#102698,#102699,#102700,#102701,
#102702,#102703,#102704,#102705,#102706,#102707,#102708,#102709,#102710,
#102711,#102712,#102713,#102714,#102715,#102716,#102717,#102718,#102719,
#102720,#102721,#102722,#102723,#102724,#102725,#102726,#102727,#102728,
#102729,#102730,#102731,#102732,#102733,#102734,#102735),.UNSPECIFIED.,
 .F.,.F.,(4,2,2,2,2,2,2,2,2,2,2,2,2,2,2,2,2,2,2,2,2,2,2,2,2,2,2,2,2,2,2,
2,2,2,2,2,2,2,2,2,2,2,2,2,2,2,2,2,2,2,2,2,2,2,2,2,2,2,2,2,2,2,2,2,2,2,2,
2,2,2,2,2,2,2,2,2,2,2,2,2,2,2,2,2,2,2,2,2,2,2,2,2,2,2,2,2,2,2,2,2,2,2,2,
2,4),(-1.48409509776007,-1.46365215592803,-1.45894857869465,-1.45752538571778,
-1.45627895076673,-1.45541393438915,-1.45461893789389,-1.45350661279528,
-1.45057452074908,-1.43256199634338,-1.41883674487716,-1.40287855432187,
-1.39953011832661,-1.3976885277089,-1.3961930247133,-1.39447035172652,-1.39153381016838,
-1.37951746797466,-1.35060641309532,-1.34119379256165,-1.33942833022474,
-1.33842056381484,-1.33758235370359,-1.33653366860193,-1.33488549223496,
-1.32612181995249,-1.29652178425105,-1.28438393670057,-1.28151713778624,
-1.27982659839912,-1.2783272933426,-1.2764390878579,-1.27346717177484,-1.25290435787762,
-1.23198666126393,-1.22355262278279,-1.22182432778564,-1.22085456877064,
-1.22001256081625,-1.21893093617151,-1.2171341083745,-1.20456891381828,
-1.17484723907971,-1.16632122444403,-1.16375674113247,-1.16213237408773,
-1.16061610126748,-1.15863103527661,-1.15418811222316,-1.12778174831265,
-1.10678708944923,-1.1046251806104,-1.10356516056424,-1.10280690625202,
-1.10184146901521,-1.10017723391488,-1.09353676262251,-1.06185144505965,
-1.04944696007946,-1.04656256101016,-1.04486822415544,-1.04336955914616,
-1.0414875072937,-1.03853581018435,-1.01988347242787,-0.997127035032357,
-0.988594396712029,-0.98686066710911,-0.985889748373163,-0.985047966850505,
-0.983968191967646,-0.98217762928574,-0.969782957786556,-0.940313378555806,
-0.931429311382468,-0.928828797385757,-0.927196613440196,-0.925683306009111,
-0.923716769363117,-0.919538735147668,-0.890475169719944,-0.87726591875141,
-0.872984620645554,-0.870035223591483,-0.868833926873195,-0.867977244406281,
-0.867170964719169,-0.865780332654773,-0.861830798468349,-0.837761487244635,
-0.81552611735145,-0.812055823235516,-0.810236723668568,-0.808887143737685,
-0.807198728495439,-0.804341414157621,-0.793856607299055,-0.766627498662389,
-0.755013942443657,-0.752416297666676,-0.751274643637468,-0.750427480885756,
-0.749481395373951,-0.747861013757768,-0.742040097680754),.UNSPECIFIED.);
#1533=B_SPLINE_CURVE_WITH_KNOTS('',3,(#102740,#102741,#102742,#102743,#102744,
#102745,#102746,#102747,#102748,#102749,#102750,#102751,#102752,#102753,
#102754,#102755,#102756,#102757,#102758,#102759,#102760,#102761,#102762,
#102763,#102764,#102765,#102766,#102767,#102768,#102769,#102770,#102771,
#102772,#102773,#102774,#102775,#102776,#102777,#102778,#102779,#102780,
#102781,#102782,#102783,#102784,#102785,#102786,#102787,#102788,#102789,
#102790,#102791,#102792,#102793,#102794,#102795,#102796,#102797,#102798,
#102799,#102800,#102801,#102802,#102803,#102804,#102805,#102806,#102807,
#102808,#102809,#102810,#102811,#102812,#102813,#102814,#102815,#102816,
#102817,#102818,#102819,#102820,#102821,#102822,#102823,#102824,#102825,
#102826,#102827,#102828,#102829,#102830,#102831,#102832,#102833,#102834,
#102835,#102836,#102837,#102838,#102839,#102840,#102841,#102842,#102843,
#102844,#102845,#102846,#102847,#102848,#102849,#102850,#102851,#102852,
#102853,#102854,#102855,#102856,#102857,#102858,#102859,#102860,#102861,
#102862,#102863,#102864,#102865,#102866,#102867,#102868,#102869,#102870,
#102871,#102872,#102873,#102874,#102875,#102876,#102877,#102878,#102879,
#102880,#102881,#102882,#102883,#102884,#102885,#102886,#102887,#102888,
#102889,#102890,#102891,#102892,#102893,#102894,#102895,#102896,#102897,
#102898,#102899,#102900,#102901,#102902,#102903,#102904,#102905,#102906,
#102907,#102908,#102909,#102910,#102911,#102912,#102913,#102914,#102915,
#102916,#102917,#102918,#102919,#102920,#102921,#102922,#102923,#102924,
#102925,#102926,#102927,#102928,#102929,#102930,#102931,#102932,#102933,
#102934,#102935,#102936,#102937,#102938,#102939,#102940,#102941,#102942,
#102943,#102944,#102945,#102946,#102947,#102948,#102949,#102950,#102951,
#102952,#102953,#102954,#102955,#102956,#102957,#102958,#102959,#102960,
#102961),.UNSPECIFIED.,.F.,.F.,(4,2,2,2,2,2,2,2,2,2,2,2,2,2,2,2,2,2,2,2,
2,2,2,2,2,2,2,2,2,2,2,2,2,2,2,2,2,2,2,2,2,2,2,2,2,2,2,2,2,2,2,2,2,2,2,2,
2,2,2,2,2,2,2,2,2,2,2,2,2,2,2,2,2,2,2,2,2,2,2,2,2,2,2,2,2,2,2,2,2,2,2,2,
2,2,2,2,2,2,2,2,2,2,2,2,2,2,2,2,2,2,4),(-0.742107893903836,-0.723841853319381,
-0.719320036308527,-0.717320605986864,-0.715801515165782,-0.714181987051595,
-0.711641703722723,-0.703353312568062,-0.673426557298028,-0.666779265901727,
-0.660210904579521,-0.658552207345801,-0.657587803307021,-0.656828985198745,
-0.655766382744891,-0.653592734810197,-0.6361268694326,-0.605655289172278,
-0.60158818045023,-0.599650379294435,-0.598145093141986,-0.596482046885033,
-0.593742721155086,-0.583326430438049,-0.563277553853061,-0.544759596113452,
-0.541827866611508,-0.540715230880491,-0.539919926661509,-0.539054455534638,
-0.537807149207063,-0.534565868582421,-0.529710825252761,-0.513262779752363,
-0.488876618375661,-0.48435474083186,-0.482355258491555,-0.480836118297064,
-0.479216528068968,-0.476676127410474,-0.468387167662968,-0.438459600605826,
-0.431812056268836,-0.425243604475989,-0.423584861666512,-0.422620427161542,
-0.421861582615796,-0.420798939934875,-0.418625198170893,-0.40115805633814,
-0.370686314148645,-0.366618953700012,-0.364681064807605,-0.363175724447664,
-0.361512632443314,-0.358773264132004,-0.348357240711471,-0.328309848599026,
-0.309788354462662,-0.30685652783641,-0.30574385439837,-0.304948523037442,
-0.304083022125781,-0.302835672510451,-0.299594277407143,-0.294739060908434,
-0.278290410270541,-0.253903466263959,-0.249381432188862,-0.247381880993904,
-0.245862688625974,-0.244243042909015,-0.241702555495137,-0.233413315282159,
-0.203484717640983,-0.196836945248695,-0.190268268346267,-0.188609468631586,
-0.187645001029137,-0.186886130441864,-0.185823451288419,-0.183649634873507,
-0.166181891192656,-0.135709237451958,-0.131641652756981,-0.129703681301153,
-0.128251772401547,-0.128203928614175,-0.128147838639546,-0.126508698259215,
-0.12379643660391,-0.120540364508337,-0.113995975198164,-0.0949246555972127,
-0.0747877879742402,-0.0718720333933413,-0.0707613980199954,-0.0699665879501811,
-0.0691005743740268,-0.0678506997401898,-0.064592748913196,-0.0597041994055956,
-0.043048780056191,-0.0253408062907407,-0.0160132388697642,-0.0132661212629756,
-0.0116012437553241,-0.0101423569917107,-0.00868747148028448,-0.00682528125065143,
-9.99999999806711E-7),.UNSPECIFIED.);
#1534=B_SPLINE_CURVE_WITH_KNOTS('',3,(#102962,#102963,#102964,#102965,#102966,
#102967,#102968,#102969,#102970,#102971,#102972,#102973,#102974,#102975,
#102976,#102977,#102978,#102979,#102980,#102981,#102982,#102983,#102984,
#102985,#102986,#102987,#102988,#102989,#102990,#102991,#102992,#102993,
#102994,#102995,#102996,#102997,#102998,#102999,#103000,#103001,#103002,
#103003,#103004,#103005,#103006,#103007,#103008,#103009,#103010,#103011,
#103012,#103013,#103014,#103015,#103016,#103017,#103018,#103019,#103020,
#103021,#103022,#103023,#103024,#103025,#103026,#103027,#103028,#103029,
#103030,#103031,#103032,#103033,#103034,#103035,#103036,#103037,#103038,
#103039,#103040,#103041,#103042,#103043,#103044,#103045,#103046,#103047,
#103048,#103049,#103050,#103051,#103052,#103053,#103054,#103055,#103056,
#103057,#103058,#103059,#103060,#103061,#103062,#103063,#103064,#103065,
#103066,#103067,#103068,#103069,#103070,#103071,#103072,#103073,#103074,
#103075,#103076,#103077,#103078,#103079,#103080,#103081,#103082,#103083,
#103084,#103085,#103086,#103087,#103088,#103089,#103090,#103091,#103092,
#103093,#103094,#103095,#103096,#103097,#103098,#103099,#103100,#103101,
#103102,#103103,#103104,#103105,#103106,#103107,#103108,#103109,#103110,
#103111,#103112,#103113,#103114,#103115,#103116,#103117,#103118,#103119,
#103120,#103121,#103122,#103123,#103124,#103125,#103126,#103127,#103128,
#103129,#103130,#103131,#103132,#103133,#103134,#103135,#103136,#103137,
#103138,#103139,#103140,#103141,#103142,#103143,#103144,#103145,#103146,
#103147,#103148,#103149,#103150,#103151,#103152,#103153,#103154,#103155,
#103156,#103157,#103158,#103159,#103160,#103161,#103162,#103163,#103164,
#103165,#103166,#103167,#103168,#103169,#103170,#103171,#103172,#103173),
 .UNSPECIFIED.,.F.,.F.,(4,2,2,2,2,2,2,2,2,2,2,2,2,2,2,2,2,2,2,2,2,2,2,2,
2,2,2,2,2,2,2,2,2,2,2,2,2,2,2,2,2,2,2,2,2,2,2,2,2,2,2,2,2,2,2,2,2,2,2,2,
2,2,2,2,2,2,2,2,2,2,2,2,2,2,2,2,2,2,2,2,2,2,2,2,2,2,2,2,2,2,2,2,2,2,2,2,
2,2,2,2,2,2,2,2,2,4),(-0.742040097680754,-0.741928316738839,-0.729948429837609,
-0.700581075524223,-0.695542425395112,-0.693588135535638,-0.692169801554734,
-0.690648408539036,-0.688596297768509,-0.683895735696293,-0.677424338593979,
-0.658727895265965,-0.638074744638377,-0.635172542237828,-0.63406406152576,
-0.633270081316746,-0.632404161444009,-0.631153103407226,-0.627884682699124,
-0.622974225453668,-0.606176516502152,-0.582251276802361,-0.577720447887504,
-0.575719928478674,-0.574201147600775,-0.5725830485224,-0.570047324567895,
-0.561795679259194,-0.531854350531205,-0.525212905936097,-0.51861528004425,
-0.516954566125179,-0.51598993750859,-0.515231541389359,-0.514170328867937,
-0.512002407706218,-0.491353088467344,-0.464604519631965,-0.460181830168216,
-0.458200327983258,-0.45668459289826,-0.455058675157748,-0.452487210289166,
-0.443893904333654,-0.414201910572,-0.401660160644848,-0.399864180153527,
-0.398782780440167,-0.397940764362255,-0.396970769803733,-0.39524153842414,
-0.386790997580685,-0.364522495549996,-0.345329501187251,-0.342369487243714,
-0.340484806069431,-0.338985753835874,-0.337292794647745,-0.3344152314195,
-0.322119157400736,-0.291358202151315,-0.283771358635228,-0.282036716586524,
-0.281055102043267,-0.280214654522631,-0.279132152861841,-0.276855449423359,
-0.273801868303748,-0.266032681782011,-0.241804682236309,-0.227533902419892,
-0.224458636483646,-0.222704262133171,-0.221359663091233,-0.21961753888327,
-0.216513699605243,-0.199883958266859,-0.185584512826758,-0.176072632947613,
-0.166514301380018,-0.164825063537784,-0.163763899908974,-0.162925019634224,
-0.161927473862387,-0.160070265809172,-0.148775665594381,-0.124625080137313,
-0.110094233000793,-0.107281026250031,-0.105440969704503,-0.104040431693504,
-0.102412525399209,-0.0996952500842602,-0.0964155471588903,-0.0898023748472433,
-0.0703637819504087,-0.0507249973331295,-0.0478029150002421,-0.046691706948221,
-0.0458969147070438,-0.0450314269784657,-0.0437831729049783,-0.040534304718124,
-0.0356636560514601,-0.0191176910841187,-6.62583249990897E-6),
 .UNSPECIFIED.);
#1535=B_SPLINE_CURVE_WITH_KNOTS('',3,(#103178,#103179,#103180,#103181,#103182,
#103183,#103184,#103185,#103186,#103187,#103188,#103189,#103190,#103191,
#103192,#103193,#103194,#103195,#103196,#103197,#103198,#103199,#103200,
#103201,#103202,#103203,#103204,#103205,#103206,#103207,#103208,#103209,
#103210,#103211,#103212,#103213,#103214,#103215,#103216,#103217,#103218,
#103219,#103220,#103221,#103222,#103223,#103224,#103225,#103226,#103227,
#103228,#103229,#103230,#103231,#103232,#103233,#103234,#103235,#103236,
#103237,#103238,#103239,#103240,#103241,#103242,#103243,#103244,#103245,
#103246,#103247,#103248,#103249,#103250,#103251,#103252,#103253,#103254,
#103255,#103256,#103257,#103258,#103259,#103260,#103261,#103262,#103263,
#103264,#103265,#103266,#103267,#103268,#103269,#103270,#103271,#103272,
#103273,#103274,#103275,#103276,#103277,#103278,#103279,#103280,#103281,
#103282,#103283,#103284,#103285,#103286,#103287,#103288,#103289,#103290,
#103291,#103292,#103293,#103294,#103295,#103296,#103297,#103298,#103299,
#103300,#103301,#103302,#103303,#103304,#103305,#103306,#103307,#103308,
#103309,#103310,#103311,#103312,#103313,#103314,#103315,#103316,#103317,
#103318,#103319,#103320,#103321,#103322,#103323,#103324,#103325,#103326,
#103327,#103328,#103329,#103330,#103331,#103332,#103333,#103334,#103335,
#103336,#103337,#103338,#103339,#103340,#103341,#103342,#103343,#103344,
#103345,#103346,#103347,#103348,#103349,#103350,#103351,#103352,#103353,
#103354,#103355,#103356,#103357,#103358,#103359,#103360,#103361,#103362,
#103363,#103364,#103365,#103366,#103367,#103368,#103369,#103370,#103371,
#103372,#103373,#103374,#103375,#103376,#103377,#103378,#103379,#103380,
#103381,#103382,#103383,#103384,#103385,#103386,#103387,#103388,#103389,
#103390,#103391,#103392,#103393,#103394,#103395,#103396,#103397),
 .UNSPECIFIED.,.F.,.F.,(4,2,2,2,2,2,2,2,2,2,2,2,2,2,2,2,2,2,2,2,2,2,2,2,
2,2,2,2,2,2,2,2,2,2,2,2,2,2,2,2,2,2,2,2,2,2,2,2,2,2,2,2,2,2,2,2,2,2,2,2,
2,2,2,2,2,2,2,2,2,2,2,2,2,2,2,2,2,2,2,2,2,2,2,2,2,2,2,2,2,2,2,2,2,2,2,2,
2,2,2,2,2,2,2,2,2,2,2,2,2,4),(-1.48414558948818,-1.48411908994632,-1.48150694578538,
-1.48044544243452,-1.47958552297644,-1.478687693243,-1.477286240022,-1.47288123924991,
-1.46545376461459,-1.44928763031837,-1.42678032231691,-1.42380983174383,
-1.42192176081098,-1.42042207910756,-1.41873059608615,-1.4158609083301,
-1.40368904567457,-1.37386147878574,-1.3653189318069,-1.36368181590189,
-1.36263632346925,-1.36179795944122,-1.36078672343039,-1.35886530984397,
-1.34546393699799,-1.31210485620013,-1.30705775011344,-1.30510175249705,
-1.30368266115583,-1.30216090244843,-1.30010907506394,-1.29541258046905,
-1.28894903780427,-1.27029529868479,-1.2495831918066,-1.24668327816823,
-1.24557485436457,-1.24478071493853,-1.24391437837728,-1.24266228879128,
-1.2393887133285,-1.23446826986368,-1.21760979406714,-1.19376563663291,
-1.18923292319908,-1.18723166497245,-1.18571234965949,-1.18409370081681,
-1.18155714295618,-1.17330273714836,-1.14335281151292,-1.13670895393039,
-1.13012479415659,-1.12846484816156,-1.12750019564856,-1.12674147986364,
-1.12567940743781,-1.12350823216857,-1.10612488555948,-1.0755490087322,
-1.07149577540665,-1.06956068926336,-1.06805582044201,-1.0663915171053,
-1.06364613118333,-1.05315421443957,-1.0328391108324,-1.01469014356287,
-1.01174971615821,-1.0106360266862,-1.00984047645838,-1.00897532116534,
-1.00772943320862,-1.00449719442477,-0.999660242143345,-0.983322816758281,
-0.958793151854156,-0.954275439396426,-0.95227676856374,-0.950757842765568,
-0.949138094133479,-0.946596631904352,-0.938296609111291,-0.908379775618584,
-0.901731632282564,-0.895169287913151,-0.893511132114086,-0.892546871951334,
-0.89178806043779,-0.890725328663062,-0.888550917911768,-0.871056320912156,
-0.840623953302691,-0.836552135988929,-0.83461347987711,-0.833108130388723,
-0.831445622960339,-0.828708594653004,-0.818319460672918,-0.798364245401951,
-0.779722517813475,-0.776791111962173,-0.775678541907763,-0.774883271670317,
-0.77401782250983,-0.77277052317967,-0.769529123387601,-0.764673784720258,
-0.748223465298814,-0.742107893903836),.UNSPECIFIED.);
#1536=B_SPLINE_CURVE_WITH_KNOTS('',3,(#103399,#103400,#103401,#103402),
 .UNSPECIFIED.,.F.,.F.,(4,4),(-6.62583249990897E-6,-1.00000009449833E-6),
 .UNSPECIFIED.);
#1537=B_SPLINE_CURVE_WITH_KNOTS('',3,(#103403,#103404,#103405,#103406,#103407,
#103408,#103409,#103410,#103411,#103412,#103413,#103414,#103415,#103416,
#103417,#103418,#103419,#103420,#103421,#103422,#103423,#103424,#103425,
#103426,#103427,#103428,#103429,#103430,#103431,#103432,#103433,#103434,
#103435,#103436,#103437,#103438,#103439,#103440,#103441,#103442,#103443,
#103444,#103445,#103446,#103447,#103448,#103449,#103450,#103451,#103452,
#103453,#103454,#103455,#103456,#103457,#103458,#103459,#103460,#103461,
#103462,#103463,#103464,#103465,#103466,#103467,#103468,#103469,#103470,
#103471,#103472,#103473,#103474,#103475,#103476,#103477,#103478,#103479,
#103480,#103481,#103482,#103483,#103484,#103485,#103486,#103487,#103488,
#103489,#103490,#103491,#103492,#103493,#103494,#103495,#103496,#103497,
#103498,#103499,#103500,#103501,#103502,#103503,#103504,#103505,#103506,
#103507,#103508,#103509,#103510,#103511,#103512,#103513,#103514,#103515,
#103516,#103517,#103518,#103519,#103520,#103521,#103522,#103523,#103524,
#103525,#103526,#103527,#103528,#103529,#103530,#103531,#103532,#103533,
#103534,#103535,#103536,#103537,#103538,#103539,#103540,#103541,#103542,
#103543,#103544,#103545,#103546,#103547,#103548,#103549,#103550,#103551,
#103552,#103553,#103554,#103555,#103556,#103557,#103558,#103559,#103560,
#103561,#103562,#103563,#103564,#103565,#103566,#103567,#103568,#103569,
#103570,#103571,#103572,#103573,#103574,#103575,#103576,#103577,#103578,
#103579,#103580,#103581,#103582,#103583,#103584,#103585,#103586,#103587,
#103588,#103589,#103590,#103591,#103592,#103593,#103594,#103595,#103596,
#103597,#103598,#103599,#103600,#103601,#103602,#103603,#103604,#103605,
#103606,#103607,#103608,#103609,#103610,#103611,#103612,#103613,#103614,
#103615,#103616,#103617,#103618,#103619,#103620,#103621,#103622,#103623,
#103624,#103625,#103626,#103627,#103628,#103629,#103630,#103631,#103632),
 .UNSPECIFIED.,.F.,.F.,(4,2,2,2,2,2,2,2,2,2,2,2,2,2,2,2,2,2,2,2,2,2,2,2,
2,2,2,2,2,2,2,2,2,2,2,2,2,2,2,2,2,2,2,2,2,2,2,2,2,2,2,2,2,2,2,2,2,2,2,2,
2,2,2,2,2,2,2,2,2,2,2,2,2,2,2,2,2,2,2,2,2,2,2,2,2,2,2,2,2,2,2,2,2,2,2,2,
2,2,2,2,2,2,2,2,2,2,2,2,2,2,2,2,2,2,4),(-2.76158278095296,-2.75605222062093,
-2.75252015463855,-2.75079750115922,-2.74938169103857,-2.74803293709578,
-2.74629352434649,-2.74328139975011,-2.73297222047276,-2.71802590952989,
-2.69561194251482,-2.69209097871679,-2.69080345453194,-2.68993048996875,
-2.68914422690617,-2.68806476187476,-2.68534507673053,-2.66099649518445,
-2.64765672528628,-2.64012478440832,-2.63653375879653,-2.63359968647192,
-2.63191263100535,-2.631881954027,-2.63184891654279,-2.63182858787095,-2.63179966169494,
-2.63175858330605,-2.63155936297703,-2.63004121488427,-2.62804158696779,
-2.62351306993557,-2.59898048444021,-2.58265345838236,-2.57781924489417,
-2.57458923269347,-2.57334426326127,-2.57247977536507,-2.57168487243578,
-2.57057215958468,-2.56763471362048,-2.54949610867631,-2.52920504772647,
-2.5187222996957,-2.51597909259466,-2.51431607421643,-2.51281234893167,
-2.51087871563253,-2.50682852114621,-2.47623740466852,-2.45886160444114,
-2.45669169014394,-2.45563033614326,-2.45487218354769,-2.45390832337159,
-2.45224995217782,-2.44567474974773,-2.43904205359092,-2.40916410391459,
-2.40086988661454,-2.39833029435195,-2.39671176261504,-2.39519400028436,
-2.39319689975507,-2.38868300291224,-2.36406870900622,-2.34778774315513,
-2.34296097751151,-2.33973464471188,-2.33849021145206,-2.33762580945154,
-2.33683075563647,-2.33571752716908,-2.33277616773452,-2.31470907729038,
-2.29436699833418,-2.28386969787479,-2.28112525357769,-2.27946193434801,
-2.27795822519108,-2.27602501577698,-2.27197721992066,-2.24136580158916,
-2.22400435763817,-2.22183480883172,-2.22077350916209,-2.22001534463373,
-2.21905139963574,-2.2173927317497,-2.21081435814262,-2.20418202568458,
-2.17429857455624,-2.16601031918294,-2.1634713120305,-2.16185287700644,
-2.16033501195311,-2.15833749419332,-2.15382141296355,-2.12927870184117,
-2.10835426015475,-2.10493382807543,-2.10366060532023,-2.10279048910964,
-2.10200142775615,-2.1009111982557,-2.09812796403039,-2.07499799568581,
-2.05039910537378,-2.04685190209,-2.04501740115274,-2.0436665820278,-2.04198967101139,
-2.03918329369144,-2.02921902657818,-2.01986711404084),.UNSPECIFIED.);
#1538=B_SPLINE_CURVE_WITH_KNOTS('',3,(#103637,#103638,#103639,#103640,#103641,
#103642,#103643,#103644,#103645,#103646,#103647,#103648,#103649,#103650,
#103651,#103652,#103653,#103654,#103655,#103656,#103657,#103658,#103659,
#103660,#103661,#103662,#103663,#103664,#103665,#103666,#103667,#103668,
#103669,#103670,#103671,#103672,#103673,#103674,#103675,#103676,#103677,
#103678,#103679,#103680,#103681,#103682,#103683,#103684,#103685,#103686,
#103687,#103688,#103689,#103690,#103691,#103692,#103693,#103694,#103695,
#103696,#103697,#103698,#103699,#103700,#103701,#103702,#103703,#103704,
#103705,#103706,#103707,#103708,#103709,#103710,#103711,#103712,#103713,
#103714,#103715,#103716,#103717,#103718,#103719,#103720,#103721,#103722,
#103723,#103724,#103725,#103726,#103727,#103728,#103729,#103730,#103731,
#103732,#103733,#103734,#103735,#103736,#103737,#103738,#103739,#103740,
#103741,#103742,#103743,#103744,#103745,#103746,#103747,#103748,#103749,
#103750,#103751,#103752,#103753,#103754,#103755,#103756,#103757,#103758,
#103759,#103760,#103761,#103762,#103763,#103764,#103765,#103766,#103767,
#103768,#103769,#103770,#103771,#103772,#103773,#103774,#103775,#103776,
#103777,#103778,#103779,#103780,#103781,#103782,#103783,#103784,#103785,
#103786,#103787,#103788,#103789,#103790,#103791,#103792,#103793,#103794,
#103795,#103796,#103797,#103798,#103799,#103800,#103801,#103802,#103803,
#103804,#103805,#103806,#103807,#103808,#103809,#103810,#103811,#103812,
#103813,#103814,#103815,#103816,#103817,#103818,#103819,#103820,#103821,
#103822,#103823,#103824,#103825,#103826,#103827,#103828,#103829,#103830,
#103831,#103832,#103833,#103834,#103835,#103836,#103837,#103838,#103839,
#103840,#103841,#103842),.UNSPECIFIED.,.F.,.F.,(4,2,2,2,2,2,2,2,2,2,2,2,
2,2,2,2,2,2,2,2,2,2,2,2,2,2,2,2,2,2,2,2,2,2,2,2,2,2,2,2,2,2,2,2,2,2,2,2,
2,2,2,2,2,2,2,2,2,2,2,2,2,2,2,2,2,2,2,2,2,2,2,2,2,2,2,2,2,2,2,2,2,2,2,2,
2,2,2,2,2,2,2,2,2,2,2,2,2,2,2,2,2,2,4),(-2.22610704996512,-2.20550128129161,
-2.18810508570363,-2.18593385519407,-2.18487195420598,-2.1841134594657,
-2.18314923262218,-2.18149031312629,-2.17491384539396,-2.16827985191087,
-2.13837887934292,-2.13009701783793,-2.12755806368416,-2.12593922555329,
-2.1244206729256,-2.12242179429114,-2.11790059634646,-2.09350040897706,
-2.07705092748205,-2.07219608325262,-2.06895549397844,-2.06770859199797,
-2.06684343992376,-2.0660483579281,-2.06493610108897,-2.06200560446663,
-2.04355595309435,-2.02348432244987,-2.01306234549602,-2.01032296387726,
-2.00866010635629,-2.00715513115915,-2.00521792529932,-2.00115280592182,
-1.97066490215077,-1.95320548549658,-1.95103219483385,-1.9499697531547,
-1.94921106840316,-1.94824686072143,-1.94658847077552,-1.94002051247477,
-1.93338478398901,-1.9034810789982,-1.89519518906706,-1.89265557121669,
-1.89103642822728,-1.88951767001313,-1.88751863485605,-1.88299756308869,
-1.85858047685114,-1.8421435772716,-1.8372906057663,-1.83405085649242,-1.83280398082922,
-1.83193876343253,-1.83114365292999,-1.83003124939392,-1.82709959948778,
-1.80876320472529,-1.78860697336739,-1.77816086984924,-1.77541960527736,
-1.77375639511096,-1.77225161060185,-1.77031536724202,-1.76625497887861,
-1.73572503766731,-1.71829337251568,-1.71612097124736,-1.71505875868473,
-1.71430012947382,-1.71333582385902,-1.71167704129297,-1.70510458415129,
-1.69846946591539,-1.66856088790109,-1.66028085519697,-1.65774179312133,
-1.65612272761624,-1.65460384775618,-1.6526043682989,-1.64808103411075,
-1.62375393070014,-1.60724954526795,-1.60238561273262,-1.59914038801131,
-1.59789263990009,-1.59702721666021,-1.59623224434579,-1.59512045131583,
-1.5921938729755,-1.57284672147576,-1.55322643404189,-1.54658021882862,
-1.5417822101871,-1.53971306786211,-1.53818853734378,-1.53677400146492,
-1.53483546570562,-1.52989695310677,-1.49640613248406,-1.48414558948818),
 .UNSPECIFIED.);
#1539=B_SPLINE_CURVE_WITH_KNOTS('',3,(#103843,#103844,#103845,#103846,#103847,
#103848,#103849,#103850,#103851,#103852,#103853,#103854,#103855,#103856,
#103857,#103858,#103859,#103860,#103861,#103862,#103863,#103864,#103865,
#103866,#103867,#103868,#103869,#103870,#103871,#103872,#103873,#103874,
#103875,#103876,#103877,#103878,#103879,#103880,#103881,#103882,#103883,
#103884,#103885,#103886,#103887,#103888,#103889,#103890,#103891,#103892,
#103893,#103894,#103895,#103896,#103897,#103898,#103899,#103900,#103901,
#103902,#103903,#103904,#103905,#103906,#103907,#103908,#103909,#103910,
#103911,#103912,#103913,#103914,#103915,#103916,#103917,#103918,#103919,
#103920,#103921,#103922,#103923,#103924,#103925,#103926,#103927,#103928,
#103929,#103930,#103931,#103932,#103933,#103934,#103935,#103936,#103937,
#103938,#103939,#103940,#103941,#103942,#103943,#103944,#103945,#103946,
#103947,#103948,#103949,#103950,#103951,#103952,#103953,#103954,#103955,
#103956,#103957,#103958,#103959,#103960,#103961,#103962,#103963,#103964,
#103965,#103966,#103967,#103968,#103969,#103970,#103971,#103972,#103973,
#103974,#103975,#103976,#103977,#103978,#103979,#103980,#103981,#103982,
#103983,#103984,#103985,#103986,#103987,#103988,#103989,#103990,#103991,
#103992,#103993,#103994,#103995,#103996,#103997,#103998,#103999,#104000,
#104001,#104002,#104003,#104004,#104005,#104006,#104007,#104008,#104009,
#104010,#104011,#104012,#104013,#104014,#104015,#104016,#104017,#104018,
#104019,#104020,#104021,#104022,#104023,#104024,#104025,#104026,#104027,
#104028,#104029,#104030,#104031,#104032,#104033,#104034,#104035,#104036,
#104037,#104038,#104039,#104040,#104041,#104042,#104043,#104044,#104045,
#104046),.UNSPECIFIED.,.F.,.F.,(4,2,2,2,2,2,2,2,2,2,2,2,2,2,2,2,2,2,2,2,
2,2,2,2,2,2,2,2,2,2,2,2,2,2,2,2,2,2,2,2,2,2,2,2,2,2,2,2,2,2,2,2,2,2,2,2,
2,2,2,2,2,2,2,2,2,2,2,2,2,2,2,2,2,2,2,2,2,2,2,2,2,2,2,2,2,2,2,2,2,2,2,2,
2,2,2,2,2,2,2,2,2,4),(-2.01986711404084,-2.00149397536358,-1.98869985377435,
-1.98679560857064,-1.98578840545589,-1.98495050181473,-1.98390199694263,
-1.98225373663555,-1.97347956546237,-1.94390368319916,-1.931772227007,-1.92890662718964,
-1.92721674900399,-1.92571800226443,-1.92383046228648,-1.9208595192094,
-1.90028859243867,-1.87939204285366,-1.87096370576033,-1.86923620077264,
-1.86826683609095,-1.86742513744043,-1.86634386872644,-1.86454754847247,
-1.85198266203283,-1.82226488292153,-1.81375197539902,-1.81118947303606,
-1.80956593526822,-1.80805014172761,-1.80606527759675,-1.80162096948806,
-1.77528345007096,-1.75425352928614,-1.75208531650031,-1.75102428683803,
-1.75026615968043,-1.74930204974309,-1.74764263301021,-1.7410551291592,
-1.73442455992968,-1.70452728965447,-1.69625800657821,-1.69372103577476,
-1.69210305660383,-1.69058502890219,-1.68858643587658,-1.68406412922213,
-1.65976367537816,-1.63862657386854,-1.63519134668002,-1.63391599699051,
-1.63304546003156,-1.63225682721722,-1.63116823537041,-1.6283944876795,
-1.6050159117426,-1.58042201924304,-1.57701317935919,-1.5752071833797,-1.57372800344111,
-1.57198301376457,-1.56894659971462,-1.5554133739678,-1.53056253375716,
-1.51890185659636,-1.51703259176242,-1.5160327895258,-1.51519450479719,
-1.51413725652466,-1.51246011860772,-1.5030928352676,-1.47407727516581,
-1.46202736520136,-1.45916732756614,-1.45747868513583,-1.45597978049687,
-1.4540903588368,-1.45111311843643,-1.42947386717785,-1.40946638269828,
-1.40121265397739,-1.39949510888014,-1.3985279274702,-1.39768589490699,
-1.39660135970672,-1.39479374167545,-1.38096342239752,-1.3469355008027,
-1.34264857626484,-1.34069204048276,-1.33918078914116,-1.33754523156273,
-1.33492714990025,-1.32585541847392,-1.29650904670547,-1.28420692247016,
-1.28242015400097,-1.281341725396,-1.28050039456192,-1.27952928510668,-1.27804052283339),
 .UNSPECIFIED.);
#1540=B_SPLINE_CURVE_WITH_KNOTS('',3,(#104051,#104052,#104053,#104054,#104055,
#104056,#104057,#104058,#104059,#104060,#104061,#104062,#104063,#104064,
#104065,#104066,#104067,#104068,#104069,#104070,#104071,#104072,#104073,
#104074,#104075,#104076,#104077,#104078,#104079,#104080,#104081,#104082,
#104083,#104084,#104085,#104086,#104087,#104088,#104089,#104090,#104091,
#104092,#104093,#104094,#104095,#104096,#104097,#104098,#104099,#104100,
#104101,#104102,#104103,#104104,#104105,#104106,#104107,#104108,#104109,
#104110,#104111,#104112,#104113,#104114,#104115,#104116,#104117,#104118,
#104119,#104120,#104121,#104122,#104123,#104124,#104125,#104126,#104127,
#104128,#104129,#104130,#104131,#104132,#104133,#104134,#104135,#104136,
#104137,#104138,#104139,#104140,#104141,#104142,#104143,#104144,#104145,
#104146,#104147,#104148,#104149,#104150,#104151,#104152,#104153,#104154,
#104155,#104156,#104157,#104158,#104159,#104160,#104161,#104162,#104163,
#104164,#104165,#104166,#104167,#104168,#104169,#104170,#104171,#104172,
#104173,#104174,#104175,#104176,#104177,#104178,#104179,#104180,#104181,
#104182,#104183,#104184,#104185,#104186,#104187,#104188,#104189,#104190,
#104191,#104192,#104193,#104194,#104195,#104196,#104197,#104198,#104199,
#104200,#104201,#104202,#104203,#104204,#104205,#104206,#104207,#104208,
#104209,#104210,#104211,#104212,#104213,#104214,#104215,#104216,#104217,
#104218,#104219,#104220,#104221,#104222,#104223,#104224,#104225,#104226,
#104227,#104228,#104229,#104230,#104231,#104232,#104233,#104234,#104235,
#104236,#104237,#104238,#104239,#104240,#104241,#104242,#104243,#104244,
#104245,#104246,#104247,#104248,#104249,#104250,#104251,#104252,#104253,
#104254,#104255,#104256,#104257,#104258,#104259,#104260,#104261,#104262,
#104263,#104264,#104265,#104266,#104267,#104268,#104269,#104270,#104271,
#104272,#104273,#104274,#104275,#104276,#104277,#104278,#104279,#104280,
#104281,#104282,#104283,#104284,#104285,#104286,#104287,#104288,#104289,
#104290,#104291,#104292,#104293,#104294,#104295,#104296,#104297,#104298,
#104299,#104300,#104301,#104302,#104303,#104304,#104305,#104306,#104307,
#104308),.UNSPECIFIED.,.F.,.F.,(4,2,2,2,2,2,2,2,2,2,2,2,2,2,2,2,2,2,2,2,
2,2,2,2,2,2,2,2,2,2,2,2,2,2,2,2,2,2,2,2,2,2,2,2,2,2,2,2,2,2,2,2,2,2,2,2,
2,2,2,2,2,2,2,2,2,2,2,2,2,2,2,2,2,2,2,2,2,2,2,2,2,2,2,2,2,2,2,2,2,2,2,2,
2,2,2,2,2,2,2,2,2,2,2,2,2,2,2,2,2,2,2,2,2,2,2,2,2,2,2,2,2,2,2,2,2,2,2,2,
4),(-2.96786886973577,-2.95785689286692,-2.95264959365992,-2.95073047369495,
-2.94925312079407,-2.94780454720857,-2.94616584058611,-2.94356098609388,
-2.93557638518036,-2.92530150922596,-2.9068384860444,-2.89433462089359,
-2.89111690778034,-2.88987259097804,-2.88900761898966,-2.88821639909733,
-2.88710809866277,-2.88417945460901,-2.86600747968086,-2.85036799118396,
-2.84068417438163,-2.83642136520946,-2.83306116457156,-2.83128235898923,
-2.83127130736516,-2.8312594227592,-2.83124664029677,-2.83123288978141,
-2.8312180952081,-2.83120217426603,-2.83118503776084,-2.83116658901647,
-2.83114672319152,-2.83112532657952,-2.83110227579331,-2.83107743693406,
-2.83105066467395,-2.83102180126969,-2.83099067553294,-2.83095710172708,
-2.83093194337139,-2.82944293157537,-2.82756454275732,-2.82460236990099,
-2.80196387274249,-2.7857332191819,-2.77468013966401,-2.77284194225298,
-2.77185340971376,-2.77101691528075,-2.76995515792267,-2.76826449997813,
-2.7586911368712,-2.74931880536028,-2.72832012133503,-2.72125262823238,
-2.7162217528034,-2.71411045653806,-2.712575689053,-2.71116608450099,-2.70925639360369,
-2.70548691941654,-2.67619614302823,-2.65797111011836,-2.65577156006441,
-2.65470130444696,-2.65393971134428,-2.6529761248051,-2.65132366454225,
-2.64484129353594,-2.63819073566558,-2.60824849336731,-2.59995769599317,
-2.59741701683377,-2.59579724938962,-2.5942779343384,-2.59227820398957,
-2.58775572281516,-2.56323072573548,-2.54684035798431,-2.54199438052968,
-2.53875813527581,-2.53751200405902,-2.53664717544212,-2.53585278187051,
-2.53474128661837,-2.53181180038879,-2.51337984726407,-2.49329180933647,
-2.48286693582478,-2.48012920001551,-2.47846785795519,-2.47696460859289,
-2.47503014860834,-2.47097292860631,-2.44040951498069,-2.42298648807979,
-2.42081582996354,-2.4197546644234,-2.41899656122737,-2.41803236896773,
-2.41637418906627,-2.40980941399887,-2.40317347318246,-2.37328077728257,
-2.36497910619027,-2.36243722704195,-2.36081719109884,-2.359297970103,-2.35729885772379,
-2.35277983584678,-2.32835023538045,-2.31194752112263,-2.30710001751538,
-2.30386268964697,-2.30261571795862,-2.30175013030088,-2.30095472900709,
-2.29984148358813,-2.29690432031969,-2.2787402395881,-2.25846564675014,
-2.24798655600512,-2.24524264317062,-2.24357887092661,-2.24207424813948,
-2.24013915151677,-2.2360846967586,-2.22610704996512),.UNSPECIFIED.);
#1541=B_SPLINE_CURVE_WITH_KNOTS('',3,(#104309,#104310,#104311,#104312,#104313,
#104314,#104315,#104316,#104317,#104318,#104319,#104320,#104321,#104322,
#104323,#104324,#104325,#104326,#104327,#104328,#104329,#104330,#104331,
#104332,#104333,#104334,#104335,#104336,#104337,#104338,#104339,#104340,
#104341,#104342,#104343,#104344,#104345,#104346,#104347,#104348,#104349,
#104350,#104351,#104352,#104353,#104354,#104355,#104356,#104357,#104358,
#104359,#104360,#104361,#104362,#104363,#104364,#104365,#104366,#104367,
#104368,#104369,#104370,#104371,#104372,#104373,#104374,#104375,#104376,
#104377,#104378,#104379,#104380,#104381,#104382,#104383,#104384,#104385,
#104386,#104387,#104388,#104389,#104390,#104391,#104392,#104393,#104394,
#104395,#104396,#104397,#104398,#104399,#104400,#104401,#104402,#104403,
#104404,#104405,#104406,#104407,#104408,#104409,#104410,#104411,#104412,
#104413,#104414,#104415,#104416,#104417,#104418,#104419,#104420,#104421,
#104422,#104423,#104424,#104425,#104426,#104427,#104428,#104429,#104430,
#104431,#104432,#104433,#104434,#104435,#104436,#104437,#104438,#104439,
#104440,#104441,#104442,#104443,#104444,#104445,#104446,#104447,#104448,
#104449,#104450,#104451,#104452,#104453,#104454,#104455,#104456,#104457,
#104458,#104459,#104460,#104461,#104462,#104463,#104464,#104465,#104466,
#104467,#104468,#104469,#104470,#104471,#104472,#104473,#104474,#104475,
#104476,#104477,#104478,#104479,#104480,#104481,#104482,#104483,#104484,
#104485,#104486,#104487,#104488,#104489,#104490,#104491,#104492,#104493,
#104494,#104495,#104496,#104497,#104498,#104499,#104500,#104501,#104502,
#104503,#104504,#104505,#104506,#104507,#104508,#104509,#104510,#104511,
#104512),.UNSPECIFIED.,.F.,.F.,(4,2,2,2,2,2,2,2,2,2,2,2,2,2,2,2,2,2,2,2,
2,2,2,2,2,2,2,2,2,2,2,2,2,2,2,2,2,2,2,2,2,2,2,2,2,2,2,2,2,2,2,2,2,2,2,2,
2,2,2,2,2,2,2,2,2,2,2,2,2,2,2,2,2,2,2,2,2,2,2,2,2,2,2,2,2,2,2,2,2,2,2,2,
2,2,2,2,2,2,2,2,2,4),(-1.27804052283339,-1.27779354277622,-1.26921374673466,
-1.24615215792371,-1.22788586669804,-1.22494349880741,-1.22306464005362,
-1.22156677634983,-1.21987148606874,-1.216980855906,-1.2044692630371,-1.17179253262613,
-1.16609567259652,-1.16449858396085,-1.16355779691929,-1.16270930512896,
-1.16155756344434,-1.15890186298369,-1.14675613267963,-1.11317457280965,
-1.10821231914223,-1.10627046533854,-1.10485553976076,-1.10333251025302,
-1.10126883004227,-1.0964992625634,-1.0899029086718,-1.07054709728567,-1.05082231426154,
-1.04789966097991,-1.0467887373645,-1.04599425310984,-1.04512934652003,
-1.04388215912375,-1.04063724818695,-1.03577359860831,-1.01926373765555,
-0.994973588639409,-0.990452015073592,-0.988453645411723,-0.986935746151702,
-0.98531786759116,-0.982780987090211,-0.97451173681847,-0.944599183842762,
-0.93795899266781,-0.931367779478571,-0.929708083375804,-0.928743947946152,
-0.927985862467296,-0.926925008439456,-0.92475761153208,-0.904022419282702,
-0.877374135679222,-0.872946620414565,-0.870964609558215,-0.869449144542359,
-0.867824159097486,-0.865255539558594,-0.856685125800273,-0.826982297168291,
-0.814445536666213,-0.812649941824788,-0.81156873662837,-0.810726698109774,
-0.809756282500682,-0.808026064681788,-0.799564003474529,-0.777217344170429,
-0.75815764559839,-0.75519983006914,-0.753315710445747,-0.751816555244499,
-0.750122884427466,-0.747242613863021,-0.734907977080816,-0.703832967923239,
-0.696571717166207,-0.694859865863391,-0.693883548589329,-0.693051219494492,
-0.691967310301918,-0.68967873316349,-0.686603634471189,-0.678748581179012,
-0.654039356211465,-0.640316839892049,-0.637271899617777,-0.635525726446294,
-0.634047723181845,-0.632245863591957,-0.628853210844796,-0.603977633476396,
-0.580825564669791,-0.578041993013366,-0.576952021167913,-0.576163327927914,
-0.575293368524894,-0.574020841920639,-0.570605445405218,-0.54976549363765,
-0.536166236652312),.UNSPECIFIED.);
#1542=B_SPLINE_CURVE_WITH_KNOTS('',3,(#104515,#104516,#104517,#104518,#104519,
#104520,#104521,#104522,#104523,#104524,#104525,#104526,#104527,#104528,
#104529,#104530,#104531,#104532,#104533,#104534,#104535,#104536,#104537,
#104538,#104539,#104540,#104541,#104542,#104543,#104544,#104545,#104546,
#104547,#104548,#104549,#104550,#104551,#104552,#104553,#104554,#104555,
#104556,#104557,#104558,#104559,#104560,#104561,#104562,#104563,#104564,
#104565,#104566,#104567,#104568,#104569,#104570,#104571,#104572,#104573,
#104574,#104575,#104576,#104577,#104578,#104579,#104580,#104581,#104582,
#104583,#104584,#104585,#104586,#104587,#104588,#104589,#104590,#104591,
#104592,#104593,#104594,#104595,#104596,#104597,#104598,#104599,#104600,
#104601,#104602,#104603,#104604,#104605,#104606,#104607,#104608,#104609,
#104610,#104611,#104612,#104613,#104614,#104615,#104616,#104617,#104618,
#104619,#104620,#104621,#104622,#104623,#104624,#104625,#104626,#104627,
#104628,#104629,#104630,#104631,#104632,#104633,#104634,#104635,#104636,
#104637,#104638,#104639,#104640,#104641,#104642,#104643,#104644,#104645,
#104646,#104647,#104648,#104649,#104650,#104651,#104652,#104653,#104654,
#104655,#104656,#104657,#104658,#104659,#104660,#104661,#104662,#104663,
#104664,#104665,#104666,#104667,#104668,#104669,#104670,#104671,#104672,
#104673,#104674,#104675,#104676,#104677,#104678,#104679,#104680,#104681,
#104682,#104683,#104684,#104685,#104686,#104687,#104688,#104689,#104690,
#104691,#104692,#104693,#104694,#104695,#104696,#104697,#104698,#104699,
#104700),.UNSPECIFIED.,.F.,.F.,(4,2,2,2,2,2,2,2,2,2,2,2,2,2,2,2,2,2,2,2,
2,2,2,2,2,2,2,2,2,2,2,2,2,2,2,2,2,2,2,2,2,2,2,2,2,2,2,2,2,2,2,2,2,2,2,2,
2,2,2,2,2,2,2,2,2,2,2,2,2,2,2,2,2,2,2,2,2,2,2,2,2,2,2,2,2,2,2,2,2,2,2,2,
4),(-0.536166236652312,-0.525085231207484,-0.520567953445079,-0.518569339787368,
-0.517050414425168,-0.515430627671845,-0.512889021249871,-0.50458736279753,
-0.474640089736819,-0.467979450327641,-0.461490579047531,-0.45983767900236,
-0.458874081698197,-0.458112632188542,-0.457042813646653,-0.454845013004687,
-0.436674870711717,-0.407327856661352,-0.403149927900042,-0.401209844509549,
-0.399697243559294,-0.398045997313867,-0.395371015272676,-0.385744469389427,
-0.35558106721775,-0.353180361775628,-0.344415240389566,-0.34276649532011,
-0.341717457261505,-0.340881832016273,-0.339882944566339,-0.337995666679841,
-0.325443190434005,-0.298765263304739,-0.287485936178323,-0.284611116821944,
-0.282909955162882,-0.281424291679214,-0.279583588819669,-0.275969299581762,
-0.254886236187246,-0.232378153060786,-0.226389972304301,-0.224770081822884,
-0.223827553192379,-0.222981410989253,-0.221843094348616,-0.219268692304207,
-0.200653577221383,-0.172015795769246,-0.167701309523609,-0.165733192751794,
-0.164213322150942,-0.162568691223491,-0.159936410440464,-0.150810104984887,
-0.121120135557507,-0.109405628083183,-0.107622248750493,-0.106526986897927,
-0.105692523569586,-0.105682773912662,-0.105673291143312,-0.105664064451981,
-0.105655083595332,-0.10564633887878,-0.105637821094948,-0.105629521513252,
-0.105621431843887,-0.105613544210896,-0.105605851112159,-0.105598345430928,
-0.105591020376947,-0.1055838694892,-0.105576886620684,-0.105570065905969,
-0.105563401742921,-0.105556888777833,-0.10555052191761,-0.105544296282815,
-0.104496551007015,-0.103346651016605,-0.101479563606578,-0.0892256042285175,
-0.0570429508974814,-0.0522112497001512,-0.0502726622426464,-0.0488425185149138,
-0.0472858284284697,-0.0451445915942411,-0.0400400193764259,-0.0328700432185351,
-1.00000014535695E-6),.UNSPECIFIED.);
#1543=B_SPLINE_CURVE_WITH_KNOTS('',3,(#104704,#104705,#104706,#104707,#104708,
#104709,#104710,#104711,#104712,#104713,#104714,#104715,#104716,#104717,
#104718,#104719,#104720,#104721,#104722,#104723,#104724,#104725,#104726,
#104727,#104728,#104729,#104730,#104731,#104732,#104733,#104734,#104735,
#104736,#104737,#104738,#104739,#104740,#104741,#104742,#104743,#104744,
#104745,#104746,#104747,#104748,#104749,#104750,#104751,#104752,#104753,
#104754,#104755,#104756,#104757,#104758,#104759,#104760,#104761,#104762,
#104763,#104764,#104765),.UNSPECIFIED.,.F.,.F.,(4,2,2,2,2,2,2,2,2,2,2,2,
2,2,2,2,2,2,2,2,2,2,2,2,2,2,2,2,2,2,4),(5.26465888469903E-5,0.00458003943048162,
0.0076256166217089,0.00923307394815808,0.0105570311839449,0.0118209960109234,
0.0134523997639754,0.0162830945574481,0.0250310363928198,0.0569680207680776,
0.0667585963604424,0.0684856004228339,0.0694262516517115,0.070257611045996,
0.0713168672239314,0.0730035599451736,0.0824114043194782,0.0932430412621605,
0.108440124136716,0.127405659390686,0.130614876340645,0.132680842693845,
0.134340156702719,0.13623440842581,0.139517071288727,0.155909768338738,
0.176205334305,0.183267029437581,0.185053305917431,0.185861120043884,0.186559797993667),
 .UNSPECIFIED.);
#1544=B_SPLINE_CURVE_WITH_KNOTS('',3,(#104766,#104767,#104768,#104769,#104770,
#104771,#104772,#104773,#104774,#104775,#104776,#104777,#104778,#104779,
#104780,#104781,#104782,#104783,#104784,#104785,#104786,#104787,#104788,
#104789,#104790,#104791,#104792,#104793,#104794,#104795,#104796,#104797,
#104798,#104799,#104800,#104801,#104802,#104803,#104804,#104805,#104806,
#104807,#104808,#104809,#104810,#104811,#104812,#104813,#104814,#104815,
#104816,#104817,#104818,#104819,#104820,#104821,#104822,#104823,#104824,
#104825,#104826,#104827,#104828,#104829,#104830,#104831,#104832),
 .UNSPECIFIED.,.F.,.F.,(4,3,3,3,3,3,3,3,3,3,3,3,3,3,3,3,3,3,3,3,3,3,4),
(152.205784650184,152.32550641777,152.44545518428,152.532661347998,152.532706586939,
152.643528857141,152.657043371795,152.776764042929,152.896367880645,153.015907297727,
153.135434595286,153.255084298657,153.374807527798,153.485184154958,153.494746688451,
153.52734741509,153.527400865785,153.641271566567,153.658393831217,153.780909296427,
153.788925130557,153.918783873189,153.938039816989),.UNSPECIFIED.);
#1545=B_SPLINE_CURVE_WITH_KNOTS('',3,(#104835,#104836,#104837,#104838,#104839,
#104840,#104841,#104842,#104843,#104844,#104845,#104846,#104847,#104848,
#104849,#104850,#104851,#104852,#104853,#104854,#104855,#104856,#104857,
#104858,#104859,#104860,#104861,#104862,#104863,#104864,#104865,#104866,
#104867,#104868,#104869,#104870,#104871,#104872,#104873,#104874,#104875,
#104876,#104877,#104878,#104879,#104880,#104881,#104882,#104883,#104884,
#104885,#104886,#104887,#104888,#104889,#104890,#104891,#104892,#104893,
#104894,#104895,#104896,#104897,#104898,#104899,#104900,#104901,#104902,
#104903,#104904,#104905,#104906,#104907,#104908,#104909,#104910,#104911,
#104912,#104913,#104914,#104915,#104916,#104917,#104918,#104919,#104920,
#104921,#104922,#104923,#104924,#104925,#104926,#104927,#104928,#104929,
#104930,#104931,#104932,#104933,#104934,#104935,#104936,#104937,#104938,
#104939,#104940,#104941,#104942,#104943,#104944,#104945,#104946,#104947,
#104948,#104949,#104950,#104951,#104952,#104953,#104954,#104955,#104956,
#104957,#104958,#104959,#104960,#104961,#104962,#104963,#104964,#104965,
#104966,#104967,#104968,#104969,#104970,#104971,#104972,#104973,#104974,
#104975,#104976,#104977,#104978,#104979,#104980,#104981,#104982,#104983,
#104984,#104985,#104986,#104987,#104988,#104989,#104990,#104991,#104992,
#104993,#104994,#104995,#104996,#104997,#104998,#104999,#105000,#105001,
#105002,#105003,#105004,#105005,#105006,#105007,#105008,#105009,#105010,
#105011,#105012,#105013,#105014,#105015,#105016,#105017,#105018,#105019,
#105020,#105021,#105022,#105023,#105024,#105025,#105026,#105027,#105028,
#105029,#105030,#105031,#105032,#105033,#105034,#105035,#105036,#105037,
#105038,#105039,#105040,#105041,#105042,#105043,#105044,#105045,#105046,
#105047,#105048,#105049,#105050,#105051,#105052,#105053,#105054,#105055,
#105056,#105057,#105058,#105059,#105060,#105061,#105062,#105063,#105064,
#105065,#105066,#105067,#105068,#105069,#105070),.UNSPECIFIED.,.F.,.F.,
(4,2,2,2,2,2,2,2,2,2,2,2,2,2,2,2,2,2,2,2,2,2,2,2,2,2,2,2,2,2,2,2,2,2,2,
2,2,2,2,2,2,2,2,2,2,2,2,2,2,2,2,2,2,2,2,2,2,2,2,2,2,2,2,2,2,2,2,2,2,2,2,
2,2,2,2,2,2,2,2,2,2,2,2,2,2,2,2,2,2,2,2,2,2,2,2,2,2,2,2,2,2,2,2,2,2,2,2,
2,2,2,2,2,2,2,2,2,2,4),(2.76458849571582,2.80165031556903,2.80595712423809,
2.8181262917974,2.82112649950848,2.82286401352687,2.82435549965188,2.82616746780645,
2.82959813973857,2.85416452357968,2.87456953748744,2.89265855727155,2.89482601013189,
2.89588753031213,2.89672429239254,2.89770372228433,2.8994747521816,2.90838575829188,
2.94946550338247,2.9516209106145,2.96397553243166,2.96699344821178,2.9687363529125,
2.97021529852142,2.97201954171125,2.97540679408675,2.99806263722299,3.02401248261017,
3.02862601575098,3.03885070485117,3.0406018817737,3.04168340260912,3.04252425522643,
3.04349603569766,3.04521969053163,3.05324472628385,3.07119368038886,3.10633505437255,
3.1112796202855,3.11322598453512,3.11464450555406,3.11616939096845,3.11822793146341,
3.12291942592611,3.14573582176358,3.17035133284012,3.17310849693219,3.1744523527326,
3.18446830513651,3.1862082673416,3.18728583679269,3.18812242788805,3.18908309561103,
3.19079023058684,3.19878265630355,3.21664964225608,3.25246155588452,3.25739226988589,
3.25932556685361,3.26073174056842,3.26224058479881,3.26427241708641,3.26887974521027,
3.28841684839569,3.3170693627333,3.33025295232948,3.33228961748616,3.33333508681242,
3.33416930774878,3.33515763893095,3.33696674428531,3.34656811712221,3.36999616002673,
3.4008104752932,3.40401526821518,3.40595966462003,3.40747501930742,3.40912562733698,
3.41178380794678,3.42096569239179,3.45233426059145,3.47599010303093,3.47810992632144,
3.47917377086082,3.48000984894567,3.48001546626198,3.48002082261248,3.48002593163293,
3.48003139267474,3.48003679562201,3.48004214154125,3.48004743145613,3.48005266638362,
3.48005784732583,3.48006297525967,3.48006805113035,3.48007307586283,3.48007805034535,
3.48008297548347,3.48008785213301,3.48009268113104,3.48009746332489,3.48010219951981,
3.48010689050661,3.48011153705322,3.4811186179993,3.48300274687985,3.49345177287389,
3.5237989557689,3.54465138515542,3.54780944427495,3.5497724456426,3.55130081457342,
3.55299013295557,3.55576687338473,3.56598343040685,3.58447765124171,3.61301883334127),
 .UNSPECIFIED.);
#1546=B_SPLINE_CURVE_WITH_KNOTS('',3,(#105073,#105074,#105075,#105076,#105077,
#105078,#105079,#105080,#105081,#105082,#105083,#105084,#105085,#105086,
#105087,#105088,#105089,#105090,#105091,#105092,#105093,#105094,#105095,
#105096,#105097,#105098,#105099,#105100,#105101,#105102,#105103,#105104,
#105105,#105106,#105107,#105108,#105109,#105110,#105111,#105112,#105113,
#105114,#105115,#105116,#105117,#105118,#105119,#105120,#105121,#105122,
#105123,#105124,#105125,#105126,#105127,#105128,#105129,#105130,#105131,
#105132,#105133,#105134,#105135,#105136,#105137,#105138,#105139,#105140,
#105141,#105142,#105143,#105144,#105145,#105146,#105147,#105148,#105149,
#105150,#105151,#105152,#105153,#105154,#105155,#105156,#105157,#105158,
#105159,#105160,#105161,#105162,#105163,#105164,#105165,#105166,#105167,
#105168,#105169,#105170,#105171,#105172,#105173,#105174,#105175,#105176,
#105177,#105178,#105179,#105180,#105181,#105182,#105183,#105184,#105185,
#105186,#105187,#105188,#105189,#105190,#105191,#105192,#105193,#105194,
#105195,#105196,#105197,#105198,#105199,#105200,#105201,#105202,#105203,
#105204,#105205,#105206,#105207,#105208,#105209,#105210,#105211,#105212,
#105213,#105214,#105215,#105216,#105217,#105218,#105219,#105220,#105221,
#105222,#105223,#105224,#105225,#105226,#105227,#105228,#105229,#105230,
#105231,#105232,#105233,#105234,#105235,#105236,#105237,#105238),
 .UNSPECIFIED.,.F.,.F.,(4,2,2,2,2,2,2,2,2,2,2,2,2,2,2,2,2,2,2,2,2,2,2,2,
2,2,2,2,2,2,2,2,2,2,2,2,2,2,2,2,2,2,2,2,2,2,2,2,2,2,2,2,2,2,2,2,2,2,2,2,
2,2,2,2,2,2,2,2,2,2,2,2,2,2,2,2,2,2,2,2,2,2,4),(5.82345211094344E-5,0.000962432406826108,
0.00218339026927038,0.00510626843170436,0.0281859504736574,0.0497092541387239,
0.060399779900796,0.0633865947713838,0.0652320784528269,0.0669226723266856,
0.0690892029088175,0.0726575785754937,0.104139277570954,0.122704290035139,
0.135602756706391,0.142206590267457,0.143830243929883,0.144790296601867,
0.145627621028536,0.146681926730478,0.148420489755403,0.159598768885037,
0.18798784120411,0.204078066656765,0.210131112885388,0.214581945054722,
0.216530737681881,0.2179716028151,0.219309491332927,0.221140566504419,0.225761634791897,
0.266437087089506,0.282474900800036,0.289912929596359,0.29152368223493,
0.292445971682925,0.293281597898723,0.294357453789363,0.296517608898025,
0.317067504076477,0.347312668885674,0.360861187175288,0.363894074149783,
0.365640323176316,0.367160809205848,0.369035709233282,0.371902596480564,
0.385693878110236,0.422840046100618,0.434096470386929,0.436016443818509,
0.437045950207626,0.437901058644632,0.438953352297794,0.440973129135816,
0.453050999205782,0.483038601769635,0.502247186452089,0.506834410277817,
0.508878002902064,0.510403932807444,0.51183215535006,0.513805602569262,
0.518894269422453,0.552635318881072,0.578948090231822,0.58163614276351,
0.582796255349648,0.583645611773807,0.5845655425837,0.586081192551398,0.590996599683048,
0.622400966429067,0.641278273758192,0.651556558477386,0.654297564592166,
0.655954021965353,0.657445163551626,0.659349476773255,0.662389166147018,
0.680299895717508,0.712120523626618,0.717606620371918),.UNSPECIFIED.);
#1547=B_SPLINE_CURVE_WITH_KNOTS('',3,(#105243,#105244,#105245,#105246,#105247,
#105248,#105249,#105250,#105251,#105252,#105253,#105254,#105255,#105256,
#105257,#105258,#105259,#105260,#105261,#105262,#105263,#105264,#105265,
#105266,#105267,#105268,#105269,#105270,#105271,#105272,#105273,#105274,
#105275,#105276,#105277,#105278,#105279,#105280,#105281,#105282,#105283,
#105284,#105285,#105286,#105287,#105288,#105289,#105290,#105291,#105292,
#105293,#105294,#105295,#105296,#105297,#105298,#105299,#105300,#105301,
#105302,#105303,#105304,#105305,#105306,#105307,#105308,#105309,#105310,
#105311,#105312,#105313,#105314,#105315,#105316,#105317,#105318,#105319,
#105320,#105321),.UNSPECIFIED.,.F.,.F.,(4,3,3,3,3,3,3,3,3,3,3,3,3,3,3,3,
3,3,3,3,3,3,3,3,3,3,4),(-0.272803646496736,-0.263130204428988,-0.245860818959094,
-0.239585991691747,-0.234115749182603,-0.216916546212463,-0.205423868019635,
-0.200353055275459,-0.196895211330308,-0.180142741104203,-0.163804796575999,
-0.154097377599458,-0.147221560984452,-0.144240702043143,-0.128386580298794,
-0.124975120669838,-0.108765198492335,-0.0956970463056653,-0.0926130492690722,
-0.0768457730014618,-0.0611559826881288,-0.053296886616634,-0.0475073198824726,
-0.0447089256306213,-0.0296007544670048,-0.0148003772335024,0.),
 .UNSPECIFIED.);
#1548=B_SPLINE_CURVE_WITH_KNOTS('',3,(#105322,#105323,#105324,#105325,#105326,
#105327,#105328,#105329,#105330,#105331,#105332,#105333,#105334,#105335),
 .UNSPECIFIED.,.F.,.F.,(4,2,2,2,2,2,4),(1.00000221648494E-6,0.0490633756002225,
0.10485433700254,0.159887956090769,0.216674600864298,0.269192125233152,
0.323332368022587),.UNSPECIFIED.);
#1549=B_SPLINE_CURVE_WITH_KNOTS('',3,(#105941,#105942,#105943,#105944,#105945,
#105946),.UNSPECIFIED.,.F.,.F.,(4,2,4),(8.69075182808115E-5,0.00135534780982827,
0.00262696644863166),.UNSPECIFIED.);
#1550=B_SPLINE_CURVE_WITH_KNOTS('',3,(#105947,#105948,#105949,#105950,#105951,
#105952,#105953,#105954,#105955,#105956,#105957,#105958,#105959,#105960),
 .UNSPECIFIED.,.F.,.F.,(4,2,2,2,2,2,4),(4.19423088180546E-5,0.0458823493220878,
0.0903849398187459,0.138485347324558,0.185100854943403,0.232357774450867,
0.273915327518736),.UNSPECIFIED.);
#1551=B_SPLINE_CURVE_WITH_KNOTS('',3,(#105965,#105966,#105967,#105968,#105969,
#105970,#105971,#105972,#105973,#105974,#105975,#105976,#105977,#105978,
#105979,#105980,#105981,#105982,#105983,#105984,#105985,#105986,#105987,
#105988,#105989,#105990,#105991,#105992,#105993,#105994,#105995,#105996,
#105997,#105998,#105999,#106000,#106001,#106002,#106003,#106004,#106005,
#106006,#106007,#106008,#106009,#106010,#106011,#106012,#106013,#106014,
#106015,#106016,#106017,#106018,#106019,#106020,#106021,#106022,#106023,
#106024,#106025,#106026,#106027,#106028,#106029,#106030,#106031,#106032,
#106033,#106034,#106035,#106036,#106037,#106038,#106039,#106040,#106041,
#106042,#106043),.UNSPECIFIED.,.F.,.F.,(4,3,3,3,3,3,3,3,3,3,3,3,3,3,3,3,
3,3,3,3,3,3,3,3,3,3,4),(-0.272803579328725,-0.263130204428921,-0.245860818959034,
-0.239089121769124,-0.233709153701305,-0.216514195238077,-0.200353057339568,
-0.196895211887197,-0.180150634784372,-0.163785286417538,-0.1543299497365,
-0.148620089158273,-0.143731840392854,-0.128386591850485,-0.124975120669821,
-0.108729756337865,-0.101103756501427,-0.0956970454135588,-0.092613048702616,
-0.0768309346477273,-0.0612146988449913,-0.0532968855853477,-0.0475073169611359,
-0.044708922933863,-0.029600746467927,-0.0148003732339635,0.),
 .UNSPECIFIED.);
#1552=B_SPLINE_CURVE_WITH_KNOTS('',3,(#106649,#106650,#106651,#106652,#106653,
#106654),.UNSPECIFIED.,.F.,.F.,(4,2,4),(-0.00257291209214509,-0.00129181487758483,
-1.00000002428626E-6),.UNSPECIFIED.);
#1553=B_SPLINE_CURVE_WITH_KNOTS('',3,(#107631,#107632,#107633,#107634,#107635,
#107636,#107637,#107638,#107639,#107640,#107641,#107642,#107643,#107644,
#107645,#107646,#107647,#107648,#107649,#107650,#107651,#107652,#107653,
#107654,#107655,#107656,#107657,#107658,#107659,#107660,#107661,#107662,
#107663,#107664,#107665,#107666,#107667,#107668,#107669,#107670,#107671,
#107672,#107673,#107674,#107675,#107676,#107677,#107678,#107679,#107680,
#107681,#107682,#107683,#107684,#107685,#107686,#107687,#107688,#107689,
#107690,#107691,#107692,#107693,#107694,#107695,#107696,#107697,#107698,
#107699,#107700,#107701,#107702,#107703,#107704,#107705,#107706,#107707,
#107708,#107709,#107710,#107711,#107712,#107713,#107714,#107715,#107716,
#107717,#107718,#107719,#107720,#107721,#107722,#107723,#107724,#107725,
#107726,#107727,#107728,#107729,#107730,#107731,#107732,#107733,#107734,
#107735,#107736,#107737,#107738,#107739,#107740,#107741,#107742,#107743,
#107744,#107745,#107746,#107747,#107748,#107749,#107750,#107751,#107752,
#107753,#107754,#107755,#107756),.UNSPECIFIED.,.F.,.F.,(4,2,2,2,2,2,2,2,
2,2,2,2,2,2,2,2,2,2,2,2,2,2,2,2,2,2,2,2,2,2,2,2,2,2,2,2,2,2,2,2,2,2,2,2,
2,2,2,2,2,2,2,2,2,2,2,2,2,2,2,2,2,2,4),(2.76410463468713,2.77789812941896,
2.78029099172256,2.78154043546213,2.78255236827767,2.78378253357171,2.78613322726203,
2.80299114552905,2.84623477508507,2.85146639624688,2.85385187931519,2.85569291033944,
2.85768346019709,2.8608647368197,2.87181382805971,2.89151307140856,2.92219014353228,
2.92546467461625,2.92689529622041,2.92791948796111,2.92800365644322,2.92802691950589,
2.92804697267802,2.92806430741348,2.92807932856926,2.92809237225132,2.92810371941849,
2.92811644168053,2.92812877912382,2.92814074852271,2.9281523656638,2.92816364545057,
2.92817460199015,2.92818524861464,2.92819559790968,2.92820566182541,2.92821545166794,
2.92822497815332,2.92823425145468,2.92824328122277,2.92825207665361,2.92826064643558,
2.92826899886783,2.92827714184007,2.92828508287351,2.92829282915032,2.92830038747757,
2.92830776434548,2.9283149659868,2.92832199832138,2.92958491940801,2.93096879994323,
2.93761211253387,2.94996160565319,2.96335951326714,2.9916822450335,2.99530203860186,
2.99761541079866,2.99946130850531,3.00155231497011,3.00512210431552,3.02061545583317,
3.06019655133367),.UNSPECIFIED.);
#1554=B_SPLINE_CURVE_WITH_KNOTS('',3,(#107759,#107760,#107761,#107762,#107763,
#107764,#107765,#107766,#107767,#107768,#107769,#107770,#107771,#107772,
#107773,#107774,#107775,#107776,#107777,#107778,#107779,#107780,#107781,
#107782,#107783,#107784,#107785,#107786,#107787,#107788,#107789),
 .UNSPECIFIED.,.F.,.F.,(4,3,3,3,3,3,3,3,3,3,4),(0.,0.116094185676976,0.232131701312071,
0.348141226325033,0.464158878026556,0.580220774075408,0.69645813588627,
0.812789557622708,0.92936017010412,0.992536683255691,1.12274180646084),
 .UNSPECIFIED.);
#1555=B_SPLINE_CURVE_WITH_KNOTS('',3,(#107794,#107795,#107796,#107797,#107798,
#107799,#107800,#107801,#107802,#107803,#107804,#107805,#107806,#107807,
#107808,#107809,#107810,#107811,#107812,#107813,#107814,#107815,#107816,
#107817,#107818,#107819,#107820,#107821,#107822,#107823,#107824,#107825,
#107826,#107827,#107828,#107829,#107830,#107831,#107832,#107833,#107834,
#107835,#107836,#107837,#107838,#107839,#107840,#107841,#107842,#107843,
#107844,#107845,#107846,#107847,#107848,#107849,#107850,#107851,#107852,
#107853,#107854,#107855,#107856,#107857,#107858,#107859,#107860,#107861,
#107862,#107863,#107864,#107865,#107866,#107867,#107868,#107869,#107870,
#107871,#107872,#107873,#107874,#107875,#107876,#107877,#107878,#107879,
#107880,#107881,#107882,#107883,#107884,#107885,#107886,#107887,#107888,
#107889,#107890,#107891,#107892,#107893,#107894,#107895,#107896,#107897,
#107898,#107899,#107900,#107901,#107902,#107903,#107904,#107905,#107906,
#107907,#107908,#107909,#107910,#107911,#107912,#107913,#107914,#107915,
#107916,#107917,#107918,#107919,#107920,#107921,#107922,#107923,#107924,
#107925,#107926,#107927,#107928,#107929,#107930,#107931,#107932,#107933,
#107934,#107935,#107936,#107937,#107938,#107939,#107940,#107941,#107942,
#107943,#107944,#107945,#107946,#107947,#107948,#107949,#107950,#107951,
#107952,#107953,#107954,#107955,#107956,#107957,#107958,#107959,#107960,
#107961,#107962,#107963,#107964,#107965,#107966,#107967,#107968,#107969,
#107970,#107971,#107972,#107973,#107974,#107975,#107976,#107977,#107978,
#107979,#107980,#107981,#107982,#107983,#107984,#107985,#107986,#107987,
#107988,#107989,#107990,#107991,#107992,#107993,#107994,#107995,#107996,
#107997,#107998,#107999),.UNSPECIFIED.,.F.,.F.,(4,2,2,2,2,2,2,2,2,2,2,2,
2,2,2,2,2,2,2,2,2,2,2,2,2,2,2,2,2,2,2,2,2,2,2,2,2,2,2,2,2,2,2,2,2,2,2,2,
2,2,2,2,2,2,2,2,2,2,2,2,2,2,2,2,2,2,2,2,2,2,2,2,2,2,2,2,2,2,2,2,2,2,2,2,
2,2,2,2,2,2,2,2,2,2,2,2,2,2,2,2,2,2,4),(1.84269843666847,1.84465206436514,
1.86466744624785,1.88909843978047,1.9044696726718,1.90665505477036,1.90796783409467,
1.90898768484762,1.91015809674146,1.9122323585912,1.92207896927376,1.9452269465831,
1.97433899529737,1.97795641832976,1.98024962844833,1.98206668280837,1.98411096986709,
1.98756517846782,2.00191160002639,2.03460536231984,2.05003291699972,2.05222065299162,
2.05353431007178,2.05455467608111,2.05572572941863,2.05780046852841,2.06763838032658,
2.0907492258872,2.11985991651743,2.12347708723234,2.12577069799239,2.12758844718778,
2.12963392691719,2.13309118363733,2.1474676822273,2.18030996796785,2.19557941550631,
2.19776169421316,2.19907374086217,2.20009333137368,2.2012632832125,2.20333853115487,
2.2132238094026,2.23655464115746,2.26545757916821,2.26907355681657,2.27136517396421,
2.27318051073824,2.27522236239165,2.27867116351496,2.29297117305714,2.32542129106005,
2.33366690394975,2.34180525325721,2.34382697877215,2.34499712305827,2.34591425164786,
2.34719192709616,2.34977952899999,2.37447329543612,2.40897414384731,2.41433829493518,
2.41674135846877,2.41857871311583,2.42054835059226,2.42365963261701,2.43399481303058,
2.45197144537995,2.47961394855035,2.48744011589297,2.48943851321585,2.49060482548682,
2.49152667176838,2.49282038950961,2.49547135894722,2.51680170906175,2.55487684006113,
2.55982438698553,2.56217952473733,2.56400748672678,2.56602509832581,2.56934289824803,
2.58184463659192,2.60541404761194,2.63028997449203,2.63388567973593,2.6352385295489,
2.63620312834631,2.63724143592376,2.63872672719072,2.64253391123869,2.64817938671692,
2.66657909981711,2.70000646731652,2.70544755102859,2.70785350904814,2.70968040878739,
2.71162645737796,2.7146740301476,2.72454162917124,2.74132224400079,2.76169470610199,
2.76410463468713),.UNSPECIFIED.);
#1556=B_SPLINE_CURVE_WITH_KNOTS('',3,(#108000,#108001,#108002,#108003,#108004,
#108005,#108006,#108007,#108008,#108009,#108010,#108011,#108012,#108013,
#108014,#108015,#108016,#108017,#108018,#108019,#108020,#108021,#108022,
#108023,#108024,#108025,#108026,#108027,#108028,#108029,#108030,#108031,
#108032,#108033,#108034,#108035,#108036,#108037,#108038,#108039,#108040,
#108041,#108042,#108043,#108044,#108045,#108046,#108047,#108048,#108049,
#108050,#108051,#108052,#108053,#108054,#108055,#108056,#108057,#108058,
#108059,#108060,#108061,#108062,#108063,#108064,#108065,#108066,#108067,
#108068,#108069,#108070,#108071,#108072,#108073,#108074,#108075,#108076,
#108077,#108078,#108079,#108080,#108081,#108082,#108083,#108084,#108085,
#108086,#108087,#108088,#108089,#108090,#108091,#108092,#108093,#108094,
#108095,#108096,#108097,#108098,#108099,#108100,#108101,#108102,#108103,
#108104,#108105,#108106,#108107,#108108,#108109,#108110,#108111,#108112,
#108113,#108114,#108115,#108116,#108117,#108118,#108119,#108120,#108121,
#108122,#108123,#108124,#108125,#108126,#108127,#108128,#108129,#108130,
#108131,#108132,#108133,#108134,#108135,#108136,#108137,#108138,#108139,
#108140,#108141,#108142,#108143,#108144,#108145,#108146,#108147,#108148,
#108149,#108150,#108151,#108152,#108153,#108154,#108155,#108156,#108157,
#108158,#108159,#108160,#108161,#108162,#108163,#108164,#108165,#108166,
#108167,#108168,#108169,#108170,#108171,#108172,#108173,#108174,#108175,
#108176,#108177,#108178,#108179,#108180,#108181,#108182,#108183,#108184,
#108185,#108186,#108187,#108188,#108189,#108190,#108191,#108192,#108193,
#108194,#108195,#108196,#108197,#108198,#108199,#108200,#108201,#108202,
#108203,#108204,#108205,#108206,#108207,#108208,#108209),.UNSPECIFIED.,
 .F.,.F.,(4,2,2,2,2,2,2,2,2,2,2,2,2,2,2,2,2,2,2,2,2,2,2,2,2,2,2,2,2,2,2,
2,2,2,2,2,2,2,2,2,2,2,2,2,2,2,2,2,2,2,2,2,2,2,2,2,2,2,2,2,2,2,2,2,2,2,2,
2,2,2,2,2,2,2,2,2,2,2,2,2,2,2,2,2,2,2,2,2,2,2,2,2,2,2,2,2,2,2,2,2,2,2,2,
2,4),(0.000399761267031184,0.0354038923493914,0.0475757413653406,0.0507498700600226,
0.052665118299736,0.054389506155791,0.0565945699565813,0.0601266017211276,
0.0900469725943057,0.106246160835366,0.118415915794598,0.124896777653985,
0.126616318895631,0.127551727208082,0.128562730137273,0.129856744256951,
0.131930054904672,0.143969798295755,0.146782220099005,0.183594347104414,
0.195488779260129,0.198784031837144,0.200815362002396,0.202674196585776,
0.205055700711521,0.210174161082761,0.245387517317568,0.267665523710923,
0.270379134128065,0.27170439868395,0.272745129037137,0.273965945445756,
0.27617422487073,0.286798406387755,0.312242333914371,0.33398952117668,0.340471820486383,
0.343097120955262,0.344972310462606,0.346671748477799,0.349365105914915,
0.354370088839332,0.386014049197861,0.411288245845744,0.415452225451261,
0.416999251761255,0.418055054273712,0.419004476870668,0.420311502973881,
0.423621027919398,0.454287009212792,0.470716343632252,0.484712895793224,
0.488126907672694,0.490153489225955,0.49195839668569,0.494240923051114,
0.497850101060658,0.526477617454613,0.547091629527813,0.559923356448015,
0.5621323675004,0.563326159800845,0.564339340622975,0.565627166301655,0.567680293843476,
0.579345217611069,0.591205943481146,0.617373085928431,0.62612762103121,
0.632333551642897,0.634910852335761,0.636773918413517,0.638477516374394,
0.640773585663114,0.645266778309606,0.682999264416808,0.704568513315369,
0.707226533438398,0.708521799455347,0.709541217013154,0.710745881195248,
0.712911733600078,0.723032759100198,0.727043210822709,0.729718387332021,
0.755044277666134,0.773420450493433,0.778249639393888,0.780579516497017,
0.782401446758974,0.784426227990873,0.787788000658176,0.799378632288752,
0.841947045258856,0.848135232477724,0.852218090185299,0.853752224696319,
0.854804710603946,0.855760817272099,0.857083418788338,0.860466964580924,
0.890220433337641,0.910689042243752,0.92190171802025),.UNSPECIFIED.);
#1557=B_SPLINE_CURVE_WITH_KNOTS('',3,(#108214,#108215,#108216,#108217,#108218,
#108219,#108220,#108221,#108222,#108223,#108224,#108225,#108226,#108227,
#108228,#108229,#108230,#108231,#108232,#108233,#108234,#108235,#108236,
#108237,#108238,#108239,#108240,#108241,#108242,#108243,#108244,#108245,
#108246,#108247,#108248,#108249,#108250,#108251,#108252,#108253,#108254,
#108255,#108256,#108257,#108258,#108259,#108260,#108261,#108262,#108263,
#108264,#108265,#108266,#108267,#108268,#108269,#108270,#108271,#108272,
#108273,#108274,#108275,#108276,#108277,#108278,#108279,#108280,#108281,
#108282,#108283,#108284,#108285,#108286,#108287,#108288,#108289,#108290,
#108291,#108292,#108293,#108294,#108295,#108296,#108297,#108298,#108299,
#108300,#108301,#108302,#108303,#108304,#108305,#108306,#108307,#108308,
#108309,#108310,#108311,#108312,#108313,#108314,#108315,#108316,#108317,
#108318,#108319,#108320,#108321,#108322,#108323,#108324,#108325,#108326,
#108327,#108328,#108329,#108330,#108331,#108332,#108333,#108334,#108335,
#108336,#108337,#108338,#108339,#108340,#108341,#108342,#108343,#108344,
#108345,#108346,#108347,#108348,#108349,#108350,#108351,#108352,#108353,
#108354,#108355,#108356,#108357,#108358,#108359,#108360,#108361,#108362,
#108363,#108364,#108365,#108366,#108367,#108368,#108369,#108370,#108371,
#108372,#108373,#108374,#108375,#108376,#108377,#108378,#108379,#108380,
#108381,#108382,#108383,#108384,#108385,#108386,#108387,#108388,#108389,
#108390,#108391,#108392,#108393,#108394,#108395,#108396,#108397,#108398,
#108399,#108400,#108401,#108402,#108403,#108404,#108405,#108406,#108407,
#108408,#108409,#108410,#108411,#108412,#108413,#108414,#108415,#108416,
#108417,#108418,#108419,#108420,#108421,#108422,#108423,#108424,#108425,
#108426,#108427,#108428,#108429,#108430,#108431,#108432,#108433,#108434,
#108435,#108436,#108437,#108438,#108439),.UNSPECIFIED.,.F.,.F.,(4,2,2,2,
2,2,2,2,2,2,2,2,2,2,2,2,2,2,2,2,2,2,2,2,2,2,2,2,2,2,2,2,2,2,2,2,2,2,2,2,
2,2,2,2,2,2,2,2,2,2,2,2,2,2,2,2,2,2,2,2,2,2,2,2,2,2,2,2,2,2,2,2,2,2,2,2,
2,2,2,2,2,2,2,2,2,2,2,2,2,2,2,2,2,2,2,2,2,2,2,2,2,2,2,2,2,2,2,2,2,2,2,2,
4),(0.921274759476541,0.924524411894003,0.955331798003363,0.959422856744768,
0.961603573824362,0.963395822341905,0.965516884118037,0.969223274006393,
0.985857093836077,1.01696676767491,1.03138812448544,1.03366693698771,1.03488127566808,
1.03589622863804,1.03717033314132,1.03917954371989,1.04997318880504,1.05265600228155,
1.08186307806757,1.09977080420862,1.10453584607552,1.10685232120785,1.10867157897424,
1.11070145120502,1.11409077440169,1.12599154243361,1.16095164213714,1.17685574226388,
1.17917915286552,1.18040290371243,1.18141747464084,1.18268080075765,1.18511783643431,
1.20349893626503,1.22149443631757,1.24307009577738,1.24935689449321,1.25194300601702,
1.25380372500567,1.25549917215905,1.25820575250134,1.26478119621306,1.31031020571826,
1.32265634058214,1.32485719315882,1.32605508245878,1.32707145396758,1.32836675455236,
1.33044575510915,1.3426550143206,1.36815018997544,1.39012680899947,1.39540978244704,
1.39782386678021,1.39965605896793,1.40163761979861,1.40480551002242,1.4146607053459,
1.42229412958812,1.45359912969482,1.46807335298029,1.47035423351201,1.4715691418609,
1.47258425799189,1.47385817109101,1.47586635828403,1.48663455185492,1.4896662483066,
1.49249726537156,1.51493078383045,1.53027695283092,1.539414452834,1.54249483493583,
1.54445737325793,1.54629679572344,1.54875777245418,1.55430187765757,1.56186146207899,
1.58293176552634,1.61176482372921,1.61518699948736,1.61651638768316,1.61747468620137,
1.61852595728505,1.62005310375601,1.62408744207596,1.63017736529024,1.65120863598262,
1.68079438459942,1.68637268739585,1.68859338931337,1.6904442269639,1.69235013975978,
1.69516439833821,1.70299321625123,1.71498283316381,1.73443750721181,1.75705093740503,
1.76066437161217,1.76216918606104,1.76320562397846,1.76429856794156,1.76602209698975,
1.77158289560727,1.78110162991792,1.81063415071968,1.81946693363781,1.83015165068634,
1.83341301906289,1.83541489534002,1.8372406717015,1.83961003620665,1.84269843666847),
 .UNSPECIFIED.);
#1558=B_SPLINE_CURVE_WITH_KNOTS('',3,(#108440,#108441,#108442,#108443,#108444,
#108445,#108446,#108447,#108448,#108449,#108450,#108451,#108452,#108453,
#108454,#108455,#108456,#108457,#108458,#108459,#108460,#108461,#108462,
#108463,#108464,#108465,#108466,#108467,#108468,#108469,#108470,#108471,
#108472,#108473,#108474,#108475,#108476,#108477,#108478,#108479,#108480,
#108481,#108482,#108483,#108484,#108485,#108486,#108487,#108488,#108489,
#108490,#108491,#108492,#108493,#108494,#108495,#108496,#108497,#108498,
#108499,#108500,#108501,#108502,#108503,#108504,#108505,#108506,#108507,
#108508,#108509,#108510,#108511,#108512,#108513,#108514,#108515,#108516,
#108517,#108518,#108519,#108520,#108521,#108522,#108523,#108524,#108525,
#108526,#108527,#108528,#108529,#108530,#108531,#108532,#108533,#108534,
#108535,#108536,#108537,#108538,#108539,#108540,#108541,#108542,#108543,
#108544,#108545,#108546,#108547,#108548,#108549,#108550,#108551,#108552,
#108553,#108554,#108555,#108556,#108557,#108558,#108559,#108560,#108561,
#108562,#108563,#108564,#108565,#108566,#108567,#108568,#108569,#108570,
#108571,#108572,#108573,#108574,#108575,#108576,#108577,#108578,#108579,
#108580,#108581,#108582,#108583,#108584,#108585,#108586,#108587,#108588,
#108589,#108590,#108591,#108592,#108593,#108594,#108595,#108596,#108597,
#108598,#108599,#108600,#108601,#108602,#108603,#108604,#108605,#108606,
#108607,#108608,#108609,#108610,#108611,#108612,#108613,#108614,#108615,
#108616,#108617,#108618,#108619,#108620,#108621,#108622,#108623,#108624,
#108625,#108626,#108627,#108628,#108629,#108630,#108631,#108632,#108633,
#108634,#108635,#108636,#108637,#108638,#108639,#108640,#108641,#108642,
#108643,#108644,#108645,#108646,#108647,#108648,#108649,#108650,#108651,
#108652,#108653,#108654,#108655,#108656,#108657,#108658,#108659,#108660,
#108661),.UNSPECIFIED.,.F.,.F.,(4,2,2,2,2,2,2,2,2,2,2,2,2,2,2,2,2,2,2,2,
2,2,2,2,2,2,2,2,2,2,2,2,2,2,2,2,2,2,2,2,2,2,2,2,2,2,2,2,2,2,2,2,2,2,2,2,
2,2,2,2,2,2,2,2,2,2,2,2,2,2,2,2,2,2,2,2,2,2,2,2,2,2,2,2,2,2,2,2,2,2,2,2,
2,2,2,2,2,2,2,2,2,2,2,2,2,2,2,2,2,2,4),(0.92190171802025,0.925097910706482,
0.927084696020978,0.928913322374671,0.931310420781255,0.936506460788974,
0.957770258313368,0.973175329250713,0.983438581459966,0.987675120157475,
0.996629540026158,0.998716171406378,0.999901209099351,1.00091874235883,
1.00223071662206,1.00499115134119,1.00869107710742,1.0180788219129,1.04664205552107,
1.06617808787567,1.06967778928561,1.07193602825733,1.07375094123707,1.07582039705739,
1.07938621299087,1.09542457581823,1.11663680013027,1.13973400610314,1.14334084377314,
1.1446962004824,1.14566180113158,1.14670751565977,1.14820508355772,1.15204259320464,
1.15773686811606,1.17637540657759,1.20917025715405,1.21463650403762,1.21705734362094,
1.21889732206621,1.22085918985489,1.22393588001835,1.23394551071447,1.2510550158773,
1.2582421502029,1.28540020775133,1.28891275600559,1.29025528172181,1.29121699906627,
1.29226492984325,1.29377560286236,1.29770085892672,1.30357069906719,1.32324230488299,
1.35461883827749,1.35959943289312,1.3622793758212,1.36397023229319,1.36583575939953,
1.36844705828791,1.3748904134451,1.39447773337755,1.41469072131754,1.43260620022306,
1.43503697760918,1.43629902294411,1.43731372504564,1.43853906029758,1.44086913857483,
1.45700189907874,1.4934566391852,1.50393811228342,1.50717790998537,1.50917532561174,
1.51100283650529,1.51338278553973,1.51847989878641,1.53893111871115,1.56585252750646,
1.57836549495523,1.58045703992866,1.5817561783554,1.58277289272859,1.58396806217407,
1.58615622409197,1.59821129282421,1.63932058147671,1.64953330184663,1.65274241570116,
1.65473284787755,1.65656191819012,1.65895539784791,1.66412700780667,1.68518352170173,
1.71636277949963,1.72439866040462,1.72641292229441,1.72758191281659,1.72849976478118,
1.72978084749162,1.73190461240497,1.74724716617857,1.76640326878732,1.79352359501647,
1.79716146568833,1.79946075024912,1.80127830738836,1.80331863519332,1.80675518548761,
1.81087512618335,1.84317688118116),.UNSPECIFIED.);
#1559=B_SPLINE_CURVE_WITH_KNOTS('',3,(#108666,#108667,#108668,#108669,#108670,
#108671,#108672,#108673,#108674,#108675,#108676,#108677,#108678,#108679,
#108680,#108681,#108682,#108683,#108684,#108685,#108686,#108687,#108688,
#108689,#108690,#108691,#108692,#108693,#108694,#108695,#108696,#108697,
#108698,#108699,#108700,#108701,#108702,#108703,#108704,#108705,#108706,
#108707,#108708,#108709,#108710,#108711,#108712,#108713,#108714,#108715,
#108716,#108717,#108718,#108719,#108720,#108721,#108722,#108723,#108724,
#108725,#108726,#108727,#108728,#108729,#108730,#108731,#108732,#108733,
#108734,#108735,#108736,#108737,#108738,#108739,#108740,#108741,#108742,
#108743,#108744,#108745,#108746,#108747,#108748,#108749,#108750,#108751,
#108752,#108753,#108754,#108755,#108756,#108757,#108758,#108759,#108760,
#108761,#108762,#108763,#108764,#108765,#108766,#108767,#108768,#108769,
#108770,#108771,#108772,#108773,#108774,#108775,#108776,#108777,#108778,
#108779,#108780,#108781,#108782,#108783,#108784,#108785,#108786,#108787,
#108788,#108789,#108790,#108791,#108792,#108793,#108794,#108795,#108796,
#108797,#108798,#108799,#108800,#108801,#108802,#108803,#108804,#108805,
#108806,#108807,#108808,#108809,#108810,#108811,#108812,#108813,#108814,
#108815,#108816,#108817,#108818,#108819,#108820,#108821,#108822,#108823,
#108824,#108825,#108826,#108827,#108828,#108829,#108830,#108831,#108832,
#108833,#108834,#108835,#108836,#108837,#108838,#108839,#108840,#108841,
#108842,#108843,#108844,#108845,#108846,#108847,#108848,#108849,#108850,
#108851,#108852,#108853,#108854,#108855,#108856,#108857,#108858,#108859,
#108860,#108861,#108862,#108863,#108864,#108865,#108866,#108867,#108868,
#108869,#108870,#108871,#108872,#108873,#108874,#108875,#108876,#108877,
#108878,#108879,#108880,#108881,#108882,#108883,#108884,#108885,#108886,
#108887,#108888,#108889,#108890,#108891,#108892,#108893),.UNSPECIFIED.,
 .F.,.F.,(4,2,2,2,2,2,2,2,2,2,2,2,2,2,2,2,2,2,2,2,2,2,2,2,2,2,2,2,2,2,2,
2,2,2,2,2,2,2,2,2,2,2,2,2,2,2,2,2,2,2,2,2,2,2,2,2,2,2,2,2,2,2,2,2,2,2,2,
2,2,2,2,2,2,2,2,2,2,2,2,2,2,2,2,2,2,2,2,2,2,2,2,2,2,2,2,2,2,2,2,2,2,2,2,
2,2,2,2,2,2,2,2,2,2,4),(4.49376522957252E-6,0.0113749598956965,0.0134880192968926,
0.0148074797055664,0.0158105913397222,0.0168025881782626,0.0179570993091921,
0.0199588523548088,0.0275744334940921,0.0360676976962523,0.0572160554608524,
0.0784496470980371,0.0849223676533522,0.0875381455987711,0.0894043571962459,
0.0910941380961687,0.0933466673929254,0.0988936033675317,0.126711578100134,
0.15507441798845,0.158036127799285,0.159694246096322,0.161135006931926,
0.162159328346036,0.163123845402985,0.164477241892783,0.168074683343924,
0.192464336244554,0.216639861558587,0.224814997892535,0.230701699195563,
0.233221644257129,0.235070576775565,0.237011650843792,0.239993831612372,
0.248373108130774,0.282724568528582,0.30315163536191,0.305735969210109,
0.307013139536424,0.307930581823168,0.309102313519474,0.311128464198215,
0.31930797917579,0.327554693713002,0.35997370661674,0.374270283175109,0.377720789227907,
0.37976413006942,0.381581109297172,0.38387525716595,0.387496190613368,0.415890591675,
0.436204773794535,0.449272756508166,0.451502939303418,0.452706982936574,
0.453722661868401,0.455009545124361,0.457060891247674,0.468707123699906,
0.480836271109797,0.516828243065623,0.522093530004954,0.524504143723025,
0.526335580309462,0.528318145672917,0.531491623640803,0.541397178631337,
0.542970680625468,0.551183071007714,0.58068522568375,0.590195560937992,
0.595753192085045,0.597476286851616,0.598569096853285,0.599605380326054,
0.601110136357807,0.604724377492192,0.62732722199006,0.646761316862511,
0.658778929904398,0.666619693918354,0.669435117988138,0.671340922475368,
0.67319096938632,0.675409888769996,0.680979216055241,0.710960536998371,
0.731661901303821,0.737698859777822,0.741707139166819,0.743230138372334,
0.744280374734848,0.745239226719529,0.746571257485783,0.750011520669876,
0.778505048035367,0.80966618209178,0.813804912842453,0.815995537387778,
0.817629170845031,0.819683532644638,0.823184844153557,0.836310774560698,
0.877142334794315,0.883241525653986,0.887280458946217,0.888808027493967,
0.889859184779243,0.890817113530748,0.892145560971097,0.89556282049056,
0.921274759476541),.UNSPECIFIED.);
#1560=B_SPLINE_CURVE_WITH_KNOTS('',3,(#108895,#108896,#108897,#108898),
 .UNSPECIFIED.,.F.,.F.,(4,4),(1.84317688118116,1.84330550588385),
 .UNSPECIFIED.);
#1561=B_SPLINE_CURVE_WITH_KNOTS('',3,(#108899,#108900,#108901,#108902,#108903,
#108904,#108905,#108906,#108907,#108908,#108909,#108910,#108911,#108912,
#108913,#108914,#108915,#108916,#108917,#108918,#108919,#108920,#108921,
#108922,#108923,#108924,#108925,#108926,#108927,#108928,#108929,#108930,
#108931,#108932,#108933,#108934,#108935,#108936,#108937,#108938,#108939,
#108940,#108941,#108942,#108943,#108944,#108945,#108946,#108947,#108948,
#108949,#108950,#108951,#108952,#108953,#108954,#108955,#108956,#108957,
#108958,#108959,#108960,#108961,#108962,#108963,#108964,#108965,#108966,
#108967,#108968,#108969,#108970,#108971,#108972,#108973,#108974,#108975,
#108976,#108977,#108978,#108979,#108980,#108981,#108982,#108983,#108984,
#108985,#108986,#108987,#108988,#108989,#108990,#108991,#108992,#108993,
#108994,#108995,#108996,#108997,#108998,#108999,#109000,#109001,#109002,
#109003,#109004,#109005,#109006,#109007,#109008,#109009,#109010,#109011,
#109012,#109013,#109014,#109015,#109016,#109017,#109018,#109019,#109020,
#109021,#109022,#109023,#109024,#109025,#109026,#109027,#109028,#109029,
#109030,#109031,#109032,#109033,#109034,#109035,#109036,#109037,#109038,
#109039,#109040,#109041,#109042,#109043,#109044,#109045,#109046,#109047,
#109048,#109049,#109050,#109051,#109052,#109053,#109054,#109055,#109056,
#109057,#109058,#109059,#109060,#109061,#109062,#109063,#109064,#109065,
#109066,#109067,#109068,#109069,#109070,#109071,#109072,#109073,#109074,
#109075,#109076,#109077,#109078,#109079,#109080,#109081,#109082,#109083,
#109084,#109085,#109086,#109087,#109088,#109089,#109090,#109091,#109092,
#109093,#109094,#109095,#109096,#109097,#109098,#109099,#109100,#109101,
#109102,#109103,#109104,#109105,#109106,#109107,#109108,#109109,#109110,
#109111,#109112,#109113,#109114,#109115),.UNSPECIFIED.,.F.,.F.,(4,3,3,3,
3,3,3,3,3,3,3,3,3,3,3,3,3,3,3,3,3,3,3,3,3,3,3,3,3,3,3,3,3,3,3,3,3,3,3,3,
3,3,3,3,3,3,3,3,3,3,3,3,3,3,3,3,3,3,3,3,3,3,3,3,3,3,3,3,3,3,3,3,4),(13.68911242082,
13.8012112614014,13.8476634851164,13.8954754250497,13.8955135655797,13.999451658463,
14.008995850694,14.1222765446835,14.235445226898,14.3485466996653,14.461625665281,
14.5748085635747,14.6880430109893,14.801490990776,14.8880121102273,14.8880502488354,
14.9919884088926,15.0015323678574,15.1148128939076,15.2279814071832,15.3410827103216,
15.4541615059267,15.5673442349873,15.6805785133411,15.7940263264698,15.8805487922504,
15.880586932091,15.9845249283623,15.9940689917698,16.1073494559926,16.220517905967,
16.3336191444456,16.4466978741456,16.5598805358895,16.6731147460388,16.7865624903498,
16.8730854756924,16.8731236153467,16.9770616866453,16.9866057538221,17.099886298756,
17.2130548305512,17.3261561518109,17.4392349651043,17.5524177110341,17.6656520058279,
17.779099834481,17.8656221591762,17.8656602986024,17.9695983715848,17.9791424083181,
18.0924229240761,18.2055914264633,18.3186927181367,18.4317715017191,18.5449542179834,
18.6581884830913,18.7716362823968,18.8581588422516,18.8581969818581,18.9621350335285,
18.9716790865825,19.0849595970672,19.1981280940124,19.311229380085,19.4243081579174,
19.5374908682451,19.6507251273037,19.7641729204494,19.8506955255481,19.8507336651138,
19.9606220100522,19.9722977279996),.UNSPECIFIED.);
#1562=B_SPLINE_CURVE_WITH_KNOTS('',3,(#109120,#109121,#109122,#109123,#109124,
#109125,#109126,#109127,#109128,#109129,#109130,#109131,#109132,#109133,
#109134,#109135,#109136,#109137,#109138,#109139,#109140,#109141,#109142,
#109143,#109144,#109145,#109146,#109147,#109148,#109149,#109150,#109151,
#109152,#109153,#109154,#109155,#109156,#109157,#109158,#109159,#109160,
#109161,#109162,#109163,#109164,#109165,#109166,#109167,#109168,#109169,
#109170,#109171,#109172,#109173,#109174,#109175,#109176,#109177,#109178,
#109179,#109180,#109181,#109182,#109183,#109184,#109185,#109186,#109187,
#109188,#109189,#109190,#109191,#109192,#109193,#109194,#109195,#109196,
#109197,#109198,#109199,#109200,#109201,#109202,#109203,#109204,#109205,
#109206,#109207,#109208,#109209,#109210,#109211,#109212,#109213,#109214,
#109215,#109216,#109217,#109218,#109219,#109220,#109221,#109222,#109223,
#109224,#109225,#109226,#109227,#109228,#109229,#109230,#109231,#109232,
#109233,#109234,#109235,#109236,#109237,#109238,#109239,#109240,#109241,
#109242,#109243,#109244,#109245,#109246,#109247,#109248,#109249,#109250,
#109251,#109252,#109253,#109254,#109255,#109256,#109257,#109258,#109259,
#109260,#109261,#109262,#109263,#109264,#109265,#109266,#109267,#109268,
#109269,#109270,#109271,#109272,#109273,#109274,#109275,#109276,#109277,
#109278,#109279,#109280,#109281,#109282,#109283,#109284,#109285,#109286,
#109287,#109288,#109289,#109290,#109291,#109292,#109293,#109294,#109295,
#109296,#109297,#109298,#109299,#109300,#109301,#109302,#109303,#109304,
#109305,#109306,#109307,#109308,#109309,#109310,#109311,#109312,#109313,
#109314,#109315,#109316,#109317,#109318,#109319,#109320,#109321,#109322,
#109323,#109324,#109325,#109326,#109327,#109328,#109329,#109330,#109331,
#109332,#109333,#109334,#109335,#109336,#109337,#109338,#109339,#109340,
#109341,#109342,#109343,#109344,#109345,#109346,#109347,#109348,#109349,
#109350,#109351,#109352,#109353,#109354,#109355,#109356,#109357,#109358,
#109359,#109360,#109361,#109362,#109363,#109364,#109365,#109366,#109367,
#109368,#109369,#109370,#109371,#109372,#109373,#109374,#109375,#109376,
#109377),.UNSPECIFIED.,.F.,.F.,(4,2,2,2,2,2,2,2,2,2,2,2,2,2,2,2,2,2,2,2,
2,2,2,2,2,2,2,2,2,2,2,2,2,2,2,2,2,2,2,2,2,2,2,2,2,2,2,2,2,2,2,2,2,2,2,2,
2,2,2,2,2,2,2,2,2,2,2,2,2,2,2,2,2,2,2,2,2,2,2,2,2,2,2,2,2,2,2,2,2,2,2,2,
2,2,2,2,2,2,2,2,2,2,2,2,2,2,2,2,2,2,2,2,2,2,2,2,2,2,2,2,2,2,2,2,2,2,2,2,
4),(0.922139440865828,0.953161415715388,0.960070350467286,0.966684456462424,
0.974893849796186,0.983240001336062,0.985280283945809,0.986455441762326,
0.987372658490879,0.988645784439311,0.991208908371169,1.0165377107103,1.05031292538638,
1.05565375139298,1.05787146489727,1.05972153203008,1.06162841902405,1.06444745047457,
1.07231177019854,1.08437694587395,1.10375333853131,1.12632352907967,1.12993886186585,
1.1314439924651,1.13248052705378,1.13357358898686,1.13529706938882,1.14085570542365,
1.15036854728225,1.1798557258133,1.18740497453879,1.19920015955819,1.20258020649556,
1.20460835140601,1.20642847238205,1.2087493603968,1.21353550303919,1.23159331623799,
1.26211195449628,1.27398281603662,1.27604748238435,1.27733851605856,1.27835464359757,
1.27955588455904,1.28177228045122,1.29448592749055,1.31511396218002,1.34360777637861,
1.34723187230794,1.34952719116486,1.35134458534677,1.35338785267183,1.35683692442122,
1.37110761611683,1.40338692627428,1.41159532411027,1.4199426259377,1.42198289882,
1.42315799672873,1.42407513359945,1.42534810609123,1.42791077319943,1.45265599708845,
1.48708157408453,1.49244446000674,1.49484683517825,1.49668361576894,1.49865258852215,
1.50176269713238,1.51209197701971,1.53004901964931,1.55762230298695,1.56557556032801,
1.56758315935155,1.56875071076571,1.5696689337195,1.57095246361897,1.57356834085825,
1.5770218829926,1.61048168844067,1.6347604555478,1.63838350743291,1.64067839881354,
1.64249560152849,1.64453880845312,1.64798815508236,1.66226594370436,1.69458698710231,
1.71045749788657,1.71265232222996,1.71396793566005,1.71498820834799,1.71499796917578,
1.71500738331674,1.71501646633788,1.71502523288589,1.71503369678327,1.71504187112695,
1.7150497682493,1.71505739984063,1.71506477701247,1.71507191024131,1.71507880947977,
1.71508548416404,1.71509194327339,1.71509819529474,1.71510424831747,1.71511011006787,
1.71511578784317,1.71512128870614,1.71512661920111,1.7151317857507,1.71513815154595,
1.71514447543104,1.71515075816516,1.7163638142909,1.71860029211483,1.72150504753066,
1.72809902616017,1.74872291573315,1.77787840905959,1.78346175125323,1.78568304986354,
1.78753384311899,1.78943915203532,1.79225146421474,1.80006782415327,1.81203164969954,
1.84370254741232),.UNSPECIFIED.);
#1563=B_SPLINE_CURVE_WITH_KNOTS('',3,(#109378,#109379,#109380,#109381,#109382,
#109383,#109384,#109385,#109386,#109387,#109388,#109389,#109390,#109391,
#109392,#109393,#109394,#109395,#109396,#109397,#109398,#109399,#109400,
#109401,#109402,#109403,#109404,#109405,#109406,#109407,#109408,#109409,
#109410,#109411,#109412,#109413,#109414,#109415,#109416,#109417,#109418,
#109419,#109420,#109421,#109422,#109423,#109424,#109425,#109426,#109427,
#109428,#109429,#109430,#109431,#109432,#109433,#109434,#109435,#109436,
#109437,#109438,#109439,#109440,#109441,#109442,#109443,#109444,#109445,
#109446,#109447,#109448,#109449,#109450,#109451,#109452,#109453,#109454,
#109455,#109456,#109457,#109458,#109459,#109460,#109461,#109462,#109463,
#109464,#109465,#109466,#109467,#109468,#109469,#109470,#109471,#109472,
#109473,#109474,#109475,#109476,#109477,#109478,#109479,#109480,#109481,
#109482,#109483,#109484,#109485,#109486,#109487,#109488,#109489,#109490,
#109491,#109492,#109493,#109494,#109495,#109496,#109497,#109498,#109499,
#109500,#109501,#109502,#109503,#109504,#109505,#109506,#109507,#109508,
#109509,#109510,#109511,#109512,#109513,#109514,#109515,#109516,#109517,
#109518,#109519,#109520,#109521,#109522,#109523,#109524,#109525,#109526,
#109527,#109528,#109529,#109530,#109531,#109532,#109533,#109534,#109535,
#109536,#109537,#109538,#109539,#109540,#109541,#109542,#109543,#109544,
#109545,#109546,#109547,#109548,#109549),.UNSPECIFIED.,.F.,.F.,(4,3,3,3,
3,3,3,3,3,3,3,3,3,3,3,3,3,3,3,3,3,3,3,3,3,3,3,3,3,3,3,3,3,3,3,3,3,3,3,3,
3,3,3,3,3,3,3,3,3,3,3,3,3,3,3,3,3,4),(19.9723059855781,20.0841134945368,
20.1957886725539,20.3073787092846,20.4189306526368,20.5305707429868,20.6422527284484,
20.7541428742084,20.8432703483695,20.9567524590299,21.0700329756447,21.1832014788343,
21.2963027712539,21.4093815555251,21.5225642723825,21.6357985380314,21.749246337785,
21.8358070316252,21.9492891420776,22.0625696584554,22.1757381613903,22.2888394535383,
22.4019182375211,22.5151009540661,22.6283352193889,22.7417830187978,22.8283437148809,
22.9418258267259,23.0551063445343,23.1682748489219,23.281376142542,23.3944549280137,
23.5076376460622,23.6208719128987,23.7343197138193,23.8208803981366,23.9343625092453,
24.0476430263037,24.1608115299334,24.2739128227892,24.3869916074918,24.5001743247693,
24.6134085908326,24.7268563909863,24.8134170813922,24.9268991925426,25.0401797096401,
25.1533482133074,25.2664495061991,25.3795282909356,25.4927110082443,25.6059452743375,
25.7193930745179,25.8059537646479,25.9278422858354,26.0494238170588,26.1705511115848,
26.2554797039036),.UNSPECIFIED.);
#1564=B_SPLINE_CURVE_WITH_KNOTS('',3,(#109554,#109555,#109556,#109557,#109558,
#109559,#109560,#109561,#109562,#109563,#109564,#109565,#109566,#109567,
#109568,#109569,#109570,#109571,#109572,#109573,#109574,#109575,#109576,
#109577,#109578,#109579,#109580,#109581,#109582,#109583,#109584,#109585,
#109586,#109587,#109588,#109589,#109590,#109591,#109592,#109593,#109594,
#109595,#109596,#109597,#109598,#109599,#109600,#109601,#109602,#109603,
#109604,#109605,#109606,#109607,#109608,#109609,#109610,#109611,#109612,
#109613,#109614,#109615,#109616,#109617,#109618,#109619,#109620,#109621,
#109622,#109623,#109624,#109625,#109626,#109627,#109628,#109629,#109630,
#109631,#109632,#109633,#109634,#109635,#109636,#109637,#109638,#109639,
#109640,#109641,#109642,#109643,#109644,#109645,#109646,#109647,#109648,
#109649,#109650,#109651,#109652,#109653,#109654,#109655,#109656,#109657,
#109658,#109659,#109660,#109661,#109662,#109663,#109664,#109665,#109666,
#109667,#109668,#109669,#109670,#109671,#109672,#109673,#109674,#109675,
#109676,#109677,#109678,#109679,#109680,#109681,#109682,#109683,#109684,
#109685,#109686,#109687,#109688,#109689,#109690,#109691,#109692,#109693,
#109694,#109695,#109696,#109697,#109698,#109699,#109700,#109701,#109702,
#109703,#109704,#109705,#109706,#109707,#109708,#109709,#109710,#109711,
#109712,#109713,#109714,#109715,#109716,#109717,#109718,#109719,#109720,
#109721,#109722,#109723,#109724,#109725,#109726,#109727,#109728,#109729,
#109730,#109731,#109732,#109733,#109734,#109735,#109736,#109737,#109738,
#109739,#109740,#109741,#109742,#109743,#109744,#109745,#109746,#109747,
#109748,#109749,#109750,#109751,#109752,#109753,#109754,#109755,#109756,
#109757,#109758,#109759,#109760,#109761,#109762,#109763,#109764,#109765,
#109766,#109767,#109768,#109769),.UNSPECIFIED.,.F.,.F.,(4,2,2,2,2,2,2,2,
2,2,2,2,2,2,2,2,2,2,2,2,2,2,2,2,2,2,2,2,2,2,2,2,2,2,2,2,2,2,2,2,2,2,2,2,
2,2,2,2,2,2,2,2,2,2,2,2,2,2,2,2,2,2,2,2,2,2,2,2,2,2,2,2,2,2,2,2,2,2,2,2,
2,2,2,2,2,2,2,2,2,2,2,2,2,2,2,2,2,2,2,2,2,2,2,2,2,2,2,4),(0.000558712531683679,
0.0303543092442183,0.0344908609805544,0.0379383069450645,0.0399809976431443,
0.0417981159065078,0.0440934061081103,0.0477180648270099,0.0722622776020328,
0.0749869819963228,0.0997555196939848,0.109640744976087,0.111729543896498,
0.112929512132167,0.11394554448846,0.115237719811978,0.117306602474994,
0.129280893441805,0.16159069337941,0.173521456781318,0.181321319996906,
0.184131206610329,0.186035860048845,0.187886767504216,0.1901090998719,0.195700035767165,
0.224162151874238,0.251968646416803,0.256299670067604,0.257869230894463,
0.258928906962958,0.25987889161532,0.26117623583237,0.2644087444951,0.295713649201497,
0.315229233110872,0.326117443109647,0.329283463224686,0.331264382741658,
0.333096339254328,0.335469727156021,0.340672970701033,0.383827390725163,
0.400434348289794,0.4027761940494,0.404003857700441,0.405018374805607,0.406277533153869,
0.408695045569298,0.425465295124815,0.450301186885433,0.468800406273494,
0.473645282751628,0.475977321239594,0.477798535307081,0.479820042035368,
0.483170537760421,0.494674489184328,0.537285187064901,0.543472809813753,
0.547555230683006,0.549089351604343,0.550141931368141,0.551098731467874,
0.552422454238078,0.555810070167633,0.585506122805496,0.606010993961614,
0.613449518579923,0.61892458051788,0.621373251721448,0.623210667291422,
0.625177860060438,0.62827992972715,0.637591682420103,0.679744683552076,
0.691878018813171,0.694069754170991,0.695265748816941,0.696282408849505,
0.697580506452813,0.699668595383467,0.712092963746128,0.723610343399227,
0.741761877277822,0.755043043057593,0.760680444658789,0.765089551777033,
0.767336044012604,0.769149314631689,0.771225403452858,0.774732502138415,
0.788414230469905,0.821689367773794,0.837233277445426,0.839547220871354,
0.840769214118043,0.841784174592153,0.843050294866388,0.845499287333106,
0.865954505965287,0.894223465796298,0.907998020110397,0.911411386991672,
0.91344696693094,0.915265905747734,0.917574559839485,0.922139440865828),
 .UNSPECIFIED.);
#1565=B_SPLINE_CURVE_WITH_KNOTS('',3,(#109770,#109771,#109772,#109773,#109774,
#109775,#109776,#109777,#109778,#109779,#109780,#109781,#109782,#109783,
#109784,#109785,#109786,#109787,#109788,#109789,#109790,#109791,#109792,
#109793,#109794,#109795,#109796,#109797,#109798,#109799,#109800,#109801,
#109802,#109803,#109804,#109805,#109806,#109807,#109808,#109809,#109810,
#109811,#109812,#109813,#109814,#109815,#109816,#109817,#109818,#109819,
#109820,#109821,#109822,#109823,#109824,#109825,#109826,#109827,#109828,
#109829,#109830,#109831,#109832,#109833,#109834,#109835,#109836,#109837,
#109838,#109839,#109840,#109841,#109842,#109843,#109844,#109845,#109846,
#109847,#109848,#109849,#109850,#109851,#109852,#109853,#109854,#109855,
#109856,#109857,#109858,#109859,#109860,#109861,#109862,#109863,#109864,
#109865,#109866,#109867,#109868,#109869,#109870,#109871,#109872,#109873,
#109874,#109875,#109876,#109877,#109878,#109879,#109880,#109881,#109882,
#109883,#109884,#109885,#109886,#109887,#109888,#109889,#109890,#109891,
#109892,#109893,#109894,#109895,#109896,#109897,#109898,#109899,#109900,
#109901,#109902,#109903,#109904,#109905,#109906,#109907,#109908,#109909,
#109910,#109911,#109912,#109913,#109914,#109915,#109916,#109917,#109918,
#109919,#109920,#109921,#109922,#109923,#109924,#109925,#109926,#109927,
#109928,#109929,#109930,#109931,#109932,#109933,#109934,#109935,#109936,
#109937,#109938,#109939,#109940,#109941,#109942,#109943,#109944,#109945,
#109946,#109947,#109948,#109949,#109950,#109951,#109952,#109953,#109954,
#109955,#109956,#109957,#109958,#109959,#109960,#109961,#109962,#109963,
#109964,#109965,#109966,#109967,#109968,#109969,#109970,#109971,#109972,
#109973,#109974,#109975,#109976,#109977,#109978,#109979,#109980,#109981,
#109982,#109983,#109984,#109985),.UNSPECIFIED.,.F.,.F.,(4,2,2,2,2,2,2,2,
2,2,2,2,2,2,2,2,2,2,2,2,2,2,2,2,2,2,2,2,2,2,2,2,2,2,2,2,2,2,2,2,2,2,2,2,
2,2,2,2,2,2,2,2,2,2,2,2,2,2,2,2,2,2,2,2,2,2,2,2,2,2,2,2,2,2,2,2,2,2,2,2,
2,2,2,2,2,2,2,2,2,2,2,2,2,2,2,2,2,2,2,2,2,2,2,2,2,2,2,4),(0.000422182612240338,
0.00230014374216202,0.00418583338429343,0.00596491858417384,0.00771271525841758,
0.00944973154873033,0.0123777201742667,0.0203870933818239,0.0605627937106026,
0.0761168735771465,0.0784312785091729,0.0796534600410549,0.0806685514793024,
0.0819348271305579,0.0843841171858574,0.104382579937836,0.122576663950065,
0.145280999014369,0.148333427195791,0.150400475656218,0.152373182422382,
0.154111251266834,0.156408944585511,0.160039881871664,0.188059454648603,
0.208139706469626,0.221770721124928,0.22402290215518,0.22523194661011,0.226247751098447,
0.227529630869021,0.229563449268175,0.240844295685968,0.271961541449092,
0.285120828661717,0.290723548969139,0.295111332127361,0.297353697503326,
0.299150220770967,0.301223834663411,0.304719363941605,0.318295246109952,
0.351664099326014,0.367230453884055,0.369545235222495,0.370767506186816,
0.3717826090661,0.37304882042102,0.375497762863803,0.396202945752565,0.420874676465013,
0.437623398785895,0.441230235107616,0.443308258062966,0.445121673007081,
0.447366353046707,0.45082268889384,0.469222142535316,0.498781851827809,
0.508301678022971,0.513863814481442,0.515587939058819,0.516681321811511,
0.517718093990286,0.519223501774321,0.522838988897575,0.545441218887071,
0.5648714408073,0.576898257533913,0.584744207926846,0.587561166042227,0.58946793066542,
0.591318855504727,0.593538768786578,0.599110321217708,0.629067971135241,
0.655538209718973,0.659781068145504,0.661338661539975,0.662396231688496,
0.663348957744016,0.66465598920104,0.667943249240449,0.698920184128574,
0.718618903341301,0.729572069214626,0.732745430682947,0.734728589991012,
0.7365610307643,0.73893281469556,0.744123389930791,0.787185848366582,0.803911791764828,
0.806257447647684,0.807486269168103,0.808501274453993,0.809760479986267,
0.812176543038197,0.829045135785397,0.848700124576346,0.865507978362181,
0.875400958599596,0.878465684826659,0.880425334127053,0.88226703783853,
0.884695712748449,0.890204221494311,0.922002138176677),.UNSPECIFIED.);
#1566=B_SPLINE_CURVE_WITH_KNOTS('',3,(#109991,#109992,#109993,#109994,#109995,
#109996,#109997,#109998,#109999,#110000,#110001,#110002,#110003,#110004,
#110005,#110006,#110007,#110008,#110009,#110010,#110011,#110012,#110013,
#110014,#110015,#110016,#110017,#110018,#110019,#110020,#110021,#110022,
#110023,#110024,#110025,#110026,#110027,#110028,#110029,#110030,#110031,
#110032,#110033,#110034,#110035,#110036,#110037,#110038,#110039,#110040,
#110041,#110042,#110043,#110044,#110045,#110046,#110047,#110048,#110049,
#110050,#110051,#110052,#110053,#110054,#110055,#110056,#110057,#110058,
#110059,#110060,#110061,#110062,#110063,#110064,#110065,#110066,#110067,
#110068,#110069,#110070,#110071,#110072,#110073,#110074,#110075,#110076,
#110077,#110078,#110079,#110080,#110081,#110082,#110083,#110084,#110085,
#110086,#110087,#110088,#110089,#110090,#110091,#110092,#110093,#110094,
#110095,#110096,#110097,#110098,#110099,#110100,#110101,#110102,#110103,
#110104,#110105,#110106,#110107,#110108,#110109,#110110,#110111,#110112,
#110113,#110114,#110115,#110116,#110117,#110118,#110119,#110120,#110121,
#110122,#110123,#110124,#110125,#110126,#110127,#110128,#110129,#110130,
#110131,#110132,#110133,#110134,#110135,#110136,#110137,#110138,#110139,
#110140,#110141,#110142,#110143,#110144,#110145,#110146,#110147,#110148,
#110149,#110150,#110151,#110152,#110153,#110154,#110155,#110156,#110157,
#110158,#110159,#110160,#110161,#110162,#110163,#110164,#110165,#110166,
#110167,#110168,#110169,#110170,#110171,#110172,#110173,#110174,#110175,
#110176,#110177,#110178,#110179,#110180,#110181,#110182,#110183,#110184,
#110185,#110186,#110187,#110188,#110189,#110190,#110191,#110192,#110193,
#110194,#110195,#110196,#110197,#110198,#110199,#110200,#110201,#110202,
#110203,#110204,#110205,#110206,#110207,#110208,#110209,#110210,#110211,
#110212,#110213,#110214),.UNSPECIFIED.,.F.,.F.,(4,2,2,2,2,2,2,2,2,2,2,2,
2,2,2,2,2,2,2,2,2,2,2,2,2,2,2,2,2,2,2,2,2,2,2,2,2,2,2,2,2,2,2,2,2,2,2,2,
2,2,2,2,2,2,2,2,2,2,2,2,2,2,2,2,2,2,2,2,2,2,2,2,2,2,2,2,2,2,2,2,2,2,2,2,
2,2,2,2,2,2,2,2,2,2,2,2,2,2,2,2,2,2,2,2,2,2,2,2,2,2,2,4),(0.921845214926218,
0.933185665857156,0.935222172523389,0.936504811047572,0.937520568875029,
0.93872876108664,0.940977251501902,0.954508611584695,0.9746858515713,1.00275128291823,
1.00638423902856,1.00868241866071,1.01050035102992,1.01254240697938,1.01598502208849,
1.03015970943304,1.06193105216681,1.0651438398602,1.06804116180917,1.07882417672254,
1.08083336064094,1.08210772416984,1.08312306664836,1.08433808483189,1.08661875864089,
1.10107238885954,1.13228481038067,1.14030868481636,1.14997115109598,1.15311647643279,
1.15509335190042,1.15692764237122,1.15935401267431,1.16470319198419,1.18723475045186,
1.21014043551825,1.21406418367441,1.22443762180443,1.22642542353472,1.22769325366856,
1.22870828008019,1.22992878348522,1.23223563398876,1.24753160356075,1.28027254350274,
1.2946783120448,1.29823574932891,1.30032333808449,1.30213552196335,1.30436639474811,
1.30869856533483,1.33898418905266,1.36806827707569,1.37148173088947,1.37280979136644,
1.3737678006107,1.37481945540795,1.37634844367025,1.38039511824596,1.38651004616567,
1.42760127436187,1.44051355085667,1.44400010440247,1.44605156769803,1.44768605707324,
1.44988189646338,1.45404413600022,1.48365278438462,1.51376647404206,1.51712674083966,
1.51844584242256,1.51940148331546,1.52045534013953,1.52199564666969,1.52612004319726,
1.55091898885604,1.58280166889616,1.5877778859282,1.59045675373167,1.59214749492838,
1.59401335279707,1.59662597448919,1.60307703508295,1.62307231559871,1.64531813048479,
1.66084576219238,1.66303683438019,1.66435138813528,1.66537158163238,1.66654118571843,
1.66846205834106,1.67686343368966,1.69507012178042,1.72436877655217,1.73267275384419,
1.73564405921602,1.7375829769771,1.73943344469706,1.7419611656308,1.74760214046776,
1.76677122254198,1.78338583643667,1.79411356416013,1.80656626655906,1.80865522462919,
1.80995349650304,1.81097004575616,1.81216561218554,1.81344047394473,1.81544462514572,
1.8193297147383,1.84320204160076),.UNSPECIFIED.);
#1567=B_SPLINE_CURVE_WITH_KNOTS('',3,(#110215,#110216,#110217,#110218),
 .UNSPECIFIED.,.F.,.F.,(4,4),(0.000429300473710356,0.000558712531683679),
 .UNSPECIFIED.);
#1568=B_SPLINE_CURVE_WITH_KNOTS('',3,(#110219,#110220,#110221,#110222,#110223,
#110224,#110225,#110226,#110227,#110228,#110229,#110230,#110231,#110232,
#110233,#110234,#110235,#110236,#110237,#110238,#110239,#110240,#110241,
#110242,#110243,#110244,#110245,#110246,#110247,#110248,#110249,#110250,
#110251,#110252,#110253,#110254,#110255,#110256,#110257,#110258,#110259,
#110260,#110261,#110262,#110263,#110264,#110265,#110266,#110267,#110268,
#110269,#110270,#110271,#110272,#110273,#110274,#110275,#110276,#110277,
#110278,#110279,#110280,#110281,#110282,#110283,#110284,#110285,#110286,
#110287,#110288,#110289,#110290,#110291,#110292,#110293,#110294,#110295,
#110296,#110297,#110298,#110299,#110300,#110301,#110302,#110303,#110304,
#110305,#110306,#110307,#110308,#110309,#110310,#110311,#110312,#110313,
#110314,#110315,#110316,#110317,#110318,#110319,#110320,#110321,#110322,
#110323,#110324,#110325,#110326,#110327,#110328,#110329,#110330,#110331,
#110332,#110333,#110334,#110335,#110336,#110337,#110338,#110339,#110340,
#110341,#110342,#110343,#110344,#110345,#110346,#110347,#110348,#110349,
#110350,#110351,#110352,#110353,#110354,#110355,#110356,#110357,#110358,
#110359,#110360,#110361,#110362,#110363,#110364,#110365,#110366,#110367,
#110368,#110369,#110370,#110371,#110372,#110373,#110374,#110375,#110376,
#110377,#110378,#110379,#110380,#110381,#110382,#110383,#110384,#110385,
#110386,#110387,#110388,#110389,#110390,#110391,#110392,#110393,#110394,
#110395,#110396,#110397,#110398,#110399,#110400,#110401,#110402,#110403,
#110404,#110405,#110406,#110407,#110408,#110409,#110410,#110411,#110412,
#110413,#110414,#110415,#110416,#110417,#110418,#110419,#110420,#110421,
#110422,#110423,#110424,#110425,#110426,#110427,#110428,#110429,#110430,
#110431,#110432,#110433,#110434,#110435,#110436,#110437,#110438,#110439,
#110440,#110441,#110442,#110443,#110444,#110445,#110446,#110447,#110448,
#110449,#110450,#110451,#110452,#110453,#110454,#110455,#110456,#110457,
#110458,#110459,#110460,#110461,#110462,#110463,#110464,#110465,#110466,
#110467,#110468,#110469,#110470,#110471,#110472,#110473,#110474,#110475,
#110476,#110477,#110478,#110479,#110480,#110481,#110482,#110483,#110484,
#110485,#110486,#110487,#110488,#110489,#110490,#110491,#110492,#110493,
#110494),.UNSPECIFIED.,.F.,.F.,(4,2,2,2,2,2,2,2,2,2,2,2,2,2,2,2,2,2,2,2,
2,2,2,2,2,2,2,2,2,2,2,2,2,2,2,2,2,2,2,2,2,2,2,2,2,2,2,2,2,2,2,2,2,2,2,2,
2,2,2,2,2,2,2,2,2,2,2,2,2,2,2,2,2,2,2,2,2,2,2,2,2,2,2,2,2,2,2,2,2,2,2,2,
2,2,2,2,2,2,2,2,2,2,2,2,2,2,2,2,2,2,2,2,2,2,2,2,2,2,2,2,2,2,2,2,2,2,2,2,
2,2,2,2,2,2,2,2,2,4),(0.922002138176677,0.922131789127635,0.947522296073982,
0.951107738256752,0.95246009871606,0.953424698801019,0.954471051166437,
0.955971641903355,0.959827837521926,0.965558829801141,0.984405314838493,
1.01693479908309,1.02241727387269,1.02484141956543,1.02668239416404,1.02864386627924,
1.03171688262267,1.04168655480851,1.05869036494434,1.08403387757733,1.08547294910327,
1.09535537305435,1.09750584308617,1.09870630086103,1.09972293521332,1.10101614002484,
1.10367941441332,1.12564258133335,1.16317782650648,1.16822549582711,1.17057117842003,
1.17239989543567,1.1743955840034,1.17762575984179,1.18917875409744,1.22429053049902,
1.22664329023082,1.23051604783466,1.24091404874388,1.24290345746829,1.24417193480783,
1.24518722178763,1.24640775246314,1.24871389701591,1.26397302767487,1.29670077320765,
1.31114866054734,1.31470947035549,1.31679813453431,1.31861071051853,1.32084138108904,
1.32517098489071,1.35535253615668,1.38454718897717,1.38795678901901,1.38928441307581,
1.39024245632873,1.39129456816539,1.39282494946702,1.39687957342737,1.40301033806786,
1.44441098533032,1.45702200878654,1.46048904203517,1.46253654019901,1.4641720245021,
1.46637458813808,1.47056779749672,1.50294552046279,1.53001112150995,1.53353160456391,
1.53487545441299,1.535837703354,1.53688577356658,1.53839588895441,1.54231546557355,
1.54817330944218,1.56776889051933,1.59925863869765,1.60423667737684,1.60691637952539,
1.60860759241162,1.61047393050294,1.61308715706424,1.61953944245918,1.63957040158522,
1.65677472958376,1.67723508763838,1.67967792804942,1.68094281037152,1.68195784567911,
1.68196248270823,1.68196706191326,1.68197158408254,1.68197605008116,1.68198046070088,
1.681984816743,1.68198911896023,1.68199336813537,1.68199756508067,1.68200171046563,
1.68200580505263,1.68200984957442,1.68201384473938,1.6820177912015,1.68202168966647,
1.68202554083482,1.68202934537668,1.68203310397398,1.68203681723418,1.6820404857585,
1.68204411019473,1.68204769117382,1.68205122931632,1.68205472513393,1.68205817914971,
1.68330411708186,1.68575853186955,1.68897844193243,1.69663103748635,1.72203223564396,
1.74714377659505,1.75077373163496,1.75307107170837,1.75488901233754,1.75693179059308,
1.76037737167948,1.77459249516826,1.8070163579622,1.81559012311616,1.82354437268877,
1.82555239270934,1.82672023258885,1.82771964005603,1.82871836377646,1.83002418007741,
1.83210346497329,1.84352467432996),.UNSPECIFIED.);
#1569=B_SPLINE_CURVE_WITH_KNOTS('',3,(#110499,#110500,#110501,#110502,#110503,
#110504,#110505,#110506,#110507,#110508,#110509,#110510,#110511,#110512,
#110513,#110514,#110515,#110516,#110517,#110518,#110519,#110520,#110521,
#110522,#110523,#110524,#110525,#110526,#110527,#110528,#110529,#110530,
#110531,#110532,#110533,#110534,#110535,#110536,#110537,#110538,#110539,
#110540,#110541,#110542,#110543,#110544,#110545,#110546,#110547,#110548,
#110549,#110550,#110551,#110552,#110553,#110554,#110555,#110556,#110557,
#110558,#110559,#110560,#110561,#110562,#110563,#110564,#110565,#110566,
#110567,#110568,#110569,#110570,#110571,#110572,#110573,#110574,#110575,
#110576,#110577,#110578,#110579,#110580,#110581,#110582,#110583,#110584,
#110585,#110586,#110587,#110588,#110589,#110590,#110591,#110592,#110593,
#110594,#110595,#110596,#110597,#110598,#110599,#110600,#110601,#110602,
#110603,#110604,#110605,#110606,#110607,#110608,#110609,#110610,#110611,
#110612,#110613,#110614,#110615,#110616,#110617,#110618,#110619,#110620,
#110621,#110622,#110623,#110624,#110625,#110626,#110627,#110628,#110629,
#110630,#110631,#110632,#110633,#110634,#110635,#110636,#110637,#110638,
#110639,#110640,#110641,#110642,#110643,#110644,#110645,#110646,#110647,
#110648,#110649,#110650,#110651,#110652,#110653,#110654,#110655,#110656,
#110657,#110658,#110659,#110660,#110661,#110662,#110663,#110664,#110665,
#110666,#110667,#110668,#110669,#110670,#110671,#110672,#110673,#110674,
#110675,#110676,#110677,#110678,#110679,#110680,#110681,#110682,#110683,
#110684,#110685,#110686,#110687,#110688,#110689,#110690,#110691,#110692,
#110693,#110694,#110695,#110696,#110697,#110698,#110699,#110700,#110701,
#110702,#110703,#110704,#110705,#110706,#110707,#110708,#110709,#110710,
#110711,#110712,#110713,#110714,#110715,#110716,#110717,#110718),
 .UNSPECIFIED.,.F.,.F.,(4,2,2,2,2,2,2,2,2,2,2,2,2,2,2,2,2,2,2,2,2,2,2,2,
2,2,2,2,2,2,2,2,2,2,2,2,2,2,2,2,2,2,2,2,2,2,2,2,2,2,2,2,2,2,2,2,2,2,2,2,
2,2,2,2,2,2,2,2,2,2,2,2,2,2,2,2,2,2,2,2,2,2,2,2,2,2,2,2,2,2,2,2,2,2,2,2,
2,2,2,2,2,2,2,2,2,2,2,2,2,4),(0.000120839695703934,0.0455676436533427,0.0550891343698512,
0.0606516894268146,0.0623756015464489,0.0634687637408005,0.0645052426716709,
0.0660100725110365,0.0696231998186394,0.0922843274643028,0.11181783426619,
0.123748531195746,0.128991447536211,0.131947275537561,0.134467042128502,
0.136293290822903,0.138149296600383,0.140390278001579,0.145738393914182,
0.178654531865889,0.197203053008805,0.202881542233866,0.2067112609413,0.208207442141353,
0.209252673206656,0.21021779473239,0.211572961825374,0.215182553955673,
0.23798700617635,0.257775853028359,0.269464050009548,0.274634044129374,
0.278751377937892,0.280937964967913,0.28273092729656,0.284848010646145,
0.288535174696274,0.304835818766062,0.336246763738113,0.350751084457187,
0.353033153430974,0.354248397109868,0.355263621792299,0.356537457531062,
0.358545132791956,0.369300041246568,0.372381135434078,0.395793388673595,
0.41827561079411,0.423618630137956,0.426043807151103,0.427877834829059,
0.429855041135546,0.433002223332262,0.442681239081158,0.450642903751783,
0.481867211514867,0.496320526560074,0.498600961178106,0.49981587437733,
0.500831138839873,0.502105422197662,0.504114527114491,0.514896962037762,
0.517875751396225,0.520928015401863,0.546031917750097,0.564584962921893,
0.569437533974991,0.571771361674194,0.57359313080324,0.575614391328937,
0.578962458160321,0.590440704604357,0.633092956662107,0.639283455500257,
0.643367517919966,0.644902088369731,0.645954924471855,0.646911916654801,
0.648235851931401,0.651623728291181,0.68133551695141,0.686131394801075,
0.703281597658528,0.713306480015122,0.716385004602834,0.71834737432617,
0.720187349722236,0.722607486460359,0.72806905981282,0.760980090844152,
0.7795390932919,0.785219751408212,0.789050697621132,0.790547193121992,0.791592588955462,
0.792557818540408,0.79391307831307,0.797522445733084,0.820390828525827,
0.855884129541508,0.860702962130679,0.863030339422605,0.864851396346624,
0.866876307473201,0.870240868187866,0.881862739111313,0.886541005314974,
0.921845214926218),.UNSPECIFIED.);
#1570=B_SPLINE_CURVE_WITH_KNOTS('',3,(#110719,#110720,#110721,#110722,#110723,
#110724,#110725,#110726,#110727,#110728,#110729,#110730,#110731,#110732,
#110733,#110734,#110735,#110736,#110737,#110738,#110739,#110740,#110741,
#110742,#110743,#110744,#110745,#110746,#110747,#110748,#110749,#110750,
#110751,#110752,#110753,#110754,#110755,#110756,#110757,#110758,#110759,
#110760,#110761,#110762,#110763,#110764,#110765,#110766,#110767,#110768,
#110769,#110770,#110771,#110772,#110773,#110774,#110775,#110776,#110777,
#110778,#110779,#110780,#110781,#110782,#110783,#110784,#110785,#110786,
#110787,#110788,#110789,#110790,#110791,#110792,#110793,#110794,#110795,
#110796,#110797,#110798,#110799,#110800,#110801,#110802,#110803,#110804,
#110805,#110806,#110807,#110808,#110809,#110810,#110811,#110812,#110813,
#110814,#110815,#110816,#110817,#110818,#110819,#110820,#110821,#110822,
#110823,#110824,#110825,#110826,#110827,#110828,#110829,#110830,#110831,
#110832,#110833,#110834,#110835,#110836,#110837,#110838,#110839,#110840,
#110841,#110842,#110843,#110844,#110845,#110846,#110847,#110848,#110849,
#110850,#110851,#110852,#110853,#110854,#110855,#110856,#110857,#110858,
#110859,#110860,#110861,#110862,#110863,#110864,#110865,#110866,#110867,
#110868,#110869,#110870,#110871,#110872,#110873,#110874,#110875,#110876,
#110877,#110878,#110879,#110880,#110881,#110882,#110883,#110884,#110885,
#110886,#110887,#110888,#110889,#110890,#110891,#110892,#110893,#110894,
#110895,#110896,#110897,#110898,#110899,#110900,#110901,#110902,#110903,
#110904,#110905,#110906,#110907,#110908,#110909,#110910,#110911,#110912,
#110913,#110914,#110915,#110916,#110917,#110918,#110919,#110920,#110921,
#110922,#110923,#110924,#110925,#110926,#110927,#110928,#110929,#110930,
#110931,#110932,#110933,#110934,#110935,#110936,#110937,#110938,#110939,
#110940,#110941,#110942),.UNSPECIFIED.,.F.,.F.,(4,2,2,2,2,2,2,2,2,2,2,2,
2,2,2,2,2,2,2,2,2,2,2,2,2,2,2,2,2,2,2,2,2,2,2,2,2,2,2,2,2,2,2,2,2,2,2,2,
2,2,2,2,2,2,2,2,2,2,2,2,2,2,2,2,2,2,2,2,2,2,2,2,2,2,2,2,2,2,2,2,2,2,2,2,
2,2,2,2,2,2,2,2,2,2,2,2,2,2,2,2,2,2,2,2,2,2,2,2,2,2,2,4),(0.000514184320873031,
0.0322186784840785,0.0441938112098259,0.0520149769162336,0.0548282071910111,
0.0567339135113913,0.058584925666832,0.0608062843752995,0.0663887988403879,
0.0955079519483176,0.116131054964101,0.122725807482339,0.125630989791039,
0.127867940242788,0.129081184927655,0.129087469474058,0.129093795157261,
0.129100162687236,0.129105332954239,0.12911066715257,0.130125491655159,
0.131388692396932,0.133824279512369,0.152326042020472,0.169802716361319,
0.186945709428819,0.196967096278412,0.200045053451801,0.202007194759573,
0.203847055070414,0.20626719230246,0.211729485227269,0.244585891014861,
0.26316690063735,0.268850870124813,0.272683346994358,0.274180000660141,
0.275225365162193,0.276190464971353,0.277545422311956,0.281153050611057,
0.303754126726062,0.323167822089898,0.335205127653032,0.343055631141181,
0.345872903167848,0.347779507116791,0.349629992462675,0.351849037985281,
0.357416552826848,0.387516011876421,0.408126768213905,0.414149747937819,
0.418151385661808,0.419673682560489,0.420724016585175,0.421683429987472,
0.4230168767433,0.426464788019815,0.454854728526462,0.476229340216446,0.483852718275466,
0.489432482782446,0.491899872705768,0.493740452892699,0.495700825152586,
0.498770695782936,0.507824088981048,0.545879449196452,0.562164090828559,
0.564498207136595,0.565724453773425,0.566739303337916,0.568000770185634,
0.570428049355293,0.588063271096944,0.612153720068695,0.625518049369035,
0.631179069301836,0.635602774794257,0.637852301622535,0.63966591321271,
0.641740092682062,0.645238480806698,0.658855391131439,0.692183590060947,
0.707739687045261,0.710054043955779,0.711276173856409,0.712291207313562,
0.713557391756719,0.716006451735459,0.735899551618312,0.752289842697189,
0.76921558000163,0.779153668774858,0.782222909945432,0.784183305095312,
0.786024204184396,0.788449616088973,0.793941003574496,0.826223971212188,
0.845220450467257,0.850976582094028,0.854845481609915,0.856347829444499,
0.857394365138296,0.858358295379293,0.859708608442635,0.863279237442187,
0.889009418862205,0.92191958549341),.UNSPECIFIED.);
#1571=B_SPLINE_CURVE_WITH_KNOTS('',3,(#110947,#110948,#110949,#110950,#110951,
#110952,#110953,#110954,#110955,#110956,#110957,#110958,#110959,#110960,
#110961,#110962,#110963,#110964,#110965,#110966,#110967,#110968,#110969,
#110970,#110971,#110972,#110973,#110974,#110975,#110976,#110977,#110978,
#110979,#110980,#110981,#110982,#110983,#110984,#110985,#110986,#110987,
#110988,#110989,#110990,#110991,#110992,#110993,#110994,#110995,#110996,
#110997,#110998,#110999,#111000,#111001,#111002,#111003,#111004,#111005,
#111006,#111007,#111008,#111009,#111010,#111011,#111012,#111013,#111014,
#111015,#111016,#111017,#111018,#111019,#111020,#111021,#111022,#111023,
#111024,#111025,#111026,#111027,#111028,#111029,#111030,#111031,#111032,
#111033,#111034,#111035,#111036,#111037,#111038,#111039,#111040,#111041,
#111042,#111043,#111044,#111045,#111046,#111047,#111048,#111049,#111050,
#111051,#111052,#111053,#111054,#111055,#111056,#111057,#111058,#111059,
#111060,#111061,#111062,#111063,#111064,#111065,#111066,#111067,#111068,
#111069,#111070,#111071,#111072,#111073,#111074,#111075,#111076,#111077,
#111078,#111079,#111080,#111081,#111082,#111083,#111084,#111085,#111086,
#111087,#111088,#111089,#111090,#111091,#111092,#111093,#111094,#111095,
#111096,#111097,#111098,#111099,#111100,#111101,#111102,#111103,#111104,
#111105,#111106,#111107,#111108,#111109,#111110,#111111,#111112,#111113,
#111114,#111115,#111116,#111117,#111118,#111119,#111120,#111121,#111122,
#111123,#111124,#111125,#111126,#111127,#111128,#111129,#111130,#111131,
#111132,#111133,#111134,#111135,#111136,#111137,#111138,#111139,#111140,
#111141,#111142,#111143,#111144,#111145,#111146,#111147,#111148,#111149,
#111150,#111151,#111152,#111153,#111154,#111155,#111156,#111157,#111158,
#111159,#111160,#111161,#111162,#111163,#111164,#111165,#111166),
 .UNSPECIFIED.,.F.,.F.,(4,2,2,2,2,2,2,2,2,2,2,2,2,2,2,2,2,2,2,2,2,2,2,2,
2,2,2,2,2,2,2,2,2,2,2,2,2,2,2,2,2,2,2,2,2,2,2,2,2,2,2,2,2,2,2,2,2,2,2,2,
2,2,2,2,2,2,2,2,2,2,2,2,2,2,2,2,2,2,2,2,2,2,2,2,2,2,2,2,2,2,2,2,2,2,2,2,
2,2,2,2,2,2,2,2,2,2,2,2,2,4),(0.921832680523177,0.951032977161874,0.956613964824321,
0.958834794682953,0.960685376336237,0.962590651187675,0.965403259289845,
0.973222741326489,0.985193528648157,1.00466256949375,1.02728211220415,1.03089451980252,
1.03239901474863,1.03343526852322,1.03452819312185,1.03625174106495,1.04181307473724,
1.05133349189691,1.08088344459705,1.09930720423002,1.10276358497415,1.10500771165741,
1.10682030213161,1.10889696018903,1.11250033370256,1.12921009882921,1.15376467379925,
1.17459284352664,1.17704051120357,1.17830608984447,1.17932069367457,1.18054234675118,
1.18285589932244,1.19840529777989,1.23170540104789,1.24536155560679,1.2488659448375,
1.25094094518432,1.25275358269939,1.25499970212062,1.25940944287171,1.26504800019322,
1.27833484108479,1.29645189574596,1.3079441886255,1.3203662744993,1.32245360210224,
1.32375122682387,1.32476751161592,1.32596305047816,1.32815392955443,1.3402803704804,
1.38234634198735,1.39172955958175,1.39483971063103,1.39680814837065,1.39864403995622,
1.40108664199351,1.40653098971685,1.41391570893857,1.43417818860011,1.46419454084351,
1.46755899305462,1.46887846251745,1.46983390239858,1.47088698868382,1.47242524014894,
1.47653862276615,1.48279129753188,1.50489476827277,1.533078641905,1.53812330140673,
1.54081968306867,1.54251297446302,1.54437474523794,1.54696870701772,1.5533071112382,
1.57388359825824,1.59919005058039,1.61141087341261,1.61348962208528,1.61478457351595,
1.61580053022497,1.61699775292987,1.61919697917837,1.63152062131788,1.67666546494988,
1.68352406156949,1.68627876436677,1.6879823432206,1.68979762493318,1.69226298490438,
1.69502133739956,1.69976555012603,1.73494159340071,1.75667848637664,1.75912741496879,
1.76039299721527,1.76140725040061,1.76262805668367,1.76493884462942,1.78041538237603,
1.81943088951654,1.82839248411727,1.83144790437885,1.83340414316616,1.83514031364755,
1.8369292665996,1.83974263793472,1.8430958654942),.UNSPECIFIED.);
#1572=B_SPLINE_CURVE_WITH_KNOTS('',3,(#111167,#111168,#111169,#111170,#111171,
#111172,#111173,#111174,#111175,#111176,#111177,#111178,#111179,#111180,
#111181,#111182,#111183,#111184,#111185,#111186,#111187,#111188,#111189,
#111190,#111191,#111192,#111193,#111194,#111195,#111196,#111197,#111198,
#111199,#111200,#111201,#111202,#111203,#111204,#111205,#111206,#111207,
#111208,#111209,#111210,#111211,#111212,#111213,#111214,#111215,#111216,
#111217,#111218,#111219,#111220,#111221,#111222,#111223,#111224,#111225,
#111226,#111227,#111228,#111229,#111230,#111231,#111232,#111233,#111234,
#111235,#111236,#111237,#111238,#111239,#111240,#111241,#111242,#111243,
#111244,#111245,#111246,#111247,#111248,#111249,#111250,#111251,#111252,
#111253,#111254,#111255,#111256,#111257,#111258,#111259,#111260,#111261,
#111262,#111263,#111264,#111265,#111266,#111267,#111268,#111269,#111270,
#111271,#111272,#111273,#111274,#111275,#111276,#111277,#111278,#111279,
#111280,#111281,#111282,#111283,#111284,#111285,#111286,#111287,#111288,
#111289,#111290,#111291,#111292,#111293,#111294,#111295,#111296,#111297,
#111298,#111299,#111300,#111301,#111302,#111303,#111304,#111305,#111306,
#111307,#111308,#111309,#111310,#111311,#111312,#111313,#111314,#111315,
#111316,#111317,#111318,#111319,#111320,#111321,#111322,#111323,#111324,
#111325,#111326,#111327,#111328,#111329,#111330,#111331,#111332,#111333,
#111334,#111335,#111336,#111337,#111338,#111339,#111340,#111341,#111342,
#111343,#111344,#111345,#111346,#111347,#111348,#111349,#111350,#111351,
#111352,#111353,#111354,#111355,#111356,#111357,#111358,#111359,#111360,
#111361,#111362,#111363,#111364,#111365,#111366,#111367,#111368,#111369,
#111370,#111371,#111372,#111373,#111374,#111375,#111376,#111377,#111378,
#111379,#111380,#111381,#111382,#111383,#111384,#111385,#111386,#111387,
#111388),.UNSPECIFIED.,.F.,.F.,(4,2,2,2,2,2,2,2,2,2,2,2,2,2,2,2,2,2,2,2,
2,2,2,2,2,2,2,2,2,2,2,2,2,2,2,2,2,2,2,2,2,2,2,2,2,2,2,2,2,2,2,2,2,2,2,2,
2,2,2,2,2,2,2,2,2,2,2,2,2,2,2,2,2,2,2,2,2,2,2,2,2,2,2,2,2,2,2,2,2,2,2,2,
2,2,2,2,2,2,2,2,2,2,2,2,2,2,2,2,2,2,4),(0.92191958549341,0.926579367833769,
0.928875863602883,0.930693640011219,0.932736764118459,0.936184217644736,
0.95042734325079,0.982562959212838,0.990740527403718,0.999255938185879,
1.00131180928417,1.00249059598165,1.00349985597227,1.0048175583881,1.00760813821281,
1.01136016505699,1.02094585198147,1.04954070246114,1.06876593590375,1.0722541534795,
1.07450846860991,1.0763224809011,1.07839334864441,1.08196775281062,1.09816144265899,
1.13874778937986,1.14518890231943,1.14708014009456,1.14821055385572,1.1492413755653,
1.15065445406444,1.15397162347375,1.16954739234742,1.21221139447352,1.21745110001137,
1.21983165370702,1.22166528737793,1.22364421626648,1.22679880689785,1.23756332287219,
1.25672146928524,1.28857288534043,1.29176477119561,1.29305538694806,1.29400393063906,
1.2950661999706,1.296646940662,1.30105597602291,1.30792658851252,1.33309893351256,
1.35964455106454,1.36329439381451,1.36559766214912,1.36741612785572,1.36945512801421,
1.37288376923044,1.38686559866481,1.40321928976217,1.43395050049501,1.4372587269574,
1.43856919098321,1.43952270479107,1.44057911084322,1.44213151129411,1.44633885271029,
1.47230005894757,1.5028500438719,1.50840757959098,1.51062507526198,1.51247518831042,
1.51438236205098,1.51720228035824,1.52507231738369,1.53714975234297,1.55650603351655,
1.57906168074817,1.58267700494955,1.58418220527175,1.58521881170999,1.5863119908356,
1.58803575348555,1.59359622787261,1.6031136914262,1.63885803511642,1.65174357722761,
1.6552278030918,1.65727880182868,1.65891342369968,1.66111009559181,1.66527613918819,
1.6705231347409,1.6824671921474,1.71470754108742,1.71491367217198,1.72265956845524,
1.72773985981153,1.72946643764562,1.73045147511664,1.73148368286488,1.73290647421248,
1.73615990929275,1.75408663822514,1.7713270689301,1.79629775262752,1.79992631497513,
1.80222306527678,1.80404072239263,1.80608337483517,1.80952921207148,1.81366286783874,
1.84340367613644),.UNSPECIFIED.);
#1573=B_SPLINE_CURVE_WITH_KNOTS('',3,(#111393,#111394,#111395,#111396,#111397,
#111398,#111399,#111400,#111401,#111402,#111403,#111404,#111405,#111406,
#111407,#111408,#111409,#111410,#111411,#111412,#111413,#111414,#111415,
#111416,#111417,#111418,#111419,#111420,#111421,#111422,#111423,#111424,
#111425,#111426,#111427,#111428,#111429,#111430,#111431,#111432,#111433,
#111434,#111435,#111436,#111437,#111438,#111439,#111440,#111441,#111442,
#111443,#111444,#111445,#111446,#111447,#111448,#111449,#111450,#111451,
#111452,#111453,#111454,#111455,#111456,#111457,#111458,#111459,#111460,
#111461,#111462,#111463,#111464,#111465,#111466,#111467,#111468,#111469,
#111470,#111471,#111472,#111473,#111474,#111475,#111476,#111477,#111478,
#111479,#111480,#111481,#111482,#111483,#111484,#111485,#111486,#111487,
#111488,#111489,#111490,#111491,#111492,#111493,#111494,#111495,#111496,
#111497,#111498,#111499,#111500,#111501,#111502,#111503,#111504,#111505,
#111506,#111507,#111508,#111509,#111510,#111511,#111512,#111513,#111514,
#111515,#111516,#111517,#111518,#111519,#111520,#111521,#111522,#111523,
#111524,#111525,#111526,#111527,#111528,#111529,#111530,#111531,#111532,
#111533,#111534,#111535,#111536,#111537,#111538,#111539,#111540,#111541,
#111542,#111543,#111544,#111545,#111546,#111547,#111548,#111549,#111550,
#111551,#111552,#111553,#111554,#111555,#111556,#111557,#111558,#111559,
#111560,#111561,#111562,#111563,#111564,#111565,#111566,#111567,#111568,
#111569,#111570,#111571,#111572,#111573,#111574,#111575,#111576,#111577,
#111578,#111579,#111580,#111581,#111582,#111583,#111584,#111585,#111586,
#111587,#111588,#111589,#111590,#111591,#111592,#111593,#111594,#111595,
#111596,#111597,#111598,#111599,#111600,#111601,#111602,#111603,#111604,
#111605,#111606,#111607,#111608,#111609,#111610,#111611,#111612,#111613,
#111614,#111615,#111616,#111617,#111618,#111619,#111620,#111621,#111622),
 .UNSPECIFIED.,.F.,.F.,(4,2,2,2,2,2,2,2,2,2,2,2,2,2,2,2,2,2,2,2,2,2,2,2,
2,2,2,2,2,2,2,2,2,2,2,2,2,2,2,2,2,2,2,2,2,2,2,2,2,2,2,2,2,2,2,2,2,2,2,2,
2,2,2,2,2,2,2,2,2,2,2,2,2,2,2,2,2,2,2,2,2,2,2,2,2,2,2,2,2,2,2,2,2,2,2,2,
2,2,2,2,2,2,2,2,2,2,2,2,2,2,2,2,2,2,4),(0.000524403676282058,0.00751668207639485,
0.0113220917333589,0.0126923919885938,0.0137134438502507,0.0146856560546402,
0.0158024627757273,0.0176338610187251,0.0235572436620335,0.0317292774025957,
0.0629190299713805,0.0747436182064204,0.0824932672144701,0.0852963038193244,
0.087199523291428,0.0890514882090771,0.0912780477840168,0.0968959088845208,
0.124749431018032,0.153079850951266,0.156040153453738,0.157697703775962,
0.159139527547368,0.160163533982415,0.161128349344055,0.162482965147253,
0.166090118711053,0.188720406112024,0.208188857076231,0.220173763010725,
0.227999130920155,0.230812466176736,0.232717830737024,0.234568191449988,
0.236788378114272,0.242365757688715,0.271877414054598,0.292940725404047,
0.299034741160938,0.303071100156101,0.304598259348679,0.305649312720744,
0.306607289002639,0.307935985517641,0.31135494875589,0.340267299751136,
0.361293718415928,0.372691770276517,0.375906472201909,0.377898041870809,
0.379726599514782,0.382077088086457,0.387155123112346,0.424392673331689,
0.446555411305695,0.449222961363215,0.450516558468262,0.451532680444599,
0.452731539269522,0.454876778672273,0.464687314003478,0.469655157036567,
0.495011818239325,0.51512094469035,0.520174522354779,0.522546042046933,
0.524372094158481,0.526372895206465,0.529629405671474,0.54026954927466,
0.583854497357847,0.590085995000661,0.594189763049214,0.595726956857285,
0.596780110707899,0.597736229173265,0.599057445976145,0.602430473901178,
0.63236765908882,0.662143556569582,0.666309877185375,0.668506388529733,
0.670140751327125,0.672191244277325,0.675674142610747,0.68854877880188,
0.694838975016591,0.724288494827162,0.733791986315476,0.739346995755445,
0.741069891163162,0.742162718616861,0.743199139318214,0.744704276942378,
0.748320550696405,0.770885068432099,0.790249321996064,0.802335872082938,
0.810209181748124,0.813029139720641,0.814935997355287,0.816785536642284,
0.819002010700611,0.824555192305118,0.855207091332126,0.875403468583031,
0.881359477781386,0.885327824467106,0.886844938876926,0.88789408451025,
0.888854296170021,0.890191313290946,0.893664648804961,0.921702227342705,
0.921832680523177),.UNSPECIFIED.);
#1574=B_SPLINE_CURVE_WITH_KNOTS('',3,(#111624,#111625,#111626,#111627),
 .UNSPECIFIED.,.F.,.F.,(4,4),(1.84340367613644,1.84353373193666),
 .UNSPECIFIED.);
#1575=B_SPLINE_CURVE_WITH_KNOTS('',3,(#111628,#111629,#111630,#111631,#111632,
#111633,#111634,#111635,#111636,#111637,#111638,#111639,#111640,#111641,
#111642,#111643,#111644,#111645,#111646,#111647,#111648,#111649,#111650,
#111651,#111652,#111653,#111654,#111655,#111656,#111657,#111658,#111659,
#111660,#111661,#111662,#111663,#111664,#111665,#111666,#111667,#111668,
#111669,#111670,#111671,#111672,#111673,#111674,#111675,#111676,#111677,
#111678,#111679,#111680,#111681,#111682,#111683,#111684,#111685,#111686,
#111687,#111688,#111689,#111690,#111691,#111692,#111693,#111694,#111695,
#111696,#111697,#111698,#111699,#111700,#111701,#111702,#111703,#111704,
#111705,#111706,#111707,#111708,#111709,#111710,#111711,#111712,#111713,
#111714,#111715,#111716,#111717,#111718,#111719,#111720,#111721,#111722,
#111723,#111724,#111725,#111726,#111727,#111728,#111729,#111730,#111731,
#111732,#111733,#111734,#111735,#111736,#111737,#111738,#111739,#111740,
#111741,#111742,#111743,#111744,#111745,#111746,#111747,#111748,#111749,
#111750,#111751,#111752,#111753,#111754,#111755,#111756,#111757,#111758,
#111759,#111760,#111761,#111762,#111763,#111764,#111765,#111766,#111767,
#111768,#111769,#111770,#111771,#111772,#111773,#111774,#111775,#111776,
#111777,#111778,#111779,#111780,#111781,#111782,#111783,#111784,#111785,
#111786,#111787,#111788,#111789,#111790,#111791,#111792,#111793,#111794,
#111795,#111796,#111797,#111798,#111799,#111800,#111801,#111802,#111803,
#111804,#111805,#111806,#111807,#111808,#111809,#111810,#111811,#111812,
#111813,#111814,#111815,#111816,#111817,#111818,#111819,#111820,#111821,
#111822,#111823,#111824,#111825,#111826,#111827,#111828,#111829,#111830,
#111831,#111832,#111833,#111834,#111835,#111836,#111837,#111838,#111839,
#111840,#111841,#111842,#111843,#111844,#111845),.UNSPECIFIED.,.F.,.F.,
(4,2,2,2,2,2,2,2,2,2,2,2,2,2,2,2,2,2,2,2,2,2,2,2,2,2,2,2,2,2,2,2,2,2,2,
2,2,2,2,2,2,2,2,2,2,2,2,2,2,2,2,2,2,2,2,2,2,2,2,2,2,2,2,2,2,2,2,2,2,2,2,
2,2,2,2,2,2,2,2,2,2,2,2,2,2,2,2,2,2,2,2,2,2,2,2,2,2,2,2,2,2,2,2,2,2,2,2,
2,4),(6.16657166538228E-5,0.0272484328133284,0.0295142882092296,0.0308961787740782,
0.0321672258211346,0.0330842569284198,0.0342610005797047,0.0363081468226688,
0.0447109857495129,0.052916879077173,0.0609339267452389,0.085445441451452,
0.0992570511726005,0.102782524613097,0.104842676833897,0.106657902238045,
0.108927669001958,0.112466780138857,0.13318458533275,0.163691858774371,
0.174561965044177,0.176636047923632,0.177840886257816,0.178856890894084,
0.180143772371423,0.182194355555759,0.193821253099834,0.224553919283199,
0.237713117079223,0.243315641515315,0.2477032179675,0.24994541606699,0.251741776054048,
0.253815168820887,0.257310247523331,0.270883160262322,0.304250485817181,
0.31981577171664,0.322130349297808,0.32335250929215,0.324367518067532,0.325633609610802,
0.328082313427743,0.34881019951447,0.373465094409642,0.390203149026289,
0.393809136304438,0.395886854867423,0.397700112982985,0.399944739536755,
0.403401260434524,0.421811111267245,0.451357251626637,0.460874680061493,
0.46643568827762,0.468159584410237,0.469252850716743,0.470289536240179,
0.471794854164713,0.475410346273516,0.498002331568398,0.517416230753731,
0.529455715569027,0.537307413673667,0.540124983715762,0.542031752431276,
0.54388236964757,0.546101539610805,0.551669182782149,0.58178479423145,0.608109877493179,
0.612342555981929,0.613898611939505,0.614955799032749,0.615908691864993,
0.617216608921445,0.620509517806219,0.651422978089403,0.671156585611706,
0.682121419079166,0.685295721641037,0.687278968140453,0.689111150705318,
0.691482122990965,0.696668957248408,0.739753360501173,0.756457718122972,
0.758802667556837,0.760031273689142,0.761046188573503,0.76230539070731,
0.764721750732512,0.781632043115149,0.813105538538973,0.827221935277099,
0.830660582758489,0.832701886267296,0.834520144506229,0.836820089447146,
0.840458525941019,0.868476476245189,0.888588954351692,0.902177372020108,
0.904427982079159,0.905636687484879,0.906652507114882,0.907934786172863,
0.909969940583127,0.921279068844543),.UNSPECIFIED.);
#1576=B_SPLINE_CURVE_WITH_KNOTS('',3,(#111850,#111851,#111852,#111853,#111854,
#111855,#111856,#111857,#111858,#111859,#111860,#111861,#111862,#111863,
#111864,#111865,#111866,#111867,#111868,#111869,#111870,#111871,#111872,
#111873,#111874,#111875,#111876,#111877,#111878,#111879,#111880,#111881,
#111882,#111883,#111884,#111885,#111886,#111887,#111888,#111889,#111890,
#111891,#111892,#111893,#111894,#111895,#111896,#111897,#111898,#111899,
#111900,#111901,#111902,#111903,#111904,#111905,#111906,#111907,#111908,
#111909,#111910,#111911,#111912,#111913,#111914,#111915,#111916,#111917,
#111918,#111919,#111920,#111921,#111922,#111923,#111924,#111925,#111926,
#111927,#111928,#111929,#111930,#111931,#111932,#111933,#111934,#111935,
#111936,#111937,#111938,#111939,#111940,#111941,#111942,#111943,#111944,
#111945,#111946,#111947,#111948,#111949,#111950,#111951,#111952,#111953,
#111954,#111955,#111956,#111957,#111958,#111959,#111960,#111961,#111962,
#111963,#111964,#111965,#111966,#111967,#111968,#111969,#111970,#111971,
#111972,#111973,#111974,#111975,#111976,#111977,#111978,#111979,#111980,
#111981,#111982,#111983,#111984,#111985,#111986,#111987,#111988,#111989,
#111990,#111991,#111992,#111993,#111994,#111995,#111996,#111997,#111998,
#111999,#112000,#112001,#112002,#112003,#112004,#112005,#112006,#112007,
#112008,#112009,#112010,#112011,#112012,#112013,#112014,#112015,#112016,
#112017,#112018,#112019,#112020,#112021,#112022,#112023,#112024,#112025,
#112026,#112027,#112028,#112029,#112030,#112031,#112032,#112033,#112034,
#112035,#112036,#112037,#112038,#112039,#112040,#112041,#112042,#112043,
#112044,#112045,#112046,#112047,#112048,#112049,#112050,#112051,#112052,
#112053,#112054,#112055,#112056,#112057,#112058,#112059,#112060,#112061),
 .UNSPECIFIED.,.F.,.F.,(4,2,2,2,2,2,2,2,2,2,2,2,2,2,2,2,2,2,2,2,2,2,2,2,
2,2,2,2,2,2,2,2,2,2,2,2,2,2,2,2,2,2,2,2,2,2,2,2,2,2,2,2,2,2,2,2,2,2,2,2,
2,2,2,2,2,2,2,2,2,2,2,2,2,2,2,2,2,2,2,2,2,2,2,2,2,2,2,2,2,2,2,2,2,2,2,2,
2,2,2,2,2,2,2,2,2,4),(0.92204535995261,0.953944386918954,0.95987018790377,
0.979899530679955,0.982348226566923,0.983614213939935,0.984629078386282,
0.985850964698843,0.988164738546376,1.00370527446872,1.0369606799699,1.0506787967077,
1.0541883361554,1.05626483944438,1.05807783867503,1.06032317518575,1.06472733276008,
1.07035646215137,1.08360855261257,1.10177243604417,1.11316225765477,1.12570188762382,
1.12779442409456,1.1290937818792,1.13011042979398,1.13130523372803,1.13349182893139,
1.14551235879845,1.18616344411341,1.19679726504982,1.20005312598398,1.2020537874123,
1.20387988115381,1.20625169695481,1.21130686297429,1.23142674796299,1.25690697381001,
1.26148320533421,1.27149992836319,1.2736571738815,1.2748587430236,1.27587461632745,
1.27716465667964,1.27981412365994,1.3013243175951,1.33942839261513,1.3439067861149,
1.34619586496282,1.34789441269299,1.34975202242548,1.35232178109057,1.35850880797521,
1.36723559464952,1.39329615774988,1.4052861720004,1.41688831647583,1.41893689253544,
1.42022287959704,1.42123841319755,1.42244294109354,1.42467574219976,1.43781332829239,
1.45808324160008,1.48647647074121,1.49009267717621,1.49238526541735,1.49420192423637,
1.49624586939909,1.49969975128897,1.51404860004353,1.54676048641741,1.55085297813547,
1.56241799419245,1.56446463347913,1.56575004329047,1.56676555241938,1.56797056103585,
1.5702055808731,1.58340004545195,1.60362472831337,1.63200790695679,1.63562166863319,
1.6379135324401,1.63973013729049,1.64177457066557,1.64523061664596,1.65960986864042,
1.69248745629916,1.70769893000109,1.7098807215789,1.7111924133257,1.71221208110609,
1.7133595224369,1.71529799943006,1.71773545028386,1.72286731565794,1.73849076693741,
1.77587843886736,1.78087576261213,1.78324617375042,1.78507754755572,1.78705954114314,
1.7902310025642,1.8011771707635,1.82085894693048,1.84342048453855),
 .UNSPECIFIED.);
#1577=B_SPLINE_CURVE_WITH_KNOTS('',3,(#112062,#112063,#112064,#112065,#112066,
#112067,#112068,#112069,#112070,#112071,#112072,#112073,#112074,#112075,
#112076,#112077,#112078,#112079,#112080,#112081,#112082,#112083,#112084,
#112085,#112086,#112087,#112088,#112089,#112090,#112091,#112092,#112093,
#112094,#112095,#112096,#112097,#112098,#112099,#112100,#112101,#112102,
#112103,#112104,#112105,#112106,#112107,#112108,#112109,#112110,#112111,
#112112,#112113,#112114,#112115,#112116,#112117,#112118,#112119,#112120,
#112121,#112122,#112123,#112124,#112125,#112126,#112127,#112128,#112129,
#112130,#112131,#112132,#112133,#112134,#112135,#112136,#112137,#112138,
#112139,#112140,#112141,#112142,#112143,#112144,#112145,#112146,#112147,
#112148,#112149,#112150,#112151,#112152,#112153,#112154,#112155,#112156,
#112157,#112158,#112159,#112160,#112161,#112162,#112163,#112164,#112165,
#112166,#112167,#112168,#112169,#112170,#112171,#112172,#112173,#112174,
#112175,#112176,#112177,#112178,#112179,#112180,#112181,#112182,#112183,
#112184,#112185,#112186,#112187,#112188,#112189,#112190,#112191,#112192,
#112193,#112194,#112195,#112196,#112197,#112198,#112199,#112200,#112201,
#112202,#112203,#112204,#112205,#112206,#112207,#112208,#112209,#112210,
#112211,#112212,#112213,#112214,#112215,#112216,#112217,#112218,#112219,
#112220,#112221,#112222,#112223,#112224,#112225,#112226,#112227,#112228,
#112229,#112230,#112231,#112232,#112233,#112234,#112235,#112236,#112237,
#112238,#112239,#112240,#112241,#112242,#112243,#112244,#112245,#112246,
#112247,#112248,#112249,#112250,#112251,#112252,#112253,#112254,#112255,
#112256,#112257,#112258,#112259,#112260,#112261,#112262,#112263,#112264,
#112265,#112266,#112267,#112268,#112269,#112270,#112271,#112272,#112273,
#112274,#112275,#112276,#112277,#112278,#112279,#112280,#112281,#112282,
#112283,#112284,#112285,#112286,#112287,#112288,#112289,#112290,#112291,
#112292,#112293,#112294,#112295,#112296,#112297,#112298,#112299,#112300,
#112301,#112302,#112303,#112304,#112305),.UNSPECIFIED.,.F.,.F.,(4,2,2,2,
2,2,2,2,2,2,2,2,2,2,2,2,2,2,2,2,2,2,2,2,2,2,2,2,2,2,2,2,2,2,2,2,2,2,2,2,
2,2,2,2,2,2,2,2,2,2,2,2,2,2,2,2,2,2,2,2,2,2,2,2,2,2,2,2,2,2,2,2,2,2,2,2,
2,2,2,2,2,2,2,2,2,2,2,2,2,2,2,2,2,2,2,2,2,2,2,2,2,2,2,2,2,2,2,2,2,2,2,2,
2,2,2,2,2,2,2,2,2,4),(0.921279068844543,0.956298513554688,0.972293124115016,
0.975958448726816,0.978070747848119,0.979864192118253,0.982056965369928,
0.98620320628717,1.01623728703387,1.04590538699293,1.04929346749591,1.05061744920304,
1.05157446840378,1.05262733179809,1.05416196739572,1.05824633558653,1.06443816262797,
1.10710918758739,1.11857348029956,1.12191991583858,1.12394079928729,1.12576262055144,
1.12809706706528,1.13295301876023,1.15153109246506,1.17676829009808,1.1799894099863,
1.18261374519873,1.19337193667338,1.19537966756903,1.19665352372206,1.19766875354577,
1.19888400766024,1.20116613989136,1.21567133503768,1.24707561127836,1.26338550538756,
1.26707327250464,1.26919046688631,1.27098339386767,1.27316978410453,1.27728631379281,
1.28245473572016,1.29413751355348,1.31390617178286,1.3366914498755,1.34029951586951,
1.3416544286229,1.3426194628133,1.34366471016383,1.34516112579781,1.34899257446693,
1.35467521278871,1.3732490689044,1.40613629730528,1.41159771901257,1.41401756893816,
1.41585724376237,1.41781921977225,1.42089698861231,1.43091863512013,1.44806122807699,
1.45212210744402,1.48260802533421,1.4859372336422,1.48725109622952,1.48820537481963,
1.48926061103684,1.49080785619653,1.49498039784081,1.52045274305289,1.55155359264667,
1.55709279681286,1.55930716111682,1.56115627166095,1.56306407153006,1.56588805723009,
1.5737905558334,1.5859380868287,1.60521561199562,1.62772447703324,1.63134117722634,
1.63284641856937,1.63388290929275,1.63497582076077,1.63669890094147,1.64225490210686,
1.65176200066512,1.68121966167649,1.69973762996546,1.70319735337777,1.70544264900406,
1.70721130373004,1.70728093234482,1.70733928756684,1.70738865583322,1.70743074575989,
1.70746686300787,1.70749802435037,1.70752503447409,1.70754853921643,1.70756906325468,
1.70761035862912,1.70765059138038,1.7076898441727,1.70772819304422,1.70776570814694,
1.70780245438651,1.70994316417093,1.71236570111559,1.7162799518059,1.72411131713937,
1.76111023988633,1.76526865793287,1.77551277306454,1.77749335770848,1.77875887925639,
1.77977366884035,1.78099584671832,1.78331123888072,1.79891507005206,1.84269217962932),
 .UNSPECIFIED.);
#1578=B_SPLINE_CURVE_WITH_KNOTS('',3,(#112310,#112311,#112312,#112313,#112314,
#112315,#112316,#112317,#112318,#112319,#112320,#112321,#112322,#112323,
#112324,#112325,#112326,#112327,#112328,#112329,#112330,#112331,#112332,
#112333,#112334,#112335,#112336,#112337,#112338,#112339,#112340,#112341,
#112342,#112343,#112344,#112345,#112346,#112347,#112348,#112349,#112350,
#112351,#112352,#112353,#112354,#112355,#112356,#112357,#112358,#112359,
#112360,#112361,#112362,#112363,#112364,#112365,#112366,#112367,#112368,
#112369,#112370,#112371,#112372,#112373,#112374,#112375,#112376,#112377,
#112378,#112379,#112380,#112381,#112382,#112383,#112384,#112385,#112386,
#112387,#112388,#112389,#112390,#112391,#112392,#112393,#112394,#112395,
#112396,#112397,#112398,#112399,#112400,#112401,#112402,#112403,#112404,
#112405,#112406,#112407,#112408,#112409,#112410,#112411,#112412,#112413,
#112414,#112415,#112416,#112417,#112418,#112419,#112420,#112421,#112422,
#112423,#112424,#112425,#112426,#112427,#112428,#112429,#112430,#112431,
#112432,#112433,#112434,#112435,#112436,#112437,#112438,#112439,#112440,
#112441,#112442,#112443,#112444,#112445,#112446,#112447,#112448,#112449,
#112450,#112451,#112452,#112453,#112454,#112455,#112456,#112457,#112458,
#112459,#112460,#112461,#112462,#112463,#112464,#112465,#112466,#112467,
#112468,#112469,#112470,#112471,#112472,#112473,#112474,#112475,#112476,
#112477,#112478,#112479,#112480,#112481,#112482,#112483,#112484,#112485,
#112486,#112487,#112488,#112489,#112490,#112491,#112492,#112493,#112494,
#112495,#112496,#112497,#112498,#112499,#112500,#112501,#112502,#112503,
#112504,#112505,#112506,#112507,#112508,#112509,#112510,#112511,#112512,
#112513,#112514,#112515,#112516,#112517,#112518,#112519,#112520,#112521,
#112522,#112523,#112524,#112525,#112526,#112527,#112528,#112529,#112530,
#112531,#112532,#112533),.UNSPECIFIED.,.F.,.F.,(4,2,2,2,2,2,2,2,2,2,2,2,
2,2,2,2,2,2,2,2,2,2,2,2,2,2,2,2,2,2,2,2,2,2,2,2,2,2,2,2,2,2,2,2,2,2,2,2,
2,2,2,2,2,2,2,2,2,2,2,2,2,2,2,2,2,2,2,2,2,2,2,2,2,2,2,2,2,2,2,2,2,2,2,2,
2,2,2,2,2,2,2,2,2,2,2,2,2,2,2,2,2,2,2,2,2,2,2,2,2,2,2,4),(0.00042260572670247,
0.0301011163856895,0.0332807977237642,0.0353998883783552,0.0374424354602521,
0.039259591213873,0.0415551516259118,0.0451806803513619,0.0698369562847597,
0.0910803951690008,0.10676058206949,0.108894709803408,0.110189664572487,
0.111205885210203,0.112403725382788,0.114544450411237,0.124277673180439,
0.151505312701787,0.168328777751004,0.178197942834237,0.18127583918798,
0.183237594244121,0.185076843302523,0.187495806182267,0.192953773733776,
0.225877582550643,0.244412318308645,0.25008783254676,0.253915826739409,
0.255411532291323,0.256456496776942,0.257421425013085,0.258776391522564,
0.262386014025757,0.285138843196942,0.304841084080135,0.316604957621866,
0.324325912206559,0.327125111226344,0.329027599970107,0.330880288697055,
0.333109452982143,0.338743482302663,0.37603618460946,0.397358616537846,
0.40000275861588,0.401291803267086,0.402307678881092,0.403510169807019,
0.405671291415577,0.415748760984687,0.420254891991418,0.428803100862613,
0.435568472256776,0.467412103385173,0.471518126514989,0.473702117681862,
0.475335338683475,0.477395158773801,0.480920685395639,0.494354713695172,
0.527852304403676,0.543447612934405,0.545762620242868,0.546984679691504,
0.547999410415133,0.54926488815002,0.551711626907463,0.571095249558754,
0.591813168085176,0.611525065672801,0.616528377380245,0.618890600239986,
0.620715590692822,0.622721331930648,0.6259997661454,0.636842210744138,0.680203536013387,
0.686425579781325,0.690524846153533,0.692061475135762,0.693114589652801,
0.694070945117811,0.695392843578168,0.698769440841013,0.728658459991538,
0.733283861022475,0.750432957156993,0.760456792246902,0.763534842372239,
0.765496875372686,0.767336511036852,0.76975616594468,0.775216498756968,
0.808126358361383,0.826678621298388,0.832357661174859,0.836187616663424,
0.837683795815743,0.838728994093165,0.839694060120821,0.841049115496593,
0.844658140300783,0.867491768400454,0.887332640603449,0.898969602078717,
0.906630545277608,0.909421839881593,0.911322953809042,0.913177373116619,
0.915828015176426,0.92204535995261),.UNSPECIFIED.);
#1579=B_SPLINE_CURVE_WITH_KNOTS('',3,(#112534,#112535,#112536,#112537,#112538,
#112539,#112540,#112541,#112542,#112543,#112544,#112545,#112546,#112547,
#112548,#112549,#112550,#112551,#112552,#112553,#112554,#112555,#112556,
#112557,#112558,#112559,#112560,#112561,#112562,#112563,#112564,#112565,
#112566,#112567,#112568,#112569,#112570,#112571,#112572,#112573,#112574,
#112575,#112576,#112577,#112578,#112579,#112580,#112581,#112582,#112583,
#112584,#112585,#112586,#112587,#112588,#112589,#112590,#112591,#112592,
#112593,#112594,#112595,#112596,#112597,#112598,#112599,#112600,#112601,
#112602,#112603,#112604,#112605,#112606,#112607,#112608,#112609,#112610,
#112611,#112612,#112613,#112614,#112615,#112616,#112617,#112618,#112619,
#112620,#112621,#112622,#112623,#112624,#112625,#112626,#112627,#112628,
#112629,#112630,#112631,#112632,#112633,#112634,#112635,#112636,#112637,
#112638,#112639,#112640,#112641,#112642,#112643,#112644,#112645,#112646,
#112647,#112648,#112649,#112650,#112651,#112652,#112653,#112654,#112655,
#112656,#112657,#112658,#112659,#112660,#112661,#112662,#112663,#112664,
#112665,#112666,#112667,#112668,#112669,#112670,#112671,#112672,#112673,
#112674,#112675,#112676,#112677,#112678,#112679,#112680,#112681,#112682,
#112683,#112684,#112685,#112686,#112687,#112688,#112689,#112690,#112691,
#112692,#112693,#112694,#112695,#112696,#112697,#112698,#112699,#112700,
#112701,#112702,#112703,#112704,#112705,#112706,#112707,#112708,#112709,
#112710,#112711,#112712,#112713,#112714,#112715,#112716,#112717,#112718,
#112719,#112720,#112721,#112722,#112723,#112724,#112725,#112726,#112727,
#112728,#112729,#112730,#112731,#112732,#112733,#112734,#112735,#112736,
#112737,#112738,#112739,#112740,#112741,#112742,#112743,#112744,#112745,
#112746,#112747,#112748,#112749,#112750,#112751,#112752,#112753,#112754,
#112755,#112756,#112757),.UNSPECIFIED.,.F.,.F.,(4,2,2,2,2,2,2,2,2,2,2,2,
2,2,2,2,2,2,2,2,2,2,2,2,2,2,2,2,2,2,2,2,2,2,2,2,2,2,2,2,2,2,2,2,2,2,2,2,
2,2,2,2,2,2,2,2,2,2,2,2,2,2,2,2,2,2,2,2,2,2,2,2,2,2,2,2,2,2,2,2,2,2,2,2,
2,2,2,2,2,2,2,2,2,2,2,2,2,2,2,2,2,2,2,2,2,2,2,2,2,2,2,4),(0.000546165661636938,
0.00390012266971836,0.00678607654953448,0.00857512239891336,0.0103140173546196,
0.0122744325894094,0.0153440613668164,0.0244041487964937,0.0654579884993774,
0.0745317781892129,0.0781480578681155,0.0808599340831022,0.0821625136740359,
0.0831796991097723,0.084372843616601,0.0864915158746407,0.0958927265309324,
0.13416601876407,0.144214806203282,0.148873822036611,0.151598743997447,
0.154040525418751,0.155852718339705,0.157795392586238,0.160783012000645,
0.16920173840781,0.212406384429208,0.224612508426159,0.226807752462525,
0.228004653962178,0.22902147307387,0.230319013074906,0.232404771488569,
0.244766080215256,0.269855628021126,0.29203687762002,0.297344791587636,
0.299763868558389,0.301597266764204,0.303577642147319,0.306738233037307,
0.316526758408449,0.324281233702563,0.355554530919044,0.370021825276057,
0.372302999250273,0.373518204052623,0.374533658977692,0.375808138304257,
0.377817486901831,0.388600334413022,0.391569652345019,0.394634644336681,
0.426478646014624,0.440667623624168,0.444111495432347,0.446153953166104,
0.447972035265999,0.450270130576169,0.453902398958874,0.481939901522743,
0.502071770694074,0.515635062022503,0.517884763157456,0.519093281332932,
0.520109122729312,0.521391656299878,0.523427634409899,0.534753787615099,
0.565826598598347,0.578982723177383,0.584584540824968,0.588971767032186,
0.591214021205559,0.593010537723858,0.595084235740598,0.598580125854212,
0.612160842838273,0.645525333867422,0.661090655301423,0.663405409267278,
0.664627675296077,0.665642779546511,0.666908999451296,0.669357977861442,
0.690001954991413,0.714705191471345,0.73148086781269,0.73508922722716,0.737167582655402,
0.738980966940695,0.741225194526251,0.74468004587663,0.763043951053706,
0.792635525159949,0.802159826518154,0.807723774363526,0.809448103288884,
0.810541531955286,0.811578277737538,0.813083541352188,0.816698031446895,
0.839325433925569,0.858800634878303,0.870784839016698,0.878610751186036,
0.881425005868438,0.883331212624748,0.885182563605453,0.887404151786532,
0.892986273077319,0.922131836389314),.UNSPECIFIED.);
#1580=B_SPLINE_CURVE_WITH_KNOTS('',3,(#112762,#112763,#112764,#112765,#112766,
#112767,#112768,#112769,#112770,#112771,#112772,#112773,#112774,#112775,
#112776,#112777,#112778,#112779,#112780,#112781,#112782,#112783,#112784,
#112785,#112786,#112787,#112788,#112789,#112790,#112791,#112792,#112793,
#112794,#112795,#112796,#112797,#112798,#112799,#112800,#112801,#112802,
#112803,#112804,#112805,#112806,#112807,#112808,#112809,#112810,#112811,
#112812,#112813,#112814,#112815,#112816,#112817,#112818,#112819,#112820,
#112821,#112822,#112823,#112824,#112825,#112826,#112827,#112828,#112829,
#112830,#112831,#112832,#112833,#112834,#112835,#112836,#112837,#112838,
#112839,#112840,#112841,#112842,#112843,#112844,#112845,#112846,#112847,
#112848,#112849,#112850,#112851,#112852,#112853,#112854,#112855,#112856,
#112857,#112858,#112859,#112860,#112861,#112862,#112863,#112864,#112865,
#112866,#112867,#112868,#112869,#112870,#112871,#112872,#112873,#112874,
#112875,#112876,#112877,#112878,#112879,#112880,#112881,#112882,#112883,
#112884,#112885,#112886,#112887,#112888,#112889,#112890,#112891,#112892,
#112893,#112894,#112895,#112896,#112897,#112898,#112899,#112900,#112901,
#112902,#112903,#112904,#112905,#112906,#112907,#112908,#112909,#112910,
#112911,#112912,#112913,#112914,#112915,#112916,#112917,#112918,#112919,
#112920,#112921,#112922,#112923,#112924,#112925,#112926,#112927,#112928,
#112929,#112930,#112931,#112932,#112933),.UNSPECIFIED.,.F.,.F.,(4,3,3,3,
3,3,3,3,3,3,3,3,3,3,3,3,3,3,3,3,3,3,3,3,3,3,3,3,3,3,3,3,3,3,3,3,3,3,3,3,
3,3,3,3,3,3,3,3,3,3,3,3,3,3,3,3,3,4),(-79.4902472066036,-79.4029346604552,
-79.2894525492148,-79.1761720320241,-79.0630035282616,-78.949902235273,
-78.8368234504382,-78.7236407330294,-78.6104064668353,-78.4969586665535,
-78.4103979771995,-78.2969158659599,-78.1836353487699,-78.0704668450082,
-77.9573655520203,-77.8442867671862,-77.7311040497783,-77.617869783585,
-77.5044219833039,-77.4178612939438,-77.3043791827041,-77.191098665514,
-77.0779301617523,-76.9648288687643,-76.8517500839302,-76.7385673665221,
-76.6253331003288,-76.5118853000477,-76.4253246106881,-76.3118424994482,
-76.198561982258,-76.0853934784961,-75.9722921855081,-75.8592134006738,
-75.7460306832656,-75.6327964170721,-75.5193486167908,-75.4327879274324,
-75.3193058161927,-75.2060252990027,-75.0928567952409,-74.979755502253,
-74.8666767174189,-74.7534940000109,-74.6402597338175,-74.5268119335365,
-74.4402512441768,-74.326769132937,-74.2134886157468,-74.1003201119849,
-73.9872188189968,-73.8741400341625,-73.7609573167544,-73.6477230505609,
-73.5342752502797,-73.4477145609211,-73.29948869365,-73.2070626855824),
 .UNSPECIFIED.);
#1581=B_SPLINE_CURVE_WITH_KNOTS('',3,(#112934,#112935,#112936,#112937,#112938,
#112939,#112940,#112941,#112942,#112943,#112944,#112945,#112946,#112947,
#112948,#112949,#112950,#112951,#112952,#112953,#112954,#112955,#112956,
#112957,#112958,#112959,#112960,#112961,#112962,#112963,#112964,#112965,
#112966,#112967,#112968,#112969,#112970,#112971,#112972,#112973,#112974,
#112975,#112976,#112977,#112978,#112979,#112980,#112981,#112982,#112983,
#112984,#112985,#112986,#112987,#112988,#112989,#112990,#112991,#112992,
#112993,#112994,#112995,#112996,#112997,#112998,#112999,#113000,#113001,
#113002,#113003,#113004,#113005,#113006,#113007,#113008,#113009,#113010,
#113011,#113012,#113013,#113014,#113015,#113016,#113017,#113018,#113019,
#113020,#113021,#113022,#113023,#113024,#113025,#113026,#113027,#113028,
#113029,#113030,#113031,#113032,#113033,#113034,#113035,#113036,#113037,
#113038,#113039,#113040,#113041,#113042,#113043,#113044,#113045,#113046,
#113047,#113048,#113049,#113050,#113051,#113052,#113053,#113054,#113055,
#113056,#113057,#113058,#113059,#113060,#113061,#113062,#113063,#113064,
#113065,#113066,#113067,#113068,#113069,#113070,#113071,#113072,#113073,
#113074,#113075,#113076,#113077,#113078,#113079,#113080,#113081,#113082,
#113083,#113084,#113085,#113086,#113087,#113088,#113089,#113090,#113091,
#113092,#113093,#113094,#113095,#113096,#113097,#113098,#113099,#113100,
#113101,#113102,#113103,#113104,#113105,#113106,#113107,#113108,#113109,
#113110,#113111,#113112,#113113,#113114,#113115,#113116,#113117,#113118,
#113119,#113120,#113121,#113122,#113123,#113124,#113125,#113126,#113127,
#113128,#113129,#113130,#113131,#113132,#113133,#113134,#113135,#113136,
#113137,#113138,#113139,#113140,#113141,#113142,#113143,#113144,#113145,
#113146,#113147,#113148,#113149,#113150,#113151,#113152,#113153,#113154,
#113155,#113156,#113157,#113158,#113159,#113160,#113161,#113162,#113163,
#113164,#113165,#113166,#113167,#113168,#113169,#113170,#113171,#113172,
#113173,#113174,#113175,#113176,#113177,#113178,#113179,#113180,#113181,
#113182,#113183,#113184,#113185,#113186,#113187,#113188,#113189,#113190,
#113191,#113192,#113193,#113194,#113195,#113196,#113197,#113198,#113199,
#113200,#113201,#113202,#113203,#113204,#113205,#113206,#113207,#113208,
#113209,#113210,#113211,#113212,#113213,#113214,#113215,#113216,#113217,
#113218,#113219,#113220,#113221,#113222,#113223,#113224,#113225,#113226,
#113227,#113228,#113229,#113230,#113231,#113232,#113233,#113234,#113235,
#113236,#113237,#113238,#113239,#113240,#113241,#113242,#113243,#113244,
#113245,#113246,#113247,#113248,#113249,#113250,#113251,#113252,#113253),
 .UNSPECIFIED.,.F.,.F.,(4,2,2,2,2,2,2,2,2,2,2,2,2,2,2,2,2,2,2,2,2,2,2,2,
2,2,2,2,2,2,2,2,2,2,2,2,2,2,2,2,2,2,2,2,2,2,2,2,2,2,2,2,2,2,2,2,2,2,2,2,
2,2,2,2,2,2,2,2,2,2,2,2,2,2,2,2,2,2,2,2,2,2,2,2,2,2,2,2,2,2,2,2,2,2,2,2,
2,2,2,2,2,2,2,2,2,2,2,2,2,2,2,2,2,2,2,2,2,2,2,2,2,2,2,2,2,2,2,2,2,2,2,2,
2,2,2,2,2,2,2,2,2,2,2,2,2,2,2,2,2,2,2,2,2,2,2,2,2,2,2,4),(0.922131836389314,
0.922262170085757,0.950341467134868,0.953812250201056,0.955149235641928,
0.956109698770761,0.957159441304046,0.958677984828669,0.962653258221853,
0.968623082936937,0.988898476370587,1.0194771585668,1.025035006869,1.02725278454895,
1.02910319328668,1.03101073401772,1.03383131248837,1.0417039792166,1.05378620317461,
1.07314302761759,1.09570100249777,1.09931702588588,1.10082249837379,1.10185928713487,
1.10295265336059,1.10467670178362,1.1102380172569,1.11975682410213,1.14928555259909,
1.1580687781151,1.16879530833217,1.17206200219198,1.17406560146509,1.1758919456092,
1.17826062777076,1.18329579101754,1.20325027346598,1.22677310948163,1.22919221591622,
1.2331184869178,1.24348767733223,1.24547536566065,1.24674323280732,1.24775837102777,
1.2489791303374,1.25128681669362,1.26660629154333,1.29932926019654,1.3137175956732,
1.31727403479016,1.31936153458299,1.32117394901371,1.32340550551232,1.32774032121055,
1.35810790355764,1.38708877082697,1.39050536028061,1.39183400845851,1.39279223837166,
1.39384391125911,1.39537257278968,1.39941637160345,1.40552534915469,1.4465091621457,
1.45951469761285,1.46300724388953,1.46506015984343,1.46669467559132,1.46888909806894,
1.47304380537896,1.47827268162891,1.49015584363016,1.50971629540219,1.53239096713076,
1.53599802882937,1.53735287296186,1.5383179313917,1.53936328802267,1.54085999656315,
1.54469293152849,1.55037838201038,1.56896735546875,1.60183747171693,1.60730030490129,
1.6097205060333,1.61156034047385,1.613522383322,1.61660003991939,1.62661931240597,
1.64375508150689,1.6651238541587,1.6798235291184,1.68198585395234,1.6832920578398,
1.68431139056386,1.68431750783836,1.68432354536141,1.68432950428872,1.6843353857784,
1.68434119097933,1.6843469210309,1.68435257705015,1.68435816010519,1.68436367127825,
1.68436911162005,1.68437448215374,1.68437978389931,1.68438501787452,1.68439018510243,
1.68439528649927,1.68440032301204,1.68440529561369,1.684410205242,1.68441505277351,
1.68441983915181,1.68442456520982,1.68442923183469,1.68443383989028,1.68443839017334,
1.6844428835534,1.68444732087386,1.68445170288335,1.6844560303425,1.68446030407582,
1.68446452481658,1.68446869332439,1.68447281030495,1.68447687654171,1.6844808927455,
1.68448485957552,1.68448877771987,1.68449264786284,1.68449647069641,1.68450024689281,
1.68450397708628,1.68450766192792,1.68451130202242,1.68574041043262,1.6881477946098,
1.69128835708962,1.6986691312011,1.71464550614072,1.74734205824822,1.75281341739043,
1.75523502857482,1.75707500900258,1.75903631674563,1.76211095147079,1.77210313640312,
1.78916893192169,1.81240495080333,1.82055865454026,1.82636921980636,1.82818757998944,
1.82930162500055,1.83027254324325,1.83129553930595,1.83267092143667,1.83644440740643,
1.84342118748583),.UNSPECIFIED.);
#1582=B_SPLINE_CURVE_WITH_KNOTS('',3,(#113258,#113259,#113260,#113261,#113262,
#113263,#113264,#113265,#113266,#113267,#113268,#113269,#113270,#113271,
#113272,#113273,#113274,#113275,#113276,#113277,#113278,#113279,#113280,
#113281,#113282,#113283,#113284,#113285,#113286,#113287,#113288,#113289,
#113290,#113291,#113292,#113293,#113294,#113295,#113296,#113297,#113298,
#113299,#113300,#113301,#113302,#113303,#113304,#113305,#113306,#113307,
#113308,#113309,#113310,#113311,#113312,#113313,#113314,#113315,#113316,
#113317,#113318,#113319,#113320,#113321,#113322,#113323,#113324,#113325,
#113326,#113327,#113328,#113329,#113330,#113331,#113332,#113333,#113334,
#113335,#113336,#113337,#113338,#113339,#113340,#113341,#113342,#113343,
#113344,#113345,#113346,#113347,#113348,#113349,#113350,#113351,#113352,
#113353,#113354,#113355,#113356,#113357,#113358,#113359,#113360,#113361,
#113362,#113363,#113364,#113365,#113366,#113367,#113368,#113369,#113370,
#113371,#113372,#113373,#113374,#113375,#113376,#113377,#113378,#113379,
#113380,#113381,#113382,#113383,#113384,#113385,#113386,#113387,#113388,
#113389,#113390,#113391,#113392,#113393,#113394,#113395,#113396,#113397,
#113398,#113399,#113400,#113401,#113402,#113403,#113404,#113405,#113406,
#113407,#113408,#113409,#113410,#113411,#113412,#113413,#113414,#113415,
#113416,#113417,#113418,#113419,#113420,#113421,#113422,#113423,#113424,
#113425,#113426,#113427,#113428,#113429,#113430,#113431,#113432,#113433,
#113434,#113435,#113436,#113437,#113438,#113439,#113440,#113441,#113442,
#113443,#113444,#113445,#113446,#113447,#113448,#113449,#113450,#113451,
#113452,#113453,#113454,#113455,#113456,#113457,#113458,#113459,#113460,
#113461,#113462,#113463,#113464,#113465,#113466,#113467,#113468,#113469,
#113470,#113471,#113472,#113473),.UNSPECIFIED.,.F.,.F.,(4,2,2,2,2,2,2,2,
2,2,2,2,2,2,2,2,2,2,2,2,2,2,2,2,2,2,2,2,2,2,2,2,2,2,2,2,2,2,2,2,2,2,2,2,
2,2,2,2,2,2,2,2,2,2,2,2,2,2,2,2,2,2,2,2,2,2,2,2,2,2,2,2,2,2,2,2,2,2,2,2,
2,2,2,2,2,2,2,2,2,2,2,2,2,2,2,2,2,2,2,2,2,2,2,2,2,2,2,4),(0.921591759352823,
0.932451005728724,0.953455716143075,0.976366610203934,0.979973856661162,
0.981328530542062,0.982293408389913,0.98333849006221,0.984834651001523,
0.98866532264372,0.994346592496436,1.01291284055534,1.04582056293844,1.05128137950628,
1.0537009066155,1.05554030536603,1.05750195193745,1.06057911763692,1.07059771434119,
1.08773255977227,1.09276592323988,1.12219662123457,1.12559555911193,1.12692105028923,
1.12787822561133,1.12893015530899,1.13046154554138,1.13452622632648,1.140678471259,
1.18253560637163,1.19473328878941,1.19815099541947,1.20018702757227,1.20182321982764,
1.20403965530232,1.20830358123231,1.23651008554497,1.26803172634206,1.27125844314878,
1.27255474745746,1.2735044368065,1.27456433436741,1.27613518384404,1.28047580165399,
1.30843253218351,1.33674420380591,1.34234076145022,1.3445638848493,1.34641488861363,
1.34831907072948,1.35112719227294,1.35891516738066,1.37081971445205,1.39035465771498,
1.41300937740942,1.41662003002663,1.41797499925442,1.41893985315528,1.41998464297692,
1.42147994921742,1.42530607778609,1.43097866844299,1.44949767356734,1.48246192319825,
1.48791848245317,1.49033701187813,1.49217600038074,1.49413754481196,1.49721525473794,
1.50724214597301,1.5244001585312,1.52709087482143,1.55780841084992,1.56194937799989,
1.56354002047432,1.56449821992207,1.56554883718642,1.56707422736817,1.57109931492969,
1.57717122925508,1.59809381032237,1.62780648546837,1.63338109654358,1.63560069821129,
1.63745075749925,1.63935600930224,1.64216955366867,1.64999809192461,1.66198887788377,
1.68143276138344,1.70403778883264,1.70764762054688,1.70900244786616,1.70996724045918,
1.71099119132066,1.71241772273805,1.7140658269906,1.71700202569571,1.72369975207093,
1.74763392170442,1.77573293633916,1.77935625475289,1.7816509178983,1.78346769024987,
1.78551015034461,1.78895759645335,1.80321740618225,1.84292101011832),
 .UNSPECIFIED.);
#1583=B_SPLINE_CURVE_WITH_KNOTS('',3,(#113474,#113475,#113476,#113477,#113478,
#113479,#113480,#113481,#113482,#113483,#113484,#113485,#113486,#113487,
#113488,#113489,#113490,#113491,#113492,#113493,#113494,#113495,#113496,
#113497,#113498,#113499,#113500,#113501,#113502,#113503,#113504,#113505,
#113506,#113507,#113508,#113509,#113510,#113511,#113512,#113513,#113514,
#113515,#113516,#113517,#113518,#113519,#113520,#113521,#113522,#113523,
#113524,#113525,#113526,#113527,#113528,#113529,#113530,#113531,#113532,
#113533,#113534,#113535,#113536,#113537,#113538,#113539,#113540,#113541,
#113542,#113543,#113544,#113545,#113546,#113547,#113548,#113549,#113550,
#113551,#113552,#113553,#113554,#113555,#113556,#113557,#113558,#113559,
#113560,#113561,#113562,#113563,#113564,#113565,#113566,#113567,#113568,
#113569,#113570,#113571,#113572,#113573,#113574,#113575,#113576,#113577,
#113578,#113579,#113580,#113581,#113582,#113583,#113584,#113585,#113586,
#113587,#113588,#113589,#113590,#113591,#113592,#113593,#113594,#113595,
#113596,#113597,#113598,#113599,#113600,#113601,#113602,#113603,#113604,
#113605,#113606,#113607,#113608,#113609,#113610,#113611,#113612,#113613,
#113614,#113615,#113616,#113617,#113618,#113619,#113620,#113621,#113622,
#113623,#113624,#113625,#113626,#113627,#113628,#113629,#113630,#113631,
#113632,#113633,#113634,#113635,#113636,#113637,#113638,#113639,#113640,
#113641,#113642,#113643,#113644,#113645,#113646,#113647,#113648,#113649,
#113650,#113651,#113652,#113653,#113654,#113655,#113656,#113657,#113658,
#113659,#113660,#113661,#113662,#113663,#113664,#113665,#113666,#113667,
#113668,#113669,#113670,#113671,#113672,#113673,#113674,#113675,#113676,
#113677,#113678,#113679,#113680,#113681,#113682,#113683,#113684,#113685,
#113686,#113687),.UNSPECIFIED.,.F.,.F.,(4,2,2,2,2,2,2,2,2,2,2,2,2,2,2,2,
2,2,2,2,2,2,2,2,2,2,2,2,2,2,2,2,2,2,2,2,2,2,2,2,2,2,2,2,2,2,2,2,2,2,2,2,
2,2,2,2,2,2,2,2,2,2,2,2,2,2,2,2,2,2,2,2,2,2,2,2,2,2,2,2,2,2,2,2,2,2,2,2,
2,2,2,2,2,2,2,2,2,2,2,2,2,2,2,2,2,2,4),(0.000109611860504862,0.0263881269654468,
0.0435355614439316,0.05355865834799,0.0566368023303898,0.0585989868178459,
0.0604388344481837,0.0628588775380518,0.06832061865916,0.10118776293088,
0.119761227349136,0.125443884151263,0.128062432820324,0.130118113203203,
0.131291991293629,0.132237584239197,0.133496730428177,0.135913359114828,
0.152383169061244,0.171898129053717,0.189060586675483,0.199089603391258,
0.2021684736055,0.204130876260641,0.205970757037948,0.208390594030031,0.213850776542714,
0.246753661562792,0.265303706951211,0.270982385116381,0.274812239740323,
0.276308533428512,0.277353866726805,0.278319114893321,0.279674517853826,
0.283285229677594,0.30638543868713,0.326162905717372,0.343554159226471,
0.347195952955449,0.349281436196038,0.351093955951958,0.353328018428925,
0.35675004901375,0.37436254188906,0.375459878242077,0.404811731646641,0.418851115055208,
0.421117652001306,0.422329674552825,0.423345186629057,0.42462316751018,
0.42664431291382,0.437666477644309,0.467986780511056,0.486994421913833,
0.491906945612887,0.494252276864854,0.496075483284056,0.498090671467135,
0.501410864631099,0.512632538612934,0.555559075955423,0.561761480576038,
0.565851324352278,0.567386772688519,0.568439812674461,0.569396689789914,
0.570720090588666,0.5741046203883,0.603858723941073,0.624323149828154,0.631753289757296,
0.637223847627348,0.639672092902816,0.641509823203909,0.64347795940623,
0.646582817594577,0.655913247034108,0.693651877372063,0.709912694420683,
0.712246415318246,0.713472665446473,0.714487638078821,0.715749407588215,
0.718177689593712,0.735863212713659,0.740573903105931,0.754394197357368,
0.771390049077395,0.781355536111029,0.784427909282053,0.786389102053476,
0.788229905384577,0.790653957208334,0.796136832279431,0.828613414878864,
0.847474370630639,0.853207423647724,0.857064816567798,0.858565484998126,
0.859611768832566,0.860576204130791,0.86192820743607,0.865511464295706,
0.890768502812618,0.921587349549934),.UNSPECIFIED.);
#1584=B_SPLINE_CURVE_WITH_KNOTS('',3,(#113692,#113693,#113694,#113695,#113696,
#113697,#113698,#113699,#113700,#113701,#113702,#113703,#113704,#113705,
#113706,#113707,#113708,#113709,#113710,#113711,#113712,#113713,#113714,
#113715,#113716,#113717,#113718,#113719,#113720,#113721,#113722,#113723,
#113724,#113725,#113726,#113727,#113728,#113729,#113730,#113731,#113732,
#113733,#113734,#113735,#113736,#113737,#113738,#113739,#113740,#113741,
#113742,#113743,#113744,#113745,#113746,#113747,#113748,#113749,#113750,
#113751,#113752,#113753,#113754,#113755,#113756,#113757,#113758,#113759,
#113760,#113761,#113762,#113763,#113764,#113765,#113766,#113767,#113768,
#113769,#113770,#113771,#113772,#113773,#113774,#113775,#113776,#113777,
#113778,#113779,#113780,#113781,#113782,#113783,#113784,#113785,#113786,
#113787,#113788,#113789,#113790,#113791,#113792,#113793,#113794,#113795,
#113796,#113797,#113798,#113799,#113800,#113801,#113802,#113803,#113804,
#113805,#113806,#113807,#113808,#113809,#113810,#113811,#113812,#113813,
#113814,#113815,#113816,#113817,#113818,#113819,#113820,#113821,#113822,
#113823,#113824,#113825,#113826,#113827,#113828,#113829,#113830,#113831,
#113832,#113833,#113834,#113835,#113836,#113837,#113838,#113839,#113840,
#113841,#113842,#113843,#113844,#113845,#113846,#113847,#113848,#113849,
#113850,#113851,#113852,#113853,#113854,#113855,#113856,#113857,#113858,
#113859,#113860,#113861,#113862,#113863,#113864,#113865,#113866,#113867,
#113868,#113869,#113870,#113871,#113872,#113873,#113874,#113875,#113876,
#113877,#113878,#113879,#113880,#113881,#113882,#113883,#113884,#113885,
#113886,#113887,#113888,#113889,#113890,#113891,#113892,#113893,#113894,
#113895,#113896,#113897,#113898,#113899,#113900,#113901,#113902,#113903,
#113904,#113905,#113906,#113907,#113908,#113909,#113910,#113911,#113912,
#113913,#113914,#113915),.UNSPECIFIED.,.F.,.F.,(4,2,2,2,2,2,2,2,2,2,2,2,
2,2,2,2,2,2,2,2,2,2,2,2,2,2,2,2,2,2,2,2,2,2,2,2,2,2,2,2,2,2,2,2,2,2,2,2,
2,2,2,2,2,2,2,2,2,2,2,2,2,2,2,2,2,2,2,2,2,2,2,2,2,2,2,2,2,2,2,2,2,2,2,2,
2,2,2,2,2,2,2,2,2,2,2,2,2,2,2,2,2,2,2,2,2,2,2,2,2,2,2,4),(0.000198811978866998,
0.0283954862359279,0.0316064030563364,0.0337383934111708,0.0357899693485767,
0.037605746168362,0.0398869767492998,0.043465054483826,0.0654303190957778,
0.081868406265388,0.103907372436054,0.106998195689001,0.10839254961266,
0.109420124828639,0.110558297245092,0.112486020649799,0.119303202645729,
0.146043418971801,0.16551955789568,0.172730562032024,0.178035166075126,
0.180475409689357,0.182311305189635,0.184281436606099,0.187397871729397,
0.196828281741222,0.234658021191554,0.250705431602909,0.253032813560649,
0.254257436305559,0.255272026881879,0.256534500806897,0.258967438645604,
0.280964180518072,0.303881875848621,0.321067887211414,0.324697946598246,
0.326780502490072,0.328592687424683,0.330829166362182,0.334260221371775,
0.3520911173789,0.382155354095163,0.391746709178854,0.395500034649312,0.398291351545985,
0.399608941551679,0.400617907413173,0.401796073379795,0.403850243884671,
0.412348503765858,0.420538281671264,0.452699786764226,0.46694790159021,
0.470395009521909,0.472437626159877,0.474254756471682,0.476550166981768,
0.48017522471286,0.508236868600793,0.528404846999591,0.537522573748585,
0.541150237274782,0.54386853254242,0.545172029626903,0.546188895566675,
0.547380436326399,0.549493378571925,0.558817362874415,0.564597320336818,
0.589718467821813,0.609799901134509,0.614849991996206,0.617220866594573,
0.619046841783186,0.621047976847007,0.624305977322694,0.634959865571651,
0.671218027920972,0.687323957967042,0.689652915735876,0.69087787503871,
0.691892463541422,0.693154584731581,0.695585856638271,0.717747344927057,
0.731804901637097,0.748794254131461,0.7587562650741,0.761827466987194,0.763787870036349,
0.765627896862348,0.76805086713259,0.773530982511415,0.806036067956404,
0.824872579154355,0.830600733020784,0.834455321437375,0.835955187772594,
0.837001003623189,0.837965067660832,0.839316615826241,0.842899179995747,
0.868121171148966,0.891692063341524,0.899753690052054,0.905577873637375,
0.908087288679488,0.909934512291451,0.911646912218673,0.91444625202759,
0.921591759352823),.UNSPECIFIED.);
#1585=B_SPLINE_CURVE_WITH_KNOTS('',3,(#113916,#113917,#113918,#113919,#113920,
#113921,#113922,#113923,#113924,#113925,#113926,#113927,#113928,#113929,
#113930,#113931,#113932,#113933,#113934,#113935,#113936,#113937,#113938,
#113939,#113940,#113941,#113942,#113943,#113944,#113945,#113946,#113947,
#113948,#113949,#113950,#113951,#113952,#113953,#113954,#113955,#113956,
#113957,#113958,#113959,#113960,#113961,#113962,#113963,#113964,#113965,
#113966,#113967,#113968,#113969,#113970,#113971,#113972,#113973,#113974,
#113975,#113976,#113977,#113978,#113979,#113980,#113981,#113982,#113983,
#113984,#113985,#113986,#113987,#113988,#113989,#113990,#113991,#113992,
#113993,#113994,#113995,#113996,#113997,#113998,#113999,#114000,#114001,
#114002,#114003,#114004,#114005,#114006,#114007,#114008,#114009,#114010,
#114011,#114012,#114013,#114014,#114015,#114016,#114017,#114018,#114019,
#114020,#114021,#114022,#114023,#114024,#114025,#114026,#114027,#114028,
#114029,#114030,#114031,#114032,#114033,#114034,#114035,#114036,#114037,
#114038,#114039,#114040,#114041,#114042,#114043,#114044,#114045,#114046,
#114047,#114048,#114049,#114050,#114051,#114052,#114053,#114054,#114055,
#114056,#114057,#114058,#114059,#114060,#114061,#114062,#114063,#114064,
#114065,#114066,#114067,#114068,#114069,#114070,#114071,#114072,#114073,
#114074,#114075,#114076,#114077,#114078,#114079,#114080,#114081,#114082,
#114083,#114084,#114085,#114086,#114087,#114088,#114089,#114090,#114091,
#114092,#114093,#114094,#114095,#114096,#114097,#114098,#114099,#114100,
#114101,#114102,#114103,#114104,#114105,#114106,#114107,#114108,#114109,
#114110,#114111,#114112,#114113,#114114,#114115,#114116,#114117,#114118,
#114119,#114120,#114121,#114122,#114123,#114124,#114125,#114126,#114127,
#114128,#114129,#114130,#114131,#114132,#114133,#114134,#114135,#114136,
#114137,#114138,#114139,#114140,#114141,#114142,#114143,#114144,#114145,
#114146,#114147),.UNSPECIFIED.,.F.,.F.,(4,2,2,2,2,2,2,2,2,2,2,2,2,2,2,2,
2,2,2,2,2,2,2,2,2,2,2,2,2,2,2,2,2,2,2,2,2,2,2,2,2,2,2,2,2,2,2,2,2,2,2,2,
2,2,2,2,2,2,2,2,2,2,2,2,2,2,2,2,2,2,2,2,2,2,2,2,2,2,2,2,2,2,2,2,2,2,2,2,
2,2,2,2,2,2,2,2,2,2,2,2,2,2,2,2,2,2,2,2,2,2,2,2,2,2,2,4),(0.921587349549934,
0.927848225935604,0.930506277226033,0.932362447347461,0.934262485923268,
0.937046879929529,0.944654855764119,0.956179016031914,0.976119790601808,
0.999006551264362,1.00261456202173,1.00396967205066,1.00493489843658,1.00598041264886,
1.0074773067909,1.01131050110182,1.01699615802948,1.035584068137,1.0684698968529,
1.07393010396914,1.07635007763632,1.07819010589254,1.08015270860964,1.08323198522045,
1.09326339944928,1.11042939241382,1.11266517609307,1.14230289420144,1.14762851318991,
1.14938739959065,1.15048843423817,1.15153264398836,1.15302269607578,1.15681177358933,
1.16241022530834,1.18050437146567,1.21408716609722,1.21897125945152,1.22162582581713,
1.22348126351797,1.22538197732328,1.22817000982117,1.2358049578323,1.24738566784906,
1.26726622894608,1.29011751618152,1.29372554012558,1.29508060502706,1.29604578740718,
1.29709124048293,1.29858802495532,1.30242081896593,1.30810578354821,1.32669046885014,
1.35957297963994,1.36503593453121,1.36745631431699,1.36929633342315,1.37125862023852,
1.37433675828564,1.38435851182503,1.40149978109816,1.40594514061497,1.43600950766017,
1.43937274097984,1.44069246176694,1.44164835177349,1.44270226206602,1.44424229536991,
1.44836390839828,1.47312325424737,1.50506461958148,1.51057216431694,1.51300031006199,
1.51484156620911,1.51680069573309,1.51986452081341,1.52975399654812,1.54655307288848,
1.56840301909368,1.57443744472218,1.58358301609946,1.58568424907112,1.58687334031403,
1.58789083302052,1.58919868265825,1.5919382733352,1.59560247100879,1.60485626607495,
1.63730049474235,1.65344709160116,1.65712271521926,1.65923722018338,1.66103036315293,
1.66322008699196,1.6673523124602,1.6725455388567,1.68431024001991,1.71487739838729,
1.7184002204474,1.7289625314812,1.73096019601263,1.73223100474799,1.73324612002173,
1.73446400565934,1.73675854429256,1.75162318622948,1.77365622565695,1.79843617363865,
1.80206351893953,1.80435992119323,1.80617756819158,1.80822048854086,1.81033983962556,
1.81351963797243,1.84313775771039),.UNSPECIFIED.);
#1586=B_SPLINE_CURVE_WITH_KNOTS('',3,(#114153,#114154,#114155,#114156,#114157,
#114158,#114159,#114160,#114161,#114162,#114163,#114164,#114165,#114166,
#114167,#114168,#114169,#114170,#114171,#114172,#114173,#114174,#114175,
#114176,#114177,#114178,#114179,#114180,#114181,#114182,#114183,#114184,
#114185,#114186,#114187,#114188,#114189,#114190,#114191,#114192,#114193,
#114194,#114195,#114196,#114197,#114198,#114199,#114200,#114201,#114202,
#114203,#114204,#114205,#114206,#114207,#114208,#114209,#114210,#114211,
#114212,#114213,#114214,#114215,#114216,#114217,#114218,#114219,#114220,
#114221,#114222,#114223,#114224,#114225,#114226,#114227,#114228,#114229,
#114230,#114231,#114232,#114233,#114234,#114235,#114236,#114237,#114238,
#114239,#114240,#114241,#114242,#114243,#114244,#114245,#114246,#114247,
#114248,#114249,#114250,#114251,#114252,#114253,#114254,#114255,#114256,
#114257,#114258,#114259,#114260,#114261,#114262,#114263,#114264,#114265,
#114266,#114267,#114268,#114269,#114270,#114271,#114272,#114273,#114274,
#114275,#114276,#114277,#114278,#114279,#114280,#114281,#114282,#114283,
#114284,#114285,#114286,#114287,#114288,#114289,#114290,#114291,#114292,
#114293,#114294,#114295,#114296,#114297,#114298,#114299,#114300,#114301,
#114302,#114303,#114304,#114305,#114306,#114307,#114308,#114309,#114310,
#114311,#114312,#114313,#114314,#114315,#114316,#114317,#114318,#114319,
#114320,#114321,#114322,#114323,#114324,#114325,#114326,#114327,#114328,
#114329,#114330,#114331,#114332,#114333,#114334,#114335,#114336,#114337,
#114338,#114339,#114340,#114341,#114342,#114343,#114344,#114345,#114346,
#114347,#114348,#114349,#114350,#114351,#114352,#114353,#114354,#114355,
#114356,#114357,#114358,#114359,#114360,#114361,#114362,#114363,#114364,
#114365,#114366,#114367,#114368),.UNSPECIFIED.,.F.,.F.,(4,2,2,2,2,2,2,2,
2,2,2,2,2,2,2,2,2,2,2,2,2,2,2,2,2,2,2,2,2,2,2,2,2,2,2,2,2,2,2,2,2,2,2,2,
2,2,2,2,2,2,2,2,2,2,2,2,2,2,2,2,2,2,2,2,2,2,2,2,2,2,2,2,2,2,2,2,2,2,2,2,
2,2,2,2,2,2,2,2,2,2,2,2,2,2,2,2,2,2,2,2,2,2,2,2,2,2,2,4),(0.922145236069275,
0.930099973352994,0.932107881168367,0.933275599929072,0.93419394686494,
0.935477640186354,0.938093815256887,0.941547728791295,0.975011963371041,
0.999294364481554,1.00291791362147,1.00521311898398,1.00703056970487,1.00907405482704,
1.01252386952128,1.02680357041686,1.05912883335261,1.06734748520995,1.0756397689485,
1.07767547467535,1.07884955548381,1.07976688396211,1.08104139240927,1.08361156963494,
1.10814217453859,1.14280125718349,1.14814571240382,1.15054486463945,1.1523811914005,
1.15435163796943,1.15746825637024,1.16785972826562,1.18598448997868,1.21399147684555,
1.22136533931493,1.22334553194136,1.22449543919053,1.22551994870709,1.22689159252903,
1.22997382566216,1.24341297343242,1.27537607707635,1.27867695058951,1.2914293368863,
1.29490169426795,1.29695004300745,1.29858493621659,1.3007850517688,1.30496798702628,
1.3354708250013,1.36458018818733,1.36799235669982,1.36932014043535,1.37027802268805,
1.37132962277312,1.37285867374941,1.37690633907274,1.38302347743107,1.42416486087504,
1.43702714683815,1.44050835770318,1.44255853625363,1.44419302360988,1.44639017986748,
1.45055935455125,1.48314428569505,1.51002997857825,1.51355800107457,1.51490256321908,
1.51586480265039,1.51691225278267,1.51842044255947,1.52232926517163,1.52816608434368,
1.54763897256609,1.57927344813945,1.5842583527272,1.58693944426067,1.58863050170565,
1.59049582075123,1.59310601413759,1.59954236567784,1.63523166251883,1.65731330519417,
1.65974532615154,1.66100769139675,1.66202239555444,1.66324739410687,1.66557615759469,
1.67898074642236,1.71454529741024,1.72809772908284,1.73159090305039,1.73366357692704,
1.73545956068647,1.73770160019749,1.74181677882735,1.7608609893505,1.77766003033577,
1.78584563173894,1.80288401998028,1.80530153286857,1.80656069248462,1.80757521002481,
1.80880287065332,1.81114470832946,1.81676095143397,1.84353659621564),
 .UNSPECIFIED.);
#1587=B_SPLINE_CURVE_WITH_KNOTS('',3,(#114369,#114370,#114371,#114372),
 .UNSPECIFIED.,.F.,.F.,(4,4),(6.73545010571804E-5,0.000198811978866998),
 .UNSPECIFIED.);
#1588=B_SPLINE_CURVE_WITH_KNOTS('',3,(#114373,#114374,#114375,#114376,#114377,
#114378,#114379,#114380,#114381,#114382,#114383,#114384,#114385,#114386,
#114387,#114388,#114389,#114390,#114391,#114392,#114393,#114394,#114395,
#114396,#114397,#114398,#114399,#114400,#114401,#114402,#114403,#114404,
#114405,#114406,#114407,#114408,#114409,#114410,#114411,#114412,#114413,
#114414,#114415,#114416,#114417,#114418,#114419,#114420,#114421,#114422,
#114423,#114424,#114425,#114426,#114427,#114428,#114429,#114430,#114431,
#114432,#114433,#114434,#114435,#114436,#114437,#114438,#114439,#114440,
#114441,#114442,#114443,#114444,#114445,#114446,#114447,#114448,#114449,
#114450,#114451,#114452,#114453,#114454,#114455,#114456,#114457,#114458,
#114459,#114460,#114461,#114462,#114463,#114464,#114465,#114466,#114467,
#114468,#114469,#114470,#114471,#114472,#114473,#114474,#114475,#114476,
#114477,#114478,#114479,#114480,#114481,#114482,#114483,#114484,#114485,
#114486,#114487,#114488,#114489,#114490,#114491,#114492,#114493,#114494,
#114495,#114496,#114497,#114498,#114499,#114500,#114501,#114502,#114503,
#114504,#114505,#114506,#114507,#114508,#114509,#114510,#114511,#114512,
#114513,#114514,#114515,#114516,#114517,#114518,#114519,#114520,#114521,
#114522,#114523,#114524,#114525,#114526,#114527,#114528,#114529,#114530,
#114531,#114532,#114533,#114534,#114535,#114536,#114537,#114538,#114539,
#114540,#114541,#114542,#114543,#114544),.UNSPECIFIED.,.F.,.F.,(4,3,3,3,
3,3,3,3,3,3,3,3,3,3,3,3,3,3,3,3,3,3,3,3,3,3,3,3,3,3,3,3,3,3,3,3,3,3,3,3,
3,3,3,3,3,3,3,3,3,3,3,3,3,3,3,3,3,4),(89.0873369787636,89.2354843443786,
89.3283014930121,89.4417836042537,89.5550641214456,89.6682326252091,89.7813339181988,
89.8944127030348,90.0075954204445,90.1208296866396,90.2342774869224,90.3208381762678,
90.4343202875066,90.5476008046957,90.6607693084565,90.7738706014435,90.8869493862768,
91.000132103684,91.1133663698766,91.2268141701569,91.3133748595235,91.4268569707589,
91.5401374879445,91.6533059917019,91.7664072846854,91.8794860695152,91.9926687869188,
92.1059030531078,92.2193508533846,92.3059115427791,92.4193936540317,92.5326741712347,
92.6458426750093,92.75894396801,92.8720227528569,92.9852054702775,93.0984397364834,
93.2118875367767,93.2984482260348,93.4119303372638,93.5252108544434,93.6383793581948,
93.7514806511725,93.8645594359965,93.9777421533947,94.0909764195785,94.2044242198503,
94.2909849092905,94.4044670205054,94.5177475376704,94.630916041407,94.7440173343696,
94.8570961191784,94.9702788365611,95.0835131027292,95.1969609029854,95.2835215925462,
95.3705214141547),.UNSPECIFIED.);
#1589=B_SPLINE_CURVE_WITH_KNOTS('',3,(#114549,#114550,#114551,#114552,#114553,
#114554,#114555,#114556,#114557,#114558,#114559,#114560,#114561,#114562,
#114563,#114564,#114565,#114566,#114567,#114568,#114569,#114570,#114571,
#114572,#114573,#114574,#114575,#114576,#114577,#114578,#114579,#114580,
#114581,#114582,#114583,#114584,#114585,#114586,#114587,#114588,#114589,
#114590,#114591,#114592,#114593,#114594,#114595,#114596,#114597,#114598,
#114599,#114600,#114601,#114602,#114603,#114604,#114605,#114606,#114607,
#114608,#114609,#114610,#114611,#114612,#114613,#114614,#114615,#114616,
#114617,#114618,#114619,#114620,#114621,#114622,#114623,#114624,#114625,
#114626,#114627,#114628,#114629,#114630,#114631,#114632,#114633,#114634,
#114635,#114636,#114637,#114638,#114639,#114640,#114641,#114642,#114643,
#114644,#114645,#114646,#114647,#114648,#114649,#114650,#114651,#114652,
#114653,#114654,#114655,#114656,#114657,#114658,#114659,#114660,#114661,
#114662,#114663,#114664,#114665,#114666,#114667,#114668,#114669,#114670,
#114671,#114672,#114673,#114674,#114675,#114676,#114677,#114678,#114679,
#114680,#114681,#114682,#114683,#114684,#114685,#114686,#114687,#114688,
#114689,#114690,#114691,#114692,#114693,#114694,#114695,#114696,#114697,
#114698,#114699,#114700,#114701,#114702,#114703,#114704,#114705,#114706,
#114707,#114708,#114709,#114710,#114711,#114712,#114713,#114714,#114715,
#114716,#114717,#114718,#114719,#114720,#114721,#114722,#114723,#114724,
#114725,#114726,#114727,#114728,#114729,#114730,#114731,#114732,#114733,
#114734,#114735,#114736,#114737,#114738,#114739,#114740,#114741,#114742,
#114743,#114744,#114745,#114746,#114747,#114748,#114749,#114750,#114751,
#114752,#114753,#114754,#114755,#114756,#114757,#114758,#114759,#114760,
#114761,#114762,#114763,#114764,#114765,#114766,#114767,#114768,#114769,
#114770,#114771,#114772),.UNSPECIFIED.,.F.,.F.,(4,2,2,2,2,2,2,2,2,2,2,2,
2,2,2,2,2,2,2,2,2,2,2,2,2,2,2,2,2,2,2,2,2,2,2,2,2,2,2,2,2,2,2,2,2,2,2,2,
2,2,2,2,2,2,2,2,2,2,2,2,2,2,2,2,2,2,2,2,2,2,2,2,2,2,2,2,2,2,2,2,2,2,2,2,
2,2,2,2,2,2,2,2,2,2,2,2,2,2,2,2,2,2,2,2,2,2,2,2,2,2,2,4),(0.000537788205222184,
0.0412154549149923,0.0561747957247499,0.0584711220099246,0.0596893029918871,
0.060704274533989,0.0619743954783404,0.0639700647646533,0.0744953586875274,
0.0781467153376516,0.115351480761497,0.123203538939702,0.127124951214964,
0.129550403514325,0.131718265746167,0.1317534451347,0.131789516174362,0.131826544704866,
0.131864602013896,0.133607805143231,0.135667900055591,0.139194515470624,
0.15258354640383,0.18634241742011,0.200418333636561,0.203572807557997,0.204957268247585,
0.205983489882934,0.207126678393224,0.209076724871123,0.216127982233253,
0.244388027293493,0.262614795684615,0.273042664231492,0.276162824680071,
0.278133902685874,0.279969707770093,0.282366583692268,0.287699205404328,
0.322466448629646,0.34689989462452,0.349453786325807,0.350724937511526,
0.351641830404646,0.352818080377451,0.354863640989318,0.36324906801713,
0.371458992655041,0.392089093937398,0.414815503947171,0.420186664783383,
0.422616735757513,0.424451309421504,0.426426078856524,0.429562858415874,
0.439157656763658,0.480981688445164,0.493091052657945,0.495281734612963,
0.496477505449941,0.49749419105753,0.498792598560036,0.500881714251003,
0.513330926556598,0.524825621125422,0.542986739446269,0.556259330361401,
0.561894294667348,0.56630190007709,0.56854809268396,0.570361345774777,0.572437660303972,
0.57594572966503,0.589640696854087,0.595021855282038,0.624454171199838,
0.633956527963948,0.639511470460461,0.641234610659879,0.642327655677003,
0.643364334865411,0.64486992673883,0.64848777310719,0.671041166307839,0.690381157664352,
0.702497828902728,0.707796369893352,0.711994655500353,0.714198114861535,
0.716008888783038,0.718118420597832,0.72177197136746,0.737592022849622,
0.769415134908327,0.784046995620602,0.786333307739155,0.787549492796133,
0.788564734455465,0.789837623775737,0.791842048642956,0.802531659933779,
0.805805796590242,0.843188169829598,0.851057059875072,0.856774479642902,
0.859265835369003,0.861110288706096,0.862827616286446,0.865189920878605,
0.869962587923911,0.905125916193915,0.922145236069275),.UNSPECIFIED.);
#1590=B_SPLINE_CURVE_WITH_KNOTS('',3,(#114773,#114774,#114775,#114776,#114777,
#114778,#114779,#114780,#114781,#114782,#114783,#114784,#114785,#114786,
#114787,#114788,#114789,#114790,#114791,#114792,#114793,#114794,#114795,
#114796,#114797,#114798,#114799,#114800,#114801,#114802,#114803,#114804,
#114805,#114806,#114807,#114808,#114809,#114810,#114811,#114812,#114813,
#114814,#114815,#114816,#114817,#114818,#114819,#114820,#114821,#114822,
#114823,#114824,#114825,#114826,#114827,#114828,#114829,#114830,#114831,
#114832,#114833,#114834,#114835,#114836,#114837,#114838,#114839,#114840,
#114841,#114842,#114843,#114844,#114845,#114846,#114847,#114848,#114849,
#114850,#114851,#114852,#114853,#114854,#114855,#114856,#114857,#114858,
#114859,#114860,#114861,#114862,#114863,#114864,#114865,#114866,#114867,
#114868,#114869,#114870,#114871,#114872,#114873,#114874,#114875,#114876,
#114877,#114878,#114879,#114880,#114881,#114882,#114883,#114884,#114885,
#114886,#114887,#114888,#114889,#114890,#114891,#114892,#114893,#114894,
#114895,#114896,#114897,#114898,#114899,#114900,#114901,#114902,#114903,
#114904,#114905,#114906,#114907,#114908,#114909,#114910,#114911,#114912,
#114913,#114914,#114915,#114916,#114917,#114918,#114919,#114920,#114921,
#114922,#114923,#114924,#114925,#114926,#114927,#114928,#114929,#114930,
#114931,#114932,#114933,#114934,#114935,#114936,#114937,#114938,#114939,
#114940,#114941,#114942,#114943,#114944,#114945,#114946,#114947,#114948,
#114949,#114950,#114951,#114952,#114953,#114954,#114955,#114956,#114957,
#114958,#114959,#114960,#114961,#114962,#114963,#114964,#114965,#114966,
#114967,#114968,#114969,#114970,#114971,#114972,#114973,#114974,#114975,
#114976,#114977,#114978,#114979,#114980,#114981,#114982,#114983,#114984,
#114985,#114986),.UNSPECIFIED.,.F.,.F.,(4,2,2,2,2,2,2,2,2,2,2,2,2,2,2,2,
2,2,2,2,2,2,2,2,2,2,2,2,2,2,2,2,2,2,2,2,2,2,2,2,2,2,2,2,2,2,2,2,2,2,2,2,
2,2,2,2,2,2,2,2,2,2,2,2,2,2,2,2,2,2,2,2,2,2,2,2,2,2,2,2,2,2,2,2,2,2,2,2,
2,2,2,2,2,2,2,2,2,2,2,2,2,2,2,2,2,2,4),(0.000422832080831237,0.0231641369034323,
0.0436625978087327,0.0548869710746597,0.0580860565639775,0.0600746485661758,
0.0619049612885063,0.0642639773300582,0.0692004724361086,0.10708315407289,
0.122398094458075,0.127468799234693,0.129886156083532,0.131810214369377,
0.132955479732407,0.133976074497356,0.135292642222996,0.137490196673243,
0.153753014059877,0.185763236143005,0.199983313654894,0.203429122416956,
0.205471854552152,0.207289640637777,0.209586632568232,0.213215705162516,
0.241260298620107,0.261402706048461,0.274947525214627,0.277196342734631,
0.278404588326497,0.279420320928489,0.28070286968664,0.282739154045147,
0.294075409440267,0.325133414300778,0.338287209650057,0.343888147688721,
0.348274722900811,0.350516688179482,0.352312994039333,0.354386472121347,
0.357882046811702,0.371462406253757,0.404821914398403,0.420385164382855,
0.422699642218197,0.423921764847353,0.424936751405952,0.426202826256647,
0.428651529042321,0.449278770776321,0.47398498145182,0.490766407620942,
0.494374781822933,0.496452990362262,0.498266155034714,0.500509992687324,
0.503964019263108,0.522315683477168,0.551912871382542,0.561437339141659,
0.567001155497484,0.568725342029325,0.569818656589941,0.570855274256569,
0.572360321741661,0.57597410741078,0.5986064122194,0.618092846594316,0.630062873602365,
0.635317654704643,0.639488477308072,0.641686324221132,0.643321251273812,
0.645371897072596,0.648853705155028,0.661720316766805,0.695742015556085,
0.711458052695675,0.713776952121576,0.715000046187486,0.716015057279447,
0.717280185453477,0.719258972012191,0.729462438497255,0.733739068057952,
0.735978580016645,0.767946736376416,0.782159037315848,0.785604382194395,
0.787647060664827,0.789464935757282,0.791762224734678,0.795392134097783,
0.823393165670096,0.847387041272158,0.857414090942898,0.859499368961179,
0.860672440979104,0.861692302950705,0.863002214592797,0.865176891512479,
0.880201143762242,0.889180545816463,0.910849041034443,0.921801751976425),
 .UNSPECIFIED.);
#1591=B_SPLINE_CURVE_WITH_KNOTS('',3,(#114991,#114992,#114993,#114994,#114995,
#114996,#114997,#114998,#114999,#115000,#115001,#115002,#115003,#115004,
#115005,#115006,#115007,#115008,#115009,#115010,#115011,#115012,#115013,
#115014,#115015,#115016,#115017,#115018,#115019,#115020,#115021,#115022,
#115023,#115024,#115025,#115026,#115027,#115028,#115029,#115030,#115031,
#115032,#115033,#115034,#115035,#115036,#115037,#115038,#115039,#115040,
#115041,#115042,#115043,#115044,#115045,#115046,#115047,#115048,#115049,
#115050,#115051,#115052,#115053,#115054,#115055,#115056,#115057,#115058,
#115059,#115060,#115061,#115062,#115063,#115064,#115065,#115066,#115067,
#115068,#115069,#115070,#115071,#115072,#115073,#115074,#115075,#115076,
#115077,#115078,#115079,#115080,#115081,#115082,#115083,#115084,#115085,
#115086,#115087,#115088,#115089,#115090,#115091,#115092,#115093,#115094,
#115095,#115096,#115097,#115098,#115099,#115100,#115101,#115102,#115103,
#115104,#115105,#115106,#115107,#115108,#115109,#115110,#115111,#115112,
#115113,#115114,#115115,#115116,#115117,#115118,#115119,#115120,#115121,
#115122,#115123,#115124,#115125,#115126,#115127,#115128,#115129,#115130,
#115131,#115132,#115133,#115134,#115135,#115136,#115137,#115138,#115139,
#115140,#115141,#115142,#115143,#115144,#115145,#115146,#115147,#115148,
#115149,#115150,#115151,#115152,#115153,#115154,#115155,#115156,#115157,
#115158,#115159,#115160,#115161,#115162,#115163,#115164,#115165,#115166,
#115167,#115168,#115169,#115170,#115171,#115172,#115173,#115174,#115175,
#115176,#115177,#115178,#115179,#115180,#115181,#115182,#115183,#115184,
#115185,#115186,#115187,#115188,#115189,#115190,#115191,#115192,#115193,
#115194,#115195,#115196,#115197,#115198,#115199,#115200,#115201,#115202,
#115203,#115204,#115205,#115206,#115207,#115208),.UNSPECIFIED.,.F.,.F.,
(4,2,2,2,2,2,2,2,2,2,2,2,2,2,2,2,2,2,2,2,2,2,2,2,2,2,2,2,2,2,2,2,2,2,2,
2,2,2,2,2,2,2,2,2,2,2,2,2,2,2,2,2,2,2,2,2,2,2,2,2,2,2,2,2,2,2,2,2,2,2,2,
2,2,2,2,2,2,2,2,2,2,2,2,2,2,2,2,2,2,2,2,2,2,2,2,2,2,2,2,2,2,2,2,2,2,2,2,
2,4),(0.921725633262079,0.949576255217166,0.953189867214194,0.95548182448934,
0.957298623741511,0.959343404706572,0.962800358457658,0.977188880417411,
1.01011684105481,1.02527247387913,1.02745077460306,1.02876154540852,1.02978121221861,
1.03095299541059,1.0330336272909,1.04298949565247,1.06664950293528,1.09512386101343,
1.09873117438062,1.10102114119684,1.10283762575705,1.10488338552217,1.10834524458052,
1.1228060898948,1.15613479000508,1.16213936875559,1.17130425944584,1.17340635277157,
1.17459539715621,1.17561249366501,1.17691934523928,1.17965512954395,1.18331309507381,
1.19254469668056,1.21260437194532,1.24060620728182,1.24424321226475,1.24654216862674,
1.24835959609691,1.25039990885999,1.2538367333725,1.2679431508107,1.2993808696953,
1.3163034270449,1.31871892067003,1.31997758933872,1.32099203109221,1.32221998760714,
1.32456343325672,1.34123456269813,1.38437212839195,1.38955319235994,1.39192246199284,
1.39375369963911,1.39573628758968,1.39891032291311,1.40988245749201,1.42963928941552,
1.46047494308472,1.46377192978575,1.46508015989422,1.4660328257747,1.46708919018995,
1.46864306126952,1.47286372986537,1.49902919577973,1.52933780257434,1.53490002355417,
1.53711764688994,1.53896719012727,1.54087307551792,1.54368975430288,1.55154167943457,
1.56358226045694,1.58297228379386,1.60554569538321,1.60915913140799,1.61066360284466,
1.61169971870757,1.61279237567419,1.61451527992088,1.62007260117396,1.62958383749003,
1.65907460141803,1.67752748807667,1.68100025182845,1.68324917394677,1.68502060376805,
1.68703021545619,1.68915402035642,1.69234554613468,1.6982002180556,1.71225799480805,
1.73404738345931,1.75283400580711,1.75527494988093,1.75653894226651,1.75755330926194,
1.75877592207479,1.76109470201267,1.77684204839185,1.81265715015851,1.82398332991216,
1.82731730843342,1.82933472530591,1.83110177755749,1.83286177871242,1.83511224080361,
1.84305992990751),.UNSPECIFIED.);
#1592=B_SPLINE_CURVE_WITH_KNOTS('',3,(#115209,#115210,#115211,#115212,#115213,
#115214,#115215,#115216,#115217,#115218,#115219,#115220,#115221,#115222,
#115223,#115224,#115225,#115226,#115227,#115228,#115229,#115230,#115231,
#115232,#115233,#115234,#115235,#115236,#115237,#115238,#115239,#115240,
#115241,#115242,#115243,#115244,#115245,#115246,#115247,#115248,#115249,
#115250,#115251,#115252,#115253,#115254,#115255,#115256,#115257,#115258,
#115259,#115260,#115261,#115262,#115263,#115264,#115265,#115266,#115267,
#115268,#115269,#115270,#115271,#115272,#115273,#115274,#115275,#115276,
#115277,#115278,#115279,#115280,#115281,#115282,#115283,#115284,#115285,
#115286,#115287,#115288,#115289,#115290,#115291,#115292,#115293,#115294,
#115295,#115296,#115297,#115298,#115299,#115300,#115301,#115302,#115303,
#115304,#115305,#115306,#115307,#115308,#115309,#115310,#115311,#115312,
#115313,#115314,#115315,#115316,#115317,#115318,#115319,#115320,#115321,
#115322,#115323,#115324,#115325,#115326,#115327,#115328,#115329,#115330,
#115331,#115332,#115333,#115334,#115335,#115336,#115337,#115338,#115339,
#115340,#115341,#115342,#115343,#115344,#115345,#115346,#115347,#115348,
#115349,#115350,#115351,#115352,#115353,#115354,#115355,#115356,#115357,
#115358,#115359,#115360,#115361,#115362,#115363,#115364,#115365,#115366,
#115367,#115368,#115369,#115370,#115371,#115372,#115373,#115374,#115375,
#115376,#115377,#115378,#115379,#115380,#115381,#115382,#115383,#115384,
#115385,#115386,#115387,#115388,#115389,#115390,#115391,#115392,#115393,
#115394,#115395,#115396,#115397,#115398,#115399,#115400,#115401,#115402,
#115403,#115404,#115405,#115406,#115407,#115408,#115409,#115410,#115411,
#115412,#115413,#115414,#115415,#115416,#115417,#115418,#115419,#115420,
#115421,#115422,#115423,#115424,#115425,#115426,#115427,#115428),
 .UNSPECIFIED.,.F.,.F.,(4,2,2,2,2,2,2,2,2,2,2,2,2,2,2,2,2,2,2,2,2,2,2,2,
2,2,2,2,2,2,2,2,2,2,2,2,2,2,2,2,2,2,2,2,2,2,2,2,2,2,2,2,2,2,2,2,2,2,2,2,
2,2,2,2,2,2,2,2,2,2,2,2,2,2,2,2,2,2,2,2,2,2,2,2,2,2,2,2,2,2,2,2,2,2,2,2,
2,2,2,2,2,2,2,2,2,2,2,2,2,4),(0.921801751976425,0.928993186603278,0.931799776086555,
0.933513930511989,0.935360977569221,0.937866490624144,0.943664922853653,
0.951678557413244,0.974996347806176,1.00053872865013,1.00411662522397,1.00546783791764,
1.00643200709162,1.00747833400396,1.00897961671964,1.01284155746269,1.01858438217066,
1.03750249382329,1.06992173477077,1.07540702596828,1.07783136247779,1.07967207047093,
1.08163286323914,1.0847039876101,1.09465992892944,1.11162999272388,1.12614995724437,
1.14781767982079,1.15026780256958,1.15153420179619,1.15254922408316,1.15377111624988,
1.15608441927888,1.17160134250916,1.20475928986257,1.21857562492971,1.222092484475,
1.22417084648222,1.22598395701949,1.22822748480154,1.23262174380447,1.23823468221565,
1.25142963165657,1.28313123267952,1.29379598527139,1.29579901905504,1.29707148805807,
1.29808671477441,1.29930328279333,1.30159142259594,1.3162792664152,1.34824968955543,
1.36388954038128,1.36753124830872,1.36963806124147,1.37144894710712,1.37365560544599,
1.37786954386904,1.40464023133291,1.43306506373248,1.43987343871292,1.44180067024132,
1.44293895137445,1.44396691933338,1.44536224453262,1.44857756177365,1.46320330103209,
1.49869174918341,1.5100892583887,1.51342827684771,1.51544750400019,1.51726963541232,
1.51960698859986,1.5244782769087,1.54317240282844,1.56862975337683,1.57684023555829,
1.58516213156876,1.58720027071113,1.58837490266454,1.58929214747542,1.59056589853921,
1.59313233728925,1.61596803153528,1.65260613776114,1.6572422425125,1.6595709083241,
1.66127960562939,1.66312985895016,1.66565600363234,1.6714502616477,1.67952631625789,
1.70317477586795,1.72825259225605,1.73183516150597,1.73318677195699,1.73415091259253,
1.73519686428201,1.73669702600259,1.74042786597807,1.76107722766996,1.77771117914622,
1.79997350278526,1.80356050888335,1.80584464387862,1.80766098276403,1.80971133938939,
1.81184137604068,1.81504719542795,1.84332610369432),.UNSPECIFIED.);
#1593=B_SPLINE_CURVE_WITH_KNOTS('',3,(#115433,#115434,#115435,#115436,#115437,
#115438,#115439,#115440,#115441,#115442,#115443,#115444,#115445,#115446,
#115447,#115448,#115449,#115450,#115451,#115452,#115453,#115454,#115455,
#115456,#115457,#115458,#115459,#115460,#115461,#115462,#115463,#115464,
#115465,#115466,#115467,#115468,#115469,#115470,#115471,#115472,#115473,
#115474,#115475,#115476,#115477,#115478,#115479,#115480,#115481,#115482,
#115483,#115484,#115485,#115486,#115487,#115488,#115489,#115490,#115491,
#115492,#115493,#115494,#115495,#115496,#115497,#115498,#115499,#115500,
#115501,#115502,#115503,#115504,#115505,#115506,#115507,#115508,#115509,
#115510,#115511,#115512,#115513,#115514,#115515,#115516,#115517,#115518,
#115519,#115520,#115521,#115522,#115523,#115524,#115525,#115526,#115527,
#115528,#115529,#115530,#115531,#115532,#115533,#115534,#115535,#115536,
#115537,#115538,#115539,#115540,#115541,#115542,#115543,#115544,#115545,
#115546,#115547,#115548,#115549,#115550,#115551,#115552,#115553,#115554,
#115555,#115556,#115557,#115558,#115559,#115560,#115561,#115562,#115563,
#115564,#115565,#115566,#115567,#115568,#115569,#115570,#115571,#115572,
#115573,#115574,#115575,#115576,#115577,#115578,#115579,#115580,#115581,
#115582,#115583,#115584,#115585,#115586,#115587,#115588,#115589,#115590,
#115591,#115592,#115593,#115594,#115595,#115596,#115597,#115598,#115599,
#115600,#115601,#115602,#115603,#115604,#115605,#115606,#115607,#115608,
#115609,#115610,#115611,#115612,#115613,#115614,#115615,#115616,#115617,
#115618,#115619,#115620,#115621,#115622,#115623,#115624,#115625,#115626,
#115627,#115628,#115629,#115630,#115631,#115632,#115633,#115634,#115635,
#115636,#115637,#115638,#115639,#115640,#115641,#115642,#115643,#115644,
#115645,#115646,#115647,#115648,#115649,#115650,#115651,#115652,#115653,
#115654,#115655,#115656),.UNSPECIFIED.,.F.,.F.,(4,2,2,2,2,2,2,2,2,2,2,2,
2,2,2,2,2,2,2,2,2,2,2,2,2,2,2,2,2,2,2,2,2,2,2,2,2,2,2,2,2,2,2,2,2,2,2,2,
2,2,2,2,2,2,2,2,2,2,2,2,2,2,2,2,2,2,2,2,2,2,2,2,2,2,2,2,2,2,2,2,2,2,2,2,
2,2,2,2,2,2,2,2,2,2,2,2,2,2,2,2,2,2,2,2,2,2,2,2,2,2,2,4),(0.000439914180201879,
0.00735087020532558,0.00879393008916023,0.00983800708509203,0.0107902023889067,
0.0117382816365723,0.0130275882263253,0.01621718725617,0.0240737006876381,
0.0379108716697168,0.0731061580349014,0.0793602683738382,0.0819450251709392,
0.0838090885747689,0.085510590644278,0.0882334997756488,0.0948843795411132,
0.130772015818668,0.145473930588226,0.150421452161862,0.152799611216542,
0.154730567995416,0.155860437615718,0.156841086144421,0.158157665395588,
0.160352965110758,0.176187006904382,0.208520885546101,0.222797291091522,
0.226247139492212,0.228290836136495,0.230108600817205,0.232404377937929,
0.236029126876226,0.264458957544217,0.28480559029371,0.297869941583472,
0.300099648808395,0.301303375678287,0.302318362360115,0.303603866209583,
0.305652649347156,0.317276676234962,0.348057424501443,0.361190729862364,
0.366784078240857,0.371164883466434,0.373403934273249,0.375214544850484,
0.377291240551271,0.380808077501874,0.394665311394709,0.427793523003757,
0.443296601352044,0.445607141407924,0.446827423762021,0.44784165043002,
0.449107498159173,0.451555884593169,0.472107645393182,0.496854401237881,
0.513671969233811,0.517282552302813,0.519361337240652,0.521174600788465,
0.52341804635096,0.52687052245169,0.545187862895212,0.574783394540152,0.584307386307393,
0.589871062274551,0.591595546539695,0.592689145907578,0.593725671640217,
0.595230689490728,0.598845268901491,0.621439980894645,0.640861505358724,
0.652888465572059,0.660733547910954,0.663549608345408,0.665455587489115,
0.667305609186157,0.669524262641367,0.675091627330956,0.70521186441497,
0.731540016359414,0.735772252645225,0.737327806530722,0.738384541076538,
0.739336892018181,0.740643902108912,0.743933653044977,0.7748710217023,0.794589057111284,
0.805547360125346,0.808720031622231,0.810702278938135,0.812533543063013,
0.814903322403207,0.820087457920443,0.856387216131039,0.872670943467903,
0.877932337236289,0.881548421551187,0.883010636458946,0.884049347976965,
0.885022626271749,0.886690364274768,0.891347346841458,0.921594694409251,
0.921725633262079),.UNSPECIFIED.);
#1594=B_SPLINE_CURVE_WITH_KNOTS('',3,(#115657,#115658,#115659,#115660,#115661,
#115662,#115663,#115664,#115665,#115666,#115667,#115668,#115669,#115670,
#115671,#115672,#115673,#115674,#115675,#115676,#115677,#115678,#115679,
#115680,#115681,#115682,#115683,#115684,#115685,#115686,#115687,#115688,
#115689,#115690,#115691,#115692,#115693,#115694,#115695,#115696,#115697,
#115698,#115699,#115700,#115701,#115702,#115703,#115704,#115705,#115706,
#115707,#115708,#115709,#115710,#115711,#115712,#115713,#115714,#115715,
#115716,#115717,#115718,#115719,#115720,#115721,#115722,#115723,#115724,
#115725,#115726,#115727,#115728,#115729,#115730,#115731,#115732,#115733,
#115734,#115735,#115736,#115737,#115738,#115739,#115740,#115741,#115742,
#115743,#115744,#115745,#115746,#115747,#115748,#115749,#115750,#115751,
#115752,#115753,#115754,#115755,#115756,#115757,#115758,#115759,#115760,
#115761,#115762,#115763,#115764,#115765,#115766,#115767,#115768,#115769,
#115770,#115771,#115772,#115773,#115774,#115775,#115776,#115777,#115778,
#115779,#115780,#115781,#115782,#115783,#115784,#115785,#115786,#115787,
#115788,#115789,#115790,#115791,#115792,#115793,#115794,#115795,#115796,
#115797,#115798,#115799,#115800,#115801,#115802,#115803,#115804,#115805,
#115806,#115807,#115808,#115809,#115810,#115811,#115812,#115813,#115814,
#115815,#115816,#115817,#115818,#115819,#115820,#115821,#115822,#115823,
#115824,#115825,#115826,#115827,#115828),.UNSPECIFIED.,.F.,.F.,(4,3,3,3,
3,3,3,3,3,3,3,3,3,3,3,3,3,3,3,3,3,3,3,3,3,3,3,3,3,3,3,3,3,3,3,3,3,3,3,3,
3,3,3,3,3,3,3,3,3,3,3,3,3,3,3,3,3,4),(107.936893664275,108.082961511445,
108.18649847487,108.299980162362,108.413260256859,108.526428338887,108.639529211831,
108.752607579042,108.865789885852,108.979023744717,109.092471148062,109.179035158126,
109.292517499002,109.405798239768,109.518966963243,109.632068471743,109.745147467543,
109.858330387305,109.971564851382,110.085012839851,110.171571841382,110.285055033765,
110.398336640939,110.511506239252,110.624608629379,110.737688511965,110.850872319289,
110.964107672719,111.077556542252,111.164108524637,111.277587519026,111.390864923171,
111.504030318546,111.617128513211,111.730204215196,111.843383897961,111.956615151618,
112.07006001287,112.156645207893,112.270129875436,112.383412908333,112.496583901166,
112.609687652534,112.722768860973,112.835953929634,112.949190510518,113.062640537437,
113.149181891149,113.262670135362,113.375956856776,113.489131603515,113.602239166777,
113.715324237775,113.828513215311,113.941753736768,114.055207705859,114.141718574404,
114.220077335694),.UNSPECIFIED.);
#1595=B_SPLINE_CURVE_WITH_KNOTS('',3,(#115834,#115835,#115836,#115837,#115838,
#115839,#115840,#115841,#115842,#115843,#115844,#115845,#115846,#115847,
#115848,#115849,#115850,#115851,#115852,#115853,#115854,#115855,#115856,
#115857,#115858,#115859,#115860,#115861,#115862,#115863,#115864,#115865,
#115866,#115867,#115868,#115869,#115870,#115871,#115872,#115873,#115874,
#115875,#115876,#115877,#115878,#115879,#115880,#115881,#115882,#115883,
#115884,#115885,#115886,#115887,#115888,#115889,#115890,#115891,#115892,
#115893,#115894,#115895,#115896,#115897,#115898,#115899,#115900,#115901,
#115902,#115903,#115904,#115905,#115906,#115907,#115908,#115909,#115910,
#115911,#115912,#115913,#115914,#115915,#115916,#115917,#115918,#115919,
#115920,#115921,#115922,#115923,#115924,#115925,#115926,#115927,#115928,
#115929,#115930,#115931,#115932,#115933,#115934,#115935,#115936,#115937,
#115938,#115939,#115940,#115941,#115942,#115943,#115944,#115945,#115946,
#115947,#115948,#115949,#115950,#115951,#115952,#115953,#115954,#115955,
#115956,#115957,#115958,#115959,#115960,#115961),.UNSPECIFIED.,.F.,.F.,
(4,2,2,2,2,2,2,2,2,2,2,2,2,2,2,2,2,2,2,2,2,2,2,2,2,2,2,2,2,2,2,2,2,2,2,
2,2,2,2,2,2,2,2,2,2,2,2,2,2,2,2,2,2,2,2,2,2,2,2,2,2,2,2,4),(5.09106672909598E-5,
0.0241638658855157,0.0402610837467883,0.0447177340941628,0.0469913146460663,
0.0488360824618075,0.0509655261534932,0.0546261785485025,0.0760251216445918,
0.0930080494465782,0.0989355387576973,0.101616095779122,0.103171951577462,
0.104504145979611,0.104514853444631,0.104525639016062,0.104536506099771,
0.104547458200618,0.104558498952096,0.104569632074016,0.105594347656082,
0.106780654969661,0.108842728681758,0.11774017688508,0.140039196639271,
0.157417603053612,0.160972874249764,0.163043381116964,0.164869773559774,
0.167162963366124,0.171801021217633,0.199299936175907,0.217990666940658,
0.220713933431138,0.222017097616605,0.223034425414255,0.224244351340609,
0.226463601966407,0.23967212336241,0.24541835094314,0.260473127118986,0.2752172229747,
0.278615744141648,0.280636993619903,0.282445322966469,0.284749909850865,
0.289533089930852,0.314228460216545,0.334759859516565,0.337903314582983,
0.339140291152666,0.340165373326709,0.341283659016612,0.343123599689444,
0.3499726812499,0.363844601673138,0.390519682143007,0.395201753085217,0.397500125611384,
0.399323161385334,0.40138188780051,0.404896755452884,0.421487789229422,
0.423925865176554),.UNSPECIFIED.);
#1596=B_SPLINE_CURVE_WITH_KNOTS('',3,(#115964,#115965,#115966,#115967,#115968,
#115969,#115970,#115971,#115972,#115973,#115974,#115975,#115976,#115977,
#115978,#115979,#115980,#115981,#115982,#115983,#115984,#115985,#115986,
#115987,#115988,#115989,#115990,#115991,#115992,#115993,#115994,#115995,
#115996,#115997,#115998,#115999,#116000,#116001,#116002,#116003,#116004,
#116005,#116006,#116007,#116008,#116009,#116010,#116011,#116012,#116013,
#116014,#116015,#116016,#116017,#116018,#116019,#116020,#116021,#116022,
#116023,#116024,#116025,#116026,#116027,#116028,#116029,#116030,#116031,
#116032,#116033,#116034,#116035,#116036,#116037,#116038,#116039,#116040,
#116041,#116042,#116043,#116044,#116045,#116046,#116047,#116048),
 .UNSPECIFIED.,.F.,.F.,(4,3,3,3,3,3,3,3,3,3,3,3,3,3,3,3,3,3,3,3,3,3,3,3,
3,3,3,3,4),(11.6159397475003,11.7280381177179,11.7400068329073,11.8625173551648,
11.985000574511,12.1074989948772,12.2327433538469,12.3554956319205,12.4819860313383,
12.5938879762662,12.608476430756,12.6085211793387,12.7160201566515,12.732543516163,
12.8509131131061,12.9691482104548,13.0873037088547,13.2054343646596,13.3236778484254,
13.4419878521927,13.5543987232013,13.5605159548505,13.6010131140117,13.6010660202626,
13.7087376969109,13.7209698655402,13.8407524390979,13.9603959036733,13.9764226451991),
 .UNSPECIFIED.);
#1597=B_SPLINE_CURVE_WITH_KNOTS('',3,(#116054,#116055,#116056,#116057,#116058,
#116059,#116060,#116061,#116062,#116063,#116064,#116065,#116066,#116067,
#116068,#116069,#116070,#116071,#116072,#116073,#116074,#116075,#116076,
#116077,#116078,#116079,#116080,#116081,#116082,#116083,#116084,#116085,
#116086,#116087,#116088,#116089,#116090,#116091,#116092,#116093,#116094,
#116095,#116096,#116097,#116098,#116099,#116100,#116101,#116102,#116103,
#116104,#116105,#116106,#116107,#116108,#116109,#116110,#116111,#116112,
#116113,#116114,#116115,#116116,#116117,#116118,#116119,#116120,#116121,
#116122,#116123,#116124,#116125,#116126,#116127,#116128,#116129,#116130,
#116131,#116132,#116133,#116134,#116135,#116136,#116137,#116138,#116139,
#116140,#116141,#116142,#116143,#116144,#116145,#116146,#116147,#116148,
#116149,#116150,#116151,#116152,#116153,#116154,#116155,#116156,#116157,
#116158,#116159,#116160,#116161,#116162,#116163,#116164,#116165,#116166,
#116167,#116168,#116169,#116170,#116171,#116172,#116173,#116174,#116175,
#116176,#116177,#116178,#116179,#116180,#116181,#116182,#116183,#116184,
#116185,#116186,#116187,#116188,#116189,#116190,#116191,#116192,#116193,
#116194,#116195,#116196,#116197,#116198,#116199,#116200,#116201,#116202,
#116203,#116204,#116205,#116206,#116207,#116208,#116209,#116210,#116211,
#116212,#116213,#116214,#116215,#116216,#116217,#116218,#116219,#116220,
#116221,#116222,#116223),.UNSPECIFIED.,.F.,.F.,(4,2,2,2,2,2,2,2,2,2,2,2,
2,2,2,2,2,2,2,2,2,2,2,2,2,2,2,2,2,2,2,2,2,2,2,2,2,2,2,2,2,2,2,2,2,2,2,2,
2,2,2,2,2,2,2,2,2,2,2,2,2,2,2,2,2,2,2,2,2,2,2,2,2,2,2,2,2,2,2,2,2,2,2,2,
4),(-0.537557832667611,-0.535822407565533,-0.533634654125646,-0.532427428703531,
-0.531407235965932,-0.530091030383935,-0.527296021085561,-0.523492515533553,
-0.513337621423678,-0.490247128196482,-0.479151045954009,-0.475893689310045,
-0.473893745368097,-0.472063645881055,-0.469672765814631,-0.464476904356826,
-0.457429258263692,-0.436939307823479,-0.43202717347025,-0.418685629751132,
-0.416650093952005,-0.415369771033602,-0.414351691054465,-0.413115744844251,
-0.410726587227658,-0.407622385020085,-0.400191466048869,-0.384364055659647,
-0.362813838478521,-0.359127228137156,-0.357013256213303,-0.355200901098753,
-0.352992086950319,-0.348745846614782,-0.343324203091915,-0.330300118791415,
-0.311929771329025,-0.301326309731941,-0.299179866175964,-0.297981992556847,
-0.296960932217056,-0.29563222951209,-0.292769857080972,-0.274346012216443,
-0.247051904308374,-0.242433765299577,-0.240151119314268,-0.238333560212228,
-0.236273669535154,-0.232738716335032,-0.215622796572841,-0.190654259769387,
-0.183632963573982,-0.181707752431304,-0.18057074189062,-0.179534472604125,
-0.178092968930831,-0.174586179165968,-0.1694481856061,-0.152477628411396,
-0.130236018990756,-0.125473704543816,-0.123133239140147,-0.121386216928384,
-0.119447871239254,-0.11742902584999,-0.11083999507127,-0.101125169307191,
-0.0860054032081894,-0.0800580615520808,-0.0670227603988455,-0.0649914366300091,
-0.0637123042694286,-0.0626946303055396,-0.061458703386694,-0.0590664189302489,
-0.0559563737445437,-0.0485023004235465,-0.0182068521094829,-0.00966129008743767,
-0.00674950767218951,-0.00480121460763317,-0.00306870101462573,-0.00162054454679811,
-9.99999993922529E-7),.UNSPECIFIED.);
#1598=B_SPLINE_CURVE_WITH_KNOTS('',3,(#116224,#116225,#116226,#116227,#116228,
#116229,#116230,#116231,#116232,#116233,#116234,#116235,#116236,#116237,
#116238,#116239,#116240,#116241,#116242,#116243,#116244,#116245,#116246,
#116247,#116248,#116249,#116250,#116251,#116252,#116253,#116254,#116255,
#116256,#116257,#116258,#116259,#116260,#116261,#116262,#116263,#116264,
#116265,#116266,#116267,#116268,#116269,#116270,#116271,#116272,#116273,
#116274,#116275,#116276,#116277,#116278,#116279,#116280,#116281,#116282,
#116283,#116284,#116285,#116286,#116287,#116288,#116289,#116290,#116291,
#116292,#116293,#116294,#116295,#116296,#116297,#116298,#116299,#116300,
#116301,#116302,#116303,#116304,#116305),.UNSPECIFIED.,.F.,.F.,(4,2,2,2,
2,2,2,2,2,2,2,2,2,2,2,2,2,2,2,2,2,2,2,2,2,2,2,2,2,2,2,2,2,2,2,2,2,2,2,2,
4),(0.423925865176554,0.445966310866901,0.453687543410289,0.4556807015525,
0.456835491098318,0.457868929006599,0.459283373692191,0.462623816461385,
0.467436850977327,0.482482956088123,0.507337740573548,0.51202829969512,
0.514378966601517,0.51615821852133,0.516505652530156,0.516613873910271,
0.516692929373497,0.516753226448358,0.516800588070662,0.516838590051585,
0.516869576459979,0.516951159518163,0.517030394606397,0.517107847019529,
0.517184008515704,0.517259315771496,0.517334164442901,0.517408920172034,
0.519810406849302,0.522622828098142,0.545876157858757,0.569321885433324,
0.572016186067571,0.573338107262603,0.574293993891912,0.575357217178122,
0.576948140445213,0.581487184219949,0.588837685997641,0.624889347384345,
0.628477952425298),.UNSPECIFIED.);
#1599=B_SPLINE_CURVE_WITH_KNOTS('',3,(#116306,#116307,#116308,#116309,#116310,
#116311,#116312,#116313,#116314,#116315,#116316,#116317,#116318,#116319,
#116320,#116321,#116322,#116323,#116324,#116325,#116326,#116327,#116328,
#116329,#116330,#116331,#116332,#116333,#116334,#116335,#116336,#116337,
#116338,#116339,#116340,#116341,#116342,#116343,#116344,#116345,#116346,
#116347,#116348,#116349,#116350,#116351,#116352,#116353,#116354,#116355,
#116356,#116357,#116358,#116359,#116360,#116361,#116362,#116363,#116364,
#116365,#116366,#116367,#116368,#116369,#116370,#116371,#116372,#116373,
#116374,#116375,#116376,#116377,#116378,#116379,#116380,#116381,#116382,
#116383,#116384,#116385,#116386,#116387,#116388,#116389,#116390,#116391,
#116392,#116393,#116394,#116395,#116396,#116397,#116398,#116399,#116400,
#116401,#116402,#116403,#116404,#116405,#116406,#116407,#116408,#116409,
#116410,#116411,#116412,#116413,#116414,#116415,#116416,#116417,#116418,
#116419,#116420,#116421,#116422,#116423,#116424,#116425,#116426,#116427,
#116428,#116429,#116430,#116431,#116432,#116433,#116434,#116435,#116436,
#116437,#116438,#116439,#116440,#116441,#116442,#116443,#116444,#116445,
#116446,#116447,#116448,#116449,#116450,#116451,#116452,#116453,#116454,
#116455,#116456,#116457,#116458,#116459,#116460,#116461,#116462,#116463,
#116464,#116465,#116466,#116467,#116468,#116469,#116470,#116471,#116472,
#116473,#116474,#116475,#116476,#116477,#116478,#116479,#116480,#116481,
#116482,#116483,#116484,#116485,#116486,#116487,#116488,#116489,#116490,
#116491,#116492,#116493,#116494,#116495,#116496,#116497,#116498,#116499,
#116500,#116501,#116502,#116503,#116504,#116505,#116506,#116507,#116508,
#116509,#116510,#116511,#116512,#116513,#116514,#116515,#116516,#116517,
#116518,#116519,#116520,#116521,#116522,#116523,#116524,#116525),
 .UNSPECIFIED.,.F.,.F.,(4,2,2,2,2,2,2,2,2,2,2,2,2,2,2,2,2,2,2,2,2,2,2,2,
2,2,2,2,2,2,2,2,2,2,2,2,2,2,2,2,2,2,2,2,2,2,2,2,2,2,2,2,2,2,2,2,2,2,2,2,
2,2,2,2,2,2,2,2,2,2,2,2,2,2,2,2,2,2,2,2,2,2,2,2,2,2,2,2,2,2,2,2,2,2,2,2,
2,2,2,2,2,2,2,2,2,2,2,2,2,4),(-2.96685071646963,-2.96055947965241,-2.95644349840884,
-2.95422512500191,-2.95245698616293,-2.9506211714232,-2.94849416910481,
-2.9448387276036,-2.93163531286041,-2.91649164060133,-2.90029701081475,
-2.89656855353828,-2.8950683705804,-2.89400191143488,-2.89285870437891,
-2.89093544498106,-2.88408124946649,-2.85875094045842,-2.84766371052407,
-2.84277412466187,-2.8388888769862,-2.83728665315147,-2.83547812721969,
-2.83349513943704,-2.83033890944714,-2.82029582524522,-2.7961230389042,
-2.78210744933936,-2.77903582942547,-2.7776689790042,-2.77664590172264,
-2.77548101227555,-2.77345890762965,-2.76479906529147,-2.76248826270108,
-2.74424710289187,-2.7312720169271,-2.72587375428122,-2.72164806535048,
-2.71945405233847,-2.71765619236946,-2.71556208005707,-2.71191866305611,
-2.68955581852852,-2.67199312687268,-2.66599265095168,-2.66207025520308,
-2.66057291134113,-2.65953291497752,-2.65856058829398,-2.65689414832487,
-2.65218513278725,-2.61674971392236,-2.60984982800802,-2.6047346107735,
-2.60235656897141,-2.60052617308624,-2.59851572976238,-2.59521757227466,
-2.58389764061721,-2.56084054661053,-2.55102794106124,-2.54730552337839,
-2.54455550097753,-2.54324554721334,-2.5422241112739,-2.54100845677239,
-2.53878305122664,-2.52575226024882,-2.51985463861266,-2.50478727050801,
-2.49014547046221,-2.48674006043157,-2.48470917714537,-2.48288850132405,
-2.48056271150524,-2.47571313289205,-2.45496249108257,-2.43674492946519,
-2.43141565992467,-2.42781453603598,-2.42635972695186,-2.42532300846213,
-2.42419568442349,-2.42230706918312,-2.41566697987194,-2.39019458588422,
-2.37318972293653,-2.36966523080757,-2.3676104276467,-2.36579679786522,
-2.36351839421594,-2.35890669529677,-2.33160000037571,-2.3124423664972,
-2.31005872141856,-2.30882546361495,-2.30780896923787,-2.30653008426544,
-2.30449694568281,-2.29198510522542,-2.28616183607307,-2.27199621039738,
-2.2573640741646,-2.25307580917052,-2.25085935356893,-2.24904768859936,
-2.24694237793296,-2.24329086251894,-2.22543560030778),.UNSPECIFIED.);
#1600=B_SPLINE_CURVE_WITH_KNOTS('',3,(#116530,#116531,#116532,#116533,#116534,
#116535,#116536,#116537,#116538,#116539,#116540,#116541,#116542,#116543,
#116544,#116545,#116546,#116547,#116548,#116549,#116550,#116551,#116552,
#116553,#116554,#116555,#116556,#116557,#116558,#116559,#116560,#116561,
#116562,#116563,#116564,#116565,#116566,#116567,#116568,#116569,#116570,
#116571,#116572,#116573,#116574,#116575,#116576,#116577,#116578,#116579,
#116580,#116581,#116582,#116583,#116584,#116585,#116586,#116587,#116588,
#116589,#116590,#116591,#116592,#116593,#116594,#116595,#116596,#116597,
#116598,#116599,#116600,#116601,#116602,#116603,#116604,#116605,#116606,
#116607,#116608,#116609,#116610,#116611,#116612,#116613,#116614,#116615,
#116616,#116617,#116618,#116619,#116620,#116621,#116622,#116623,#116624,
#116625,#116626,#116627,#116628,#116629,#116630,#116631,#116632,#116633,
#116634,#116635,#116636,#116637,#116638,#116639,#116640,#116641,#116642,
#116643,#116644,#116645,#116646,#116647,#116648,#116649,#116650,#116651,
#116652,#116653,#116654,#116655,#116656,#116657,#116658,#116659,#116660,
#116661,#116662,#116663,#116664,#116665,#116666,#116667,#116668,#116669,
#116670,#116671,#116672,#116673,#116674,#116675,#116676,#116677,#116678,
#116679,#116680,#116681,#116682,#116683,#116684,#116685,#116686,#116687,
#116688,#116689,#116690,#116691,#116692,#116693,#116694,#116695,#116696,
#116697,#116698,#116699,#116700,#116701,#116702,#116703,#116704,#116705,
#116706,#116707,#116708,#116709,#116710,#116711,#116712,#116713,#116714,
#116715,#116716,#116717,#116718,#116719,#116720,#116721,#116722,#116723,
#116724,#116725,#116726,#116727,#116728,#116729),.UNSPECIFIED.,.F.,.F.,
(4,2,2,2,2,2,2,2,2,2,2,2,2,2,2,2,2,2,2,2,2,2,2,2,2,2,2,2,2,2,2,2,2,2,2,
2,2,2,2,2,2,2,2,2,2,2,2,2,2,2,2,2,2,2,2,2,2,2,2,2,2,2,2,2,2,2,2,2,2,2,2,
2,2,2,2,2,2,2,2,2,2,2,2,2,2,2,2,2,2,2,2,2,2,2,2,2,2,2,2,4),(-1.27961565155533,
-1.27297154738489,-1.25817211112012,-1.25204962479169,-1.23923900027455,
-1.23719605956918,-1.23591369383386,-1.23489572689644,-1.23366200019947,
-1.23128322551577,-1.21220821504543,-1.18480637761599,-1.18020125751498,
-1.17792150087167,-1.17610462027137,-1.17404376132814,-1.17050274441277,
-1.15323151340705,-1.12942437499849,-1.12155796802723,-1.11955841934318,
-1.11840539889111,-1.11737544514129,-1.11597092924467,-1.1126821094562,
-1.10796712845717,-1.09345280017569,-1.06780649672651,-1.06307131797335,
-1.06076646781195,-1.05894714564179,-1.05690204580128,-1.05343427489531,
-1.03770691156908,-1.01401711910753,-1.00454473900329,-1.00246327074327,
-1.00128011226314,-1.00035961713557,-0.999067045670789,-0.996394165447802,
-0.980423173921308,-0.952755332360289,-0.946676309849489,-0.94432164773791,
-0.942606667433677,-0.940757507371457,-0.93823936220053,-0.932301733272365,
-0.923878025266427,-0.892019365888256,-0.886646637842979,-0.884893253039671,
-0.883794326630226,-0.882739625746801,-0.881193921466839,-0.876993428202555,
-0.870408633008915,-0.856039535161199,-0.833524025299349,-0.828687430490428,
-0.826363109590969,-0.824541487119236,-0.822507375886747,-0.819091323474351,
-0.804306172510864,-0.789287267072459,-0.782851102148691,-0.770368449340278,
-0.768335418519258,-0.767055949957634,-0.766037984958139,-0.764801471243592,
-0.762409476468235,-0.759300495607515,-0.751852196982988,-0.736041497487957,
-0.714471002413865,-0.710806290360515,-0.70869725023484,-0.706884661565346,
-0.70466996099924,-0.700394437015238,-0.67882456183225,-0.654118764459058,
-0.651256045966331,-0.649941382691362,-0.648919551934597,-0.647727228259855,
-0.645546341251571,-0.632538709536092,-0.604766886209205,-0.595902137899208,
-0.592889513063825,-0.590942534810059,-0.589092493672625,-0.586570151213908,
-0.580608059708203,-0.547418652798889,-0.537557832667611),.UNSPECIFIED.);
#1601=B_SPLINE_CURVE_WITH_KNOTS('',3,(#116730,#116731,#116732,#116733,#116734,
#116735,#116736,#116737,#116738,#116739,#116740,#116741,#116742,#116743,
#116744,#116745,#116746,#116747,#116748,#116749,#116750,#116751,#116752,
#116753,#116754,#116755,#116756,#116757,#116758,#116759,#116760,#116761,
#116762,#116763,#116764,#116765,#116766,#116767,#116768,#116769,#116770,
#116771,#116772,#116773,#116774,#116775,#116776,#116777,#116778,#116779,
#116780,#116781,#116782,#116783,#116784,#116785,#116786,#116787,#116788,
#116789,#116790,#116791,#116792,#116793,#116794,#116795,#116796,#116797,
#116798,#116799,#116800,#116801,#116802,#116803,#116804,#116805,#116806,
#116807,#116808,#116809,#116810,#116811,#116812,#116813,#116814,#116815,
#116816,#116817,#116818,#116819,#116820,#116821,#116822,#116823,#116824,
#116825,#116826,#116827,#116828,#116829,#116830,#116831,#116832,#116833,
#116834,#116835,#116836,#116837,#116838,#116839,#116840,#116841,#116842,
#116843,#116844,#116845,#116846,#116847,#116848,#116849,#116850,#116851,
#116852,#116853,#116854,#116855,#116856,#116857,#116858,#116859,#116860,
#116861,#116862,#116863,#116864,#116865,#116866,#116867,#116868,#116869,
#116870,#116871,#116872,#116873,#116874,#116875,#116876,#116877,#116878,
#116879,#116880,#116881,#116882,#116883,#116884,#116885,#116886,#116887,
#116888,#116889,#116890,#116891,#116892,#116893,#116894,#116895,#116896,
#116897,#116898,#116899,#116900,#116901,#116902,#116903,#116904,#116905,
#116906,#116907,#116908,#116909,#116910,#116911,#116912,#116913,#116914,
#116915,#116916,#116917,#116918,#116919,#116920,#116921,#116922,#116923,
#116924,#116925,#116926,#116927,#116928,#116929,#116930,#116931,#116932,
#116933,#116934,#116935,#116936,#116937,#116938,#116939,#116940,#116941,
#116942,#116943),.UNSPECIFIED.,.F.,.F.,(4,2,2,2,2,2,2,2,2,2,2,2,2,2,2,2,
2,2,2,2,2,2,2,2,2,2,2,2,2,2,2,2,2,2,2,2,2,2,2,2,2,2,2,2,2,2,2,2,2,2,2,2,
2,2,2,2,2,2,2,2,2,2,2,2,2,2,2,2,2,2,2,2,2,2,2,2,2,2,2,2,2,2,2,2,2,2,2,2,
2,2,2,2,2,2,2,2,2,2,2,2,2,2,2,2,2,2,4),(-2.22543560030778,-2.22346995110092,
-2.19766668743467,-2.19369352880723,-2.19218089423719,-2.19113291758194,
-2.19002472527881,-2.18822657659134,-2.18246509920158,-2.17453946428187,
-2.15761531171578,-2.14023848126831,-2.13596883444132,-2.13375659654113,
-2.13194574075725,-2.12983840606076,-2.1261759035639,-2.10460241237019,
-2.08878669957219,-2.08134069297737,-2.07823339232187,-2.07584309019904,
-2.07460770676217,-2.07359085883657,-2.07231307992573,-2.07028325392101,
-2.0573292418964,-2.05134704593693,-2.03628211938002,-2.02160563381292,
-2.01819874955883,-2.0161680453255,-2.0143482087055,-2.01202444059825,-2.00718266000176,
-1.98640745700003,-1.96823701680219,-1.96291549160832,-1.95931821305553,
-1.95786377303689,-1.95682672861602,-1.9556977767367,-1.95380520587897,
-1.94713648574973,-1.94057297743912,-1.93483669394144,-1.92066836599361,
-1.90462735267213,-1.90114557885655,-1.89909841656881,-1.89728103142439,
-1.89498374134024,-1.89028269729641,-1.86409570078748,-1.84390585352744,
-1.8415628523317,-1.84033701157129,-1.83931941830871,-1.83802977064273,
-1.83596085311572,-1.81957867583272,-1.79844854979183,-1.78691121105397,
-1.78372726249022,-1.78174458661736,-1.77991173483215,-1.77753120883033,
-1.77223997334062,-1.74359891010144,-1.73190742382553,-1.72573211176272,
-1.72395573001499,-1.72285234140212,-1.72181421325108,-1.72029708341537,
-1.71741135408668,-1.69876256518131,-1.68659007488242,-1.67034632885863,
-1.66685429501999,-1.66480483018073,-1.66298766513066,-1.66069370763473,
-1.65601052653078,-1.62954610873251,-1.61557903138443,-1.61096730234711,
-1.60773339236998,-1.60633881514178,-1.60531082600416,-1.60415400827282,
-1.60213497191957,-1.59399314372386,-1.57057663470836,-1.55327373188853,
-1.54973316449134,-1.5476732062146,-1.54585750638439,-1.54357975590212,
-1.53913100716567,-1.51077344741973,-1.49233899208333,-1.49004889907942,
-1.48883402383142,-1.48781555479757,-1.48651205680211,-1.48387134362921),
 .UNSPECIFIED.);
#1602=B_SPLINE_CURVE_WITH_KNOTS('',3,(#116948,#116949,#116950,#116951,#116952,
#116953,#116954,#116955,#116956,#116957,#116958,#116959,#116960,#116961,
#116962,#116963,#116964,#116965,#116966,#116967,#116968,#116969,#116970,
#116971,#116972,#116973,#116974,#116975,#116976,#116977,#116978,#116979,
#116980,#116981,#116982,#116983,#116984,#116985,#116986,#116987,#116988,
#116989,#116990,#116991,#116992,#116993,#116994,#116995,#116996,#116997,
#116998,#116999,#117000,#117001,#117002,#117003,#117004,#117005,#117006,
#117007,#117008,#117009,#117010,#117011,#117012,#117013,#117014,#117015,
#117016,#117017,#117018,#117019,#117020,#117021,#117022,#117023,#117024,
#117025,#117026,#117027,#117028,#117029,#117030,#117031,#117032,#117033,
#117034,#117035,#117036,#117037,#117038,#117039,#117040,#117041,#117042,
#117043,#117044,#117045,#117046,#117047,#117048,#117049,#117050,#117051,
#117052,#117053,#117054,#117055,#117056,#117057,#117058,#117059,#117060,
#117061,#117062,#117063,#117064,#117065,#117066,#117067,#117068,#117069,
#117070,#117071,#117072,#117073,#117074,#117075,#117076,#117077,#117078,
#117079,#117080,#117081,#117082,#117083,#117084,#117085,#117086,#117087,
#117088,#117089,#117090,#117091,#117092,#117093,#117094,#117095,#117096,
#117097,#117098,#117099,#117100,#117101,#117102,#117103,#117104,#117105,
#117106,#117107,#117108,#117109,#117110,#117111,#117112,#117113,#117114,
#117115,#117116,#117117,#117118,#117119,#117120,#117121,#117122,#117123,
#117124,#117125,#117126,#117127,#117128,#117129,#117130,#117131,#117132,
#117133,#117134,#117135,#117136,#117137,#117138,#117139,#117140,#117141,
#117142,#117143,#117144,#117145,#117146,#117147,#117148,#117149,#117150,
#117151),.UNSPECIFIED.,.F.,.F.,(4,2,2,2,2,2,2,2,2,2,2,2,2,2,2,2,2,2,2,2,
2,2,2,2,2,2,2,2,2,2,2,2,2,2,2,2,2,2,2,2,2,2,2,2,2,2,2,2,2,2,2,2,2,2,2,2,
2,2,2,2,2,2,2,2,2,2,2,2,2,2,2,2,2,2,2,2,2,2,2,2,2,2,2,2,2,2,2,2,2,2,2,2,
2,2,2,2,2,2,2,2,2,4),(-2.02159988673811,-2.01023874891081,-2.00476139218147,
-2.00048106180913,-1.99826561944067,-1.99645327508937,-1.9943454811568,
-1.9906853890789,-1.96900276011331,-1.95310248249342,-1.94221870637194,
-1.94012097174003,-1.93894665041687,-1.93792196804332,-1.9365802692999,
-1.93356724722753,-1.91067655430104,-1.88989982509215,-1.88408416831748,
-1.88158630640505,-1.87974060469866,-1.87778569811498,-1.87473488677416,
-1.86555118526279,-1.83804850031722,-1.8262089759111,-1.82337552390372,
-1.82205235419196,-1.82103190246641,-1.8198304039197,-1.8176674096707,-1.80666123908907,
-1.77305041475846,-1.76696226052818,-1.76441982698929,-1.76256667793041,
-1.76085765001004,-1.75852617640153,-1.75259841564563,-1.71899376981925,
-1.70792022772854,-1.70575424469168,-1.70455206256328,-1.70353165673122,
-1.7022093722014,-1.69938073674376,-1.68758403258962,-1.66018665301785,
-1.65089710486703,-1.64783375461423,-1.64587610473106,-1.64403153343535,
-1.64154097548185,-1.63576948054799,-1.61550340513709,-1.59195506464101,
-1.58901572155697,-1.58766662163375,-1.58664094767425,-1.58547091502716,
-1.58339327701468,-1.57293280076989,-1.54813027272964,-1.53445320006987,
-1.53099939773501,-1.52895731307537,-1.52731948571513,-1.52509955957985,
-1.52079742865841,-1.50557223902687,-1.48217508196827,-1.47329301346568,
-1.47124748926732,-1.47007249173212,-1.46915066797477,-1.46784622188022,
-1.46511175757561,-1.44436385079241,-1.41946169081447,-1.41469162418968,
-1.41238009758397,-1.41056005989801,-1.4085189199942,-1.40506957540279,
-1.38968854045139,-1.36869005698206,-1.36317650789737,-1.3558692392975,
-1.35391959916482,-1.35277750305365,-1.35174406844184,-1.35031651507144,
-1.34689030058723,-1.3419096224148,-1.32589075076654,-1.30233948918634,
-1.29752242087111,-1.29520195404796,-1.29338093701748,-1.29134499790602,
-1.2879197982415,-1.27961565155533),.UNSPECIFIED.);
#1603=B_SPLINE_CURVE_WITH_KNOTS('',3,(#117152,#117153,#117154,#117155,#117156,
#117157,#117158,#117159,#117160,#117161,#117162,#117163,#117164,#117165,
#117166,#117167,#117168,#117169,#117170,#117171,#117172,#117173,#117174,
#117175,#117176,#117177,#117178,#117179,#117180,#117181,#117182,#117183,
#117184,#117185,#117186,#117187,#117188,#117189,#117190,#117191,#117192,
#117193,#117194,#117195,#117196,#117197,#117198,#117199,#117200,#117201,
#117202,#117203,#117204,#117205,#117206,#117207,#117208,#117209,#117210,
#117211,#117212,#117213,#117214,#117215,#117216,#117217,#117218,#117219,
#117220,#117221,#117222,#117223,#117224,#117225,#117226,#117227,#117228,
#117229,#117230,#117231,#117232,#117233,#117234,#117235,#117236,#117237,
#117238,#117239,#117240,#117241,#117242,#117243,#117244,#117245,#117246,
#117247,#117248,#117249,#117250,#117251,#117252,#117253,#117254,#117255,
#117256,#117257,#117258,#117259,#117260,#117261,#117262,#117263,#117264,
#117265,#117266,#117267,#117268,#117269,#117270,#117271,#117272,#117273,
#117274,#117275,#117276,#117277,#117278,#117279,#117280,#117281,#117282,
#117283,#117284,#117285,#117286,#117287,#117288,#117289,#117290,#117291,
#117292,#117293,#117294,#117295,#117296,#117297,#117298,#117299,#117300,
#117301,#117302,#117303,#117304,#117305,#117306,#117307,#117308,#117309,
#117310,#117311,#117312,#117313,#117314,#117315,#117316,#117317,#117318,
#117319,#117320,#117321,#117322,#117323,#117324,#117325,#117326,#117327,
#117328,#117329,#117330,#117331,#117332,#117333,#117334,#117335,#117336,
#117337,#117338,#117339,#117340,#117341,#117342,#117343,#117344,#117345,
#117346,#117347,#117348,#117349,#117350,#117351,#117352,#117353,#117354,
#117355,#117356,#117357),.UNSPECIFIED.,.F.,.F.,(4,2,2,2,2,2,2,2,2,2,2,2,
2,2,2,2,2,2,2,2,2,2,2,2,2,2,2,2,2,2,2,2,2,2,2,2,2,2,2,2,2,2,2,2,2,2,2,2,
2,2,2,2,2,2,2,2,2,2,2,2,2,2,2,2,2,2,2,2,2,2,2,2,2,2,2,2,2,2,2,2,2,2,2,2,
2,2,2,2,2,2,2,2,2,2,2,2,2,2,2,2,2,2,4),(-1.48387134362921,-1.48377999702024,
-1.46315723794815,-1.43813415029469,-1.43337170539462,-1.43106250797207,
-1.42924371447017,-1.42720336243635,-1.42375388509515,-1.4083422761872,
-1.38704739695505,-1.37506804135528,-1.37286554620323,-1.37165565777335,
-1.37063677096227,-1.36932683772982,-1.36656102064039,-1.36280830306064,
-1.35286232469363,-1.32972610022241,-1.31846318547549,-1.31517376640477,
-1.31316805463049,-1.31134171861673,-1.30896874229698,-1.30386433522966,
-1.29697777657784,-1.26171163520227,-1.25685812970614,-1.25517188789329,
-1.25419564337877,-1.25315077728875,-1.25165434126708,-1.247788841154,-1.2419201373854,
-1.21962247097283,-1.20193469350586,-1.19832039525319,-1.19622331836809,
-1.19441093373294,-1.19218371788766,-1.18784253369973,-1.17232706365384,
-1.14657216912726,-1.14006904698983,-1.13818127016854,-1.13705305445912,
-1.13601488192044,-1.13455646060163,-1.13093742878364,-1.12557392212731,
-1.10712523158652,-1.08481734015431,-1.08116132413674,-1.07905480238783,
-1.07724293037825,-1.07502729372302,-1.07074417235852,-1.06526128227778,
-1.05199936901524,-1.0329339726823,-1.0233021801812,-1.0212125850191,-1.02002785178597,
-1.01910800514188,-1.01781879106991,-1.01516171667161,-1.01160016095842,
-1.00243615273952,-0.98032154049671,-0.976874022524991,-0.966643428518402,
-0.963476480296804,-0.96149693748438,-0.959661951932099,-0.957229891846341,
-0.951797079031165,-0.927113465870233,-0.907790871667674,-0.904920845167456,
-0.903407487642196,-0.902369759714737,-0.9012644969737,-0.899480953313526,
-0.893236370584017,-0.881336325875826,-0.851477393574428,-0.847588927226387,
-0.845246357168156,-0.843418426218387,-0.841416548376831,-0.838146247005505,
-0.825537529619766,-0.794520541486454,-0.788375703241604,-0.78653492087652,
-0.785416997372842,-0.784373940272735,-0.782888147237172,-0.77909382736156,
-0.773373272137859,-0.752303317712854,-0.741992569555718),.UNSPECIFIED.);
#1604=B_SPLINE_CURVE_WITH_KNOTS('',3,(#117362,#117363,#117364,#117365,#117366,
#117367,#117368,#117369,#117370,#117371,#117372,#117373,#117374,#117375,
#117376,#117377,#117378,#117379,#117380,#117381,#117382,#117383,#117384,
#117385,#117386,#117387,#117388,#117389,#117390,#117391,#117392,#117393,
#117394,#117395,#117396,#117397,#117398,#117399,#117400,#117401,#117402,
#117403,#117404,#117405,#117406,#117407,#117408,#117409,#117410,#117411,
#117412,#117413,#117414,#117415,#117416,#117417,#117418,#117419,#117420,
#117421,#117422,#117423,#117424,#117425,#117426,#117427,#117428,#117429,
#117430,#117431,#117432,#117433,#117434,#117435,#117436,#117437,#117438,
#117439,#117440,#117441,#117442,#117443,#117444,#117445,#117446,#117447,
#117448,#117449,#117450,#117451,#117452,#117453,#117454,#117455,#117456,
#117457,#117458,#117459,#117460,#117461,#117462,#117463,#117464,#117465,
#117466,#117467,#117468,#117469,#117470,#117471,#117472,#117473,#117474,
#117475,#117476,#117477,#117478,#117479,#117480,#117481,#117482,#117483,
#117484,#117485,#117486,#117487,#117488,#117489,#117490,#117491,#117492,
#117493,#117494,#117495,#117496,#117497,#117498,#117499,#117500,#117501,
#117502,#117503,#117504,#117505,#117506,#117507,#117508,#117509,#117510,
#117511,#117512,#117513,#117514,#117515,#117516,#117517,#117518,#117519,
#117520,#117521,#117522,#117523,#117524,#117525,#117526,#117527,#117528,
#117529,#117530,#117531,#117532,#117533,#117534,#117535,#117536,#117537,
#117538,#117539,#117540,#117541,#117542,#117543,#117544,#117545,#117546,
#117547,#117548,#117549,#117550,#117551,#117552,#117553,#117554,#117555,
#117556,#117557,#117558,#117559,#117560,#117561,#117562,#117563,#117564,
#117565,#117566,#117567,#117568,#117569,#117570,#117571,#117572,#117573,
#117574,#117575),.UNSPECIFIED.,.F.,.F.,(4,2,2,2,2,2,2,2,2,2,2,2,2,2,2,2,
2,2,2,2,2,2,2,2,2,2,2,2,2,2,2,2,2,2,2,2,2,2,2,2,2,2,2,2,2,2,2,2,2,2,2,2,
2,2,2,2,2,2,2,2,2,2,2,2,2,2,2,2,2,2,2,2,2,2,2,2,2,2,2,2,2,2,2,2,2,2,2,2,
2,2,2,2,2,2,2,2,2,2,2,2,2,2,2,2,2,2,4),(-2.76333442860709,-2.76333283318913,
-2.76068421758337,-2.75939667777254,-2.75847703137243,-2.75729111816091,
-2.75519622044825,-2.74546055096043,-2.72204380573131,-2.70637394934725,
-2.70291038561152,-2.70086669644073,-2.69904797092557,-2.69674298407476,
-2.6920043013292,-2.66644103123076,-2.65186306973592,-2.64713693765569,
-2.64384289432828,-2.64243781001507,-2.64140809953394,-2.64025606848278,
-2.63825980070012,-2.63042820661761,-2.60660521887019,-2.58935394258163,
-2.58581502241089,-2.58375509013378,-2.58193884709238,-2.57965965269024,
-2.57505486325027,-2.54765370769002,-2.52857370256385,-2.52619431060883,
-2.52496071488969,-2.52394310882237,-2.52266152223482,-2.52062044354352,
-2.50786845093339,-2.50171570027642,-2.48696620136139,-2.47198610863194,
-2.46856010726826,-2.4665244319741,-2.4647041052505,-2.46238514244044,-2.4575735596559,
-2.43384322357729,-2.41794861781208,-2.41298942078168,-2.40957479272484,
-2.40814943301167,-2.40711661658967,-2.40597410768787,-2.40402153207336,
-2.39667421855921,-2.37219136413258,-2.35502329163313,-2.35148777367013,
-2.34942848327379,-2.34761200604477,-2.34533145334806,-2.34072016310816,
-2.31338254103153,-2.29997954768587,-2.2932698555125,-2.29144319627224,
-2.29032841871975,-2.28929572498656,-2.28804280562818,-2.28483351190113,
-2.2669858372421,-2.25102750315509,-2.24205204956476,-2.23583113164242,
-2.23326770717714,-2.23141107475487,-2.22970698791456,-2.22739479686671,
-2.22158245255139,-2.18670116004057,-2.17651391584756,-2.17445007223402,
-2.17328312112535,-2.17225690792152,-2.17090294959828,-2.16782034662982,
-2.14609448340949,-2.12912665379621,-2.12276692297633,-2.11796266727518,
-2.11564478307702,-2.11382422033606,-2.11178715526263,-2.10835608385699,
-2.09512584728045,-2.07301216042403,-2.06387076306505,-2.06031472479081,
-2.05766089717045,-2.05637211286587,-2.05545210550099,-2.05426646501974,
-2.05217370664708,-2.04248713622254,-2.02347769295184,-2.02159988673811),
 .UNSPECIFIED.);
#1605=B_SPLINE_CURVE_WITH_KNOTS('',3,(#117576,#117577,#117578,#117579,#117580,
#117581,#117582,#117583,#117584,#117585,#117586,#117587,#117588,#117589,
#117590,#117591,#117592,#117593,#117594,#117595,#117596,#117597,#117598,
#117599,#117600,#117601,#117602,#117603,#117604,#117605,#117606,#117607,
#117608,#117609,#117610,#117611,#117612,#117613,#117614,#117615,#117616,
#117617,#117618,#117619,#117620,#117621,#117622,#117623,#117624,#117625,
#117626,#117627,#117628,#117629,#117630,#117631,#117632,#117633,#117634,
#117635,#117636,#117637,#117638,#117639,#117640,#117641,#117642,#117643,
#117644,#117645,#117646,#117647,#117648,#117649,#117650,#117651,#117652,
#117653,#117654,#117655,#117656,#117657,#117658,#117659,#117660,#117661,
#117662,#117663,#117664,#117665,#117666,#117667,#117668,#117669,#117670,
#117671,#117672,#117673,#117674,#117675,#117676,#117677,#117678,#117679,
#117680,#117681,#117682,#117683,#117684,#117685,#117686,#117687,#117688,
#117689,#117690,#117691,#117692,#117693,#117694,#117695,#117696,#117697,
#117698,#117699,#117700,#117701,#117702,#117703,#117704,#117705,#117706,
#117707,#117708,#117709,#117710,#117711,#117712,#117713,#117714,#117715,
#117716,#117717,#117718,#117719,#117720,#117721,#117722,#117723,#117724,
#117725,#117726,#117727,#117728,#117729,#117730,#117731,#117732,#117733,
#117734,#117735,#117736,#117737,#117738,#117739,#117740,#117741,#117742,
#117743,#117744,#117745,#117746,#117747,#117748,#117749,#117750,#117751,
#117752,#117753,#117754,#117755,#117756,#117757,#117758,#117759,#117760,
#117761,#117762,#117763,#117764,#117765,#117766,#117767,#117768,#117769,
#117770,#117771,#117772,#117773,#117774,#117775,#117776,#117777,#117778,
#117779,#117780,#117781,#117782,#117783,#117784,#117785,#117786,#117787,
#117788,#117789,#117790,#117791,#117792,#117793,#117794,#117795,#117796,
#117797,#117798,#117799,#117800,#117801,#117802,#117803,#117804,#117805,
#117806,#117807,#117808,#117809,#117810,#117811,#117812,#117813,#117814,
#117815,#117816,#117817,#117818,#117819,#117820,#117821,#117822,#117823,
#117824,#117825,#117826,#117827,#117828,#117829,#117830,#117831),
 .UNSPECIFIED.,.F.,.F.,(4,2,2,2,2,2,2,2,2,2,2,2,2,2,2,2,2,2,2,2,2,2,2,2,
2,2,2,2,2,2,2,2,2,2,2,2,2,2,2,2,2,2,2,2,2,2,2,2,2,2,2,2,2,2,2,2,2,2,2,2,
2,2,2,2,2,2,2,2,2,2,2,2,2,2,2,2,2,2,2,2,2,2,2,2,2,2,2,2,2,2,2,2,2,2,2,2,
2,2,2,2,2,2,2,2,2,2,2,2,2,2,2,2,2,2,2,2,2,2,2,2,2,2,2,2,2,2,2,4),(-0.741992569555718,
-0.73318870284283,-0.729544201474817,-0.72744012484644,-0.725627892883925,
-0.723408709494159,-0.719108690195953,-0.698710957662591,-0.676815334076249,
-0.671082751472562,-0.669287268239637,-0.668179306736096,-0.667130835562251,
-0.665615972295351,-0.661627853229084,-0.635574802920313,-0.615979417880168,
-0.612329099901808,-0.610223693915561,-0.608411508990924,-0.606193886264462,
-0.601901750326023,-0.574660631713768,-0.556146881016924,-0.552949987367722,
-0.551698911756885,-0.55066658726682,-0.549550740848841,-0.547719605691151,
-0.540960731484522,-0.527393877360477,-0.50032045343663,-0.495684922990846,
-0.493399515498577,-0.491582416478181,-0.489525891164254,-0.486003918819416,
-0.469156001182718,-0.443411036230704,-0.436804851844572,-0.434917651980441,
-0.433789425269804,-0.432750961736503,-0.431291737825382,-0.427668733650887,
-0.422297610217772,-0.403800552084539,-0.381543276603508,-0.377887030756206,
-0.375780204774764,-0.373967970320406,-0.371751763604743,-0.367467131324538,
-0.361982062257574,-0.348713292113806,-0.329632105657695,-0.320015336911719,
-0.317926239922814,-0.316741479352543,-0.315821422152957,-0.314531668249012,
-0.311872599352975,-0.308307780362068,-0.299131738821657,-0.276999731355626,
-0.263835630332816,-0.260414487317775,-0.258379646139239,-0.256558803036898,
-0.254237459345754,-0.249414573004908,-0.243021937136065,-0.225901994101888,
-0.204380046542002,-0.201276607848063,-0.199919020965707,-0.198892358721255,
-0.197727576686562,-0.195673638922233,-0.185675182893973,-0.170669577703329,
-0.149049340936359,-0.144188447454653,-0.141859933535519,-0.140038284626923,
-0.139966586884795,-0.139892322074679,-0.139833040363475,-0.13978570294262,
-0.13974788951397,-0.139717673366876,-0.139693520463697,-0.139652268856524,
-0.139612907247453,-0.139575334970087,-0.139539457351,-0.139505185367904,
-0.1394724353068,-0.139441128439938,-0.139411190722675,-0.139382552491046,
-0.13935514818376,-0.139328916082467,-0.139303798069155,-0.139279739377783,
-0.139256688398259,-0.139234596455869,-0.137002123313113,-0.132221133101487,
-0.125843419857235,-0.108793559695371,-0.0871769081942999,-0.0840706230298656,
-0.0827125328941422,-0.0816857959390228,-0.0805212845319382,-0.0784686181302189,
-0.0685069531331131,-0.0556620206200613,-0.0401284664204443,-0.0291025594357174,
-0.0258527632426961,-0.0238549937213871,-0.0220252775992914,-0.0202402506975366,
-0.0179126868020217,-0.0119193789141974,-9.99999999473644E-7),
 .UNSPECIFIED.);
#1606=B_SPLINE_CURVE_WITH_KNOTS('',3,(#117837,#117838,#117839,#117840),
 .UNSPECIFIED.,.F.,.F.,(4,4),(-7.37639246660687E-6,-1.00000002898216E-6),
 .UNSPECIFIED.);
#1607=B_SPLINE_CURVE_WITH_KNOTS('',3,(#117841,#117842,#117843,#117844,#117845,
#117846,#117847,#117848,#117849,#117850,#117851,#117852,#117853,#117854,
#117855,#117856,#117857,#117858,#117859,#117860,#117861,#117862,#117863,
#117864,#117865,#117866,#117867,#117868,#117869,#117870,#117871,#117872,
#117873,#117874,#117875,#117876,#117877,#117878,#117879,#117880,#117881,
#117882,#117883,#117884,#117885,#117886,#117887,#117888,#117889,#117890,
#117891,#117892,#117893,#117894,#117895,#117896,#117897,#117898,#117899,
#117900,#117901,#117902,#117903,#117904,#117905,#117906,#117907,#117908,
#117909,#117910,#117911,#117912,#117913,#117914,#117915,#117916,#117917,
#117918,#117919,#117920,#117921,#117922,#117923,#117924,#117925,#117926,
#117927,#117928,#117929,#117930,#117931,#117932,#117933,#117934,#117935,
#117936,#117937,#117938,#117939,#117940,#117941,#117942,#117943,#117944,
#117945,#117946,#117947,#117948,#117949,#117950,#117951,#117952,#117953,
#117954,#117955,#117956,#117957,#117958,#117959,#117960,#117961,#117962,
#117963,#117964,#117965,#117966,#117967,#117968,#117969,#117970,#117971,
#117972,#117973,#117974,#117975,#117976,#117977,#117978,#117979,#117980,
#117981,#117982,#117983,#117984,#117985,#117986,#117987,#117988,#117989,
#117990,#117991,#117992,#117993,#117994,#117995,#117996,#117997,#117998,
#117999,#118000,#118001,#118002,#118003,#118004,#118005,#118006,#118007,
#118008,#118009,#118010,#118011,#118012,#118013,#118014,#118015,#118016,
#118017,#118018,#118019,#118020,#118021,#118022,#118023,#118024,#118025,
#118026,#118027,#118028,#118029,#118030,#118031,#118032,#118033,#118034,
#118035,#118036,#118037,#118038),.UNSPECIFIED.,.F.,.F.,(4,2,2,2,2,2,2,2,
2,2,2,2,2,2,2,2,2,2,2,2,2,2,2,2,2,2,2,2,2,2,2,2,2,2,2,2,2,2,2,2,2,2,2,2,
2,2,2,2,2,2,2,2,2,2,2,2,2,2,2,2,2,2,2,2,2,2,2,2,2,2,2,2,2,2,2,2,2,2,2,2,
2,2,2,2,2,2,2,2,2,2,2,2,2,2,2,2,2,2,4),(-3.50505994913951,-3.47315403237273,
-3.46775638294582,-3.46412091975709,-3.46266001459946,-3.46162152312737,
-3.46049449643126,-3.45861169729268,-3.45207912793899,-3.42151459665575,
-3.41319486600962,-3.40916149875354,-3.405844748922,-3.40387667570559,-3.40206020637225,
-3.39977588084231,-3.39514355310517,-3.3681740534866,-3.35453116357743,
-3.34775157983184,-3.3459190072022,-3.3448030816471,-3.34377129766263,-3.34252149820814,
-3.33933111088432,-3.32091973657367,-3.3085606603361,-3.2922666791688,-3.28877179370144,
-3.28672145357713,-3.28490398551821,-3.28261027070267,-3.27808552992817,
-3.25045211862615,-3.23210446468634,-3.22939123268064,-3.2280912179084,
-3.2271702655456,-3.22599322079007,-3.2239372834672,-3.21487057319751,-3.1954261927615,
-3.17649417550572,-3.17220033200873,-3.16998265801461,-3.16817081999811,
-3.16606624589857,-3.16241843340655,-3.14299208292389,-3.12218336990926,
-3.11649610308137,-3.11271852186062,-3.11123545095678,-3.11019302404303,
-3.10907437217193,-3.10722972766805,-3.10104586735349,-3.0701072550709,
-3.06175744616636,-3.05585852503814,-3.05334751972596,-3.05150025881259,
-3.04955115883133,-3.04652485756429,-3.03753851975265,-3.00988138395361,
-2.99798279447741,-2.99514317674569,-2.99381919458604,-2.99279906792931,
-2.9915990726788,-2.98944140454965,-2.97854507599638,-2.94491057303494,
-2.93877172904217,-2.93622183601537,-2.93436800015261,-2.93266163317722,
-2.93033888045945,-2.92446095743522,-2.88968186573152,-2.8795037355228,
-2.87744081810128,-2.8762742821151,-2.87524835897929,-2.87389468678925,
-2.87081233432166,-2.84910487704185,-2.83213431964646,-2.82577481456576,
-2.82097102244665,-2.81865364521651,-2.81683360481558,-2.81479725323633,
-2.81136769791102,-2.79805617471201,-2.77598814858421,-2.76688011497481,
-2.76333442860709),.UNSPECIFIED.);
#1608=B_SPLINE_CURVE_WITH_KNOTS('',3,(#118039,#118040,#118041,#118042,#118043,
#118044,#118045,#118046,#118047,#118048,#118049,#118050,#118051,#118052,
#118053,#118054,#118055,#118056,#118057,#118058,#118059,#118060,#118061,
#118062,#118063,#118064,#118065,#118066,#118067,#118068,#118069,#118070,
#118071,#118072,#118073,#118074,#118075,#118076,#118077,#118078,#118079,
#118080,#118081,#118082,#118083,#118084,#118085,#118086,#118087,#118088,
#118089,#118090,#118091,#118092,#118093,#118094,#118095,#118096,#118097,
#118098,#118099,#118100,#118101,#118102,#118103,#118104,#118105,#118106,
#118107,#118108,#118109,#118110,#118111,#118112,#118113,#118114,#118115,
#118116,#118117,#118118,#118119,#118120,#118121,#118122,#118123,#118124,
#118125,#118126,#118127,#118128,#118129,#118130,#118131,#118132,#118133,
#118134,#118135,#118136,#118137,#118138,#118139,#118140,#118141,#118142,
#118143,#118144,#118145,#118146,#118147,#118148,#118149,#118150,#118151,
#118152,#118153,#118154,#118155,#118156,#118157,#118158,#118159,#118160,
#118161,#118162,#118163,#118164,#118165,#118166,#118167,#118168,#118169,
#118170,#118171,#118172,#118173,#118174,#118175,#118176,#118177,#118178,
#118179,#118180,#118181,#118182,#118183,#118184,#118185,#118186,#118187,
#118188,#118189,#118190,#118191,#118192,#118193,#118194,#118195,#118196,
#118197,#118198,#118199,#118200,#118201,#118202,#118203,#118204,#118205,
#118206,#118207,#118208,#118209,#118210,#118211,#118212,#118213,#118214,
#118215,#118216,#118217,#118218,#118219,#118220,#118221,#118222,#118223,
#118224,#118225,#118226,#118227,#118228,#118229,#118230,#118231,#118232,
#118233,#118234,#118235,#118236,#118237,#118238,#118239,#118240,#118241,
#118242,#118243,#118244,#118245,#118246,#118247,#118248,#118249,#118250,
#118251,#118252,#118253,#118254,#118255,#118256,#118257,#118258,#118259,
#118260,#118261,#118262,#118263,#118264,#118265,#118266),.UNSPECIFIED.,
 .F.,.F.,(4,2,2,2,2,2,2,2,2,2,2,2,2,2,2,2,2,2,2,2,2,2,2,2,2,2,2,2,2,2,2,
2,2,2,2,2,2,2,2,2,2,2,2,2,2,2,2,2,2,2,2,2,2,2,2,2,2,2,2,2,2,2,2,2,2,2,2,
2,2,2,2,2,2,2,2,2,2,2,2,2,2,2,2,2,2,2,2,2,2,2,2,2,2,2,2,2,2,2,2,2,2,2,2,
2,2,2,2,2,2,2,2,2,2,4),(-2.96761844200665,-2.93767638030957,-2.93548019648945,
-2.9336592562878,-2.93254600130476,-2.9315131451599,-2.93025844008825,-2.92716409765907,
-2.90650829392983,-2.8888379059781,-2.8823315150323,-2.87749151310647,-2.8753219616522,
-2.87527613194927,-2.87522753684484,-2.87517583173089,-2.87512061413181,
-2.87329858116516,-2.87127510210733,-2.86790350393687,-2.85550729588206,
-2.82989684850021,-2.82244673261111,-2.81933798348305,-2.81694664596374,
-2.81571078257054,-2.81469354533725,-2.81341526634235,-2.8113846499091,
-2.7982052469369,-2.79242601858666,-2.77758943642391,-2.76271667977566,
-2.75929738765832,-2.75726349489495,-2.7554434059559,-2.75312289383221,
-2.74830125028984,-2.72496885149802,-2.708776646864,-2.70376743420223,-2.70032738663267,
-2.69889804992327,-2.69786482227434,-2.69672460861366,-2.69478164684512,
-2.68754275776878,-2.66678912334879,-2.64703561785448,-2.64276764051325,
-2.64055537390903,-2.63874405581574,-2.63663568557671,-2.63297010513757,
-2.61132181153184,-2.59543763763128,-2.58808364660803,-2.58500168474834,
-2.58262637971013,-2.58139379988205,-2.58037641061561,-2.57909434548578,
-2.57705114926448,-2.56325661067326,-2.55807480885457,-2.54290715044706,
-2.52836819659951,-2.52496852603686,-2.52293885483448,-2.52111790244483,
-2.51878988367364,-2.51392857361376,-2.4929891476698,-2.47496368494581,
-2.46966307373379,-2.46607588426237,-2.4646226941432,-2.4635855664214,-2.46245556543585,
-2.46055906021209,-2.45385008040142,-2.44729131397717,-2.42663083758384,
-2.41129714329299,-2.40785189514679,-2.40581236922416,-2.40399327843769,
-2.40168229466265,-2.39691101489519,-2.37205368528113,-2.35125224167795,
-2.348517985985,-2.34721399762815,-2.3461954232727,-2.34498074761048,-2.34275704041747,
-2.32968049854632,-2.32380163528694,-2.30871456669348,-2.29405779654679,
-2.29065093418213,-2.28861962433217,-2.28679885511071,-2.28447335269856,
-2.27962588423449,-2.25870320887828,-2.24064482911579,-2.23533909950807,
-2.23174929490462,-2.23029563194362,-2.22925837447632,-2.22812845793281,
-2.22623254049717,-2.22593322706991),.UNSPECIFIED.);
#1609=B_SPLINE_CURVE_WITH_KNOTS('',3,(#118271,#118272,#118273,#118274,#118275,
#118276,#118277,#118278,#118279,#118280,#118281,#118282,#118283,#118284,
#118285,#118286,#118287,#118288,#118289,#118290,#118291,#118292,#118293,
#118294,#118295,#118296,#118297,#118298,#118299,#118300,#118301,#118302,
#118303,#118304,#118305,#118306,#118307,#118308,#118309,#118310,#118311,
#118312,#118313,#118314,#118315,#118316,#118317,#118318,#118319,#118320,
#118321,#118322,#118323,#118324,#118325,#118326,#118327,#118328,#118329,
#118330,#118331,#118332,#118333,#118334,#118335,#118336,#118337,#118338,
#118339,#118340,#118341,#118342,#118343,#118344,#118345,#118346,#118347,
#118348,#118349,#118350,#118351,#118352,#118353,#118354,#118355,#118356,
#118357,#118358,#118359,#118360,#118361,#118362,#118363,#118364,#118365,
#118366,#118367,#118368,#118369,#118370,#118371,#118372,#118373,#118374,
#118375,#118376,#118377,#118378,#118379,#118380,#118381,#118382,#118383,
#118384,#118385,#118386,#118387,#118388,#118389,#118390,#118391,#118392,
#118393,#118394,#118395,#118396,#118397,#118398,#118399,#118400,#118401,
#118402,#118403,#118404,#118405,#118406,#118407,#118408,#118409,#118410,
#118411,#118412,#118413,#118414,#118415,#118416,#118417,#118418,#118419,
#118420,#118421,#118422,#118423,#118424,#118425,#118426,#118427,#118428,
#118429,#118430,#118431,#118432,#118433,#118434,#118435,#118436,#118437,
#118438,#118439,#118440,#118441,#118442,#118443,#118444,#118445,#118446,
#118447,#118448,#118449,#118450,#118451,#118452,#118453,#118454,#118455,
#118456,#118457,#118458,#118459,#118460,#118461,#118462,#118463,#118464,
#118465,#118466,#118467,#118468,#118469,#118470,#118471,#118472,#118473,
#118474,#118475,#118476,#118477,#118478,#118479,#118480,#118481,#118482,
#118483,#118484,#118485,#118486,#118487,#118488,#118489,#118490,#118491,
#118492,#118493,#118494),.UNSPECIFIED.,.F.,.F.,(4,2,2,2,2,2,2,2,2,2,2,2,
2,2,2,2,2,2,2,2,2,2,2,2,2,2,2,2,2,2,2,2,2,2,2,2,2,2,2,2,2,2,2,2,2,2,2,2,
2,2,2,2,2,2,2,2,2,2,2,2,2,2,2,2,2,2,2,2,2,2,2,2,2,2,2,2,2,2,2,2,2,2,2,2,
2,2,2,2,2,2,2,2,2,2,2,2,2,2,2,2,2,2,2,2,2,2,2,2,2,2,2,4),(-0.742112763578935,
-0.727061281829163,-0.722288707659859,-0.719976552121643,-0.718156277868983,
-0.716115142797653,-0.712666468742061,-0.697302911406439,-0.676462712432556,
-0.66399562117025,-0.661963327744964,-0.660684073406103,-0.659666095868948,
-0.658429341915493,-0.656036286403435,-0.652925557060773,-0.645471068072106,
-0.629664810654427,-0.608098954927716,-0.604434092649939,-0.602324978154874,
-0.600512332017134,-0.598297568700903,-0.594021944671633,-0.572450882452868,
-0.547745965683558,-0.544883050965748,-0.543568324645918,-0.542546455406132,
-0.541354095005308,-0.539173162230857,-0.526165755512889,-0.498395084105655,
-0.48952989129908,-0.486517177448293,-0.484570153612476,-0.482720077252544,
-0.480197699155873,-0.474235583314371,-0.441046239068091,-0.429448447310168,
-0.427260622291499,-0.42605338083039,-0.42503324097333,-0.423717177313737,
-0.420922601092093,-0.417119811234962,-0.406967813557909,-0.383888849225869,
-0.372775422093107,-0.36951646000599,-0.367516230418958,-0.365686331015219,
-0.363296383097122,-0.358105309888169,-0.351066129489304,-0.326977507093747,
-0.312343672992127,-0.310283518804771,-0.308995810007337,-0.307977354236198,
-0.306747568929113,-0.304388912333526,-0.301335672727778,-0.268385915888379,
-0.25576465302906,-0.252376083045881,-0.250347846979684,-0.248524922392752,
-0.246189851639557,-0.241296587464822,-0.234782495934772,-0.217085539253761,
-0.196417331824234,-0.193319624540132,-0.192063716207234,-0.191029941686005,
-0.189915746832888,-0.188093350758696,-0.181437709394761,-0.168221536479482,
-0.140578045065258,-0.136057031252293,-0.133763207470923,-0.131944696436363,
-0.13186632269449,-0.131803688724853,-0.13175369384992,-0.131713823231323,
-0.131682047934474,-0.129585548653185,-0.127332074427384,-0.123815420715499,
-0.117008595736625,-0.0978331338304588,-0.079280032901386,-0.0763948936646742,
-0.0748772570631236,-0.0738383714654832,-0.0727337095512854,-0.0709544215164448,
-0.0647593847788353,-0.0530138957397964,-0.0346913996586432,-0.0218253839118807,
-0.0182147852973583,-0.016117783036972,-0.0143078318254824,-0.0125677029833169,
-0.0103865823899228,-0.00631987000565794,-7.37639246660687E-6),
 .UNSPECIFIED.);
#1610=B_SPLINE_CURVE_WITH_KNOTS('',3,(#118495,#118496,#118497,#118498,#118499,
#118500,#118501,#118502,#118503,#118504,#118505,#118506,#118507,#118508,
#118509,#118510,#118511,#118512,#118513,#118514,#118515,#118516,#118517,
#118518,#118519,#118520,#118521,#118522,#118523,#118524,#118525,#118526,
#118527,#118528,#118529,#118530,#118531,#118532,#118533,#118534,#118535,
#118536,#118537,#118538,#118539,#118540,#118541,#118542,#118543,#118544,
#118545,#118546,#118547,#118548,#118549,#118550,#118551,#118552,#118553,
#118554,#118555,#118556,#118557,#118558,#118559,#118560,#118561,#118562,
#118563,#118564,#118565,#118566,#118567,#118568,#118569,#118570,#118571,
#118572,#118573,#118574,#118575,#118576,#118577,#118578,#118579,#118580,
#118581,#118582,#118583,#118584,#118585,#118586,#118587,#118588,#118589,
#118590,#118591,#118592,#118593,#118594,#118595,#118596,#118597,#118598,
#118599,#118600,#118601,#118602,#118603,#118604,#118605,#118606,#118607,
#118608,#118609,#118610,#118611,#118612,#118613,#118614,#118615,#118616,
#118617,#118618,#118619,#118620,#118621,#118622,#118623,#118624,#118625,
#118626,#118627,#118628,#118629,#118630,#118631,#118632,#118633,#118634,
#118635,#118636,#118637,#118638,#118639,#118640,#118641,#118642,#118643,
#118644,#118645,#118646,#118647,#118648,#118649,#118650,#118651,#118652,
#118653,#118654,#118655,#118656,#118657,#118658,#118659,#118660,#118661,
#118662,#118663,#118664,#118665,#118666,#118667,#118668,#118669,#118670,
#118671,#118672,#118673,#118674,#118675,#118676,#118677,#118678,#118679,
#118680,#118681,#118682,#118683,#118684,#118685,#118686,#118687,#118688,
#118689,#118690,#118691,#118692,#118693,#118694,#118695,#118696),
 .UNSPECIFIED.,.F.,.F.,(4,2,2,2,2,2,2,2,2,2,2,2,2,2,2,2,2,2,2,2,2,2,2,2,
2,2,2,2,2,2,2,2,2,2,2,2,2,2,2,2,2,2,2,2,2,2,2,2,2,2,2,2,2,2,2,2,2,2,2,2,
2,2,2,2,2,2,2,2,2,2,2,2,2,2,2,2,2,2,2,2,2,2,2,2,2,2,2,2,2,2,2,2,2,2,2,2,
2,2,2,2,4),(-2.22593322706991,-2.21953112565396,-2.21297056419295,-2.20668574539589,
-2.19166772652078,-2.1769127101204,-2.17350000824533,-2.17146740944946,
-2.16964684772091,-2.16732348817461,-2.16248752947384,-2.13999724481421,
-2.12559948620941,-2.1157953171276,-2.11375217469596,-2.11258997203901,
-2.11156309561059,-2.11020203273382,-2.10707711764329,-2.08624076422116,
-2.06868339382152,-2.0621998217347,-2.05732433500123,-2.05499349847257,
-2.05317204991695,-2.0511435828802,-2.04775016493561,-2.03503194109297,
-2.00214006565418,-1.99910871877699,-1.99676368690714,-1.99553714979222,
-1.99451915022935,-1.99322922796777,-1.99116040290091,-1.97552361412581,
-1.97214598083311,-1.95683519985974,-1.94248622408338,-1.93909738044412,
-1.93706968354457,-1.93524769324632,-1.93291445424272,-1.92802750292512,
-1.90665816348616,-1.8889938903102,-1.88374754623271,-1.8801872460834,-1.87873810635213,
-1.87770142886847,-1.87656925829213,-1.87466383019428,-1.86785708755501,
-1.86131259863678,-1.84073047145756,-1.8254027251819,-1.82195705553556,
-1.81991706735598,-1.81809743346858,-1.81578558127099,-1.81101185082757,
-1.78617368158807,-1.76534201698589,-1.76260677022686,-1.76130236840509,
-1.76028349954876,-1.75906850665928,-1.75684430159575,-1.74379854502861,
-1.73788596356335,-1.72307132868658,-1.70815857599283,-1.70473603071085,
-1.70270095572413,-1.70088027528091,-1.69855964985648,-1.69374016171822,
-1.6702369877515,-1.64815745880669,-1.64540977591381,-1.64410294295502,
-1.6430838515852,-1.64187059085465,-1.6396544127336,-1.62739774240837,-1.60705133675503,
-1.59105274609926,-1.58757148371704,-1.58552365748868,-1.58370509907058,
-1.58140554079275,-1.5766970335215,-1.5505562822561,-1.53028006958655,-1.52794301035101,
-1.52671798131452,-1.52569967968587,-1.52440740454272,-1.52233113542177,
-1.50493410620379,-1.48402414970713),.UNSPECIFIED.);
#1611=B_SPLINE_CURVE_WITH_KNOTS('',3,(#118701,#118702,#118703,#118704,#118705,
#118706,#118707,#118708,#118709,#118710,#118711,#118712,#118713,#118714,
#118715,#118716,#118717,#118718,#118719,#118720,#118721,#118722,#118723,
#118724,#118725,#118726,#118727,#118728,#118729,#118730,#118731,#118732,
#118733,#118734,#118735,#118736,#118737,#118738,#118739,#118740,#118741,
#118742,#118743,#118744,#118745,#118746,#118747,#118748,#118749,#118750,
#118751,#118752,#118753,#118754,#118755,#118756,#118757,#118758,#118759,
#118760,#118761,#118762,#118763,#118764,#118765,#118766,#118767,#118768,
#118769,#118770,#118771,#118772,#118773,#118774,#118775,#118776,#118777,
#118778,#118779,#118780,#118781,#118782,#118783,#118784,#118785,#118786,
#118787,#118788,#118789,#118790,#118791,#118792,#118793,#118794,#118795,
#118796,#118797,#118798,#118799,#118800,#118801,#118802,#118803,#118804,
#118805,#118806,#118807,#118808,#118809,#118810,#118811,#118812,#118813,
#118814,#118815,#118816,#118817,#118818,#118819,#118820,#118821,#118822,
#118823,#118824,#118825,#118826,#118827,#118828,#118829,#118830,#118831,
#118832,#118833,#118834,#118835,#118836,#118837,#118838,#118839,#118840,
#118841,#118842,#118843,#118844,#118845,#118846,#118847,#118848,#118849,
#118850,#118851,#118852,#118853,#118854,#118855,#118856,#118857,#118858,
#118859,#118860,#118861,#118862,#118863,#118864,#118865,#118866,#118867,
#118868,#118869,#118870,#118871,#118872,#118873,#118874,#118875,#118876,
#118877,#118878,#118879,#118880,#118881,#118882,#118883,#118884,#118885,
#118886,#118887,#118888,#118889,#118890,#118891,#118892,#118893,#118894,
#118895,#118896,#118897,#118898,#118899,#118900,#118901,#118902,#118903,
#118904,#118905,#118906,#118907,#118908,#118909,#118910,#118911,#118912,
#118913,#118914,#118915,#118916,#118917,#118918,#118919,#118920),
 .UNSPECIFIED.,.F.,.F.,(4,2,2,2,2,2,2,2,2,2,2,2,2,2,2,2,2,2,2,2,2,2,2,2,
2,2,2,2,2,2,2,2,2,2,2,2,2,2,2,2,2,2,2,2,2,2,2,2,2,2,2,2,2,2,2,2,2,2,2,2,
2,2,2,2,2,2,2,2,2,2,2,2,2,2,2,2,2,2,2,2,2,2,2,2,2,2,2,2,2,2,2,2,2,2,2,2,
2,2,2,2,2,2,2,2,2,2,2,2,2,4),(-1.48419021204294,-1.48218378775787,-1.48101315824072,
-1.48009053040463,-1.47877941151569,-1.47601000501141,-1.47225160644337,
-1.46228499926441,-1.43911667662998,-1.42789216537953,-1.42460483990733,
-1.42259874951587,-1.42077098719917,-1.41839459796471,-1.41327651641115,
-1.40636693667328,-1.37070917493401,-1.36617581273004,-1.3645333229462,
-1.36356520205338,-1.36251274873407,-1.36097887816494,-1.35686241463103,
-1.35046119277678,-1.33355109572006,-1.31140156200382,-1.30774455349713,
-1.30563705480767,-1.30382409477266,-1.3016068057226,-1.29731940696517,
-1.29183032348863,-1.27854826632138,-1.25943090419546,-1.24986193966554,
-1.24777487645582,-1.2465902982298,-1.24566977766055,-1.24437856481664,
-1.24171353968761,-1.23813870739911,-1.22892416044852,-1.22713125957704,
-1.20301083681601,-1.19311422522434,-1.18998242293793,-1.18800971988834,
-1.18617073171274,-1.18371779040802,-1.17816969209402,-1.15874058175379,
-1.13493115936447,-1.13139254209156,-1.13005000383784,-1.12908852242119,
-1.12802972518176,-1.12646409826591,-1.12212107126218,-1.11522035782837,
-1.07924233184699,-1.07410278051337,-1.07174787986452,-1.06991742105179,
-1.06791993085555,-1.06467304669819,-1.05238585055491,-1.03800737060559,
-1.01696169390139,-1.01384527862247,-1.01248518659566,-1.01145792746855,
-1.01029394739306,-1.00824469117645,-0.998342120341819,-0.983643346582729,
-0.961583123922189,-0.956739850300681,-0.954414240329411,-0.952592443832404,
-0.950559003523848,-0.947146172610424,-0.932416884743305,-0.917357368760218,
-0.911109752915589,-0.904546648676946,-0.897787864690021,-0.895886057620949,
-0.894754397968665,-0.893716891405269,-0.89226475358036,-0.888687907973293,
-0.883409779187262,-0.865538288076789,-0.844397515202518,-0.839545615215156,
-0.837218390249218,-0.835396426255118,-0.833363932830224,-0.829955430603124,
-0.815299054069314,-0.800188327554611,-0.794245652075295,-0.781213164006394,
-0.778987212211267,-0.777771576307993,-0.776752345280325,-0.775447686036176,
-0.772712548625201,-0.751918186273301,-0.742112763578935),.UNSPECIFIED.);
#1612=B_SPLINE_CURVE_WITH_KNOTS('',3,(#118921,#118922,#118923,#118924,#118925,
#118926,#118927,#118928,#118929,#118930,#118931,#118932,#118933,#118934,
#118935,#118936,#118937,#118938,#118939,#118940,#118941,#118942,#118943,
#118944,#118945,#118946,#118947,#118948,#118949,#118950,#118951,#118952,
#118953,#118954,#118955,#118956,#118957,#118958,#118959,#118960,#118961,
#118962,#118963,#118964,#118965,#118966,#118967,#118968,#118969,#118970,
#118971,#118972,#118973,#118974,#118975,#118976,#118977,#118978,#118979,
#118980,#118981,#118982,#118983,#118984,#118985,#118986,#118987,#118988,
#118989,#118990,#118991,#118992,#118993,#118994,#118995,#118996,#118997,
#118998,#118999,#119000,#119001,#119002,#119003,#119004,#119005,#119006,
#119007,#119008,#119009,#119010,#119011,#119012,#119013,#119014,#119015,
#119016,#119017,#119018,#119019,#119020,#119021,#119022,#119023,#119024,
#119025,#119026,#119027,#119028,#119029,#119030,#119031,#119032,#119033,
#119034,#119035,#119036,#119037,#119038,#119039,#119040,#119041,#119042,
#119043,#119044,#119045,#119046,#119047,#119048,#119049,#119050,#119051,
#119052,#119053,#119054,#119055,#119056,#119057,#119058,#119059,#119060,
#119061,#119062,#119063,#119064,#119065,#119066,#119067,#119068,#119069,
#119070,#119071,#119072,#119073,#119074,#119075,#119076,#119077,#119078,
#119079,#119080,#119081,#119082,#119083,#119084,#119085,#119086,#119087,
#119088,#119089,#119090,#119091,#119092,#119093,#119094,#119095,#119096,
#119097,#119098,#119099,#119100,#119101,#119102,#119103,#119104,#119105,
#119106,#119107,#119108,#119109,#119110,#119111,#119112,#119113,#119114,
#119115,#119116,#119117,#119118,#119119,#119120,#119121,#119122,#119123,
#119124,#119125,#119126,#119127,#119128,#119129,#119130,#119131,#119132,
#119133,#119134,#119135,#119136),.UNSPECIFIED.,.F.,.F.,(4,2,2,2,2,2,2,2,
2,2,2,2,2,2,2,2,2,2,2,2,2,2,2,2,2,2,2,2,2,2,2,2,2,2,2,2,2,2,2,2,2,2,2,2,
2,2,2,2,2,2,2,2,2,2,2,2,2,2,2,2,2,2,2,2,2,2,2,2,2,2,2,2,2,2,2,2,2,2,2,2,
2,2,2,2,2,2,2,2,2,2,2,2,2,2,2,2,2,2,2,2,2,2,2,2,2,2,2,4),(-1.48402414970713,
-1.48386902271208,-1.47329677017161,-1.47009145873531,-1.46810329736781,
-1.46627059428127,-1.46385672872211,-1.45852924500984,-1.45124389717394,
-1.42934011570267,-1.41299688403725,-1.41092631703839,-1.40963573774516,
-1.40861750151737,-1.40739101152478,-1.40504699141599,-1.38507466244869,
-1.35863008259914,-1.35394363573545,-1.35164826065279,-1.34983004600115,
-1.34777947376678,-1.34428575295072,-1.32804275936578,-1.31835679519701,
-1.29702186517173,-1.29391946443402,-1.2925620380903,-1.29153537611592,
-1.29037045358503,-1.28831595315114,-1.27830755480595,-1.26327037388336,
-1.24170341859183,-1.23683462937683,-1.23450459447146,-1.23268273424493,
-1.23065273978464,-1.22725419546221,-1.21275462026739,-1.19753334629008,
-1.19256519393886,-1.17852556835761,-1.17647654750295,-1.17519244799117,
-1.17417455072479,-1.17294268915125,-1.17057248190465,-1.16749969414661,
-1.13451096006151,-1.12196447640015,-1.11858174215839,-1.11655531091684,
-1.11473295889365,-1.11239717435145,-1.10749697314075,-1.10097009783791,
-1.08320735078966,-1.06264185319504,-1.05980702702136,-1.05830276994263,
-1.05726665359571,-1.05615823719905,-1.05436068926936,-1.04797011243133,
-1.03561416416639,-1.00655033194157,-1.00256819054537,-1.00019875669666,
-0.99836683666612,-0.996377596164948,-0.993166245935335,-0.981313397103145,
-0.955301253663928,-0.949413257716968,-0.943289635095021,-0.941451072565698,
-0.940333616646599,-0.939290276415498,-0.937803050749906,-0.933999533416799,
-0.928260039157953,-0.907039523288692,-0.888100935658694,-0.884458712495661,
-0.882355104923363,-0.880542778844311,-0.878322851169783,-0.874019351741301,
-0.858781886714686,-0.835176779061912,-0.833679631812814,-0.826304893164126,
-0.824349717177918,-0.823206544320609,-0.822173766398724,-0.820749403607453,
-0.817341491304575,-0.812396317308845,-0.796585544834842,-0.772746656663903,
-0.767937769357755,-0.765619119899626,-0.763798612446761,-0.761762300022572,
-0.758334204017837,-0.743328397463449,-0.741997157565065),.UNSPECIFIED.);
#1613=B_SPLINE_CURVE_WITH_KNOTS('',3,(#119141,#119142,#119143,#119144,#119145,
#119146,#119147,#119148,#119149,#119150,#119151,#119152,#119153,#119154,
#119155,#119156,#119157,#119158,#119159,#119160,#119161,#119162,#119163,
#119164,#119165,#119166,#119167,#119168,#119169,#119170,#119171,#119172,
#119173,#119174,#119175,#119176,#119177,#119178,#119179,#119180,#119181,
#119182,#119183,#119184,#119185,#119186,#119187,#119188,#119189,#119190,
#119191,#119192,#119193,#119194,#119195,#119196,#119197,#119198,#119199,
#119200,#119201,#119202,#119203,#119204,#119205,#119206,#119207,#119208,
#119209,#119210,#119211,#119212,#119213,#119214,#119215,#119216,#119217,
#119218,#119219,#119220,#119221,#119222,#119223,#119224,#119225,#119226,
#119227,#119228,#119229,#119230,#119231,#119232,#119233,#119234,#119235,
#119236,#119237,#119238,#119239,#119240,#119241,#119242,#119243,#119244,
#119245,#119246,#119247,#119248,#119249,#119250,#119251,#119252,#119253,
#119254,#119255,#119256,#119257,#119258,#119259,#119260,#119261,#119262,
#119263,#119264,#119265,#119266,#119267,#119268,#119269,#119270,#119271,
#119272,#119273,#119274,#119275,#119276,#119277,#119278,#119279,#119280,
#119281,#119282,#119283,#119284,#119285,#119286,#119287,#119288,#119289,
#119290,#119291,#119292,#119293,#119294,#119295,#119296,#119297,#119298,
#119299,#119300,#119301,#119302,#119303,#119304,#119305,#119306,#119307,
#119308,#119309,#119310,#119311,#119312,#119313,#119314,#119315,#119316,
#119317,#119318,#119319,#119320,#119321,#119322,#119323,#119324,#119325,
#119326,#119327,#119328,#119329,#119330,#119331,#119332,#119333,#119334,
#119335,#119336,#119337,#119338,#119339,#119340,#119341,#119342,#119343,
#119344,#119345,#119346),.UNSPECIFIED.,.F.,.F.,(4,2,2,2,2,2,2,2,2,2,2,2,
2,2,2,2,2,2,2,2,2,2,2,2,2,2,2,2,2,2,2,2,2,2,2,2,2,2,2,2,2,2,2,2,2,2,2,2,
2,2,2,2,2,2,2,2,2,2,2,2,2,2,2,2,2,2,2,2,2,2,2,2,2,2,2,2,2,2,2,2,2,2,2,2,
2,2,2,2,2,2,2,2,2,2,2,2,2,2,2,2,2,2,4),(-2.22608676643451,-2.20726309333763,
-2.1937123379699,-2.18695881985012,-2.18512815033227,-2.18401241697167,
-2.18298003559482,-2.18172871979647,-2.17853017582475,-2.16075985761862,
-2.14494711928046,-2.13582836423958,-2.12953504509966,-2.12696004683478,
-2.12510121517364,-2.1233993485002,-2.12065573164219,-2.11376224262234,
-2.08689525161069,-2.07146002627653,-2.06863393377325,-2.06731222386601,
-2.06629198356956,-2.06508965528965,-2.06292263589511,-2.05181528796755,
-2.02561483179469,-2.01372958303666,-2.01051548053703,-2.0085254914483,
-2.00669350536859,-2.00432485095476,-2.00034590751655,-1.97124001084136,
-1.9588983175329,-1.95251256562008,-1.95071530670252,-1.94960686956509,
-1.94857054382749,-1.94706568375257,-1.9442289364259,-1.92374976668429,
-1.90904750276677,-1.89661902115088,-1.89336185253027,-1.8913624303113,
-1.88953307745642,-1.88718359411602,-1.88327223080929,-1.853578629355,-1.83681731374779,
-1.83414344894614,-1.83285070285945,-1.83193021346715,-1.83074722401876,
-1.82866644601452,-1.81920397570096,-1.80003238027993,-1.78673538177809,
-1.78124279493265,-1.77695312398073,-1.77473568364263,-1.7729230953229,
-1.77081658769254,-1.76716272455683,-1.74459620798524,-1.72632685790298,
-1.7209886938557,-1.7173823093171,-1.71592556479101,-1.71488738365343,-1.71375782010907,
-1.71186514152084,-1.7052065218983,-1.68402963362545,-1.66400989463197,
-1.65973937647502,-1.65752581492613,-1.65571343598548,-1.65360382095896,
-1.64993602071104,-1.62862459442818,-1.60936723860382,-1.60388647319068,
-1.60020945106807,-1.59874157348474,-1.5977014928129,-1.59657637431063,
-1.59470381433327,-1.58825446612154,-1.58116121273384,-1.5750856244477,
-1.56002521396891,-1.54532294391199,-1.541912198669,-1.53987938693197,-1.53805776791121,
-1.53573185373234,-1.53088599402871,-1.50888621928476,-1.49413085231136,
-1.48421012225063,-1.48419021204294),.UNSPECIFIED.);
#1614=B_SPLINE_CURVE_WITH_KNOTS('',3,(#119347,#119348,#119349,#119350,#119351,
#119352,#119353,#119354,#119355,#119356,#119357,#119358,#119359,#119360,
#119361,#119362,#119363,#119364,#119365,#119366,#119367,#119368,#119369,
#119370,#119371,#119372,#119373,#119374,#119375,#119376,#119377,#119378,
#119379,#119380,#119381,#119382,#119383,#119384,#119385,#119386,#119387,
#119388,#119389,#119390,#119391,#119392,#119393,#119394,#119395,#119396,
#119397,#119398,#119399,#119400,#119401,#119402,#119403,#119404,#119405,
#119406,#119407,#119408,#119409,#119410,#119411,#119412,#119413,#119414,
#119415,#119416,#119417,#119418,#119419,#119420,#119421,#119422,#119423,
#119424,#119425,#119426,#119427,#119428,#119429,#119430,#119431,#119432,
#119433,#119434,#119435,#119436,#119437,#119438,#119439,#119440,#119441,
#119442,#119443,#119444,#119445,#119446,#119447,#119448,#119449,#119450,
#119451,#119452,#119453,#119454,#119455,#119456,#119457,#119458,#119459,
#119460,#119461,#119462,#119463,#119464,#119465,#119466,#119467,#119468,
#119469,#119470,#119471,#119472,#119473,#119474,#119475,#119476,#119477,
#119478,#119479,#119480,#119481,#119482,#119483,#119484,#119485,#119486,
#119487,#119488,#119489,#119490,#119491,#119492,#119493,#119494,#119495,
#119496,#119497,#119498,#119499,#119500,#119501,#119502,#119503,#119504,
#119505,#119506,#119507,#119508,#119509,#119510,#119511,#119512,#119513,
#119514,#119515,#119516,#119517,#119518,#119519,#119520,#119521,#119522,
#119523,#119524,#119525,#119526,#119527,#119528,#119529,#119530,#119531,
#119532,#119533,#119534,#119535,#119536,#119537,#119538,#119539,#119540,
#119541,#119542,#119543,#119544,#119545,#119546,#119547,#119548,#119549,
#119550,#119551,#119552,#119553,#119554,#119555,#119556,#119557,#119558,
#119559,#119560,#119561,#119562,#119563,#119564,#119565,#119566),
 .UNSPECIFIED.,.F.,.F.,(4,2,2,2,2,2,2,2,2,2,2,2,2,2,2,2,2,2,2,2,2,2,2,2,
2,2,2,2,2,2,2,2,2,2,2,2,2,2,2,2,2,2,2,2,2,2,2,2,2,2,2,2,2,2,2,2,2,2,2,2,
2,2,2,2,2,2,2,2,2,2,2,2,2,2,2,2,2,2,2,2,2,2,2,2,2,2,2,2,2,2,2,2,2,2,2,2,
2,2,2,2,2,2,2,2,2,2,2,2,2,4),(-0.741997157565065,-0.728572633296522,-0.722291508979075,
-0.715722384418041,-0.709001205149917,-0.707103099315564,-0.705972493802639,
-0.704935074437573,-0.703481857250529,-0.699896439939264,-0.694600682114955,
-0.676609818948818,-0.653737675961877,-0.650071834712697,-0.647962905077023,
-0.646150865642299,-0.643937416035677,-0.639666211520541,-0.619574407583386,
-0.598283007078139,-0.591766262696187,-0.589880478273266,-0.588752562278465,
-0.587713963648858,-0.586253956617637,-0.582626015483684,-0.577244956375353,
-0.558679987688215,-0.536506076107584,-0.532850532802642,-0.530743861647133,
-0.528931613735612,-0.526715205973186,-0.522429589952349,-0.516942905714233,
-0.503667923990456,-0.48456923586704,-0.474976915285377,-0.472889131984864,
-0.471704667210622,-0.470784564721378,-0.469494392033032,-0.466833179027015,
-0.463264628586587,-0.454073693161898,-0.453215635711422,-0.430301112416084,
-0.418600480856284,-0.415283609643857,-0.413271355113976,-0.411445613406979,
-0.409082723854666,-0.404036991037775,-0.397255230843478,-0.378208812850448,
-0.359479489619188,-0.356595311326521,-0.355078156793945,-0.354039596801582,
-0.352935299794781,-0.351156664812063,-0.344964769249125,-0.333227625140076,
-0.304399024096692,-0.299274495127334,-0.296922794975267,-0.295093330602675,
-0.293095427075587,-0.289844492602138,-0.277495408096522,-0.262975474257854,
-0.242164261102668,-0.239035374043058,-0.237673404462222,-0.236646192914751,
-0.235483992690002,-0.233441733337095,-0.223659387130257,-0.209330127320179,
-0.186759042122723,-0.181923788104845,-0.179600194733689,-0.177779192358314,
-0.175745834492589,-0.172331221563639,-0.157557695393221,-0.142531306356899,
-0.125060732804245,-0.121940415051461,-0.120664111979058,-0.119665820805118,
-0.118599316442255,-0.117478324788082,-0.115847619865693,-0.0990038844796983,
-0.0707289323749749,-0.0652192497652088,-0.0629576091979782,-0.061265790591419,
-0.059397923888038,-0.0567726546030518,-0.0501515511055032,-0.0403676753941963,
-0.0110688761212782,-0.0054956478613353,-0.00375609781177683,-0.0026448724528549,
-0.00167735725160652,-0.000891022296295099,-9.99999999917733E-7),
 .UNSPECIFIED.);
#1615=B_SPLINE_CURVE_WITH_KNOTS('',3,(#119571,#119572,#119573,#119574,#119575,
#119576,#119577,#119578,#119579,#119580,#119581,#119582,#119583,#119584,
#119585,#119586,#119587,#119588,#119589,#119590,#119591,#119592,#119593,
#119594,#119595,#119596,#119597,#119598,#119599,#119600,#119601,#119602,
#119603,#119604,#119605,#119606,#119607,#119608,#119609,#119610,#119611,
#119612,#119613,#119614,#119615,#119616,#119617,#119618,#119619,#119620,
#119621,#119622,#119623,#119624,#119625,#119626,#119627,#119628,#119629,
#119630,#119631,#119632,#119633,#119634,#119635,#119636,#119637,#119638,
#119639,#119640,#119641,#119642,#119643,#119644,#119645,#119646,#119647,
#119648,#119649,#119650,#119651,#119652,#119653,#119654,#119655,#119656,
#119657,#119658,#119659,#119660,#119661,#119662,#119663,#119664,#119665,
#119666,#119667,#119668,#119669,#119670,#119671,#119672,#119673,#119674,
#119675,#119676,#119677,#119678,#119679,#119680,#119681,#119682,#119683,
#119684,#119685,#119686,#119687,#119688,#119689,#119690,#119691,#119692,
#119693,#119694,#119695,#119696,#119697,#119698,#119699,#119700,#119701,
#119702,#119703,#119704,#119705,#119706,#119707,#119708,#119709,#119710,
#119711,#119712,#119713,#119714,#119715,#119716,#119717,#119718,#119719,
#119720,#119721,#119722,#119723,#119724,#119725,#119726,#119727,#119728,
#119729,#119730,#119731,#119732,#119733,#119734,#119735,#119736,#119737,
#119738,#119739,#119740,#119741,#119742,#119743,#119744,#119745,#119746,
#119747,#119748,#119749,#119750,#119751,#119752,#119753,#119754,#119755,
#119756,#119757,#119758,#119759,#119760,#119761,#119762,#119763,#119764,
#119765,#119766,#119767,#119768,#119769,#119770,#119771,#119772,#119773,
#119774,#119775,#119776,#119777,#119778,#119779,#119780,#119781,#119782,
#119783,#119784,#119785,#119786,#119787,#119788,#119789,#119790,#119791,
#119792,#119793,#119794,#119795,#119796,#119797,#119798,#119799,#119800,
#119801,#119802,#119803,#119804,#119805,#119806,#119807,#119808,#119809,
#119810,#119811,#119812,#119813,#119814,#119815,#119816,#119817,#119818,
#119819,#119820,#119821,#119822,#119823,#119824,#119825,#119826,#119827,
#119828,#119829,#119830,#119831,#119832),.UNSPECIFIED.,.F.,.F.,(4,2,2,2,
2,2,2,2,2,2,2,2,2,2,2,2,2,2,2,2,2,2,2,2,2,2,2,2,2,2,2,2,2,2,2,2,2,2,2,2,
2,2,2,2,2,2,2,2,2,2,2,2,2,2,2,2,2,2,2,2,2,2,2,2,2,2,2,2,2,2,2,2,2,2,2,2,
2,2,2,2,2,2,2,2,2,2,2,2,2,2,2,2,2,2,2,2,2,2,2,2,2,2,2,2,2,2,2,2,2,2,2,2,
2,2,2,2,2,2,2,2,2,2,2,2,2,2,2,2,2,2,4),(-2.96774370793825,-2.95691337121733,
-2.95119318194074,-2.94877962072619,-2.94696532202346,-2.94512123982102,
-2.94316545926379,-2.94010786907299,-2.93085947243012,-2.91702940083278,
-2.90086534003985,-2.89041205828235,-2.8883345613625,-2.88716494585088,
-2.88613985631808,-2.88479183023501,-2.88174104500079,-2.8595196773211,
-2.84288406306168,-2.83659729946576,-2.83186882414787,-2.82964656440494,
-2.82962354836739,-2.8295995245032,-2.8295744413791,-2.82954824444592,-2.82952087583186,
-2.82949227411457,-2.82946237408205,-2.82943110648194,-2.82939839773653,
-2.82936416966736,-2.82932833919924,-2.82929081804144,-2.82925151235605,
-2.82921032243071,-2.82918648407176,-2.82915667241775,-2.82911938112325,
-2.82907272063437,-2.82901432083922,-2.82894121110194,-2.82889805228096,
-2.82872855034397,-2.8268972112756,-2.82452938261826,-2.82055180181568,
-2.7914769617933,-2.7791246514421,-2.77273643292514,-2.77093936623985,-2.76983122390776,
-2.76879531921187,-2.76729128510585,-2.76445666280324,-2.74395459894712,
-2.72618437749715,-2.71965726480536,-2.71475679111166,-2.71242126143093,
-2.71059925204096,-2.7085733396414,-2.7051917858923,-2.6926559866327,-2.659656721078,
-2.65658407325577,-2.65421422186697,-2.65298254452811,-2.65196478553647,
-2.65068081852581,-2.64863193766583,-2.63457057553929,-2.62965093275844,
-2.61445773560999,-2.59995507505905,-2.59655693786095,-2.59452721087574,
-2.59270559271037,-2.59037586012033,-2.58550765200907,-2.56392543158225,
-2.54889540567895,-2.53888995871644,-2.53683576545242,-2.53567100647635,
-2.53464445631786,-2.53328713069123,-2.53018466006796,-2.50869152597703,
-2.49158372393118,-2.48519446016765,-2.48037324705607,-2.47805234210953,
-2.47623166198625,-2.47419680551015,-2.47077514189218,-2.45759998322799,
-2.43545671446359,-2.42629105838255,-2.42272910519923,-2.42007196092014,
-2.41878263408276,-2.4178626761167,-2.41667770961938,-2.41458750897691,
-2.40494486365705,-2.38590752884688,-2.37265962288026,-2.36718021266936,
-2.36289876059312,-2.36068327325347,-2.35887115502185,-2.35676392121772,
-2.35310555882761,-2.33101233536977,-2.31237978797182,-2.30698881677355,
-2.303356392832,-2.30189571570355,-2.30085703904073,-2.29972943526284,-2.29784493692715,
-2.29132389915938,-2.2655802373753,-2.24868780790604,-2.24516421743623,
-2.24310736701001,-2.24129033897382,-2.23900548920624,-2.23437273187573,
-2.22608676643451),.UNSPECIFIED.);
#1616=B_SPLINE_CURVE_WITH_KNOTS('',3,(#119833,#119834,#119835,#119836,#119837,
#119838,#119839,#119840,#119841,#119842,#119843,#119844,#119845,#119846,
#119847,#119848,#119849,#119850,#119851,#119852,#119853,#119854,#119855,
#119856,#119857,#119858,#119859,#119860,#119861,#119862,#119863,#119864,
#119865,#119866,#119867,#119868,#119869,#119870,#119871,#119872,#119873,
#119874,#119875,#119876,#119877,#119878,#119879,#119880,#119881,#119882,
#119883,#119884,#119885,#119886,#119887,#119888,#119889,#119890,#119891,
#119892,#119893,#119894,#119895,#119896,#119897,#119898,#119899,#119900,
#119901,#119902,#119903,#119904,#119905,#119906,#119907,#119908,#119909,
#119910,#119911,#119912,#119913,#119914,#119915,#119916,#119917,#119918,
#119919,#119920,#119921,#119922,#119923,#119924,#119925,#119926,#119927,
#119928,#119929,#119930,#119931,#119932,#119933,#119934,#119935,#119936,
#119937,#119938,#119939,#119940,#119941,#119942,#119943,#119944,#119945,
#119946,#119947,#119948,#119949,#119950,#119951,#119952,#119953,#119954,
#119955,#119956,#119957,#119958,#119959,#119960,#119961,#119962,#119963,
#119964,#119965,#119966,#119967,#119968,#119969,#119970,#119971,#119972,
#119973,#119974,#119975,#119976,#119977,#119978,#119979,#119980,#119981,
#119982,#119983,#119984,#119985,#119986,#119987,#119988,#119989,#119990,
#119991,#119992,#119993,#119994,#119995,#119996,#119997,#119998,#119999,
#120000,#120001,#120002,#120003,#120004,#120005,#120006,#120007,#120008,
#120009,#120010,#120011,#120012,#120013,#120014,#120015,#120016,#120017,
#120018,#120019,#120020,#120021,#120022,#120023,#120024,#120025,#120026,
#120027,#120028,#120029,#120030,#120031,#120032,#120033,#120034,#120035,
#120036,#120037,#120038,#120039,#120040,#120041,#120042,#120043,#120044,
#120045,#120046,#120047,#120048,#120049,#120050,#120051,#120052,#120053,
#120054,#120055,#120056,#120057,#120058,#120059,#120060,#120061,#120062,
#120063,#120064,#120065,#120066,#120067,#120068,#120069,#120070,#120071,
#120072,#120073,#120074,#120075,#120076),.UNSPECIFIED.,.F.,.F.,(4,2,2,2,
2,2,2,2,2,2,2,2,2,2,2,2,2,2,2,2,2,2,2,2,2,2,2,2,2,2,2,2,2,2,2,2,2,2,2,2,
2,2,2,2,2,2,2,2,2,2,2,2,2,2,2,2,2,2,2,2,2,2,2,2,2,2,2,2,2,2,2,2,2,2,2,2,
2,2,2,2,2,2,2,2,2,2,2,2,2,2,2,2,2,2,2,2,2,2,2,2,2,2,2,2,2,2,2,2,2,2,2,2,
2,2,2,2,2,2,2,2,2,4),(-2.96786375617954,-2.96378011212947,-2.93841144513886,
-2.91929099895211,-2.91502414866376,-2.91281199116845,-2.91100052850842,
-2.90889172503984,-2.90522471437712,-2.88398853022001,-2.86864283089649,
-2.85684768434756,-2.85530143633461,-2.85396946682291,-2.85395746328359,
-2.8539454580821,-2.85393344738246,-2.85392142729917,-2.85390939387554,
-2.85389734305823,-2.853885270717,-2.85387317263873,-2.85386104450872,-2.85384888189198,
-2.85383668022117,-2.85382443485175,-2.85381214097922,-2.85379979364217,
-2.85379255029808,-2.8537850850793,-2.85377738427235,-2.85376943297857,
-2.8537612150429,-2.85375271278093,-2.85276266139395,-2.85154560427922,
-2.84935661837392,-2.83722774254759,-2.81722281878852,-2.80079809171344,
-2.7972967887381,-2.79524507431375,-2.79342784258526,-2.79113639099924,
-2.78646762546614,-2.75979460067696,-2.74595953704414,-2.74137263781126,
-2.73815166175674,-2.73675915076909,-2.73573129179428,-2.73457306029961,
-2.73254810965919,-2.72432663497843,-2.70137977818497,-2.68371618065551,
-2.68016008967731,-2.67809656907524,-2.67628098234639,-2.67400768311489,
-2.66958142973605,-2.64101270337113,-2.63656659279805,-2.62706253283171,
-2.62341680381072,-2.6207118305187,-2.61941342363992,-2.61849267611034,
-2.61731462257691,-2.61525416760211,-2.60611241832179,-2.58671418373808,
-2.57333631493625,-2.56512093122223,-2.56227796791665,-2.5603673603776,
-2.55851785594919,-2.55589001287662,-2.54972562592053,-2.51530424097516,
-2.50514778971678,-2.50308577858156,-2.50191936374699,-2.50089328894623,
-2.49953911482938,-2.49645440143038,-2.47476441782474,-2.45776926702449,
-2.45140380837669,-2.44659638211607,-2.44427816219535,-2.44245787160905,
-2.4404216766947,-2.43699347410117,-2.4238051775546,-2.40166689409547,-2.39250649030868,
-2.3889458124976,-2.38628940489537,-2.38500026543142,-2.38408037723338,
-2.3828954386582,-2.3808051774687,-2.37116096120318,-2.35211820748262,-2.33886668702043,
-2.33338622950079,-2.32910415154005,-2.32688861386955,-2.32507660019495,
-2.32296966191593,-2.31931228559718,-2.2972224280038,-2.28037895714556,
-2.2738897040351,-2.26973360365978,-2.26819453784391,-2.2671414493785,-2.26604118243269,
-2.26428045255196,-2.2588435727881,-2.2259764122215),.UNSPECIFIED.);
#1617=B_SPLINE_CURVE_WITH_KNOTS('',3,(#120081,#120082,#120083,#120084,#120085,
#120086,#120087,#120088,#120089,#120090,#120091,#120092,#120093,#120094,
#120095,#120096,#120097,#120098,#120099,#120100,#120101,#120102,#120103,
#120104,#120105,#120106,#120107,#120108,#120109,#120110,#120111,#120112,
#120113,#120114,#120115,#120116,#120117,#120118,#120119,#120120,#120121,
#120122,#120123,#120124,#120125,#120126,#120127,#120128,#120129,#120130,
#120131,#120132,#120133,#120134,#120135,#120136,#120137,#120138,#120139,
#120140,#120141,#120142,#120143,#120144,#120145,#120146,#120147,#120148,
#120149,#120150,#120151,#120152,#120153,#120154,#120155,#120156,#120157,
#120158,#120159,#120160,#120161,#120162,#120163,#120164,#120165,#120166,
#120167,#120168,#120169,#120170,#120171,#120172,#120173,#120174,#120175,
#120176,#120177,#120178,#120179,#120180,#120181,#120182,#120183,#120184,
#120185,#120186,#120187,#120188,#120189,#120190,#120191,#120192,#120193,
#120194,#120195,#120196,#120197,#120198,#120199,#120200,#120201,#120202,
#120203,#120204,#120205,#120206,#120207,#120208,#120209,#120210,#120211,
#120212,#120213,#120214,#120215,#120216,#120217,#120218,#120219,#120220,
#120221,#120222,#120223,#120224,#120225,#120226,#120227,#120228,#120229,
#120230,#120231,#120232,#120233,#120234,#120235,#120236,#120237,#120238,
#120239,#120240,#120241,#120242,#120243,#120244,#120245,#120246,#120247,
#120248,#120249,#120250,#120251,#120252,#120253,#120254,#120255,#120256,
#120257,#120258,#120259,#120260,#120261,#120262,#120263,#120264,#120265,
#120266,#120267,#120268,#120269,#120270,#120271,#120272,#120273,#120274,
#120275,#120276,#120277,#120278,#120279,#120280,#120281,#120282,#120283,
#120284,#120285,#120286,#120287,#120288,#120289,#120290,#120291,#120292,
#120293,#120294),.UNSPECIFIED.,.F.,.F.,(4,2,2,2,2,2,2,2,2,2,2,2,2,2,2,2,
2,2,2,2,2,2,2,2,2,2,2,2,2,2,2,2,2,2,2,2,2,2,2,2,2,2,2,2,2,2,2,2,2,2,2,2,
2,2,2,2,2,2,2,2,2,2,2,2,2,2,2,2,2,2,2,2,2,2,2,2,2,2,2,2,2,2,2,2,2,2,2,2,
2,2,2,2,2,2,2,2,2,2,2,2,2,2,2,2,2,2,4),(-0.74213368445771,-0.741060461331361,
-0.739913267852274,-0.738881528423136,-0.73746498088996,-0.734104923777809,
-0.729252868746627,-0.713978510749945,-0.689407102522553,-0.684623742302791,
-0.682309682649795,-0.680489371994206,-0.67844972183358,-0.675007291837811,
-0.659752468392614,-0.645099581600553,-0.638038602406348,-0.62628217224783,
-0.624088265812981,-0.622879857130139,-0.621860134935974,-0.620546416786616,
-0.617763138683222,-0.613980105693608,-0.603909895994989,-0.581115795296927,
-0.569702119864442,-0.566398037747063,-0.564388368144093,-0.562561632247161,
-0.560192693704824,-0.555115080641119,-0.548277159539189,-0.513885374889266,
-0.508253198435443,-0.506468872213815,-0.505363106188769,-0.504312691935271,
-0.502789118743533,-0.498743663735054,-0.492495368135684,-0.466566401205063,
-0.452794176426897,-0.449309095402972,-0.447260050771829,-0.445622959088123,
-0.443412291706371,-0.439157121738554,-0.424311686470956,-0.403979524002424,
-0.391863094776248,-0.389653195630644,-0.388441105957018,-0.387421541700861,
-0.386112214189044,-0.38335273720478,-0.379612047668472,-0.369720065740236,
-0.346651344500311,-0.33524447399746,-0.331940601323955,-0.3299307620635,
-0.32810368053141,-0.325734021066061,-0.320653777535694,-0.313811558375602,
-0.27936170952052,-0.273775642141207,-0.271996509396533,-0.270891768378505,
-0.269840442791227,-0.268312789488573,-0.264240237845529,-0.257934128724755,
-0.231372863825376,-0.218199398417869,-0.214776626821744,-0.212740839503349,
-0.210919154211932,-0.208596732040243,-0.203771525467293,-0.197375655071753,
-0.180244532455095,-0.158730966505941,-0.155627320835404,-0.1542693264795,
-0.153242218763514,-0.152076744565603,-0.150021137204183,-0.140003437519451,
-0.107427986167811,-0.099789382732737,-0.096937101024957,-0.0952149089678628,
-0.0933697957912819,-0.0911703237474851,-0.0861569041583209,-0.0793539652609495,
-0.0606703468593545,-0.0416052063917316,-0.0384147364760087,-0.0371643586513535,
-0.0361318961322054,-0.0350149612168854,-0.0331802271212109,-0.0309635957031294,
-9.99999994588663E-7),.UNSPECIFIED.);
#1618=B_SPLINE_CURVE_WITH_KNOTS('',3,(#120295,#120296,#120297,#120298,#120299,
#120300,#120301,#120302,#120303,#120304,#120305,#120306,#120307,#120308,
#120309,#120310,#120311,#120312,#120313,#120314,#120315,#120316,#120317,
#120318,#120319,#120320,#120321,#120322,#120323,#120324,#120325,#120326,
#120327,#120328,#120329,#120330,#120331,#120332,#120333,#120334,#120335,
#120336,#120337,#120338,#120339,#120340,#120341,#120342,#120343,#120344,
#120345,#120346,#120347,#120348,#120349,#120350,#120351,#120352,#120353,
#120354,#120355,#120356,#120357,#120358,#120359,#120360,#120361,#120362,
#120363,#120364,#120365,#120366,#120367,#120368,#120369,#120370,#120371,
#120372,#120373,#120374,#120375,#120376,#120377,#120378,#120379,#120380,
#120381,#120382,#120383,#120384,#120385,#120386,#120387,#120388,#120389,
#120390,#120391,#120392,#120393,#120394,#120395,#120396,#120397,#120398,
#120399,#120400,#120401,#120402,#120403,#120404,#120405,#120406,#120407,
#120408,#120409,#120410,#120411,#120412,#120413,#120414,#120415,#120416,
#120417,#120418,#120419,#120420,#120421,#120422,#120423,#120424,#120425,
#120426,#120427,#120428,#120429,#120430,#120431,#120432,#120433,#120434,
#120435,#120436,#120437,#120438,#120439,#120440,#120441,#120442,#120443,
#120444,#120445,#120446,#120447,#120448,#120449,#120450,#120451,#120452,
#120453,#120454,#120455,#120456,#120457,#120458,#120459,#120460,#120461,
#120462,#120463,#120464,#120465,#120466,#120467,#120468,#120469,#120470,
#120471,#120472,#120473,#120474,#120475,#120476,#120477,#120478,#120479,
#120480,#120481,#120482,#120483,#120484,#120485,#120486,#120487,#120488,
#120489,#120490,#120491,#120492,#120493,#120494,#120495,#120496,#120497,
#120498,#120499,#120500,#120501,#120502,#120503,#120504,#120505,#120506,
#120507,#120508),.UNSPECIFIED.,.F.,.F.,(4,2,2,2,2,2,2,2,2,2,2,2,2,2,2,2,
2,2,2,2,2,2,2,2,2,2,2,2,2,2,2,2,2,2,2,2,2,2,2,2,2,2,2,2,2,2,2,2,2,2,2,2,
2,2,2,2,2,2,2,2,2,2,2,2,2,2,2,2,2,2,2,2,2,2,2,2,2,2,2,2,2,2,2,2,2,2,2,2,
2,2,2,2,2,2,2,2,2,2,2,2,2,2,2,2,2,2,4),(-2.2259764122215,-2.22425628378077,
-2.21740905304554,-2.21232608992596,-2.20995671416596,-2.20813050011741,
-2.20612227226823,-2.20282260378006,-2.19145154282195,-2.16834133453937,
-2.15843797074299,-2.15469518279821,-2.1519350443964,-2.15062600491296,
-2.14960696389469,-2.1483958697176,-2.14618874234476,-2.13411461014791,
-2.11292307752032,-2.09752380211373,-2.0940745053629,-2.0920338685433,-2.09021457674336,
-2.08790441429328,-2.08313879335939,-2.05812210350068,-2.03745952708545,
-2.03472599290275,-2.03342200053563,-2.03240325553752,-2.03118817642637,
-2.02896324264578,-2.01596972923931,-2.01001250965625,-1.99493413568077,
-1.98025840719109,-1.97684995940238,-1.97481807056782,-1.97299701031433,
-1.97067145059373,-1.96582504370401,-1.94386208011153,-1.92908086965547,
-1.9191527491163,-1.9171026907723,-1.91593886843292,-1.91491217572012,-1.91355344204157,
-1.91044266794885,-1.88932528614479,-1.87194878512497,-1.86550251094958,
-1.86064834204034,-1.85832128657316,-1.85650001406538,-1.85446887765395,
-1.85106408999226,-1.83816812869897,-1.81132451768157,-1.80499344509727,
-1.80091021846368,-1.79938153804988,-1.79833044452903,-1.79722693783769,
-1.79545160635758,-1.78989248233265,-1.75544062518884,-1.74860128995825,
-1.74352274392376,-1.7411541246853,-1.73932795300417,-1.73731923040808,
-1.73401749430364,-1.72247941086814,-1.69945047463344,-1.68960775261839,
-1.68587949384137,-1.68312755324843,-1.68182004825567,-1.68089815279672,
-1.67972595593863,-1.6776916143627,-1.66897074193232,-1.66500010961163,
-1.6447789055654,-1.62878015876585,-1.62529937335927,-1.62325188517156,
-1.62143366189215,-1.61913457459874,-1.61442720270841,-1.58828677187455,
-1.56803155580148,-1.56568690462733,-1.56446043519854,-1.56344241534644,
-1.56215237055494,-1.56008316907118,-1.5443132260124,-1.52965471026575,
-1.51325822354984,-1.50879867441267,-1.50654770813344,-1.50475016736747,
-1.50267628825316,-1.4991657852467,-1.48408042832229),.UNSPECIFIED.);
#1619=B_SPLINE_CURVE_WITH_KNOTS('',3,(#120513,#120514,#120515,#120516,#120517,
#120518,#120519,#120520,#120521,#120522,#120523,#120524,#120525,#120526,
#120527,#120528,#120529,#120530,#120531,#120532,#120533,#120534,#120535,
#120536,#120537,#120538,#120539,#120540,#120541,#120542,#120543,#120544,
#120545,#120546,#120547,#120548,#120549,#120550,#120551,#120552,#120553,
#120554,#120555,#120556,#120557,#120558,#120559,#120560,#120561,#120562,
#120563,#120564,#120565,#120566,#120567,#120568,#120569,#120570,#120571,
#120572,#120573,#120574,#120575,#120576,#120577,#120578,#120579,#120580,
#120581,#120582,#120583,#120584,#120585,#120586,#120587,#120588,#120589,
#120590,#120591,#120592,#120593,#120594,#120595,#120596,#120597,#120598,
#120599,#120600,#120601,#120602,#120603,#120604,#120605,#120606,#120607,
#120608,#120609,#120610,#120611,#120612,#120613,#120614,#120615,#120616,
#120617,#120618,#120619,#120620,#120621,#120622,#120623,#120624,#120625,
#120626,#120627,#120628,#120629,#120630,#120631,#120632,#120633,#120634,
#120635,#120636,#120637,#120638,#120639,#120640,#120641,#120642,#120643,
#120644,#120645,#120646,#120647,#120648,#120649,#120650,#120651,#120652,
#120653,#120654,#120655,#120656,#120657,#120658,#120659,#120660,#120661,
#120662,#120663,#120664,#120665,#120666,#120667,#120668,#120669,#120670,
#120671,#120672,#120673,#120674,#120675,#120676,#120677,#120678,#120679,
#120680,#120681,#120682,#120683,#120684,#120685,#120686,#120687,#120688,
#120689,#120690,#120691,#120692,#120693,#120694,#120695,#120696,#120697,
#120698,#120699,#120700,#120701,#120702,#120703,#120704,#120705,#120706,
#120707,#120708,#120709,#120710,#120711,#120712,#120713,#120714,#120715,
#120716),.UNSPECIFIED.,.F.,.F.,(4,2,2,2,2,2,2,2,2,2,2,2,2,2,2,2,2,2,2,2,
2,2,2,2,2,2,2,2,2,2,2,2,2,2,2,2,2,2,2,2,2,2,2,2,2,2,2,2,2,2,2,2,2,2,2,2,
2,2,2,2,2,2,2,2,2,2,2,2,2,2,2,2,2,2,2,2,2,2,2,2,2,2,2,2,2,2,2,2,2,2,2,2,
2,2,2,2,2,2,2,2,2,4),(-1.48412040656859,-1.48082148178739,-1.46574011190158,
-1.45962859656999,-1.44680686389676,-1.44476382001585,-1.4434814452826,
-1.44246351060667,-1.44122987116206,-1.43885139570483,-1.41849408519134,
-1.39255622452202,-1.38783773326304,-1.38553615482571,-1.38371725275182,
-1.38167035033535,-1.3781938923928,-1.36229547724367,-1.33907177662105,
-1.32934887034997,-1.32725398897561,-1.32606783682932,-1.32514784158701,
-1.32385962122743,-1.32120888197452,-1.31765862536708,-1.30854075520546,
-1.28648398574501,-1.2731842051744,-1.26975462372141,-1.26771780557239,
-1.2658970655478,-1.26357841092839,-1.25877057215442,-1.25240403450815,
-1.23540594709219,-1.21369531991906,-1.2106101871287,-1.20925570946243,
-1.20822936030441,-1.20706253266058,-1.20499956509593,-1.19483020961972,
-1.16017891010646,-1.15420560452021,-1.15186693942054,-1.15015613169257,
-1.14830437428156,-1.14576988545933,-1.13973084436134,-1.13111087709734,
-1.10547618480664,-1.09500491757566,-1.09287013930818,-1.09167502967595,
-1.09065385665762,-1.08932175709915,-1.08644010912123,-1.07417759234089,
-1.0521670197258,-1.03878081073498,-1.03534604319968,-1.03330817432964,
-1.03148774786634,-1.02917120837372,-1.02437412304914,-1.01802602864954,
-1.00111316188268,-0.979274228817487,-0.976497079413082,-0.975155231787754,
-0.974194139420834,-0.973135642989955,-0.971570248014536,-0.967226486820596,
-0.960323152528731,-0.924233981012744,-0.919182874805421,-0.916844410137595,
-0.915016757839911,-0.913012198141236,-0.909730633684257,-0.8969752878299,
-0.864614557572141,-0.859691904762698,-0.857996031461812,-0.857017649022139,
-0.855973612590148,-0.854483314218406,-0.850660632927603,-0.844881660672618,
-0.82334110480409,-0.804783359721267,-0.801147009071279,-0.799044493782142,
-0.797231742973639,-0.795009557879451,-0.790695996527068,-0.775387421492797,
-0.750606962364917,-0.743033356308706,-0.74213368445771),.UNSPECIFIED.);
#1620=B_SPLINE_CURVE_WITH_KNOTS('',3,(#120717,#120718,#120719,#120720,#120721,
#120722,#120723,#120724,#120725,#120726,#120727,#120728,#120729,#120730,
#120731,#120732,#120733,#120734,#120735,#120736,#120737,#120738,#120739,
#120740,#120741,#120742,#120743,#120744,#120745,#120746,#120747,#120748,
#120749,#120750,#120751,#120752,#120753,#120754,#120755,#120756,#120757,
#120758,#120759,#120760,#120761,#120762,#120763,#120764,#120765,#120766,
#120767,#120768,#120769,#120770,#120771,#120772,#120773,#120774,#120775,
#120776,#120777,#120778,#120779,#120780,#120781,#120782,#120783,#120784,
#120785,#120786,#120787,#120788,#120789,#120790,#120791,#120792,#120793,
#120794,#120795,#120796,#120797,#120798,#120799,#120800,#120801,#120802,
#120803,#120804,#120805,#120806,#120807,#120808,#120809,#120810,#120811,
#120812,#120813,#120814,#120815,#120816,#120817,#120818,#120819,#120820,
#120821,#120822,#120823,#120824,#120825,#120826,#120827,#120828,#120829,
#120830,#120831,#120832,#120833,#120834,#120835,#120836,#120837,#120838,
#120839,#120840,#120841,#120842,#120843,#120844,#120845,#120846,#120847,
#120848,#120849,#120850,#120851,#120852,#120853,#120854,#120855,#120856,
#120857,#120858,#120859,#120860,#120861,#120862,#120863,#120864,#120865,
#120866,#120867,#120868,#120869,#120870,#120871,#120872,#120873,#120874,
#120875,#120876,#120877,#120878,#120879,#120880,#120881,#120882,#120883,
#120884,#120885,#120886,#120887,#120888,#120889,#120890,#120891,#120892,
#120893,#120894,#120895,#120896,#120897,#120898,#120899,#120900,#120901,
#120902,#120903,#120904,#120905,#120906,#120907,#120908,#120909,#120910,
#120911,#120912,#120913,#120914,#120915,#120916,#120917,#120918,#120919,
#120920,#120921,#120922,#120923,#120924,#120925,#120926),.UNSPECIFIED.,
 .F.,.F.,(4,2,2,2,2,2,2,2,2,2,2,2,2,2,2,2,2,2,2,2,2,2,2,2,2,2,2,2,2,2,2,
2,2,2,2,2,2,2,2,2,2,2,2,2,2,2,2,2,2,2,2,2,2,2,2,2,2,2,2,2,2,2,2,2,2,2,2,
2,2,2,2,2,2,2,2,2,2,2,2,2,2,2,2,2,2,2,2,2,2,2,2,2,2,2,2,2,2,2,2,2,2,2,2,
2,4),(-1.48408042832229,-1.48376664299265,-1.46114076049178,-1.45054639973923,
-1.4484008663561,-1.44720343557792,-1.44618273513266,-1.44485447556968,
-1.44199291362653,-1.4235726312338,-1.39629157020093,-1.39167501278574,
-1.38939333124003,-1.38757663247404,-1.38551782371353,-1.38198502686217,
-1.36489249373927,-1.33976498747468,-1.33286042335265,-1.33094627999807,
-1.32981214828741,-1.32877614612721,-1.32733141389717,-1.32379881274751,
-1.31860832013949,-1.30130110862416,-1.2794458178099,-1.27459629617925,
-1.27226999993658,-1.27044868397678,-1.26841684067741,-1.26500927844663,
-1.25035576603178,-1.23524420141299,-1.22931597518159,-1.21626791406282,
-1.21404279911828,-1.21282759713475,-1.21180872549969,-1.21050455178258,
-1.20777055250332,-1.18703788587951,-1.16211551129242,-1.15734647651094,
-1.15503547263141,-1.15321586934416,-1.15117524933759,-1.14772688983962,
-1.13235471934567,-1.11143780144199,-1.1076205454009,-1.09873985078699,
-1.09669472316324,-1.09551999073136,-1.09459840878217,-1.09329437668301,
-1.09056107817527,-1.06990751197003,-1.04489968762296,-1.04013433919366,
-1.03782405067679,-1.03600453765067,-1.03396352455051,-1.03051328787816,
-1.01510613239754,-0.993891289332276,-0.981815317663498,-0.979607850191654,
-0.978396577969166,-0.97737738353288,-0.976068154383664,-0.973307619550056,
-0.969564684118706,-0.95966171815368,-0.936579865867218,-0.925201037611923,
-0.921900427748099,-0.919891794237271,-0.918065315730189,-0.915695746899244,
-0.910613014351861,-0.903765701502042,-0.869218524085517,-0.863722291686634,
-0.861954189398518,-0.860852150939333,-0.859799822597651,-0.858265493893037,
-0.854144009175637,-0.847731408440624,-0.830833549532936,-0.808689718737118,
-0.805032781718992,-0.80292566070683,-0.801113233015744,-0.798896866184818,
-0.794612169914818,-0.789127165718284,-0.775859502758688,-0.75678345007552,
-0.747155533671208,-0.745065666409472,-0.743880654051961,-0.742960514511092,
-0.74204764888634),.UNSPECIFIED.);
#1621=B_SPLINE_CURVE_WITH_KNOTS('',3,(#120931,#120932,#120933,#120934,#120935,
#120936,#120937,#120938,#120939,#120940,#120941,#120942,#120943,#120944,
#120945,#120946,#120947,#120948,#120949,#120950,#120951,#120952,#120953,
#120954,#120955,#120956,#120957,#120958,#120959,#120960,#120961,#120962,
#120963,#120964,#120965,#120966,#120967,#120968,#120969,#120970,#120971,
#120972,#120973,#120974,#120975,#120976,#120977,#120978,#120979,#120980,
#120981,#120982,#120983,#120984,#120985,#120986,#120987,#120988,#120989,
#120990,#120991,#120992,#120993,#120994,#120995,#120996,#120997,#120998,
#120999,#121000,#121001,#121002,#121003,#121004,#121005,#121006,#121007,
#121008,#121009,#121010,#121011,#121012,#121013,#121014,#121015,#121016,
#121017,#121018,#121019,#121020,#121021,#121022,#121023,#121024,#121025,
#121026,#121027,#121028,#121029,#121030,#121031,#121032,#121033,#121034,
#121035,#121036,#121037,#121038,#121039,#121040,#121041,#121042,#121043,
#121044,#121045,#121046,#121047,#121048,#121049,#121050,#121051,#121052,
#121053,#121054,#121055,#121056,#121057,#121058,#121059,#121060,#121061,
#121062,#121063,#121064,#121065,#121066,#121067,#121068,#121069,#121070,
#121071,#121072,#121073,#121074,#121075,#121076,#121077,#121078,#121079,
#121080,#121081,#121082,#121083,#121084,#121085,#121086,#121087,#121088,
#121089,#121090,#121091,#121092,#121093,#121094,#121095,#121096,#121097,
#121098,#121099,#121100,#121101,#121102,#121103,#121104,#121105,#121106,
#121107,#121108,#121109,#121110,#121111,#121112,#121113,#121114,#121115,
#121116,#121117,#121118,#121119,#121120,#121121,#121122,#121123,#121124,
#121125,#121126,#121127,#121128,#121129,#121130,#121131,#121132,#121133,
#121134,#121135,#121136,#121137,#121138,#121139,#121140,#121141,#121142,
#121143,#121144),.UNSPECIFIED.,.F.,.F.,(4,2,2,2,2,2,2,2,2,2,2,2,2,2,2,2,
2,2,2,2,2,2,2,2,2,2,2,2,2,2,2,2,2,2,2,2,2,2,2,2,2,2,2,2,2,2,2,2,2,2,2,2,
2,2,2,2,2,2,2,2,2,2,2,2,2,2,2,2,2,2,2,2,2,2,2,2,2,2,2,2,2,2,2,2,2,2,2,2,
2,2,2,2,2,2,2,2,2,2,2,2,2,2,2,2,2,2,4),(-2.22609961801482,-2.22556332767558,
-2.21080189555777,-2.20738749015127,-2.20535379388558,-2.20353218821009,
-2.2012074015045,-2.19636805452909,-2.17552754132884,-2.15790385451442,
-2.15227350392173,-2.14852307968545,-2.14704371560362,-2.14600154677802,
-2.14488065646882,-2.14302754487163,-2.13676884940031,-2.13122332319925,
-2.09748507458848,-2.0916169857361,-2.08911033753154,-2.08726311582116,
-2.0853111594724,-2.08227442410342,-2.07320934779991,-2.04560457994546,
-2.03266082996555,-2.03048206813715,-2.02929026865605,-2.02826846957923,
-2.02695333547304,-2.024087628352,-1.99943236232436,-1.97784586923063,-1.97357138152013,
-1.97135698244195,-1.96954451780279,-1.96743548224453,-1.96377042358467,
-1.94218576237533,-1.92635985520588,-1.91891549606693,-1.91580777306001,
-1.91341673991637,-1.91218047247507,-1.91116257480152,-1.90988302330995,
-1.90784956118684,-1.89535776847603,-1.88895093563702,-1.87395577686803,
-1.85916083006046,-1.85574455991814,-1.85371050838847,-1.85188905360386,
-1.84956510532392,-1.84472992223066,-1.82202909975717,-1.80777706002198,
-1.80121781824838,-1.79702943468748,-1.79548550233807,-1.79443121460751,
-1.79346554220677,-1.7918351220653,-1.78738538641425,-1.75165173785602,
-1.74474065300278,-1.73962138582896,-1.7372449481181,-1.7354173462335,-1.73341162800042,
-1.73012537265356,-1.71891090606944,-1.69571141668826,-1.68574279946609,
-1.68198409700383,-1.67921480268087,-1.67790378212643,-1.67688431170144,
-1.6756740005234,-1.67347138468028,-1.66150733172289,-1.65461876349508,
-1.6398073631068,-1.62476962615438,-1.62133964197631,-1.61930275103474,
-1.61748204878895,-1.6151635832835,-1.61035666076,-1.58642277066181,-1.56530819942813,
-1.56219585771367,-1.56083661460074,-1.55980961468118,-1.55864548475794,
-1.55659497610999,-1.54666410758093,-1.5318732939339,-1.5099507302706,-1.50510418815635,
-1.50277820190063,-1.5009566292511,-1.49892397477586,-1.49551375850441,
-1.48412040656859),.UNSPECIFIED.);
#1622=B_SPLINE_CURVE_WITH_KNOTS('',3,(#121145,#121146,#121147,#121148,#121149,
#121150,#121151,#121152,#121153,#121154,#121155,#121156,#121157,#121158,
#121159,#121160,#121161,#121162,#121163,#121164,#121165,#121166,#121167,
#121168,#121169,#121170,#121171,#121172,#121173,#121174,#121175,#121176,
#121177,#121178,#121179,#121180,#121181,#121182,#121183,#121184,#121185,
#121186,#121187,#121188,#121189,#121190,#121191,#121192,#121193,#121194,
#121195,#121196,#121197,#121198,#121199,#121200,#121201,#121202,#121203,
#121204,#121205,#121206,#121207,#121208,#121209,#121210,#121211,#121212,
#121213,#121214,#121215,#121216,#121217,#121218,#121219,#121220,#121221,
#121222,#121223,#121224,#121225,#121226,#121227,#121228,#121229,#121230,
#121231,#121232,#121233,#121234,#121235,#121236,#121237,#121238,#121239,
#121240,#121241,#121242,#121243,#121244,#121245,#121246,#121247,#121248,
#121249,#121250,#121251,#121252,#121253,#121254,#121255,#121256,#121257,
#121258,#121259,#121260,#121261,#121262,#121263,#121264,#121265,#121266,
#121267,#121268,#121269,#121270,#121271,#121272,#121273,#121274,#121275,
#121276,#121277,#121278,#121279,#121280,#121281,#121282,#121283,#121284,
#121285,#121286,#121287,#121288,#121289,#121290,#121291,#121292,#121293,
#121294,#121295,#121296,#121297,#121298,#121299,#121300,#121301,#121302,
#121303,#121304,#121305,#121306,#121307,#121308,#121309,#121310,#121311,
#121312,#121313,#121314,#121315,#121316,#121317,#121318,#121319,#121320,
#121321,#121322,#121323,#121324,#121325,#121326,#121327,#121328,#121329,
#121330,#121331,#121332,#121333,#121334,#121335,#121336,#121337,#121338,
#121339,#121340,#121341,#121342,#121343,#121344,#121345,#121346,#121347,
#121348,#121349,#121350,#121351,#121352,#121353,#121354,#121355,#121356,
#121357,#121358,#121359,#121360,#121361,#121362,#121363,#121364,#121365,
#121366,#121367,#121368,#121369,#121370,#121371,#121372),.UNSPECIFIED.,
 .F.,.F.,(4,2,2,2,2,2,2,2,2,2,2,2,2,2,2,2,2,2,2,2,2,2,2,2,2,2,2,2,2,2,2,
2,2,2,2,2,2,2,2,2,2,2,2,2,2,2,2,2,2,2,2,2,2,2,2,2,2,2,2,2,2,2,2,2,2,2,2,
2,2,2,2,2,2,2,2,2,2,2,2,2,2,2,2,2,2,2,2,2,2,2,2,2,2,2,2,2,2,2,2,2,2,2,2,
2,2,2,2,2,2,2,2,2,2,4),(-0.74204764888634,-0.741670791865605,-0.739012316314998,
-0.735448644722572,-0.726277726514639,-0.704151134559818,-0.690970543427621,
-0.687548117910528,-0.685512860146582,-0.683691858811255,-0.681370608177842,
-0.676549015115992,-0.670158822644936,-0.653051742934083,-0.631508312556897,
-0.628403527682639,-0.627045618070197,-0.626018821544591,-0.624854014741848,
-0.622800318503052,-0.612809549364189,-0.597830478773235,-0.576171490404625,
-0.571309192892764,-0.568980263000083,-0.567158399832068,-0.56512750846632,
-0.56172531021177,-0.54716850794111,-0.531985435400949,-0.526618440682185,
-0.512984136553094,-0.510943076728187,-0.509661307973488,-0.508643420409092,
-0.507409341360159,-0.505028665738601,-0.501938496769546,-0.494557409918824,
-0.47869437733524,-0.457076808974808,-0.453405307478627,-0.451294929893803,
-0.449482702788917,-0.447270349220692,-0.443005509136648,-0.425901253236259,
-0.408473004259165,-0.401912962552111,-0.395131608666908,-0.393228056902245,
-0.392096150899994,-0.391059047653106,-0.389608388598855,-0.386039746323683,
-0.380777780233697,-0.363011746042743,-0.341732737130473,-0.336880754347417,
-0.334553780609715,-0.332732152642795,-0.330700186805467,-0.327292963617882,
-0.312651624283672,-0.297527702476826,-0.291669261037713,-0.278543052645347,
-0.276317319176379,-0.275101870655147,-0.274082849712495,-0.272778558271081,
-0.270044561968888,-0.249357556165051,-0.224378423698583,-0.21961090779958,
-0.217299980563585,-0.215480146480685,-0.213438963421036,-0.209988906109757,
-0.194592806373508,-0.173490174260136,-0.161291623309227,-0.159078164370229,
-0.157865444820671,-0.156846199323849,-0.155538400039576,-0.152786026073709,
-0.149057693378639,-0.139216379301996,-0.125356799839326,-0.105416407194767,
-0.101751945956182,-0.0996431355881328,-0.0978308038861879,-0.0977586976386119,
-0.0976923001905339,-0.0976308451375815,-0.0975736963287582,-0.0975203211224048,
-0.0974702699703891,-0.097423160629703,-0.0973786658315197,-0.0952050846410103,
-0.0903331681393833,-0.083786017071551,-0.0659268366182135,-0.0454950428270455,
-0.0426547737456153,-0.0411489605696309,-0.0401124249770891,-0.0390042464901762,
-0.0372083444533776,-0.0308374795419021,-9.99999999917733E-7),
 .UNSPECIFIED.);
#1623=B_SPLINE_CURVE_WITH_KNOTS('',3,(#121377,#121378,#121379,#121380,#121381,
#121382,#121383,#121384,#121385,#121386,#121387,#121388,#121389,#121390,
#121391,#121392,#121393,#121394,#121395,#121396,#121397,#121398,#121399,
#121400,#121401,#121402,#121403,#121404,#121405,#121406,#121407,#121408,
#121409,#121410,#121411,#121412,#121413,#121414,#121415,#121416,#121417,
#121418,#121419,#121420,#121421,#121422,#121423,#121424,#121425,#121426,
#121427,#121428,#121429,#121430,#121431,#121432,#121433,#121434,#121435,
#121436,#121437,#121438,#121439,#121440,#121441,#121442,#121443,#121444,
#121445,#121446,#121447,#121448,#121449,#121450,#121451,#121452,#121453,
#121454,#121455,#121456,#121457,#121458,#121459,#121460,#121461,#121462,
#121463,#121464,#121465,#121466,#121467,#121468,#121469,#121470,#121471,
#121472,#121473,#121474,#121475,#121476,#121477,#121478,#121479,#121480,
#121481,#121482,#121483,#121484,#121485,#121486,#121487,#121488,#121489,
#121490,#121491,#121492,#121493,#121494,#121495,#121496,#121497,#121498,
#121499,#121500,#121501,#121502,#121503,#121504,#121505,#121506,#121507,
#121508,#121509,#121510,#121511,#121512,#121513,#121514,#121515,#121516,
#121517,#121518,#121519,#121520,#121521,#121522,#121523,#121524,#121525,
#121526,#121527,#121528,#121529,#121530,#121531,#121532,#121533,#121534,
#121535,#121536,#121537,#121538,#121539,#121540,#121541,#121542,#121543,
#121544,#121545,#121546,#121547,#121548,#121549,#121550,#121551,#121552,
#121553,#121554,#121555,#121556,#121557,#121558,#121559,#121560,#121561,
#121562,#121563,#121564,#121565,#121566,#121567,#121568,#121569,#121570,
#121571,#121572,#121573,#121574,#121575,#121576,#121577,#121578,#121579,
#121580,#121581,#121582,#121583,#121584,#121585,#121586,#121587,#121588,
#121589,#121590,#121591,#121592,#121593,#121594,#121595,#121596),
 .UNSPECIFIED.,.F.,.F.,(4,2,2,2,2,2,2,2,2,2,2,2,2,2,2,2,2,2,2,2,2,2,2,2,
2,2,2,2,2,2,2,2,2,2,2,2,2,2,2,2,2,2,2,2,2,2,2,2,2,2,2,2,2,2,2,2,2,2,2,2,
2,2,2,2,2,2,2,2,2,2,2,2,2,2,2,2,2,2,2,2,2,2,2,2,2,2,2,2,2,2,2,2,2,2,2,2,
2,2,2,2,2,2,2,2,2,2,2,2,2,4),(-2.96804921651682,-2.96740018557415,-2.96636690768878,
-2.9652244441556,-2.96327309443646,-2.95594501532251,-2.95235016748792,
-2.93395364698124,-2.91557597381258,-2.91128095729757,-2.90906245417739,
-2.90724982949593,-2.9051442184243,-2.90149429568817,-2.88201497995418,
-2.85583203712465,-2.85183614570248,-2.85031989175863,-2.84927095635197,
-2.84816299218549,-2.84636837540087,-2.84064565571773,-2.83513624202623,
-2.81674471798401,-2.80371791225676,-2.79829564462427,-2.79404873373829,
-2.79183984473697,-2.79002755182002,-2.78791378799744,-2.7842278770267,
-2.76265490157924,-2.74680552123245,-2.73580893222999,-2.73370582241923,
-2.73253023540477,-2.73150562286161,-2.73016551489865,-2.7271620745997,
-2.70404947525284,-2.68351131196158,-2.67766824547294,-2.67516559838338,
-2.67331889938587,-2.67136526914252,-2.66832130501516,-2.65919749540911,
-2.63163968534097,-2.61977691757225,-2.61694057164501,-2.61561674400291,
-2.61459610465318,-2.6133947619652,-2.61123293034756,-2.60026061716805,
-2.56663224468561,-2.56052505473452,-2.5579793309458,-2.55612540546224,
-2.55418625212886,-2.55120988808159,-2.54263542946784,-2.51733662235103,
-2.51508602961282,-2.50585484299411,-2.50227616797712,-2.49960926619588,
-2.4983178408928,-2.49739745978806,-2.49621344778694,-2.49412828150278,
-2.48458654653846,-2.4654704513213,-2.45219295846012,-2.44670534290785,
-2.44241865517638,-2.44020176127328,-2.43838913146348,-2.43628202441509,
-2.43262571917638,-2.41010828841658,-2.39180159508405,-2.38645778274185,
-2.38284854737319,-2.38139131429905,-2.38035301855822,-2.37922358384149,
-2.37733161982564,-2.37068125132752,-2.36410984526234,-2.35777659506131,
-2.34276442753719,-2.32799245906315,-2.32457748261986,-2.32254368610575,
-2.32072213964739,-2.31839763373028,-2.31355964007905,-2.29270730497905,
-2.27457051600587,-2.26925197284302,-2.26565531310506,-2.26420006447268,
-2.26316209000569,-2.2620318174849,-2.26013611012157,-2.25344495903044,
-2.24688051099489,-2.2405835000354,-2.22609961801482),.UNSPECIFIED.);
#1624=B_SPLINE_CURVE_WITH_KNOTS('',3,(#121597,#121598,#121599,#121600,#121601,
#121602,#121603,#121604,#121605,#121606,#121607,#121608,#121609,#121610,
#121611,#121612,#121613,#121614,#121615,#121616,#121617,#121618,#121619,
#121620,#121621,#121622,#121623,#121624,#121625,#121626,#121627,#121628,
#121629,#121630,#121631,#121632,#121633,#121634,#121635,#121636,#121637,
#121638,#121639,#121640,#121641,#121642,#121643,#121644,#121645,#121646,
#121647,#121648,#121649,#121650,#121651,#121652,#121653,#121654,#121655,
#121656,#121657,#121658,#121659,#121660,#121661,#121662,#121663,#121664,
#121665,#121666,#121667,#121668,#121669,#121670,#121671,#121672,#121673,
#121674,#121675,#121676,#121677,#121678,#121679,#121680,#121681,#121682,
#121683,#121684,#121685,#121686,#121687,#121688,#121689,#121690,#121691,
#121692,#121693,#121694,#121695,#121696,#121697,#121698,#121699,#121700,
#121701,#121702,#121703,#121704,#121705,#121706,#121707,#121708,#121709,
#121710,#121711,#121712,#121713,#121714,#121715,#121716,#121717,#121718,
#121719,#121720,#121721,#121722,#121723,#121724,#121725,#121726,#121727,
#121728,#121729,#121730,#121731,#121732,#121733,#121734,#121735,#121736,
#121737,#121738,#121739,#121740,#121741,#121742,#121743,#121744,#121745,
#121746,#121747,#121748,#121749,#121750,#121751,#121752,#121753,#121754,
#121755,#121756,#121757,#121758,#121759,#121760,#121761,#121762,#121763,
#121764,#121765,#121766,#121767,#121768,#121769,#121770,#121771,#121772,
#121773,#121774,#121775,#121776,#121777,#121778,#121779,#121780,#121781,
#121782,#121783,#121784,#121785,#121786,#121787,#121788,#121789,#121790,
#121791,#121792,#121793,#121794,#121795,#121796,#121797,#121798,#121799,
#121800,#121801,#121802,#121803,#121804,#121805,#121806,#121807,#121808,
#121809,#121810,#121811,#121812,#121813,#121814,#121815,#121816,#121817,
#121818,#121819,#121820,#121821,#121822,#121823,#121824,#121825,#121826,
#121827,#121828,#121829,#121830,#121831,#121832,#121833,#121834,#121835,
#121836,#121837,#121838),.UNSPECIFIED.,.F.,.F.,(4,2,2,2,2,2,2,2,2,2,2,2,
2,2,2,2,2,2,2,2,2,2,2,2,2,2,2,2,2,2,2,2,2,2,2,2,2,2,2,2,2,2,2,2,2,2,2,2,
2,2,2,2,2,2,2,2,2,2,2,2,2,2,2,2,2,2,2,2,2,2,2,2,2,2,2,2,2,2,2,2,2,2,2,2,
2,2,2,2,2,2,2,2,2,2,2,2,2,2,2,2,2,2,2,2,2,2,2,2,2,2,2,2,2,2,2,2,2,2,2,2,
4),(-3.17249826874624,-3.15996572603712,-3.157529950244,-3.15570792548478,
-3.15398958290604,-3.15229751877215,-3.15003259406328,-3.14450001108718,
-3.13163795961908,-3.10262595841067,-3.09812298178249,-3.09653671995918,
-3.09547440212686,-3.09451803466948,-3.09293426290759,-3.08879133768354,
-3.06558234112219,-3.05075155693984,-3.04487784726782,-3.04039185782308,
-3.03815996048887,-3.03813008624643,-3.038098823617,-3.03806609921834,-3.03803183529047,
-3.03799594943884,-3.037958354382,-3.03791895762843,-3.0378776612519,-3.03785330622156,
-3.03782282349539,-3.03778467372763,-3.0377369341454,-3.03767720680599,
-3.03760250894207,-3.03752383761234,-3.0357030316206,-3.03337492711704,
-3.02851240858195,-3.0063911165544,-2.99175817505828,-2.98187903292201,
-2.97983211928711,-2.97866922844905,-2.97764276181246,-2.97628355749059,
-2.97316846357522,-2.95216989591933,-2.94231298690757,-2.92598537941526,
-2.92248908762707,-2.92043861528152,-2.91862145887172,-2.91632872476524,
-2.91165239880608,-2.88508965512769,-2.86523538391448,-2.86288366085681,
-2.86165593334355,-2.86063828518764,-2.85935050180203,-2.85728824587902,
-2.84239039005393,-2.83927346191504,-2.81867833424378,-2.8116151234893,
-2.80641105707509,-2.80401992766183,-2.80219107587269,-2.8001939239654,
-2.79694440017387,-2.78591222668791,-2.76276300193371,-2.75259060918443,
-2.74878399583113,-2.74598797163831,-2.74467225243698,-2.74365287369737,
-2.74244713445332,-2.74026351870955,-2.72873497984704,-2.70290988376886,
-2.69109561439306,-2.68788816846166,-2.6859001556504,-2.6840685702862,-2.68169844644491,
-2.67771255398351,-2.64868002347202,-2.63629863002996,-2.62990104654788,
-2.6281031535377,-2.62699487168615,-2.62595915763727,-2.62445590644093,
-2.6216241247957,-2.60103789025177,-2.58331614647095,-2.57679872877489,
-2.57190382443153,-2.56956941470045,-2.56774763218338,-2.56572131731914,
-2.5623375498601,-2.54976784915376,-2.51678453095886,-2.51226582424226,
-2.51067718289416,-2.5096141517007,-2.50865784006037,-2.50733388925779,
-2.50463059782684,-2.48140117165499,-2.46089262065977,-2.4551090437446,
-2.45261698569481,-2.45077266883969,-2.44881655782831,-2.44575829990954,
-2.43650710435452,-2.43074206186157),.UNSPECIFIED.);
#1625=B_SPLINE_CURVE_WITH_KNOTS('',3,(#121844,#121845,#121846,#121847,#121848,
#121849,#121850,#121851,#121852,#121853,#121854,#121855,#121856,#121857,
#121858,#121859,#121860,#121861,#121862,#121863,#121864,#121865,#121866,
#121867,#121868,#121869,#121870,#121871,#121872,#121873,#121874,#121875,
#121876,#121877,#121878,#121879,#121880,#121881,#121882,#121883,#121884,
#121885,#121886,#121887,#121888,#121889,#121890,#121891,#121892,#121893,
#121894,#121895,#121896,#121897,#121898,#121899,#121900,#121901,#121902,
#121903,#121904,#121905,#121906,#121907,#121908,#121909,#121910,#121911,
#121912,#121913,#121914,#121915,#121916,#121917,#121918,#121919,#121920,
#121921,#121922,#121923,#121924,#121925,#121926,#121927,#121928,#121929,
#121930,#121931,#121932,#121933,#121934,#121935,#121936,#121937,#121938,
#121939,#121940,#121941,#121942,#121943,#121944,#121945,#121946,#121947,
#121948,#121949,#121950,#121951,#121952,#121953,#121954,#121955,#121956,
#121957,#121958,#121959,#121960,#121961,#121962,#121963,#121964,#121965,
#121966,#121967,#121968,#121969,#121970,#121971,#121972,#121973,#121974,
#121975,#121976,#121977,#121978,#121979,#121980,#121981,#121982,#121983,
#121984,#121985,#121986,#121987,#121988,#121989,#121990,#121991,#121992,
#121993,#121994,#121995,#121996,#121997,#121998,#121999,#122000,#122001,
#122002,#122003),.UNSPECIFIED.,.F.,.F.,(4,2,2,2,2,2,2,2,2,2,2,2,2,2,2,2,
2,2,2,2,2,2,2,2,2,2,2,2,2,2,2,2,2,2,2,2,2,2,2,2,2,2,2,2,2,2,2,2,2,2,2,2,
2,2,2,2,2,2,2,2,2,2,2,2,2,2,2,2,2,2,2,2,2,2,2,2,2,2,2,4),(-0.53741600959432,
-0.534484832243604,-0.519854900077587,-0.512786627924429,-0.501043645279421,
-0.498850283075522,-0.497641989366339,-0.496622245743267,-0.49530834754258,
-0.492524155824832,-0.488739511942901,-0.478662573346859,-0.455844798656207,
-0.444459269895697,-0.441157627619831,-0.439148475591579,-0.437321587095685,
-0.434951562703679,-0.429868086290401,-0.423019805479859,-0.388456053145617,
-0.382977631523204,-0.381211419722964,-0.380109634403813,-0.379056725781395,
-0.37752030930671,-0.373385664998653,-0.366944843583964,-0.350032573219157,
-0.327956050256951,-0.324296892333281,-0.322188981340229,-0.320376151089173,
-0.318159630407206,-0.313875681754338,-0.308392189512478,-0.295131263573339,
-0.276072580496971,-0.26642335744724,-0.264332057561692,-0.263146559066483,
-0.262226231407268,-0.260936461599468,-0.258278639091771,-0.254716292615004,
-0.245551357234333,-0.223432343813054,-0.219982607683143,-0.209749035659174,
-0.206580727778321,-0.204600199583779,-0.202764199958113,-0.200330633835428,
-0.194893670207973,-0.17142556703497,-0.150823119788353,-0.147988968339029,
-0.146484558743827,-0.145448079924042,-0.144338981131448,-0.142539753285958,
-0.136218438314228,-0.124042816166063,-0.0947797854898783,-0.0903781093229487,
-0.0881090574085132,-0.0862927524872583,-0.0842239697971216,-0.0810315137100925,
-0.0671218210259667,-0.049808689118311,-0.0336457193529712,-0.0304704048723358,
-0.0292224599991369,-0.0281906302242398,-0.0270726134321287,-0.0259062656496201,
-0.0241633810584764,-0.0209596523026307,-9.99999999362622E-7),
 .UNSPECIFIED.);
#1626=B_SPLINE_CURVE_WITH_KNOTS('',3,(#122004,#122005,#122006,#122007,#122008,
#122009,#122010,#122011,#122012,#122013,#122014,#122015,#122016,#122017,
#122018,#122019,#122020,#122021,#122022,#122023,#122024,#122025,#122026,
#122027,#122028,#122029,#122030,#122031,#122032,#122033,#122034,#122035,
#122036,#122037,#122038,#122039,#122040,#122041,#122042,#122043,#122044,
#122045,#122046,#122047,#122048,#122049,#122050,#122051,#122052,#122053,
#122054,#122055,#122056,#122057,#122058,#122059,#122060,#122061),
 .UNSPECIFIED.,.F.,.F.,(4,2,2,2,2,2,2,2,2,2,2,2,2,2,2,2,2,2,2,2,2,2,2,2,
2,2,2,2,4),(-3.17264791624771,-3.15505568789391,-3.14811105788344,-3.14571795912332,
-3.14348337569644,-3.14166987417207,-3.13957692736989,-3.13598326905043,
-3.11889625329433,-3.0980938169293,-3.08771727849231,-3.08548745148271,
-3.08425564172295,-3.08323758771176,-3.08195301449682,-3.07990273649253,
-3.06579456529562,-3.042135875813,-3.03122600181549,-3.02781438490697,-3.0257814219777,
-3.02395989650779,-3.02163441749417,-3.01679064919694,-2.99317995059097,
-2.97721906467787,-2.97224790087894,-2.9688268726201,-2.96804921651682),
 .UNSPECIFIED.);
#1627=B_SPLINE_CURVE_WITH_KNOTS('',3,(#122062,#122063,#122064,#122065,#122066,
#122067,#122068,#122069,#122070,#122071,#122072,#122073,#122074,#122075,
#122076,#122077,#122078,#122079,#122080,#122081,#122082,#122083,#122084,
#122085,#122086,#122087,#122088,#122089,#122090,#122091,#122092,#122093,
#122094,#122095,#122096,#122097,#122098,#122099,#122100,#122101,#122102,
#122103,#122104,#122105,#122106,#122107,#122108,#122109,#122110,#122111,
#122112,#122113,#122114,#122115,#122116,#122117,#122118,#122119,#122120,
#122121,#122122,#122123,#122124,#122125,#122126,#122127,#122128,#122129,
#122130,#122131,#122132,#122133,#122134,#122135,#122136,#122137,#122138,
#122139,#122140,#122141,#122142,#122143,#122144,#122145,#122146,#122147,
#122148,#122149,#122150,#122151,#122152,#122153,#122154,#122155,#122156,
#122157,#122158,#122159,#122160,#122161,#122162,#122163,#122164,#122165,
#122166,#122167,#122168,#122169,#122170,#122171,#122172,#122173,#122174,
#122175,#122176,#122177,#122178,#122179,#122180,#122181,#122182,#122183,
#122184,#122185,#122186,#122187,#122188,#122189,#122190,#122191,#122192,
#122193,#122194,#122195,#122196,#122197,#122198,#122199,#122200,#122201,
#122202,#122203,#122204,#122205,#122206,#122207,#122208,#122209,#122210,
#122211,#122212,#122213,#122214,#122215,#122216,#122217,#122218,#122219,
#122220,#122221,#122222,#122223,#122224,#122225,#122226,#122227,#122228,
#122229,#122230,#122231,#122232,#122233,#122234,#122235,#122236,#122237,
#122238,#122239,#122240,#122241,#122242,#122243,#122244,#122245,#122246,
#122247,#122248,#122249,#122250,#122251,#122252,#122253,#122254,#122255,
#122256,#122257,#122258,#122259,#122260,#122261,#122262,#122263,#122264,
#122265),.UNSPECIFIED.,.F.,.F.,(4,2,2,2,2,2,2,2,2,2,2,2,2,2,2,2,2,2,2,2,
2,2,2,2,2,2,2,2,2,2,2,2,2,2,2,2,2,2,2,2,2,2,2,2,2,2,2,2,2,2,2,2,2,2,2,2,
2,2,2,2,2,2,2,2,2,2,2,2,2,2,2,2,2,2,2,2,2,2,2,2,2,2,2,2,2,2,2,2,2,2,2,2,
2,2,2,2,2,2,2,2,2,4),(-2.43074206186157,-2.4090569147898,-2.39724404997104,
-2.39441402941403,-2.39309173731544,-2.39207163503482,-2.3908701905365,
-2.38870648531317,-2.37767316280368,-2.34407760162979,-2.33799939804609,
-2.33545901911373,-2.33360665066793,-2.33189784981673,-2.32956593126672,
-2.32363291502396,-2.2889091748288,-2.27873194303697,-2.27666881871534,
-2.27550214106668,-2.27447608853296,-2.27312227022324,-2.27003972310494,
-2.24810593095924,-2.23128039512432,-2.22495134245193,-2.22016500351806,
-2.21785074144045,-2.21603082923062,-2.21399221563774,-2.21055300399553,
-2.19709354860412,-2.17079964462455,-2.16451717080728,-2.16045648992661,
-2.15893104801878,-2.15788056607248,-2.15691112567371,-2.15526036840917,
-2.15066541382706,-2.11510333833867,-2.1082013764317,-2.10308749213984,
-2.10071241106036,-2.09888539526737,-2.09687987329407,-2.09359293297056,
-2.08236515068073,-2.05917242582913,-2.0492084126796,-2.04545104019528,
-2.04268263341402,-2.04137198849434,-2.04035279662942,-2.03914282894785,
-2.03694089838078,-2.02498393131013,-2.01841566722429,-2.0043888570307,
-1.98833699660259,-1.98485346220588,-1.98280534318475,-1.9809871590231,
-1.97868893031814,-1.97398624522421,-1.94777049685608,-1.92757886243888,
-1.92523579783067,-1.92400963582356,-1.92299156692938,-1.92170107468881,
-1.91963043915727,-1.90293500712316,-1.88915843602945,-1.87128125497875,
-1.86771584884128,-1.86564998426402,-1.86383415040595,-1.86156293960789,
-1.85714839721741,-1.82846098495934,-1.81586772974028,-1.80940302599846,
-1.80759847251117,-1.80648848700649,-1.80545315353217,-1.80395335841114,
-1.80033667488877,-1.77661694535968,-1.75713805832133,-1.75165581368674,
-1.74921489748148,-1.747378348378,-1.7456429577935,-1.74271782478029,-1.7345447129076,
-1.70887823035537,-1.69435077256306,-1.69122943348981,-1.68985402446978,
-1.68882815015699,-1.68866836701421),.UNSPECIFIED.);
#1628=B_SPLINE_CURVE_WITH_KNOTS('',3,(#122270,#122271,#122272,#122273,#122274,
#122275,#122276,#122277,#122278,#122279,#122280,#122281,#122282,#122283,
#122284,#122285,#122286,#122287,#122288,#122289,#122290,#122291,#122292,
#122293,#122294,#122295,#122296,#122297,#122298,#122299,#122300,#122301,
#122302,#122303,#122304,#122305,#122306,#122307,#122308,#122309,#122310,
#122311,#122312,#122313,#122314,#122315,#122316,#122317,#122318,#122319,
#122320,#122321,#122322,#122323,#122324,#122325,#122326,#122327,#122328,
#122329,#122330,#122331,#122332,#122333,#122334,#122335,#122336,#122337,
#122338,#122339,#122340,#122341,#122342,#122343,#122344,#122345,#122346,
#122347,#122348,#122349,#122350,#122351,#122352,#122353,#122354,#122355,
#122356,#122357,#122358,#122359,#122360,#122361,#122362,#122363,#122364,
#122365,#122366,#122367,#122368,#122369,#122370,#122371,#122372,#122373,
#122374,#122375,#122376,#122377,#122378,#122379,#122380,#122381,#122382,
#122383,#122384,#122385,#122386,#122387,#122388,#122389,#122390,#122391,
#122392,#122393,#122394,#122395,#122396,#122397,#122398,#122399,#122400,
#122401,#122402,#122403,#122404,#122405,#122406,#122407,#122408,#122409,
#122410,#122411,#122412,#122413,#122414,#122415,#122416,#122417,#122418,
#122419,#122420,#122421,#122422,#122423,#122424,#122425,#122426,#122427,
#122428,#122429,#122430,#122431,#122432,#122433,#122434,#122435,#122436,
#122437,#122438,#122439,#122440,#122441,#122442,#122443,#122444,#122445,
#122446,#122447,#122448,#122449,#122450,#122451,#122452,#122453,#122454,
#122455,#122456,#122457,#122458,#122459,#122460,#122461,#122462,#122463,
#122464,#122465,#122466,#122467,#122468,#122469,#122470,#122471,#122472,
#122473,#122474,#122475,#122476,#122477,#122478,#122479,#122480,#122481),
 .UNSPECIFIED.,.F.,.F.,(4,2,2,2,2,2,2,2,2,2,2,2,2,2,2,2,2,2,2,2,2,2,2,2,
2,2,2,2,2,2,2,2,2,2,2,2,2,2,2,2,2,2,2,2,2,2,2,2,2,2,2,2,2,2,2,2,2,2,2,2,
2,2,2,2,2,2,2,2,2,2,2,2,2,2,2,2,2,2,2,2,2,2,2,2,2,2,2,2,2,2,2,2,2,2,2,2,
2,2,2,2,2,2,2,2,2,4),(-1.27924578165543,-1.27363190609435,-1.2642977297301,
-1.26122973084357,-1.25927146425767,-1.25742796374932,-1.25494140697023,
-1.24919109281031,-1.22936566748064,-1.20529050297461,-1.2023621082489,
-1.20103577987058,-1.20001308664896,-1.19882947187116,-1.19668788578905,
-1.18475869372216,-1.16952282675743,-1.14835190002979,-1.14468473223606,
-1.142575611829,-1.14076373297092,-1.13855087682873,-1.13428204777997,-1.11481019004502,
-1.09451565542147,-1.08661733085815,-1.08461569158226,-1.08346239205533,
-1.08243285547877,-1.08102981810248,-1.07774846564997,-1.07304738312471,
-1.05860561927177,-1.03286582706281,-1.02813720395848,-1.02583395193099,
-1.02401518244914,-1.02196995912114,-1.01850013800645,-1.00272081400972,
-0.97886595052194,-0.969606756653152,-0.967537518435581,-0.966357306748276,
-0.965436626301309,-0.964140581092339,-0.961448788895081,-0.957826721370322,
-0.948419697753517,-0.943730926363833,-0.915317806405154,-0.910876294510142,
-0.908599503501079,-0.906783222421048,-0.904721151758604,-0.901173245196586,
-0.883725870038095,-0.860957991008182,-0.852349631852284,-0.850321839434271,
-0.849151056019276,-0.848228745774727,-0.846918651915113,-0.844153594702399,
-0.840402605742695,-0.830465518135808,-0.807339613158091,-0.796053612439536,
-0.792761304123363,-0.79075446003744,-0.788927490730511,-0.786554248729905,
-0.781451429737925,-0.774568393654032,-0.739380289571229,-0.734456982475254,
-0.732761011859199,-0.731782603874834,-0.730738567977097,-0.729248314777892,
-0.725425990236165,-0.719647779091906,-0.698113708376985,-0.679547984343296,
-0.675911456109227,-0.673808888170751,-0.671996121473987,-0.669773954229791,
-0.665460548821992,-0.650153266734758,-0.625390789732032,-0.617800454356525,
-0.615825747012055,-0.614678148095272,-0.613646521560169,-0.612230784497594,
-0.608875621559339,-0.604033050420835,-0.588812496673201,-0.564165628442818,
-0.559385140058434,-0.557071611044161,-0.55525133964979,-0.553211339052226,
-0.549767352328332,-0.53741600959432),.UNSPECIFIED.);
#1629=B_SPLINE_CURVE_WITH_KNOTS('',3,(#122482,#122483,#122484,#122485,#122486,
#122487,#122488,#122489,#122490,#122491,#122492,#122493,#122494,#122495,
#122496,#122497,#122498,#122499,#122500,#122501,#122502,#122503,#122504,
#122505,#122506,#122507,#122508,#122509,#122510,#122511,#122512,#122513,
#122514,#122515,#122516,#122517,#122518,#122519,#122520,#122521,#122522,
#122523,#122524,#122525,#122526,#122527,#122528,#122529,#122530,#122531,
#122532,#122533,#122534,#122535,#122536,#122537,#122538,#122539,#122540,
#122541,#122542,#122543,#122544,#122545,#122546,#122547,#122548,#122549,
#122550,#122551,#122552,#122553,#122554,#122555,#122556,#122557,#122558,
#122559,#122560,#122561,#122562,#122563,#122564,#122565,#122566,#122567,
#122568,#122569,#122570,#122571,#122572,#122573,#122574,#122575,#122576,
#122577,#122578,#122579,#122580,#122581,#122582,#122583,#122584,#122585,
#122586,#122587,#122588,#122589,#122590,#122591,#122592,#122593,#122594,
#122595,#122596,#122597,#122598,#122599,#122600,#122601,#122602,#122603,
#122604,#122605,#122606,#122607,#122608,#122609,#122610,#122611,#122612,
#122613,#122614,#122615,#122616,#122617,#122618,#122619,#122620,#122621,
#122622,#122623,#122624,#122625,#122626,#122627,#122628,#122629,#122630,
#122631,#122632,#122633,#122634,#122635,#122636,#122637,#122638,#122639,
#122640,#122641,#122642,#122643,#122644,#122645,#122646,#122647,#122648,
#122649,#122650,#122651,#122652,#122653,#122654,#122655,#122656,#122657,
#122658,#122659,#122660,#122661,#122662,#122663,#122664,#122665,#122666,
#122667,#122668,#122669,#122670,#122671,#122672,#122673,#122674,#122675,
#122676,#122677,#122678,#122679,#122680,#122681,#122682,#122683,#122684,
#122685,#122686,#122687,#122688,#122689),.UNSPECIFIED.,.F.,.F.,(4,2,2,2,
2,2,2,2,2,2,2,2,2,2,2,2,2,2,2,2,2,2,2,2,2,2,2,2,2,2,2,2,2,2,2,2,2,2,2,2,
2,2,2,2,2,2,2,2,2,2,2,2,2,2,2,2,2,2,2,2,2,2,2,2,2,2,2,2,2,2,2,2,2,2,2,2,
2,2,2,2,2,2,2,2,2,2,2,2,2,2,2,2,2,2,2,2,2,2,2,2,2,2,2,4),(-1.68866836701421,
-1.68766003423988,-1.6856441604167,-1.67721851905643,-1.65335343849554,
-1.63810952549874,-1.63380486913827,-1.63158465220404,-1.62977223375796,
-1.62766868049812,-1.62402696439383,-1.60219375242694,-1.58623145092022,
-1.57564406792919,-1.57349871134111,-1.57230127023743,-1.57128048908813,
-1.56995203104287,-1.56708970214844,-1.54866551661408,-1.52138662442643,
-1.5167693673048,-1.51448745315367,-1.51267062076208,-1.51061171569116,
-1.50707889302881,-1.48999019440203,-1.46483184721473,-1.45794703092893,
-1.45603453311759,-1.45490071366645,-1.45386448642712,-1.4524187272107,
-1.44888014014972,-1.44367788574291,-1.42629671695579,-1.40454044140624,
-1.39968518745367,-1.39735771198411,-1.39553615420813,-1.3935047444938,
-1.3900996068696,-1.37548984238613,-1.36034594721379,-1.35464908177789,
-1.34135625090745,-1.33932228955552,-1.33804271129841,-1.33702498931849,
-1.33578919905587,-1.33339987244181,-1.33029517854445,-1.32286166325756,
-1.30703877634558,-1.28549539029785,-1.28180856903748,-1.27969487980205,
-1.2778830066361,-1.27567508402203,-1.27143154808291,-1.26601397942529,
-1.25300387770382,-1.23467307055161,-1.22401733820856,-1.22186906649175,
-1.22067096231294,-1.21965025107821,-1.21832270910871,-1.2154653455333,
-1.20341724369821,-1.17519556375446,-1.16678899363816,-1.16383428965986,
-1.16189998836635,-1.16004392430862,-1.15748433761299,-1.15128860406224,
-1.14236223506171,-1.12629683593003,-1.1084254567127,-1.10521449493295,
-1.10396122945004,-1.10292838564219,-1.10181362539722,-1.09998738289662,
-1.09328353553487,-1.07990326569269,-1.05253619241229,-1.04792748526969,
-1.04564728977325,-1.04383068209268,-1.04177080822787,-1.03823322455044,
-1.02103273135173,-0.996631374783848,-0.98920258671719,-0.987242851936966,
-0.986098684347984,-0.98506625075259,-0.983644075971947,-0.980249305024847,
-0.975329701243524,-0.95966761514608,-0.946673080131941),.UNSPECIFIED.);
#1630=B_SPLINE_CURVE_WITH_KNOTS('',3,(#122694,#122695,#122696,#122697,#122698,
#122699,#122700,#122701,#122702,#122703,#122704,#122705,#122706,#122707,
#122708,#122709,#122710,#122711,#122712,#122713,#122714,#122715,#122716,
#122717,#122718,#122719,#122720,#122721,#122722,#122723,#122724,#122725,
#122726,#122727,#122728,#122729,#122730,#122731,#122732,#122733,#122734,
#122735,#122736,#122737,#122738,#122739,#122740,#122741,#122742,#122743,
#122744,#122745,#122746,#122747,#122748,#122749,#122750,#122751,#122752,
#122753,#122754,#122755,#122756,#122757,#122758,#122759,#122760,#122761,
#122762,#122763,#122764,#122765,#122766,#122767,#122768,#122769,#122770,
#122771,#122772,#122773,#122774,#122775,#122776,#122777,#122778,#122779,
#122780,#122781,#122782,#122783,#122784,#122785,#122786,#122787,#122788,
#122789,#122790,#122791,#122792,#122793,#122794,#122795,#122796,#122797,
#122798,#122799,#122800,#122801,#122802,#122803,#122804,#122805,#122806,
#122807,#122808,#122809,#122810,#122811,#122812,#122813,#122814,#122815,
#122816,#122817,#122818,#122819,#122820,#122821,#122822,#122823,#122824,
#122825,#122826,#122827,#122828,#122829,#122830,#122831,#122832,#122833,
#122834,#122835,#122836,#122837,#122838,#122839,#122840,#122841,#122842,
#122843,#122844,#122845,#122846,#122847,#122848,#122849,#122850,#122851,
#122852,#122853,#122854,#122855,#122856,#122857,#122858,#122859,#122860,
#122861,#122862,#122863,#122864,#122865,#122866,#122867,#122868,#122869,
#122870,#122871,#122872,#122873,#122874,#122875,#122876,#122877,#122878,
#122879,#122880,#122881,#122882,#122883,#122884,#122885,#122886,#122887,
#122888,#122889,#122890,#122891,#122892,#122893,#122894,#122895,#122896,
#122897,#122898,#122899,#122900,#122901,#122902,#122903,#122904,#122905),
 .UNSPECIFIED.,.F.,.F.,(4,2,2,2,2,2,2,2,2,2,2,2,2,2,2,2,2,2,2,2,2,2,2,2,
2,2,2,2,2,2,2,2,2,2,2,2,2,2,2,2,2,2,2,2,2,2,2,2,2,2,2,2,2,2,2,2,2,2,2,2,
2,2,2,2,2,2,2,2,2,2,2,2,2,2,2,2,2,2,2,2,2,2,2,2,2,2,2,2,2,2,2,2,2,2,2,2,
2,2,2,2,2,2,2,2,2,4),(-2.02096473940897,-2.0207001392651,-2.01966945009549,
-2.01842486118067,-2.0152685424195,-1.99515219974244,-1.97126241300299,
-1.96583507629916,-1.96340398073594,-1.96156911882332,-1.95958912000209,
-1.95642013419931,-1.94617045210257,-1.92235583906836,-1.9214297946144,
-1.9117088824231,-1.90801016868078,-1.90527499978267,-1.90397068781599,
-1.9029519058378,-1.90173700694308,-1.89951292524769,-1.88642369092045,
-1.88055889265947,-1.86547088755815,-1.85081923536881,-1.84741228612423,
-1.84538070415464,-1.84355954433598,-1.84123332963993,-1.8363835113232,
-1.81566520436901,-1.79745118092209,-1.79212206588293,-1.7885204839487,
-1.78706477697706,-1.7860270171828,-1.78489756770433,-1.78300439878093,
-1.7763360747173,-1.7697705313992,-1.75234065077155,-1.73415217818814,-1.73052424934472,
-1.72842395480023,-1.72661155391675,-1.7243878154464,-1.7200647842999,-1.69003315527847,
-1.67298354502583,-1.67091102683763,-1.66961996453208,-1.66860183748791,
-1.66737604028128,-1.66503484169274,-1.662010158347,-1.62914395437748,-1.6164212327105,
-1.61302751305175,-1.61099881182171,-1.60917710618397,-1.60684586582125,
-1.60196922788607,-1.59548303547423,-1.57791396803449,-1.55707633338049,
-1.55395031816943,-1.55258893341696,-1.55156188425926,-1.55039951748663,
-1.54835615770544,-1.53854999290055,-1.52414341589642,-1.50169758667576,
-1.49686240702736,-1.49453897672409,-1.49271814459168,-1.49068501187754,
-1.48727083626137,-1.47249854911327,-1.45748153307026,-1.45106850387174,
-1.43857029121308,-1.43653712334913,-1.43525790644315,-1.43424036755935,
-1.43300464325958,-1.43061497350352,-1.42750950428366,-1.42007225407143,
-1.40426248153534,-1.38269506585492,-1.37903197992924,-1.37692384113659,
-1.37511200629303,-1.37289820000553,-1.36862431350211,-1.34699163713018,
-1.32238427279142,-1.31951282693004,-1.31819688750572,-1.31717529623337,
-1.31598471622319,-1.3138105949162,-1.30098464557554,-1.27924578165543),
 .UNSPECIFIED.);
#1631=B_SPLINE_CURVE_WITH_KNOTS('',3,(#122906,#122907,#122908,#122909,#122910,
#122911,#122912,#122913,#122914,#122915,#122916,#122917,#122918,#122919,
#122920,#122921,#122922,#122923,#122924,#122925,#122926,#122927,#122928,
#122929,#122930,#122931,#122932,#122933,#122934,#122935,#122936,#122937,
#122938,#122939,#122940,#122941,#122942,#122943,#122944,#122945,#122946,
#122947,#122948,#122949,#122950,#122951,#122952,#122953,#122954,#122955,
#122956,#122957,#122958,#122959,#122960,#122961,#122962,#122963,#122964,
#122965,#122966,#122967,#122968,#122969,#122970,#122971,#122972,#122973,
#122974,#122975,#122976,#122977,#122978,#122979,#122980,#122981,#122982,
#122983,#122984,#122985,#122986,#122987,#122988,#122989,#122990,#122991,
#122992,#122993,#122994,#122995,#122996,#122997,#122998,#122999,#123000,
#123001,#123002,#123003,#123004,#123005,#123006,#123007,#123008,#123009,
#123010,#123011,#123012,#123013,#123014,#123015,#123016,#123017,#123018,
#123019,#123020,#123021,#123022,#123023,#123024,#123025,#123026,#123027,
#123028,#123029,#123030,#123031,#123032,#123033,#123034,#123035,#123036,
#123037,#123038,#123039,#123040,#123041,#123042,#123043,#123044,#123045,
#123046,#123047,#123048,#123049,#123050,#123051,#123052,#123053,#123054,
#123055,#123056,#123057,#123058,#123059,#123060,#123061,#123062,#123063,
#123064,#123065,#123066,#123067,#123068,#123069,#123070,#123071,#123072,
#123073,#123074,#123075,#123076,#123077,#123078,#123079,#123080,#123081,
#123082,#123083,#123084,#123085,#123086,#123087,#123088,#123089,#123090,
#123091,#123092,#123093,#123094,#123095,#123096,#123097,#123098,#123099,
#123100,#123101,#123102,#123103,#123104,#123105,#123106,#123107,#123108,
#123109,#123110,#123111,#123112,#123113,#123114,#123115,#123116,#123117),
 .UNSPECIFIED.,.F.,.F.,(4,2,2,2,2,2,2,2,2,2,2,2,2,2,2,2,2,2,2,2,2,2,2,2,
2,2,2,2,2,2,2,2,2,2,2,2,2,2,2,2,2,2,2,2,2,2,2,2,2,2,2,2,2,2,2,2,2,2,2,2,
2,2,2,2,2,2,2,2,2,2,2,2,2,2,2,2,2,2,2,2,2,2,2,2,2,2,2,2,2,2,2,2,2,2,2,2,
2,2,2,2,2,2,2,2,2,4),(-0.946673080131941,-0.935626006097239,-0.930823601939602,
-0.928506193560378,-0.92668583442944,-0.924648829194281,-0.921217475209467,
-0.906153837844209,-0.891343295666385,-0.884392217971758,-0.87247788876375,
-0.870277544085949,-0.869067839219171,-0.868048471210341,-0.866737101317524,
-0.863965411416058,-0.860202762729112,-0.850217585935452,-0.827024272926127,
-0.815840526288103,-0.81255738436404,-0.810552505904783,-0.80872498722333,
-0.806347692829656,-0.801222818589417,-0.794300799206035,-0.758401741841977,
-0.754063973351398,-0.752451587588511,-0.751489408091924,-0.750431919954055,
-0.748871715256692,-0.744566193094111,-0.737748837531389,-0.713139203061365,
-0.698961982861916,-0.695474001672571,-0.693424537578214,-0.691787821654563,
-0.689578597318098,-0.685329515246036,-0.679903059085688,-0.666860115880548,
-0.648434847417636,-0.637906155227199,-0.635763822650013,-0.634566956589963,
-0.633545930416142,-0.632216197126501,-0.629347641449624,-0.617202843921097,
-0.588483038482858,-0.580546844005023,-0.577653746245591,-0.575924255590045,
-0.574084246106177,-0.571621989604517,-0.566017280792925,-0.551719748590105,
-0.528867530047163,-0.520442056219144,-0.518425922436248,-0.517257660152455,
-0.516231646089653,-0.514856058674415,-0.511734291946429,-0.497205469745065,
-0.471529893004746,-0.463380141304061,-0.460457723407912,-0.458722682847371,
-0.456885568607325,-0.454442313596543,-0.448947912763836,-0.425437939714836,
-0.404965998159196,-0.402126943930736,-0.400621421142603,-0.399584912143404,
-0.398476579557482,-0.396680093219113,-0.390303479771554,-0.377993408307067,
-0.348839715601933,-0.344866157587136,-0.342498903767759,-0.340666992245494,
-0.338676086111014,-0.33545829751017,-0.323532117757917,-0.29712737881507,
-0.286210775684609,-0.28405125746133,-0.282850529357465,-0.281829973841278,
-0.280505733202747,-0.277666635066594,-0.265779840422882,-0.238163707008377,
-0.229121938702919,-0.226088026588155,-0.224136694904447,-0.222289224506927,
-0.219780937754473,-0.213902979691889,-0.204532409010266),.UNSPECIFIED.);
#1632=B_SPLINE_CURVE_WITH_KNOTS('',3,(#123122,#123123,#123124,#123125,#123126,
#123127,#123128,#123129,#123130,#123131,#123132,#123133,#123134,#123135,
#123136,#123137,#123138,#123139,#123140,#123141,#123142,#123143,#123144,
#123145,#123146,#123147,#123148,#123149,#123150,#123151,#123152,#123153,
#123154,#123155,#123156,#123157,#123158,#123159,#123160,#123161,#123162,
#123163,#123164,#123165,#123166,#123167,#123168,#123169,#123170,#123171,
#123172,#123173,#123174,#123175,#123176,#123177,#123178,#123179,#123180,
#123181,#123182,#123183,#123184,#123185,#123186,#123187,#123188,#123189,
#123190,#123191,#123192,#123193,#123194,#123195,#123196,#123197,#123198,
#123199,#123200,#123201,#123202,#123203,#123204,#123205,#123206,#123207,
#123208,#123209,#123210,#123211,#123212,#123213,#123214,#123215,#123216,
#123217,#123218,#123219,#123220,#123221,#123222,#123223,#123224,#123225,
#123226,#123227,#123228,#123229,#123230,#123231,#123232,#123233,#123234,
#123235,#123236,#123237,#123238,#123239,#123240,#123241,#123242,#123243,
#123244,#123245,#123246,#123247,#123248,#123249,#123250,#123251,#123252,
#123253,#123254,#123255,#123256,#123257,#123258,#123259,#123260,#123261,
#123262,#123263,#123264,#123265,#123266,#123267,#123268,#123269,#123270,
#123271,#123272,#123273,#123274,#123275,#123276,#123277,#123278,#123279,
#123280,#123281,#123282,#123283,#123284,#123285,#123286,#123287,#123288,
#123289,#123290,#123291,#123292,#123293,#123294,#123295,#123296,#123297,
#123298,#123299,#123300,#123301,#123302,#123303,#123304,#123305,#123306,
#123307,#123308,#123309,#123310,#123311,#123312,#123313,#123314,#123315,
#123316,#123317,#123318,#123319,#123320,#123321,#123322,#123323),
 .UNSPECIFIED.,.F.,.F.,(4,2,2,2,2,2,2,2,2,2,2,2,2,2,2,2,2,2,2,2,2,2,2,2,
2,2,2,2,2,2,2,2,2,2,2,2,2,2,2,2,2,2,2,2,2,2,2,2,2,2,2,2,2,2,2,2,2,2,2,2,
2,2,2,2,2,2,2,2,2,2,2,2,2,2,2,2,2,2,2,2,2,2,2,2,2,2,2,2,2,2,2,2,2,2,2,2,
2,2,2,2,4),(-2.7627136742397,-2.74760750538693,-2.72756916375101,-2.72523029199539,
-2.72400534826976,-2.72298773880131,-2.72169711456732,-2.71962489439385,
-2.70247686396111,-2.68193471826147,-2.6705609044919,-2.66739090472042,
-2.66541122098641,-2.66357729275388,-2.66118988637063,-2.65585952912302,
-2.61797084562576,-2.61242594454177,-2.60871789594637,-2.60724566909461,
-2.6062052368122,-2.60508256720467,-2.60321981134333,-2.59686203922748,
-2.56610720588711,-2.5577716816043,-2.55188012910689,-2.54937023693817,
-2.54752306269227,-2.54580703469866,-2.54298381485341,-2.53554142777646,
-2.50274358845909,-2.49271029691211,-2.49065471525136,-2.48948967859719,
-2.48846329009461,-2.48710664973158,-2.48400758364922,-2.46256886503251,
-2.44542381011884,-2.43902701285583,-2.43420159701271,-2.43188008523737,
-2.43005954725324,-2.42802549060667,-2.42460672876648,-2.41147393581952,
-2.38487628181305,-2.37856780832695,-2.37449526167128,-2.37296821996719,
-2.37191751645818,-2.37081362773828,-2.36903625070745,-2.36345865803876,
-2.32904303053547,-2.32220734697397,-2.31713105174476,-2.31476298711301,
-2.31293702456317,-2.31092830502834,-2.30762602542793,-2.29596060092727,
-2.27333996513071,-2.26331827752009,-2.25954740692162,-2.25677148058451,
-2.25545948817148,-2.25444959454968,-2.25324483074787,-2.2510659748943,
-2.23965723364532,-2.21858202528268,-2.20244174064115,-2.1989542064734,
-2.19690535746983,-2.19508749950381,-2.19279098579296,-2.18809645651082,
-2.16179099851405,-2.14772072408464,-2.14081765617953,-2.13897415466464,
-2.13785571521514,-2.1368249113606,-2.13557965889867,-2.13241884878729,
-2.11261622874445,-2.10134724215732,-2.08528250050539,-2.08179858226312,
-2.07975044500786,-2.07793236112261,-2.0756344057589,-2.07093275342417,
-2.0447267828665,-2.0305871921962,-2.023664271598,-2.02181900182672,-2.02096473940897),
 .UNSPECIFIED.);
#1633=B_SPLINE_CURVE_WITH_KNOTS('',3,(#123325,#123326,#123327,#123328,#123329,
#123330,#123331,#123332,#123333,#123334,#123335,#123336,#123337,#123338,
#123339,#123340,#123341,#123342,#123343,#123344,#123345,#123346,#123347,
#123348,#123349,#123350,#123351,#123352,#123353,#123354,#123355,#123356,
#123357,#123358,#123359,#123360,#123361,#123362,#123363,#123364,#123365,
#123366,#123367,#123368,#123369,#123370,#123371,#123372,#123373,#123374,
#123375,#123376,#123377,#123378,#123379,#123380,#123381,#123382,#123383,
#123384,#123385,#123386,#123387,#123388,#123389,#123390,#123391,#123392),
 .UNSPECIFIED.,.F.,.F.,(4,2,2,2,2,2,2,2,2,2,2,2,2,2,2,2,2,2,2,2,2,2,2,2,
2,2,2,2,2,2,2,2,2,4),(-0.204532409010266,-0.194924932902125,-0.171058061330753,
-0.167580129499482,-0.166245255876008,-0.165285928558312,-0.164225470541549,
-0.162650657065151,-0.158238086983778,-0.125426654891204,-0.112590818373553,
-0.109184993804583,-0.10715335998345,-0.105414591283973,-0.105351688545113,
-0.105292623790695,-0.105236888767858,-0.105184055192759,-0.105133758874891,
-0.105085687463357,-0.102894543815645,-0.100315808264756,-0.0959954645696802,
-0.0867881052724889,-0.0710444130250007,-0.053306962456332,-0.050147685259005,
-0.0488816456134193,-0.0478455880490776,-0.0467366517880079,-0.044937191567511,
-0.0385279941781553,-0.0261139800210841,-1.0000001292032E-6),
 .UNSPECIFIED.);
#1634=B_SPLINE_CURVE_WITH_KNOTS('',3,(#123393,#123394,#123395,#123396,#123397,
#123398,#123399,#123400,#123401,#123402,#123403,#123404,#123405,#123406,
#123407,#123408,#123409,#123410,#123411,#123412,#123413,#123414,#123415,
#123416,#123417,#123418,#123419,#123420,#123421,#123422,#123423,#123424,
#123425,#123426,#123427,#123428,#123429,#123430,#123431,#123432,#123433,
#123434,#123435,#123436,#123437,#123438,#123439,#123440,#123441,#123442,
#123443,#123444,#123445,#123446,#123447,#123448,#123449,#123450,#123451,
#123452,#123453,#123454,#123455,#123456,#123457,#123458,#123459,#123460,
#123461,#123462,#123463,#123464,#123465,#123466,#123467,#123468,#123469,
#123470,#123471,#123472,#123473,#123474,#123475,#123476,#123477,#123478,
#123479,#123480,#123481,#123482,#123483,#123484,#123485,#123486,#123487,
#123488,#123489,#123490,#123491,#123492,#123493,#123494,#123495,#123496,
#123497,#123498,#123499,#123500,#123501,#123502,#123503,#123504,#123505,
#123506,#123507,#123508,#123509,#123510,#123511,#123512,#123513,#123514,
#123515,#123516,#123517,#123518,#123519,#123520,#123521,#123522,#123523,
#123524,#123525,#123526,#123527,#123528,#123529,#123530,#123531,#123532,
#123533,#123534,#123535,#123536,#123537,#123538,#123539,#123540,#123541,
#123542,#123543,#123544,#123545,#123546,#123547,#123548,#123549,#123550,
#123551,#123552,#123553,#123554,#123555,#123556,#123557,#123558),
 .UNSPECIFIED.,.F.,.F.,(4,2,2,2,2,2,2,2,2,2,2,2,2,2,2,2,2,2,2,2,2,2,2,2,
2,2,2,2,2,2,2,2,2,2,2,2,2,2,2,2,2,2,2,2,2,2,2,2,2,2,2,2,2,2,2,2,2,2,2,2,
2,2,2,2,2,2,2,2,2,2,2,2,2,2,2,2,2,2,2,2,2,2,4),(-1.81503280713751,-1.81069981961972,
-1.80759276479933,-1.80580583034795,-1.80406479795658,-1.80209824698256,
-1.79898871711039,-1.78926359027205,-1.76295057239896,-1.75068537642654,
-1.74780444958829,-1.74647302196291,-1.74546171232084,-1.74427142252917,
-1.74215590334836,-1.73200843122411,-1.71333810717845,-1.70021960555422,
-1.69477478505897,-1.69175866186095,-1.68971040142769,-1.6877555233977,
-1.68602911904562,-1.68370725577307,-1.67887703274963,-1.65855113979732,
-1.64110174187218,-1.63506485100915,-1.63111999738201,-1.62961202629393,
-1.6285652877668,-1.6274559475313,-1.62565240929404,-1.61984272044714,-1.58568991710473,
-1.57887130130342,-1.5738051126339,-1.57143952335733,-1.56961455121706,
-1.56760600912896,-1.5643019264818,-1.55286714756856,-1.52980751085361,
-1.51993809569984,-1.51620413605914,-1.51344930902468,-1.5121416681231,
-1.51122015751256,-1.51004910805787,-1.50801819129573,-1.49933752343943,
-1.47962099595857,-1.46612766114278,-1.45786695651096,-1.4550191289998,
-1.45310805176318,-1.4512601882012,-1.44863828804738,-1.44250965410269,
-1.41489418244456,-1.41178533340499,-1.40252842423068,-1.39894431739321,
-1.39627479936842,-1.3949835313354,-1.39406385318909,-1.39288160338511,
-1.39080144874296,-1.38132764517926,-1.3808517104182,-1.35760121078074,
-1.34195867604981,-1.33849763362988,-1.33645508445692,-1.3346371710014,
-1.33233294992883,-1.32759494175085,-1.30204640962113,-1.28746206108587,
-1.28273540121226,-1.27944140541104,-1.27803671668043,-1.27782408552841),
 .UNSPECIFIED.);
#1635=B_SPLINE_CURVE_WITH_KNOTS('',3,(#123563,#123564,#123565,#123566,#123567,
#123568,#123569,#123570,#123571,#123572,#123573,#123574,#123575,#123576,
#123577,#123578,#123579,#123580,#123581,#123582,#123583,#123584,#123585,
#123586,#123587,#123588,#123589,#123590,#123591,#123592,#123593,#123594,
#123595,#123596,#123597,#123598,#123599,#123600,#123601,#123602,#123603,
#123604,#123605,#123606,#123607,#123608,#123609,#123610,#123611,#123612,
#123613,#123614,#123615,#123616,#123617,#123618,#123619,#123620,#123621,
#123622,#123623,#123624,#123625,#123626,#123627,#123628,#123629,#123630,
#123631,#123632,#123633,#123634,#123635,#123636,#123637,#123638,#123639,
#123640,#123641,#123642,#123643,#123644,#123645,#123646,#123647,#123648,
#123649,#123650,#123651,#123652,#123653,#123654,#123655,#123656,#123657,
#123658,#123659,#123660,#123661,#123662,#123663,#123664,#123665,#123666,
#123667,#123668,#123669,#123670,#123671,#123672,#123673,#123674,#123675,
#123676,#123677,#123678,#123679,#123680,#123681,#123682,#123683,#123684,
#123685,#123686,#123687,#123688,#123689,#123690,#123691,#123692,#123693,
#123694,#123695,#123696,#123697,#123698,#123699,#123700,#123701,#123702,
#123703,#123704,#123705,#123706,#123707,#123708,#123709,#123710,#123711,
#123712,#123713,#123714,#123715,#123716,#123717,#123718,#123719,#123720,
#123721,#123722,#123723,#123724,#123725,#123726,#123727,#123728,#123729,
#123730,#123731,#123732,#123733,#123734,#123735,#123736,#123737,#123738,
#123739,#123740,#123741,#123742,#123743,#123744,#123745,#123746,#123747,
#123748,#123749,#123750,#123751,#123752,#123753,#123754,#123755,#123756,
#123757,#123758,#123759,#123760,#123761,#123762,#123763,#123764,#123765,
#123766,#123767,#123768,#123769,#123770,#123771,#123772,#123773,#123774,
#123775,#123776,#123777,#123778),.UNSPECIFIED.,.F.,.F.,(4,2,2,2,2,2,2,2,
2,2,2,2,2,2,2,2,2,2,2,2,2,2,2,2,2,2,2,2,2,2,2,2,2,2,2,2,2,2,2,2,2,2,2,2,
2,2,2,2,2,2,2,2,2,2,2,2,2,2,2,2,2,2,2,2,2,2,2,2,2,2,2,2,2,2,2,2,2,2,2,2,
2,2,2,2,2,2,2,2,2,2,2,2,2,2,2,2,2,2,2,2,2,2,2,2,2,2,2,4),(-3.50413679931849,
-3.49590987031219,-3.49100908839452,-3.48860580968547,-3.48679049718976,
-3.48505425934406,-3.48333887870094,-3.48100178508058,-3.47507574420192,
-3.46212039058586,-3.4369866640505,-3.4320360545749,-3.42862446149258,-3.42719904529355,
-3.42616712469117,-3.42503194270083,-3.42309244796776,-3.4158099622432,
-3.39508062099519,-3.38118444829873,-3.37554950017391,-3.37246772029541,
-3.36978904110003,-3.36793947953406,-3.36609627761575,-3.36344886980306,
-3.35706623725807,-3.32956258591042,-3.32661252784782,-3.31400625547146,
-3.31109577402588,-3.30976516605439,-3.30875766895029,-3.30757401278248,
-3.30548940801067,-3.29594876245353,-3.27683265978024,-3.26354729792033,
-3.2580546351264,-3.25376292148752,-3.25154251098197,-3.24972643626906,
-3.24761455977581,-3.24394754645604,-3.22281910613394,-3.20751639591832,
-3.19579692305258,-3.19365860294311,-3.19247285593897,-3.1914475180448,
-3.19011509057152,-3.18715699906652,-3.16344576325454,-3.14112639399976,
-3.13685335263498,-3.13463966382662,-3.13282773953272,-3.1307192775451,
-3.12705507922154,-3.10538545893922,-3.0894919765626,-3.07857452758075,
-3.07647644664878,-3.07530268378633,-3.07427947089646,-3.07294077941223,
-3.06993792494916,-3.04689019301246,-3.02631410306661,-3.02047959131481,
-3.01798093165929,-3.01613735335176,-3.01418722248511,-3.01114920317816,
-3.00204915819561,-2.9744754598127,-2.9626146412364,-2.95978073152702,-2.95845876314082,
-2.95743945954545,-2.95623932141187,-2.9540808568736,-2.94316287873158,
-2.90954003559155,-2.90341166898242,-2.90086310015065,-2.89900915166713,
-2.89730192170372,-2.89452753337548,-2.88741260709016,-2.86079519058316,
-2.85865434170654,-2.84532430335765,-2.84259059757052,-2.84128636783062,
-2.84026753860776,-2.83905249035476,-2.83682697913635,-2.82389353315059,
-2.81855228183661,-2.80449603841603,-2.78831602751527,-2.78482726838424,
-2.78277849255522,-2.78096118025786,-2.77866600531978,-2.77397657432156,
-2.7627136742397),.UNSPECIFIED.);
#1636=B_SPLINE_CURVE_WITH_KNOTS('',3,(#123779,#123780,#123781,#123782,#123783,
#123784,#123785,#123786,#123787,#123788,#123789,#123790,#123791,#123792,
#123793,#123794,#123795,#123796,#123797,#123798,#123799,#123800,#123801,
#123802,#123803,#123804,#123805,#123806,#123807,#123808,#123809,#123810,
#123811,#123812,#123813,#123814,#123815,#123816,#123817,#123818,#123819,
#123820,#123821,#123822,#123823,#123824,#123825,#123826,#123827,#123828,
#123829,#123830,#123831,#123832,#123833,#123834,#123835,#123836,#123837,
#123838,#123839,#123840,#123841,#123842,#123843,#123844,#123845,#123846,
#123847,#123848,#123849,#123850,#123851,#123852,#123853,#123854,#123855,
#123856,#123857,#123858,#123859,#123860,#123861,#123862,#123863,#123864,
#123865,#123866,#123867,#123868,#123869,#123870,#123871,#123872,#123873,
#123874,#123875,#123876,#123877,#123878,#123879,#123880,#123881,#123882,
#123883,#123884,#123885,#123886,#123887,#123888,#123889,#123890,#123891,
#123892,#123893,#123894,#123895,#123896,#123897,#123898,#123899,#123900,
#123901,#123902,#123903,#123904,#123905,#123906,#123907,#123908,#123909,
#123910,#123911,#123912,#123913,#123914,#123915,#123916,#123917,#123918,
#123919,#123920,#123921,#123922,#123923,#123924,#123925,#123926,#123927,
#123928,#123929,#123930,#123931,#123932,#123933,#123934,#123935,#123936,
#123937,#123938,#123939,#123940,#123941,#123942,#123943,#123944,#123945,
#123946,#123947,#123948,#123949,#123950,#123951,#123952,#123953,#123954,
#123955,#123956,#123957,#123958,#123959,#123960,#123961,#123962,#123963,
#123964,#123965,#123966,#123967,#123968,#123969,#123970,#123971,#123972,
#123973,#123974,#123975,#123976,#123977,#123978,#123979,#123980),
 .UNSPECIFIED.,.F.,.F.,(4,2,2,2,2,2,2,2,2,2,2,2,2,2,2,2,2,2,2,2,2,2,2,2,
2,2,2,2,2,2,2,2,2,2,2,2,2,2,2,2,2,2,2,2,2,2,2,2,2,2,2,2,2,2,2,2,2,2,2,2,
2,2,2,2,2,2,2,2,2,2,2,2,2,2,2,2,2,2,2,2,2,2,2,2,2,2,2,2,2,2,2,2,2,2,2,2,
2,2,2,2,4),(-1.27782408552841,-1.27700744843732,-1.27585611518679,-1.27386152192946,
-1.26604387234503,-1.24155901253228,-1.22490854839876,-1.22139758046917,
-1.21934425388906,-1.21752803589453,-1.21524113476472,-1.21059333879667,
-1.18369148601385,-1.17001696913576,-1.1632285724226,-1.16139555307866,
-1.16027972848832,-1.15924827904952,-1.15799920069739,-1.15481245546084,
-1.13590214908377,-1.12404871419593,-1.10774680020317,-1.10425208402406,
-1.10220208188184,-1.10038506410701,-1.09809212763459,-1.09356964927776,
-1.06591623509627,-1.05271418884702,-1.04606509809328,-1.04424434984758,
-1.04313117127479,-1.04209849058864,-1.04084400231322,-1.03775008283869,
-1.01709280661423,-0.999424224147688,-0.992918543041473,-0.988030755869076,
-0.985698179287253,-0.983877162069481,-0.981851020003204,-0.978465928688977,
-0.965862976968039,-0.932911646393505,-0.929852129901944,-0.927490350469066,
-0.926260650127288,-0.925243244661346,-0.923958165246924,-0.921904712265766,
-0.907573653906144,-0.884583599093049,-0.873034819418677,-0.869732134957923,
-0.867723486857646,-0.865897800961454,-0.863530408941509,-0.858456908094493,
-0.851625094044048,-0.817300255843636,-0.811620743739196,-0.80983140096965,
-0.808724822179306,-0.807675113362555,-0.806155258474049,-0.802135746087605,
-0.775504484471682,-0.756552995034251,-0.75291093240851,-0.750807102714669,
-0.748994375106247,-0.746773669450533,-0.742467656594624,-0.727214627360076,
-0.703302196578544,-0.694910798872665,-0.692897308279438,-0.691729816029914,
-0.690704786917919,-0.689330380182545,-0.686208874600118,-0.671665160824926,
-0.645948757699798,-0.637840731634461,-0.63492588503852,-0.63319383827778,
-0.631358821769959,-0.628916565289571,-0.623416864518652,-0.59868497174726,
-0.579511699625379,-0.576640082361904,-0.57512701986566,-0.574089986632705,
-0.572985554076917,-0.57120470940897,-0.564984759893283,-0.553162204596557,
-0.536047533639214),.UNSPECIFIED.);
#1637=B_SPLINE_CURVE_WITH_KNOTS('',3,(#123983,#123984,#123985,#123986,#123987,
#123988,#123989,#123990,#123991,#123992,#123993,#123994,#123995,#123996,
#123997,#123998,#123999,#124000,#124001,#124002,#124003,#124004,#124005,
#124006,#124007,#124008,#124009,#124010,#124011,#124012,#124013,#124014,
#124015,#124016,#124017,#124018,#124019,#124020,#124021,#124022,#124023,
#124024,#124025,#124026,#124027,#124028,#124029,#124030,#124031,#124032,
#124033,#124034,#124035,#124036,#124037,#124038,#124039,#124040,#124041,
#124042,#124043,#124044,#124045,#124046,#124047,#124048,#124049,#124050,
#124051,#124052,#124053,#124054,#124055,#124056,#124057,#124058,#124059,
#124060,#124061,#124062,#124063,#124064,#124065,#124066,#124067,#124068,
#124069,#124070,#124071,#124072,#124073,#124074,#124075,#124076,#124077,
#124078,#124079,#124080,#124081,#124082,#124083,#124084,#124085,#124086,
#124087,#124088,#124089,#124090,#124091,#124092,#124093,#124094,#124095,
#124096,#124097,#124098,#124099,#124100,#124101,#124102,#124103,#124104,
#124105,#124106,#124107,#124108,#124109,#124110,#124111,#124112,#124113,
#124114,#124115,#124116,#124117,#124118,#124119,#124120,#124121,#124122,
#124123,#124124,#124125,#124126,#124127,#124128,#124129,#124130,#124131,
#124132,#124133,#124134,#124135,#124136,#124137,#124138,#124139,#124140,
#124141,#124142,#124143,#124144,#124145,#124146,#124147,#124148,#124149,
#124150,#124151,#124152,#124153,#124154,#124155,#124156,#124157,#124158,
#124159,#124160,#124161,#124162,#124163,#124164,#124165,#124166,#124167,
#124168,#124169,#124170,#124171,#124172),.UNSPECIFIED.,.F.,.F.,(4,2,2,2,
2,2,2,2,2,2,2,2,2,2,2,2,2,2,2,2,2,2,2,2,2,2,2,2,2,2,2,2,2,2,2,2,2,2,2,2,
2,2,2,2,2,2,2,2,2,2,2,2,2,2,2,2,2,2,2,2,2,2,2,2,2,2,2,2,2,2,2,2,2,2,2,2,
2,2,2,2,2,2,2,2,2,2,2,2,2,2,2,2,2,2,4),(-0.536047533639214,-0.52399885171329,
-0.5191418345236,-0.51681386044327,-0.51499206653414,-0.512960546072856,
-0.50955554956382,-0.494947057225457,-0.479827449156403,-0.474042924106341,
-0.460859879018046,-0.458631996800147,-0.457415386092451,-0.456393388474596,
-0.455083034564835,-0.452333245550669,-0.44861226264521,-0.438808977029807,
-0.415787915339652,-0.404424222966805,-0.401120959226698,-0.399108661379668,
-0.397277386413001,-0.394899360003346,-0.389788857269007,-0.382897753187339,
-0.347709148442755,-0.342751932427427,-0.341051268531925,-0.340071816487764,
-0.339035557306534,-0.337562497544506,-0.333805206831877,-0.32815082965446,
-0.307574270578932,-0.287646486813658,-0.284003445079414,-0.281908596678359,
-0.280109547254434,-0.277913384027072,-0.273681342470775,-0.268273073581708,
-0.255264360341712,-0.23694535907824,-0.226252973921614,-0.22411121235287,
-0.222918799531449,-0.221909562376785,-0.220589323919137,-0.21777493670625,
-0.213938499391572,-0.203655402571684,-0.180162614763938,-0.169322462829239,
-0.166079711731662,-0.164077142773677,-0.162236891490299,-0.159821276372025,
-0.154522453365636,-0.147292561345917,-0.125699525127139,-0.109176941674625,
-0.106895801112883,-0.105660587506475,-0.104645952324828,-0.104633561435904,
-0.104621312149598,-0.104609199094343,-0.104597217086387,-0.104585361125445,
-0.104573626424971,-0.104562008308446,-0.104550502282346,-0.104539104016455,
-0.104527809305687,-0.104516614067934,-0.104505514375394,-0.104494506409772,
-0.104483586458463,-0.104472750918138,-0.10446199632122,-0.104451319278702,
-0.103118243704271,-0.101561016763444,-0.098876620287455,-0.0929360043824338,
-0.0760446284376168,-0.0563580902694081,-0.0515877124908065,-0.0492537501845121,
-0.0474046239728219,-0.0453179671092674,-0.0417576343573112,-0.0249627090523748,
-9.99999997475243E-7),.UNSPECIFIED.);
#1638=B_SPLINE_CURVE_WITH_KNOTS('',3,(#124176,#124177,#124178,#124179,#124180,
#124181,#124182,#124183,#124184,#124185,#124186,#124187,#124188,#124189,
#124190,#124191,#124192,#124193,#124194,#124195,#124196,#124197,#124198,
#124199,#124200,#124201,#124202,#124203,#124204,#124205,#124206,#124207,
#124208,#124209,#124210,#124211,#124212,#124213,#124214,#124215,#124216,
#124217,#124218,#124219,#124220,#124221,#124222,#124223,#124224,#124225,
#124226,#124227,#124228,#124229,#124230,#124231,#124232,#124233),
 .UNSPECIFIED.,.F.,.F.,(4,2,2,2,2,2,2,2,2,2,2,2,2,2,2,2,2,2,2,2,2,2,2,2,
2,2,2,2,4),(5.15211709134537E-5,0.00655144725415278,0.00869323351133672,
0.0103519278912827,0.0119948184923338,0.0138623089950716,0.0168900595936218,
0.0269226222271582,0.0455925782724488,0.0661451986302976,0.0683674394977015,
0.0695297613193126,0.0705349598656515,0.0718094328174083,0.0738312522614602,
0.085736896500158,0.0932115525345353,0.111958373848329,0.127062062352944,
0.130865085822168,0.133119269195534,0.134933720040114,0.137408194121271,
0.142294210116158,0.162787875320058,0.181511848037067,0.184359249810965,
0.185542544508814,0.186520187542269),.UNSPECIFIED.);
#1639=B_SPLINE_CURVE_WITH_KNOTS('',3,(#124234,#124235,#124236,#124237,#124238,
#124239,#124240,#124241,#124242,#124243,#124244,#124245,#124246,#124247,
#124248,#124249,#124250,#124251,#124252,#124253,#124254,#124255,#124256,
#124257,#124258,#124259,#124260,#124261,#124262,#124263,#124264,#124265,
#124266,#124267,#124268,#124269,#124270,#124271,#124272,#124273,#124274,
#124275,#124276,#124277,#124278,#124279,#124280,#124281,#124282,#124283,
#124284,#124285,#124286,#124287,#124288,#124289,#124290,#124291,#124292,
#124293,#124294,#124295,#124296,#124297,#124298,#124299,#124300),
 .UNSPECIFIED.,.F.,.F.,(4,3,3,3,3,3,3,3,3,3,3,3,3,3,3,3,3,3,3,3,3,3,4),
(127.073099465779,127.192848546177,127.312825622574,127.406393326248,127.406438144991,
127.517358027634,127.530505230398,127.650260561131,127.769899548496,127.889474529566,
128.009037730339,128.128722920694,128.248481837206,128.358789105211,128.368455012374,
128.398921923044,128.398974828247,128.513022470957,128.530246689258,128.653089710286,
128.66777274281,128.79787167666,128.805298587658),.UNSPECIFIED.);
#1640=B_SPLINE_CURVE_WITH_KNOTS('',3,(#124303,#124304,#124305,#124306,#124307,
#124308,#124309,#124310,#124311,#124312,#124313,#124314,#124315,#124316,
#124317,#124318,#124319,#124320,#124321,#124322,#124323,#124324,#124325,
#124326,#124327,#124328,#124329,#124330,#124331,#124332,#124333,#124334,
#124335,#124336,#124337,#124338,#124339,#124340,#124341,#124342,#124343,
#124344,#124345,#124346,#124347,#124348,#124349,#124350,#124351,#124352,
#124353,#124354,#124355,#124356,#124357,#124358,#124359,#124360,#124361,
#124362,#124363,#124364,#124365,#124366,#124367,#124368,#124369,#124370,
#124371,#124372,#124373,#124374,#124375,#124376,#124377,#124378,#124379,
#124380,#124381,#124382,#124383,#124384,#124385,#124386,#124387,#124388,
#124389,#124390,#124391,#124392,#124393,#124394,#124395,#124396,#124397,
#124398,#124399,#124400,#124401,#124402,#124403,#124404,#124405,#124406,
#124407,#124408,#124409,#124410,#124411,#124412,#124413,#124414,#124415,
#124416,#124417,#124418,#124419,#124420,#124421,#124422,#124423,#124424,
#124425,#124426,#124427,#124428,#124429,#124430,#124431,#124432,#124433,
#124434,#124435,#124436,#124437,#124438,#124439,#124440,#124441,#124442,
#124443,#124444,#124445,#124446,#124447,#124448,#124449,#124450,#124451,
#124452,#124453,#124454,#124455,#124456,#124457,#124458,#124459,#124460,
#124461,#124462,#124463,#124464,#124465,#124466,#124467,#124468,#124469,
#124470,#124471,#124472,#124473,#124474,#124475,#124476,#124477,#124478,
#124479,#124480,#124481,#124482,#124483,#124484,#124485,#124486,#124487,
#124488,#124489,#124490,#124491,#124492,#124493,#124494,#124495,#124496,
#124497,#124498),.UNSPECIFIED.,.F.,.F.,(4,3,3,3,3,3,3,3,3,3,3,3,3,3,3,3,
3,3,3,3,3,3,3,3,3,3,3,3,3,3,3,3,3,3,3,3,3,3,3,3,3,3,3,3,3,3,3,3,3,3,3,3,
3,3,3,3,3,3,3,3,3,3,3,3,3,4),(114.220077335694,114.33434957594,114.446371905497,
114.558296674362,114.670170562004,114.786191735918,114.898176860493,115.010235018737,
115.11261136392,115.122481064781,115.134217102282,115.13425525766,115.238194100788,
115.247761589678,115.361066064117,115.474258346336,115.587383199224,115.700485285426,
115.81369072395,115.926947423793,116.040416912324,116.126754127008,116.126791940916,
116.230802571534,116.240305554226,116.353618126926,116.466818999181,116.579952912647,
116.693064509343,116.806280067485,116.919547240532,117.033027640638,117.119289858741,
117.119328624171,117.223112043074,117.232655671037,117.345780955494,117.458794234581,
117.571740577994,117.684664955273,117.79769531587,117.910778123356,118.024077818661,
118.111827279956,118.111865307427,118.215860201835,118.225558196699,118.339047810285,
118.452424216398,118.565731855983,118.679015068459,118.792397641909,118.905829519251,
119.019468834404,119.10436589177,119.104401990683,119.207910461063,119.217456662739,
119.329494590553,119.441426415126,119.553298846381,119.667183976568,119.779143127069,
119.893991247099,120.002398983502,120.00883936713),.UNSPECIFIED.);
#1641=B_SPLINE_CURVE_WITH_KNOTS('',3,(#124501,#124502,#124503,#124504,#124505,
#124506,#124507,#124508,#124509,#124510,#124511,#124512,#124513,#124514,
#124515,#124516,#124517,#124518,#124519,#124520,#124521,#124522,#124523,
#124524,#124525,#124526,#124527,#124528,#124529,#124530,#124531,#124532,
#124533,#124534,#124535,#124536,#124537,#124538,#124539,#124540,#124541,
#124542,#124543,#124544,#124545,#124546,#124547,#124548,#124549,#124550,
#124551,#124552,#124553,#124554,#124555,#124556,#124557,#124558,#124559,
#124560,#124561,#124562,#124563,#124564,#124565,#124566,#124567,#124568,
#124569,#124570,#124571,#124572,#124573,#124574,#124575,#124576,#124577,
#124578,#124579,#124580,#124581,#124582,#124583,#124584,#124585,#124586,
#124587,#124588,#124589,#124590,#124591,#124592,#124593,#124594,#124595,
#124596,#124597,#124598,#124599,#124600,#124601,#124602,#124603,#124604,
#124605,#124606,#124607,#124608,#124609,#124610,#124611,#124612,#124613,
#124614,#124615,#124616,#124617,#124618,#124619,#124620,#124621,#124622,
#124623,#124624,#124625,#124626,#124627,#124628,#124629,#124630,#124631,
#124632,#124633,#124634,#124635,#124636),.UNSPECIFIED.,.F.,.F.,(4,3,3,3,
3,3,3,3,3,3,3,3,3,3,3,3,3,3,3,3,3,3,3,3,3,3,3,3,3,3,3,3,3,3,3,3,3,3,3,3,
3,3,3,3,3,4),(-122.08201204045,-121.965917445828,-121.84987950632,-121.73386954936,
-121.617851459242,-121.501789119903,-121.38555131248,-121.269219443816,
-121.152648388576,-121.089475357194,-120.977120237893,-120.864991994256,
-120.752990586367,-120.641069346948,-120.529181735418,-120.417198453266,
-120.305170328657,-120.19292473749,-120.096938673939,-119.983292274015,
-119.869847663663,-119.756515326666,-119.64325077363,-119.53000961553,-119.416667246722,
-119.303274605463,-119.189672534295,-119.104401990683,-118.990730137739,
-118.877253694146,-118.763885635601,-118.650581534411,-118.537297058507,
-118.423905835679,-118.310461187396,-118.196802551937,-118.111865307427,
-117.996552974004,-117.884544281931,-117.772645207091,-117.660808992061,
-117.548988983923,-117.437070174475,-117.325090175962,-117.212929561234,
-117.189366640045),.UNSPECIFIED.);
#1642=B_SPLINE_CURVE_WITH_KNOTS('',3,(#124641,#124642,#124643,#124644,#124645,
#124646,#124647,#124648,#124649,#124650,#124651,#124652,#124653,#124654,
#124655,#124656,#124657,#124658,#124659,#124660,#124661,#124662,#124663,
#124664,#124665,#124666,#124667,#124668,#124669,#124670,#124671,#124672,
#124673,#124674,#124675,#124676,#124677,#124678,#124679,#124680,#124681,
#124682,#124683,#124684,#124685,#124686,#124687,#124688,#124689,#124690,
#124691,#124692,#124693,#124694,#124695,#124696,#124697,#124698,#124699,
#124700,#124701,#124702,#124703,#124704,#124705,#124706,#124707,#124708,
#124709,#124710,#124711,#124712,#124713,#124714,#124715,#124716,#124717,
#124718,#124719,#124720,#124721,#124722),.UNSPECIFIED.,.F.,.F.,(4,3,3,3,
3,3,3,3,3,3,3,3,3,3,3,3,3,3,3,3,3,3,3,3,3,3,3,4),(-0.272868023033693,-0.262502242400483,
-0.24527561767975,-0.237903293088585,-0.234230035432386,-0.217032391147809,
-0.20548949783366,-0.200475199976904,-0.197081245750112,-0.180328401578601,
-0.16398380749676,-0.154160166781224,-0.14719926789301,-0.144231535113113,
-0.128376931012345,-0.124689244634614,-0.108443690652105,-0.100974559826481,
-0.0956859974770197,-0.0926107843079526,-0.0768446513362621,-0.0611547177757335,
-0.05329672619646,-0.0475077033060932,-0.0447092358393594,-0.0296005801383283,
-0.0148002900691642,0.),.UNSPECIFIED.);
#1643=B_SPLINE_CURVE_WITH_KNOTS('',3,(#124723,#124724,#124725,#124726,#124727,
#124728,#124729,#124730,#124731,#124732,#124733,#124734,#124735,#124736),
 .UNSPECIFIED.,.F.,.F.,(4,2,2,2,2,2,4),(9.99999625904413E-7,0.0430920561884333,
0.0851072847416361,0.126567605991081,0.169373405344057,0.208996427770222,
0.24979679593988),.UNSPECIFIED.);
#1644=B_SPLINE_CURVE_WITH_KNOTS('',3,(#125242,#125243,#125244,#125245,#125246,
#125247),.UNSPECIFIED.,.F.,.F.,(4,2,4),(8.45004561326557E-5,0.00132119826430728,
0.00256099238825395),.UNSPECIFIED.);
#1645=B_SPLINE_CURVE_WITH_KNOTS('',3,(#125249,#125250,#125251,#125252,#125253,
#125254,#125255,#125256,#125257,#125258,#125259,#125260,#125261,#125262,
#125263,#125264,#125265,#125266,#125267,#125268,#125269,#125270,#125271,
#125272,#125273,#125274,#125275,#125276,#125277,#125278,#125279,#125280,
#125281,#125282,#125283,#125284,#125285,#125286,#125287,#125288,#125289,
#125290,#125291,#125292,#125293,#125294,#125295,#125296,#125297,#125298,
#125299,#125300,#125301,#125302,#125303,#125304,#125305,#125306,#125307,
#125308,#125309,#125310,#125311,#125312,#125313,#125314,#125315,#125316,
#125317,#125318,#125319,#125320,#125321,#125322,#125323,#125324,#125325,
#125326,#125327,#125328,#125329,#125330,#125331,#125332,#125333),
 .UNSPECIFIED.,.F.,.F.,(4,3,3,3,3,3,3,3,3,3,3,3,3,3,3,3,3,3,3,3,3,3,3,3,
3,3,3,3,4),(-0.276631791712731,-0.266078274757453,-0.25142944697914,-0.244605027091712,
-0.241150782754899,-0.225852149777011,-0.215097155747404,-0.211769086231776,
-0.208422910451095,-0.192472307416272,-0.176609029381956,-0.16739153228391,
-0.162510949576809,-0.159609420310082,-0.143083140167058,-0.139739040989771,
-0.123776906696283,-0.115962699697761,-0.111035505377364,-0.107829669889836,
-0.0911010363506398,-0.0743724028114436,-0.0648654694233928,-0.0586676892110244,
-0.0555403299923495,-0.0380585004240356,-0.020721803007727,-0.00352182003484276,
0.),.UNSPECIFIED.);
#1646=B_SPLINE_CURVE_WITH_KNOTS('',3,(#125334,#125335,#125336,#125337),
 .UNSPECIFIED.,.F.,.F.,(4,4),(-0.0121033717511618,0.),.UNSPECIFIED.);
#1647=B_SPLINE_CURVE_WITH_KNOTS('',3,(#125342,#125343,#125344,#125345,#125346,
#125347,#125348,#125349,#125350,#125351,#125352,#125353,#125354,#125355,
#125356,#125357,#125358,#125359,#125360,#125361,#125362,#125363,#125364,
#125365,#125366,#125367,#125368,#125369,#125370,#125371,#125372,#125373,
#125374,#125375,#125376,#125377,#125378,#125379,#125380,#125381,#125382,
#125383,#125384,#125385,#125386,#125387,#125388,#125389,#125390,#125391,
#125392,#125393,#125394,#125395,#125396,#125397,#125398,#125399,#125400,
#125401,#125402,#125403,#125404,#125405,#125406,#125407,#125408,#125409,
#125410,#125411,#125412,#125413,#125414,#125415,#125416,#125417,#125418,
#125419,#125420,#125421,#125422,#125423),.UNSPECIFIED.,.F.,.F.,(4,3,3,3,
3,3,3,3,3,3,3,3,3,3,3,3,3,3,3,3,3,3,3,3,3,3,3,4),(-0.272867943863341,-0.262502242400497,
-0.245275617679762,-0.237903297370454,-0.234230038512527,-0.21703119377903,
-0.205489500611459,-0.200475208558893,-0.19708124562454,-0.180335625911279,
-0.163965603178691,-0.154160171865287,-0.14719928547427,-0.144231543166927,
-0.128376945114741,-0.124689244634617,-0.108477769606106,-0.100974564290966,
-0.0956859981647498,-0.0926107839869569,-0.0768294319563884,-0.0611547141438257,
-0.0532967250836255,-0.0475076998648919,-0.0447092326529874,-0.0296829840600132,
-0.0148414920300066,0.),.UNSPECIFIED.);
#1648=B_SPLINE_CURVE_WITH_KNOTS('',3,(#125929,#125930,#125931,#125932,#125933,
#125934),.UNSPECIFIED.,.F.,.F.,(4,2,4),(-0.00251068061179639,-0.00126056420704893,
-1.00000002448055E-6),.UNSPECIFIED.);
#1649=B_SPLINE_CURVE_WITH_KNOTS('',3,(#126911,#126912,#126913,#126914,#126915,
#126916,#126917,#126918,#126919,#126920,#126921,#126922,#126923,#126924,
#126925,#126926,#126927,#126928,#126929,#126930,#126931,#126932,#126933,
#126934,#126935,#126936,#126937,#126938,#126939,#126940,#126941,#126942,
#126943,#126944,#126945,#126946,#126947,#126948,#126949,#126950,#126951,
#126952,#126953,#126954,#126955,#126956,#126957,#126958,#126959,#126960,
#126961,#126962),.UNSPECIFIED.,.F.,.F.,(4,3,3,3,3,3,3,3,3,3,3,3,3,3,3,3,
3,4),(-4.09157007060746,-4.04267459647314,-3.91804643852106,-3.79360664990601,
-3.66929160873361,-3.54503793099914,-3.42067389293025,-3.29626244717563,
-3.17156478702648,-3.05406931124741,-2.92480942306547,-2.79577237913115,
-2.66690816470504,-2.53816707784842,-2.40945958659725,-2.28078154682162,
-2.15200653753529,-2.0654640260217),.UNSPECIFIED.);
#1650=B_SPLINE_CURVE_WITH_KNOTS('',3,(#126965,#126966,#126967,#126968,#126969,
#126970,#126971,#126972,#126973,#126974,#126975,#126976,#126977,#126978,
#126979,#126980,#126981,#126982,#126983,#126984,#126985,#126986,#126987,
#126988,#126989,#126990,#126991,#126992),.UNSPECIFIED.,.F.,.F.,(4,3,3,3,
3,3,3,3,3,4),(0.,0.128770504077986,0.257463953946973,0.386129758592228,
0.514817261654237,0.643692750510219,0.772663027875016,0.901926079013672,
0.989884320813703,1.11548660900397),.UNSPECIFIED.);
#1651=B_SPLINE_CURVE_WITH_KNOTS('',3,(#126997,#126998,#126999,#127000,#127001,
#127002,#127003,#127004,#127005,#127006,#127007,#127008,#127009,#127010,
#127011,#127012,#127013,#127014,#127015,#127016,#127017,#127018,#127019,
#127020,#127021,#127022,#127023,#127024,#127025,#127026,#127027,#127028,
#127029,#127030,#127031,#127032,#127033,#127034,#127035,#127036,#127037,
#127038,#127039,#127040,#127041,#127042,#127043,#127044,#127045,#127046,
#127047,#127048,#127049,#127050,#127051,#127052,#127053,#127054,#127055,
#127056,#127057,#127058,#127059,#127060,#127061,#127062,#127063,#127064,
#127065,#127066,#127067,#127068,#127069,#127070,#127071,#127072,#127073,
#127074,#127075,#127076,#127077,#127078,#127079,#127080,#127081,#127082,
#127083,#127084,#127085,#127086,#127087,#127088,#127089,#127090,#127091,
#127092,#127093,#127094,#127095,#127096,#127097,#127098,#127099,#127100,
#127101,#127102,#127103,#127104,#127105,#127106,#127107,#127108,#127109,
#127110,#127111,#127112,#127113,#127114,#127115,#127116,#127117,#127118,
#127119,#127120,#127121,#127122,#127123,#127124,#127125,#127126,#127127,
#127128,#127129,#127130,#127131,#127132,#127133,#127134,#127135,#127136,
#127137,#127138,#127139,#127140,#127141,#127142,#127143,#127144,#127145,
#127146,#127147,#127148,#127149,#127150,#127151,#127152,#127153,#127154,
#127155,#127156,#127157,#127158,#127159,#127160,#127161,#127162,#127163,
#127164,#127165,#127166,#127167,#127168,#127169,#127170,#127171,#127172,
#127173,#127174,#127175,#127176,#127177,#127178,#127179,#127180,#127181,
#127182,#127183,#127184,#127185,#127186,#127187,#127188,#127189),
 .UNSPECIFIED.,.F.,.F.,(4,3,3,3,3,3,3,3,3,3,3,3,3,3,3,3,3,3,3,3,3,3,3,3,
3,3,3,3,3,3,3,3,3,3,3,3,3,3,3,3,3,3,3,3,3,3,3,3,3,3,3,3,3,3,3,3,3,3,3,3,
3,3,3,3,4),(-10.3747553770227,-10.2366360171358,-10.1065918341442,-10.097621507011,
-9.97435184766567,-9.97430630782751,-9.85805755748757,-9.84843734717473,
-9.72275709682591,-9.59720432091665,-9.47171800663457,-9.34614035145364,
-9.22052340584574,-9.09465137971492,-8.98574649523054,-8.98570102260178,
-8.86943094769939,-8.85978588593879,-8.73405959725147,-8.60846101885127,
-8.48292923617449,-8.35730705327952,-8.23164602820857,-8.10573130030452,
-7.9971408564736,-7.99709573737606,-7.88075327220879,-7.87117390366413,
-7.74544034467922,-7.61983394815419,-7.49429382402376,-7.36866257916642,
-7.24299208158905,-7.11706734697963,-7.00853658425701,-7.00849045215032,
-6.89238358877969,-6.88275794584282,-6.75721440838983,-6.63179830794794,
-6.50644833672224,-6.38100523841909,-6.25552208387502,-6.12978064259321,
-6.0199304705395,-6.0198851669246,-5.90354891647336,-5.89377144736946,-5.7678473942784,
-5.64205230085332,-5.51632568434797,-5.39051310093208,-5.26466383335606,
-5.13856714447721,-5.03132314697593,-5.03127988169887,-4.91519179536761,
-4.90623388686583,-4.78137263497701,-4.65663321639741,-4.53195294699382,
-4.40718096255982,-4.28235977243278,-4.15730670558814,-4.09157124239226),
 .UNSPECIFIED.);
#1652=B_SPLINE_CURVE_WITH_KNOTS('',3,(#127190,#127191,#127192,#127193,#127194,
#127195,#127196,#127197,#127198,#127199,#127200,#127201,#127202,#127203,
#127204,#127205,#127206,#127207,#127208,#127209,#127210,#127211,#127212,
#127213,#127214,#127215,#127216,#127217,#127218,#127219,#127220,#127221,
#127222,#127223,#127224,#127225,#127226,#127227,#127228,#127229,#127230,
#127231,#127232,#127233,#127234,#127235,#127236,#127237,#127238,#127239,
#127240,#127241,#127242,#127243,#127244,#127245,#127246,#127247,#127248,
#127249,#127250,#127251,#127252,#127253,#127254,#127255,#127256,#127257,
#127258,#127259,#127260,#127261,#127262,#127263,#127264,#127265,#127266,
#127267,#127268,#127269,#127270,#127271,#127272,#127273,#127274,#127275,
#127276,#127277,#127278,#127279,#127280,#127281,#127282,#127283,#127284,
#127285,#127286,#127287,#127288,#127289,#127290,#127291,#127292,#127293,
#127294,#127295,#127296,#127297,#127298,#127299,#127300,#127301,#127302,
#127303,#127304,#127305,#127306,#127307,#127308,#127309,#127310,#127311,
#127312,#127313,#127314,#127315,#127316,#127317,#127318,#127319,#127320,
#127321,#127322,#127323,#127324,#127325,#127326,#127327,#127328,#127329,
#127330,#127331,#127332,#127333,#127334,#127335,#127336,#127337,#127338,
#127339,#127340,#127341,#127342,#127343,#127344,#127345,#127346,#127347,
#127348,#127349,#127350,#127351,#127352,#127353,#127354,#127355,#127356,
#127357,#127358,#127359,#127360,#127361,#127362,#127363,#127364,#127365),
 .UNSPECIFIED.,.F.,.F.,(4,2,2,2,2,2,2,2,2,2,2,2,2,2,2,2,2,2,2,2,2,2,2,2,
2,2,2,2,2,2,2,2,2,2,2,2,2,2,2,2,2,2,2,2,2,2,2,2,2,2,2,2,2,2,2,2,2,2,2,2,
2,2,2,2,2,2,2,2,2,2,2,2,2,2,2,2,2,2,2,2,2,2,2,2,2,2,2,4),(0.000261646384316517,
0.0104924062465661,0.0260785968740954,0.0314686564231903,0.0343533113436317,
0.0368068389339,0.039813369304345,0.0456471493868944,0.0699359697100838,
0.0772288638425005,0.0818877276898668,0.0837832704086861,0.0851993880928992,
0.0869287609772795,0.0901709616532053,0.103770211934126,0.118549793829608,
0.127379387968971,0.130950725410799,0.133610817884919,0.136496694037172,
0.141284992766288,0.157275839707537,0.169927706991005,0.176474951605186,
0.17871844945781,0.180248987572319,0.181937634491626,0.185026125922963,
0.201953413384733,0.220518120216993,0.224785518830655,0.227548278686829,
0.230193218108385,0.233974595353628,0.244051689035776,0.245270298020942,
0.261852191084533,0.271911101446268,0.274414412264434,0.275971457591503,
0.277527655559406,0.280058748146808,0.290002469312615,0.308293612311992,
0.31803591741021,0.321673273167989,0.324297130762851,0.327062674753666,
0.331451761887082,0.354460658499812,0.363540349683242,0.368942050663461,
0.37100398708861,0.372474576449311,0.374186823311687,0.377347332450581,
0.391965672135443,0.406001920509121,0.414545700221812,0.41805035590891,
0.420672662087154,0.423526323958717,0.42827248989015,0.448032783400729,
0.462974579000867,0.465956762587759,0.467617303251053,0.469100891045124,
0.471297103908426,0.477206238672996,0.499268651330173,0.509763136066544,
0.513498286254066,0.516152580317041,0.518916554069543,0.523233147159251,
0.546707891920172,0.5555022822345,0.560801060174836,0.562857398999995,0.564332349502359,
0.566055861942539,0.569275343848298,0.582354352730892,0.594203837528408,
0.605560438582849,0.609378420130365),.UNSPECIFIED.);
#1653=B_SPLINE_CURVE_WITH_KNOTS('',3,(#127370,#127371,#127372,#127373,#127374,
#127375,#127376,#127377,#127378,#127379,#127380,#127381,#127382,#127383,
#127384,#127385,#127386,#127387,#127388,#127389,#127390,#127391,#127392,
#127393,#127394,#127395,#127396,#127397,#127398,#127399,#127400,#127401,
#127402,#127403,#127404,#127405,#127406,#127407,#127408,#127409,#127410,
#127411,#127412,#127413,#127414,#127415,#127416,#127417,#127418,#127419,
#127420,#127421,#127422,#127423,#127424,#127425,#127426,#127427,#127428,
#127429,#127430,#127431,#127432,#127433,#127434,#127435,#127436,#127437,
#127438,#127439,#127440,#127441,#127442,#127443,#127444,#127445,#127446,
#127447,#127448,#127449,#127450,#127451,#127452,#127453,#127454,#127455,
#127456,#127457,#127458,#127459,#127460,#127461,#127462,#127463,#127464,
#127465,#127466,#127467,#127468,#127469,#127470,#127471,#127472,#127473,
#127474,#127475,#127476,#127477,#127478,#127479,#127480,#127481,#127482,
#127483,#127484,#127485,#127486,#127487,#127488,#127489,#127490,#127491,
#127492,#127493,#127494,#127495,#127496,#127497,#127498,#127499,#127500,
#127501,#127502,#127503,#127504,#127505,#127506,#127507,#127508,#127509,
#127510,#127511,#127512,#127513,#127514,#127515,#127516,#127517,#127518,
#127519,#127520,#127521,#127522,#127523,#127524,#127525,#127526,#127527,
#127528,#127529,#127530,#127531,#127532,#127533,#127534,#127535,#127536,
#127537,#127538,#127539,#127540,#127541,#127542,#127543,#127544,#127545,
#127546,#127547,#127548,#127549,#127550,#127551),.UNSPECIFIED.,.F.,.F.,
(4,2,2,2,2,2,2,2,2,2,2,2,2,2,2,2,2,2,2,2,2,2,2,2,2,2,2,2,2,2,2,2,2,2,2,
2,2,2,2,2,2,2,2,2,2,2,2,2,2,2,2,2,2,2,2,2,2,2,2,2,2,2,2,2,2,2,2,2,2,2,2,
2,2,2,2,2,2,2,2,2,2,2,2,2,2,2,2,2,2,2,4),(0.609195619805639,0.625836591744223,
0.630724530933535,0.633663812077152,0.636369805467325,0.640000451724975,
0.649019629401262,0.664447742241405,0.676787354309999,0.680005585928994,
0.681762653288162,0.683296445509315,0.685489354608689,0.691518502334891,
0.702306140883459,0.721763852827824,0.726595122380225,0.729523082525254,
0.732232962020334,0.735890994775529,0.745123409561988,0.761279856723455,
0.773672716489257,0.77633483124701,0.777957126369306,0.779564627000971,
0.782156874269418,0.793050204386433,0.818300652538408,0.822773432172227,
0.825629936986889,0.828373004224322,0.832241027854228,0.843353789820006,
0.855520513510064,0.868397105928568,0.871641143390267,0.873403587583718,
0.874935820666734,0.877117908059764,0.883061100411173,0.893587699113478,
0.913469840618771,0.918270373770518,0.921192159859008,0.923904250351927,
0.927577684486519,0.936933185417741,0.950676183130047,0.965226615234117,
0.967935362305547,0.969567488647443,0.971165872655077,0.973715185559099,
0.983803321260223,0.998853179383179,1.01078026119092,1.01484334543049,1.01734359536002,
1.02010113950087,1.02405357629441,1.03609574529333,1.05440800406234,1.06167553801317,
1.06406534882108,1.06561660540468,1.06728797508272,1.07018324501945,1.0738730609813,
1.08266770840829,1.10591969986608,1.11030869246259,1.11314860394664,1.11590197609641,
1.11983028820028,1.13159375606052,1.14334493874623,1.15587132646578,1.15909683180329,
1.16085540183652,1.16238927915248,1.16458041464355,1.17059173982159,1.18132582692828,
1.18815902010274,1.20225533145114,1.20637803713945,1.20888907459917,1.21142899558228,
1.21454154335485,1.21829292486733),.UNSPECIFIED.);
#1654=B_SPLINE_CURVE_WITH_KNOTS('',3,(#127552,#127553,#127554,#127555,#127556,
#127557,#127558,#127559,#127560,#127561,#127562,#127563,#127564,#127565,
#127566,#127567,#127568,#127569,#127570,#127571,#127572,#127573,#127574,
#127575,#127576,#127577,#127578,#127579,#127580,#127581,#127582,#127583,
#127584,#127585,#127586,#127587,#127588,#127589,#127590,#127591,#127592,
#127593,#127594,#127595,#127596,#127597,#127598,#127599,#127600,#127601,
#127602,#127603,#127604,#127605,#127606,#127607,#127608,#127609,#127610,
#127611,#127612,#127613,#127614,#127615,#127616,#127617,#127618,#127619,
#127620,#127621,#127622,#127623,#127624,#127625,#127626,#127627,#127628,
#127629,#127630,#127631,#127632,#127633,#127634,#127635,#127636,#127637,
#127638,#127639,#127640,#127641,#127642,#127643,#127644,#127645,#127646,
#127647,#127648,#127649,#127650,#127651,#127652,#127653,#127654,#127655,
#127656,#127657,#127658,#127659,#127660,#127661,#127662,#127663,#127664,
#127665,#127666,#127667,#127668,#127669,#127670,#127671,#127672,#127673,
#127674,#127675,#127676,#127677,#127678,#127679,#127680,#127681,#127682,
#127683,#127684,#127685,#127686,#127687,#127688,#127689,#127690,#127691,
#127692,#127693,#127694,#127695,#127696,#127697,#127698,#127699,#127700,
#127701,#127702,#127703,#127704,#127705,#127706,#127707,#127708,#127709,
#127710,#127711,#127712,#127713,#127714,#127715,#127716,#127717,#127718,
#127719,#127720,#127721,#127722,#127723,#127724,#127725,#127726,#127727),
 .UNSPECIFIED.,.F.,.F.,(4,2,2,2,2,2,2,2,2,2,2,2,2,2,2,2,2,2,2,2,2,2,2,2,
2,2,2,2,2,2,2,2,2,2,2,2,2,2,2,2,2,2,2,2,2,2,2,2,2,2,2,2,2,2,2,2,2,2,2,2,
2,2,2,2,2,2,2,2,2,2,2,2,2,2,2,2,2,2,2,2,2,2,2,2,2,2,2,4),(0.609378420130365,
0.612018261019042,0.614749532539526,0.618912068663256,0.636505046351328,
0.65494406438821,0.657910724626156,0.659563280054749,0.661060644757464,
0.663265236923216,0.669740261678691,0.682089605334379,0.699480950387193,
0.704309301736647,0.707176017406193,0.709787490275448,0.713242974764558,
0.72146460941387,0.734601179923452,0.750546235794313,0.753668305013858,
0.755372632290222,0.756853898894493,0.758951506429721,0.764551085502066,
0.774164185389945,0.795931707416114,0.800483792711178,0.803294285009617,
0.80592385165699,0.80951130973408,0.818725931862822,0.833852378769016,0.846389382724306,
0.849576729273647,0.851294237547501,0.852771318082724,0.854841262120309,
0.860237659074661,0.86929352202869,0.892195415241358,0.896592589213518,
0.899371750568979,0.902015529817111,0.905693754047723,0.915674529561137,
0.934989613237843,0.943714825136999,0.946183102048811,0.94757844128154,
0.949109895292506,0.951495967565137,0.959876597557263,0.981786870823796,
0.990051400722908,0.993239578710188,0.99587603083011,0.9986181447563,1.00282732834149,
1.02167459701192,1.03853736295692,1.04158991940377,1.04327888819084,1.04476389158991,
1.04688982785566,1.05270942557411,1.06295651185913,1.08354366128914,1.08823160115648,
1.09106936404024,1.09368842933782,1.09720558872425,1.1058787280598,1.12032334244059,
1.13427287713437,1.13744942777678,1.1391647027966,1.14064244752089,1.14271684560393,
1.14814511063743,1.1572866691416,1.18000809371754,1.18443110260207,1.18721558580083,
1.18985695499119,1.19351949368841,1.19766710350325,1.21853221181177),
 .UNSPECIFIED.);
#1655=B_SPLINE_CURVE_WITH_KNOTS('',3,(#127732,#127733,#127734,#127735,#127736,
#127737,#127738,#127739,#127740,#127741,#127742,#127743,#127744,#127745,
#127746,#127747,#127748,#127749,#127750,#127751,#127752,#127753,#127754,
#127755,#127756,#127757,#127758,#127759,#127760,#127761,#127762,#127763,
#127764,#127765,#127766,#127767,#127768,#127769,#127770,#127771,#127772,
#127773,#127774,#127775,#127776,#127777,#127778,#127779,#127780,#127781,
#127782,#127783,#127784,#127785,#127786,#127787,#127788,#127789,#127790,
#127791,#127792,#127793,#127794,#127795,#127796,#127797,#127798,#127799,
#127800,#127801,#127802,#127803,#127804,#127805,#127806,#127807,#127808,
#127809,#127810,#127811,#127812,#127813,#127814,#127815,#127816,#127817,
#127818,#127819,#127820,#127821,#127822,#127823,#127824,#127825,#127826,
#127827,#127828,#127829,#127830,#127831,#127832,#127833,#127834,#127835,
#127836,#127837,#127838,#127839,#127840,#127841,#127842,#127843,#127844,
#127845,#127846,#127847,#127848,#127849,#127850,#127851,#127852,#127853,
#127854,#127855,#127856,#127857,#127858,#127859,#127860,#127861,#127862,
#127863,#127864,#127865,#127866,#127867,#127868,#127869,#127870,#127871,
#127872,#127873,#127874,#127875,#127876,#127877,#127878,#127879,#127880,
#127881,#127882,#127883,#127884,#127885,#127886,#127887,#127888,#127889,
#127890,#127891,#127892,#127893,#127894,#127895,#127896,#127897,#127898,
#127899,#127900,#127901,#127902,#127903,#127904,#127905,#127906,#127907,
#127908,#127909,#127910,#127911),.UNSPECIFIED.,.F.,.F.,(4,2,2,2,2,2,2,2,
2,2,2,2,2,2,2,2,2,2,2,2,2,2,2,2,2,2,2,2,2,2,2,2,2,2,2,2,2,2,2,2,2,2,2,2,
2,2,2,2,2,2,2,2,2,2,2,2,2,2,2,2,2,2,2,2,2,2,2,2,2,2,2,2,2,2,2,2,2,2,2,2,
2,2,2,2,2,2,2,2,2,4),(0.000273487393315781,0.00668233346743799,0.00878609781692979,
0.0103134599133232,0.0117975148680287,0.0135777641845307,0.0169067857893203,
0.0328729072272741,0.0429255957088579,0.053160566460337,0.0569373680766626,
0.0596652430555349,0.0625495357509145,0.0671628630974127,0.0887819817328903,
0.101670084334189,0.104999883847082,0.106760479612903,0.108293146614009,
0.110478679342832,0.116039509789547,0.134351598502859,0.143681644379522,
0.150343388885038,0.153616877504323,0.15602876636482,0.159081955031285,
0.16439949414022,0.186476116936597,0.197789695721472,0.200945388483554,
0.202670896217642,0.204215149808471,0.206113165149188,0.21099136274985,
0.23403270957221,0.244710670866626,0.248535132571594,0.251270903461355,
0.254140288972433,0.258678092552839,0.280869681227153,0.29340072818385,
0.296692921680029,0.298446052454859,0.299980974008835,0.30218176067146,
0.307838946549081,0.324246377305529,0.334620885239953,0.341766160368095,
0.345121457282295,0.34777266769147,0.350854357541875,0.356310502244138,
0.381933264092872,0.390755454099656,0.393221589200865,0.394803403819953,
0.396250867000954,0.39883513326232,0.408673790254529,0.426868100434012,
0.436631947879639,0.440355252498272,0.443074997540403,0.44597830587298,
0.450685673024221,0.471527379754759,0.481503349307649,0.485473236366192,
0.488532010842608,0.490237701450933,0.491772503840068,0.494067898864919,
0.500448675418648,0.517953107030139,0.531646616867548,0.535722368892298,
0.538502798460077,0.541309275474993,0.545523490887629,0.561305512379495,
0.575700119524876,0.582747278133253,0.585056256017955,0.586608656824652,
0.588314878278613,0.591376326626021,0.609195619805639),.UNSPECIFIED.);
#1656=B_SPLINE_CURVE_WITH_KNOTS('',3,(#127912,#127913,#127914,#127915,#127916,
#127917,#127918,#127919,#127920,#127921,#127922,#127923,#127924,#127925,
#127926,#127927,#127928,#127929,#127930,#127931,#127932,#127933,#127934,
#127935,#127936,#127937,#127938,#127939,#127940,#127941,#127942,#127943,
#127944,#127945,#127946,#127947,#127948,#127949,#127950,#127951,#127952,
#127953,#127954,#127955,#127956,#127957,#127958,#127959,#127960,#127961,
#127962,#127963,#127964,#127965,#127966,#127967,#127968,#127969,#127970,
#127971,#127972,#127973,#127974,#127975,#127976,#127977,#127978,#127979,
#127980,#127981,#127982,#127983,#127984,#127985,#127986,#127987,#127988,
#127989,#127990,#127991,#127992,#127993,#127994,#127995,#127996,#127997,
#127998,#127999,#128000,#128001,#128002,#128003,#128004,#128005,#128006,
#128007,#128008,#128009,#128010,#128011,#128012,#128013,#128014,#128015,
#128016,#128017,#128018,#128019,#128020,#128021,#128022,#128023,#128024,
#128025,#128026,#128027,#128028,#128029,#128030,#128031,#128032,#128033,
#128034,#128035,#128036,#128037,#128038,#128039,#128040,#128041,#128042,
#128043,#128044,#128045,#128046,#128047,#128048,#128049,#128050,#128051,
#128052,#128053,#128054,#128055,#128056,#128057,#128058,#128059,#128060,
#128061,#128062,#128063,#128064,#128065,#128066,#128067,#128068,#128069,
#128070,#128071,#128072,#128073,#128074,#128075,#128076,#128077,#128078,
#128079,#128080,#128081,#128082,#128083,#128084,#128085,#128086,#128087,
#128088,#128089,#128090,#128091,#128092,#128093,#128094,#128095,#128096,
#128097,#128098,#128099),.UNSPECIFIED.,.F.,.F.,(4,2,2,2,2,2,2,2,2,2,2,2,
2,2,2,2,2,2,2,2,2,2,2,2,2,2,2,2,2,2,2,2,2,2,2,2,2,2,2,2,2,2,2,2,2,2,2,2,
2,2,2,2,2,2,2,2,2,2,2,2,2,2,2,2,2,2,2,2,2,2,2,2,2,2,2,2,2,2,2,2,2,2,2,2,
2,2,2,2,2,2,2,2,2,4),(5.28102015283622E-5,0.00943930468759837,0.0136584492307033,
0.015350078067837,0.016722480911901,0.0182094940979389,0.0200110829088309,
0.024481371733638,0.0415374280043719,0.0566370430245147,0.0573842064374152,
0.0588664171978575,0.0590581142496318,0.0627484768252054,0.0653944205673456,
0.0681701130928783,0.0725493070509845,0.0955555996973102,0.104549675921614,
0.109923152915613,0.111989992268153,0.113466774101365,0.115186208271291,
0.118382598729794,0.131101908410891,0.142486572219041,0.154560154990933,
0.158443034388585,0.161122777535872,0.163847727456843,0.16796965475202,
0.18356756801777,0.195266214822312,0.204966827504056,0.207445173091656,
0.208995498356967,0.210565679766474,0.213137768772695,0.22391462815933,
0.241502950806235,0.248020485280757,0.253162610366718,0.256091017966324,
0.258687209439581,0.26202081568506,0.269433422636807,0.29255360431755,0.301080861792751,
0.303478172252538,0.305011843272254,0.306602299809132,0.30926959749595,
0.323933588846315,0.33772529688717,0.347094881854784,0.350701445715302,
0.353333829207641,0.356137147819951,0.360654259109438,0.382671153379249,
0.392146790415539,0.39769701183653,0.399787776390432,0.401267701438489,
0.402974118293782,0.406108992539898,0.421411792528695,0.434990439825889,
0.443370045702156,0.446847013982485,0.449460369231819,0.452315181419452,
0.457088513067437,0.484034309722774,0.49293939660373,0.495364979368958,
0.496904460196579,0.498292439523088,0.500720829281657,0.508895055080013,
0.528724418268833,0.538814464662127,0.542505308417374,0.545151401306737,
0.547594734661768,0.551661442879315,0.565353561274739,0.579655298254744,
0.588843029197885,0.591288270136979,0.592831733882104,0.594409860179039,
0.597019166477871,0.608918989341705),.UNSPECIFIED.);
#1657=B_SPLINE_CURVE_WITH_KNOTS('',3,(#128104,#128105,#128106,#128107,#128108,
#128109,#128110,#128111,#128112,#128113,#128114,#128115,#128116,#128117,
#128118,#128119,#128120,#128121,#128122,#128123,#128124,#128125,#128126,
#128127,#128128,#128129,#128130,#128131,#128132,#128133,#128134,#128135,
#128136,#128137,#128138,#128139,#128140,#128141,#128142,#128143,#128144,
#128145,#128146,#128147,#128148,#128149,#128150,#128151,#128152,#128153,
#128154,#128155,#128156,#128157,#128158,#128159,#128160,#128161,#128162,
#128163,#128164,#128165,#128166,#128167,#128168,#128169,#128170,#128171,
#128172,#128173,#128174,#128175,#128176,#128177,#128178,#128179,#128180,
#128181,#128182,#128183,#128184,#128185,#128186,#128187,#128188,#128189,
#128190,#128191,#128192,#128193,#128194,#128195,#128196,#128197,#128198,
#128199,#128200,#128201,#128202,#128203,#128204,#128205,#128206,#128207,
#128208,#128209,#128210,#128211,#128212,#128213,#128214,#128215,#128216,
#128217,#128218,#128219,#128220,#128221,#128222,#128223,#128224,#128225,
#128226,#128227,#128228,#128229,#128230,#128231,#128232,#128233,#128234,
#128235,#128236,#128237,#128238,#128239,#128240,#128241,#128242,#128243,
#128244,#128245,#128246,#128247,#128248,#128249,#128250,#128251,#128252,
#128253,#128254,#128255,#128256,#128257),.UNSPECIFIED.,.F.,.F.,(4,3,3,3,
3,3,3,3,3,3,3,3,3,3,3,3,3,3,3,3,3,3,3,3,3,3,3,3,3,3,3,3,3,3,3,3,3,3,3,3,
3,3,3,3,3,3,3,3,3,3,3,4),(-29.2243093234641,-29.0911455076753,-28.9577015471726,
-28.823781010616,-28.7578067271164,-28.6319159028052,-28.5062137687136,
-28.3806391369115,-28.2551310424176,-28.129531928478,-28.0038936673963,
-27.8780008716122,-27.7692014418906,-27.6433106177164,-27.5176084837613,
-27.3920338520949,-27.2665257577356,-27.1409266439278,-27.0152883829764,
-26.8893955873186,-26.7805961566649,-26.6547053325348,-26.5290031986255,
-26.4034285670066,-26.2779204726964,-26.1523213589396,-26.0266830980403,
-25.9007903024356,-25.7919908714392,-25.6661000466945,-25.5403979121686,
-25.4148232799325,-25.2893151850059,-25.1637160706394,-25.0380778091335,
-24.9121850129357,-24.8033855862134,-24.6774947626185,-24.5517926292399,
-24.4262179981462,-24.3007099043544,-24.1751107911009,-24.0494725306974,
-23.9235797355689,-23.8147803009877,-23.6905595755302,-23.566526324309,
-23.4426162002402,-23.3172456242379,-23.1933193126604,-23.0672266044457,
-22.941133896231),.UNSPECIFIED.);
#1658=B_SPLINE_CURVE_WITH_KNOTS('',3,(#128258,#128259,#128260,#128261,#128262,
#128263,#128264,#128265,#128266,#128267,#128268,#128269,#128270,#128271,
#128272,#128273,#128274,#128275,#128276,#128277,#128278,#128279,#128280,
#128281,#128282,#128283,#128284,#128285,#128286,#128287,#128288,#128289,
#128290,#128291,#128292,#128293,#128294,#128295,#128296,#128297,#128298,
#128299,#128300,#128301,#128302,#128303,#128304,#128305,#128306,#128307,
#128308,#128309,#128310,#128311,#128312,#128313,#128314,#128315,#128316,
#128317,#128318,#128319,#128320,#128321,#128322,#128323,#128324,#128325,
#128326,#128327,#128328,#128329,#128330,#128331,#128332,#128333,#128334,
#128335,#128336,#128337,#128338,#128339,#128340,#128341,#128342,#128343,
#128344,#128345,#128346,#128347,#128348,#128349,#128350,#128351,#128352,
#128353,#128354,#128355,#128356,#128357,#128358,#128359,#128360,#128361,
#128362,#128363,#128364,#128365,#128366,#128367,#128368,#128369,#128370,
#128371,#128372,#128373,#128374,#128375,#128376,#128377,#128378,#128379,
#128380,#128381,#128382,#128383,#128384,#128385,#128386,#128387,#128388,
#128389,#128390,#128391,#128392,#128393,#128394,#128395,#128396,#128397,
#128398,#128399,#128400,#128401,#128402,#128403,#128404,#128405,#128406,
#128407,#128408,#128409,#128410,#128411,#128412,#128413,#128414,#128415,
#128416,#128417,#128418,#128419,#128420,#128421,#128422,#128423,#128424,
#128425,#128426,#128427,#128428,#128429,#128430,#128431,#128432,#128433,
#128434,#128435),.UNSPECIFIED.,.F.,.F.,(4,2,2,2,2,2,2,2,2,2,2,2,2,2,2,2,
2,2,2,2,2,2,2,2,2,2,2,2,2,2,2,2,2,2,2,2,2,2,2,2,2,2,2,2,2,2,2,2,2,2,2,2,
2,2,2,2,2,2,2,2,2,2,2,2,2,2,2,2,2,2,2,2,2,2,2,2,2,2,2,2,2,2,2,2,2,2,2,2,
4),(0.608918989341705,0.632484436711806,0.637273809156127,0.640131774699361,
0.642744032348447,0.646213563623638,0.654541386609907,0.667973786822127,
0.683457893919245,0.686599175903856,0.688306897401734,0.689786345308303,
0.691874324148808,0.697404001959282,0.706823346973857,0.728972833995634,
0.733474289118519,0.736274343968621,0.738907918764235,0.742522989269425,
0.751964794522928,0.765674055561374,0.780303875070739,0.782969515737605,
0.784559545195217,0.786093298710694,0.788491532060691,0.797030781120296,
0.820237459707686,0.827591627808917,0.830915854723068,0.833510868366637,
0.836444335081826,0.841613195675993,0.848176484966463,0.866064239814026,
0.876456469708276,0.879010354951903,0.880576553732779,0.882130191610296,
0.884624970483063,0.894601588162329,0.910884464927515,0.922141959064336,
0.926017983330025,0.928428747876728,0.931103967257791,0.934963560827957,
0.946770646479986,0.958401217906793,0.971160568215792,0.974358619255303,
0.97607824984295,0.977554668640882,0.979620354387249,0.984986735521101,
0.99396307148355,1.01702366990304,1.02139639696923,1.02417049213732,1.02681661387665,
1.03051008576096,1.04062992210639,1.0606214488029,1.06860239311554,1.07101249078323,
1.07239689032026,1.07393981267283,1.07638331109697,1.08554723066564,1.10040223557177,
1.11362534522306,1.11767233363091,1.12011197650495,1.12276016036437,1.12646557909108,
1.13669345648822,1.1572378961673,1.16464061788624,1.16699804118402,1.16837290655736,
1.16992817595086,1.17243062336994,1.18254094045894,1.19737834953709,1.20973700949331,
1.2136250316396,1.2159190614085,1.21794213992136),.UNSPECIFIED.);
#1659=B_SPLINE_CURVE_WITH_KNOTS('',3,(#128440,#128441,#128442,#128443,#128444,
#128445,#128446,#128447,#128448,#128449,#128450,#128451,#128452,#128453,
#128454,#128455,#128456,#128457,#128458,#128459,#128460,#128461,#128462,
#128463,#128464,#128465,#128466,#128467,#128468,#128469,#128470,#128471,
#128472,#128473,#128474,#128475,#128476,#128477,#128478,#128479,#128480,
#128481,#128482,#128483,#128484,#128485,#128486,#128487,#128488,#128489,
#128490,#128491,#128492,#128493,#128494,#128495,#128496,#128497,#128498,
#128499,#128500,#128501,#128502,#128503,#128504,#128505,#128506,#128507,
#128508,#128509,#128510,#128511,#128512,#128513,#128514,#128515,#128516,
#128517,#128518,#128519,#128520,#128521,#128522,#128523,#128524,#128525,
#128526,#128527,#128528,#128529,#128530,#128531,#128532,#128533,#128534,
#128535,#128536,#128537,#128538,#128539,#128540,#128541,#128542,#128543,
#128544,#128545,#128546,#128547,#128548,#128549,#128550,#128551,#128552,
#128553,#128554,#128555,#128556,#128557,#128558,#128559,#128560,#128561,
#128562,#128563,#128564,#128565,#128566,#128567,#128568,#128569,#128570,
#128571,#128572,#128573,#128574,#128575,#128576,#128577,#128578,#128579,
#128580,#128581,#128582,#128583,#128584,#128585,#128586,#128587,#128588,
#128589,#128590,#128591,#128592,#128593,#128594,#128595,#128596,#128597,
#128598,#128599,#128600,#128601,#128602,#128603,#128604,#128605,#128606,
#128607,#128608,#128609,#128610,#128611,#128612,#128613),.UNSPECIFIED.,
 .F.,.F.,(4,2,2,2,2,2,2,2,2,2,2,2,2,2,2,2,2,2,2,2,2,2,2,2,2,2,2,2,2,2,2,
2,2,2,2,2,2,2,2,2,2,2,2,2,2,2,2,2,2,2,2,2,2,2,2,2,2,2,2,2,2,2,2,2,2,2,2,
2,2,2,2,2,2,2,2,2,2,2,2,2,2,2,2,2,2,2,4),(0.60887951146085,0.63078846196145,
0.636246071514392,0.639327828687595,0.641978652326842,0.645332871968072,
0.652473656908019,0.662838048063838,0.679225586919404,0.684888859343448,
0.687090294742984,0.688625163796033,0.690377561068731,0.693666908008892,
0.706172946614204,0.728420820783908,0.732952316780898,0.735820161194292,
0.73855611564422,0.742383636555123,0.7530970173112,0.776415355770046,0.781045890247718,
0.782906669269154,0.784442815939323,0.786190758553567,0.789458148429817,
0.801761723123946,0.824340727456653,0.828825622237181,0.831684162025967,
0.834425220388517,0.838283641176352,0.849303731922222,0.869851599669049,
0.876304128448469,0.878607601932729,0.88014339990219,0.881845072863965,
0.884886194535029,0.900814123069112,0.919405902405354,0.924273431886802,
0.927208019920632,0.929914422328036,0.933552900126604,0.942638452712715,
0.958293277779198,0.970324330388045,0.973530591100979,0.975284783676508,
0.976818788544093,0.979015726960102,0.98508074568147,0.995981619500491,
1.01524747154595,1.0200880836682,1.02301732688048,1.02572563834081,1.02937727686331,
1.03856518792535,1.05457076711339,1.06715902030929,1.06982112990831,1.07144311326391,
1.07304999990307,1.07564079581327,1.08651692922536,1.11178506740517,1.11625085324721,
1.11910537720804,1.1218482805648,1.12571905643322,1.13686879287472,1.1488418285501,
1.16184046939339,1.16509218560743,1.16685590326623,1.16838706086445,1.17056466767868,
1.17647680310206,1.18691247212009,1.20692216688272,1.21162581167888,1.21450938681323,
1.21633432088655,1.21787769075378),.UNSPECIFIED.);
#1660=B_SPLINE_CURVE_WITH_KNOTS('',3,(#128614,#128615,#128616,#128617,#128618,
#128619,#128620,#128621,#128622,#128623,#128624,#128625,#128626,#128627,
#128628,#128629,#128630,#128631,#128632,#128633,#128634,#128635,#128636,
#128637,#128638,#128639,#128640,#128641,#128642,#128643,#128644,#128645,
#128646,#128647,#128648,#128649,#128650,#128651,#128652,#128653,#128654,
#128655,#128656,#128657,#128658,#128659,#128660,#128661,#128662,#128663,
#128664,#128665,#128666,#128667,#128668,#128669,#128670,#128671,#128672,
#128673,#128674,#128675,#128676,#128677,#128678,#128679,#128680,#128681,
#128682,#128683,#128684,#128685,#128686,#128687,#128688,#128689,#128690,
#128691,#128692,#128693,#128694,#128695,#128696,#128697,#128698,#128699,
#128700,#128701,#128702,#128703,#128704,#128705,#128706,#128707,#128708,
#128709,#128710,#128711,#128712,#128713,#128714,#128715,#128716,#128717,
#128718,#128719,#128720,#128721,#128722,#128723,#128724,#128725,#128726,
#128727,#128728,#128729,#128730,#128731,#128732,#128733,#128734,#128735,
#128736,#128737,#128738,#128739,#128740,#128741,#128742,#128743,#128744,
#128745,#128746,#128747,#128748,#128749,#128750,#128751,#128752,#128753,
#128754,#128755,#128756,#128757,#128758,#128759,#128760,#128761,#128762,
#128763,#128764,#128765,#128766,#128767,#128768,#128769,#128770,#128771,
#128772,#128773,#128774,#128775,#128776,#128777,#128778,#128779,#128780,
#128781,#128782,#128783,#128784,#128785,#128786,#128787,#128788,#128789,
#128790,#128791),.UNSPECIFIED.,.F.,.F.,(4,2,2,2,2,2,2,2,2,2,2,2,2,2,2,2,
2,2,2,2,2,2,2,2,2,2,2,2,2,2,2,2,2,2,2,2,2,2,2,2,2,2,2,2,2,2,2,2,2,2,2,2,
2,2,2,2,2,2,2,2,2,2,2,2,2,2,2,2,2,2,2,2,2,2,2,2,2,2,2,2,2,2,2,2,2,2,2,2,
4),(8.19526309981665E-5,0.00244591647159546,0.00565097144129316,0.0199149569692758,
0.0346688995672485,0.0401375564983184,0.0439812982325549,0.0458055837598293,
0.0472688651094312,0.0491522821191064,0.0534505013740185,0.0774954801291768,
0.0882801505299676,0.0920443731556304,0.0947027717025768,0.0971306863623881,
0.101108584909388,0.113304743877449,0.128199856417806,0.138358251533931,
0.140863250575921,0.142419113123174,0.143983132271331,0.146526606389028,
0.156612415718612,0.174766481132769,0.181372385347927,0.186565427051088,
0.189503749625414,0.192098088266055,0.195414590006257,0.202437264464677,
0.224067039983559,0.231008360773772,0.235545672652667,0.237488118646269,
0.238813405926997,0.24054720908878,0.243812627023049,0.264827399178171,
0.274644925797415,0.281500937427829,0.284743957184957,0.287332042226077,
0.290318764903073,0.295607812312921,0.321605051886933,0.330427486138935,
0.332846830259632,0.334384888614309,0.33577375103773,0.338207607091329,
0.346450387533153,0.366212155480024,0.37628750741496,0.379976352313982,
0.382621825170941,0.385397563055197,0.389778004250474,0.412770634735769,
0.421769357309952,0.427144369638574,0.429211275916643,0.43068793648639,
0.432407029232186,0.435602298287446,0.448305247961947,0.459984858139832,
0.467953544759689,0.473896732047786,0.476978724664271,0.47956182752582,
0.482689285081147,0.488682379930929,0.511611371954516,0.522106312313085,
0.524629487098124,0.526189242649236,0.527561164028974,0.529901660446056,
0.53711005792618,0.55785815136795,0.568126553747768,0.571836688000997,0.574485777607362,
0.576924569385596,0.580966197696916,0.594087692635498,0.609138008733486),
 .UNSPECIFIED.);
#1661=B_SPLINE_CURVE_WITH_KNOTS('',3,(#128796,#128797,#128798,#128799,#128800,
#128801,#128802,#128803,#128804,#128805,#128806,#128807,#128808,#128809,
#128810,#128811,#128812,#128813,#128814,#128815,#128816,#128817,#128818,
#128819,#128820,#128821,#128822,#128823,#128824,#128825,#128826,#128827,
#128828,#128829,#128830,#128831,#128832,#128833,#128834,#128835,#128836,
#128837,#128838,#128839,#128840,#128841,#128842,#128843,#128844,#128845,
#128846,#128847,#128848,#128849,#128850,#128851,#128852,#128853,#128854,
#128855,#128856,#128857,#128858,#128859,#128860,#128861,#128862,#128863,
#128864,#128865,#128866,#128867,#128868,#128869,#128870,#128871,#128872,
#128873,#128874,#128875,#128876,#128877,#128878,#128879,#128880,#128881,
#128882,#128883,#128884,#128885,#128886,#128887,#128888,#128889,#128890,
#128891,#128892,#128893,#128894,#128895,#128896,#128897,#128898,#128899,
#128900,#128901,#128902,#128903,#128904,#128905,#128906,#128907,#128908,
#128909,#128910,#128911,#128912,#128913,#128914,#128915,#128916,#128917,
#128918,#128919,#128920,#128921,#128922,#128923,#128924,#128925,#128926,
#128927,#128928,#128929,#128930,#128931,#128932,#128933,#128934,#128935,
#128936,#128937,#128938,#128939,#128940,#128941,#128942,#128943,#128944,
#128945,#128946,#128947,#128948,#128949,#128950,#128951,#128952,#128953,
#128954,#128955,#128956,#128957,#128958,#128959,#128960,#128961,#128962,
#128963,#128964,#128965,#128966,#128967,#128968,#128969,#128970,#128971,
#128972,#128973,#128974,#128975),.UNSPECIFIED.,.F.,.F.,(4,2,2,2,2,2,2,2,
2,2,2,2,2,2,2,2,2,2,2,2,2,2,2,2,2,2,2,2,2,2,2,2,2,2,2,2,2,2,2,2,2,2,2,2,
2,2,2,2,2,2,2,2,2,2,2,2,2,2,2,2,2,2,2,2,2,2,2,2,2,2,2,2,2,2,2,2,2,2,2,2,
2,2,2,2,2,2,2,2,2,4),(5.12893345518819E-5,0.00961602028826353,0.0138783864723404,
0.0156577421109236,0.0170829123827336,0.0186135194993552,0.0207841578286592,
0.0262525119274115,0.0479517746797167,0.058911971909783,0.0628681794158502,
0.0656265742126552,0.0681264307526814,0.072186322735615,0.0840825386761356,
0.0991420979771004,0.10923377375189,0.111783160187943,0.113381645735688,
0.115013709611778,0.117722508140764,0.132281156871619,0.146032956853938,
0.155390619215895,0.159064220483621,0.161776114995443,0.164697371586683,
0.169496306846321,0.189372877381887,0.199890315284252,0.205830294353542,
0.208011752229538,0.209543788477623,0.211306257456261,0.21455078464435,
0.227436396483612,0.239609130322308,0.250725515970482,0.254593950766497,
0.257336970593552,0.260193122774559,0.264664753603286,0.289900385296866,
0.300787723467629,0.303379280451442,0.30498658958962,0.306608894513891,
0.309271446940452,0.321678209138169,0.33783682768254,0.347070195129053,
0.350728277760952,0.353437994709968,0.356365584223798,0.361195850267435,
0.380634609718299,0.39141847616228,0.397446093878205,0.399638629425916,
0.401172283903535,0.402929258052662,0.40614760768069,0.418485323473566,
0.433927164536807,0.442950562303215,0.446581596511575,0.4492873896495,0.452225977633481,
0.457111666114936,0.473971883262096,0.486538924812271,0.491039882527733,
0.494396709786513,0.496162646300481,0.497693793009992,0.499868740166097,
0.505364259950254,0.52720459259777,0.538212727787643,0.542070519412112,
0.54481173291316,0.547670938937443,0.552158024087738,0.577320729651941,
0.588246094979848,0.590839482092983,0.592447175756965,0.594069070452291,
0.596729685440606,0.60887951146085),.UNSPECIFIED.);
#1662=B_SPLINE_CURVE_WITH_KNOTS('',3,(#128976,#128977,#128978,#128979,#128980,
#128981,#128982,#128983,#128984,#128985,#128986,#128987,#128988,#128989,
#128990,#128991,#128992,#128993,#128994,#128995,#128996,#128997,#128998,
#128999,#129000,#129001,#129002,#129003,#129004,#129005,#129006,#129007,
#129008,#129009,#129010,#129011,#129012,#129013,#129014,#129015,#129016,
#129017,#129018,#129019,#129020,#129021,#129022,#129023,#129024,#129025,
#129026,#129027,#129028,#129029,#129030,#129031,#129032,#129033,#129034,
#129035,#129036,#129037,#129038,#129039,#129040,#129041,#129042,#129043,
#129044,#129045,#129046,#129047,#129048,#129049,#129050,#129051,#129052,
#129053,#129054,#129055,#129056,#129057,#129058,#129059,#129060,#129061,
#129062,#129063,#129064,#129065,#129066,#129067,#129068,#129069,#129070,
#129071,#129072,#129073,#129074,#129075,#129076,#129077,#129078,#129079,
#129080,#129081,#129082,#129083,#129084,#129085,#129086,#129087,#129088,
#129089,#129090,#129091,#129092,#129093,#129094,#129095,#129096,#129097,
#129098,#129099,#129100,#129101,#129102,#129103,#129104,#129105,#129106,
#129107,#129108,#129109,#129110,#129111,#129112,#129113,#129114,#129115,
#129116,#129117,#129118,#129119,#129120,#129121,#129122,#129123,#129124,
#129125,#129126,#129127,#129128,#129129,#129130,#129131,#129132,#129133,
#129134,#129135,#129136,#129137,#129138,#129139,#129140,#129141,#129142,
#129143,#129144,#129145,#129146,#129147,#129148,#129149,#129150,#129151,
#129152,#129153,#129154,#129155,#129156,#129157,#129158,#129159),
 .UNSPECIFIED.,.F.,.F.,(4,2,2,2,2,2,2,2,2,2,2,2,2,2,2,2,2,2,2,2,2,2,2,2,
2,2,2,2,2,2,2,2,2,2,2,2,2,2,2,2,2,2,2,2,2,2,2,2,2,2,2,2,2,2,2,2,2,2,2,2,
2,2,2,2,2,2,2,2,2,2,2,2,2,2,2,2,2,2,2,2,2,2,2,2,2,2,2,2,2,2,2,4),(0.609138008733486,
0.618121686590817,0.620604124036998,0.622002105544986,0.623530686121969,
0.625903148796938,0.63411857238587,0.654830264979436,0.664113515625273,
0.667800981357054,0.670420033508957,0.673189666814462,0.677539534727236,
0.682745306721759,0.69406344669956,0.712962843599388,0.716008422889573,
0.717695663655213,0.719180811500166,0.721309152445293,0.727149459063446,
0.737458921942084,0.757930808098366,0.762629080484255,0.765468653405884,
0.768086592985896,0.771597950377354,0.78023050055152,0.794553633104294,
0.808650559203278,0.81183956428775,0.813557331675355,0.815034252303567,
0.81710348489575,0.82249526626144,0.831539337123217,0.854458488696198,0.858852055941957,
0.861630393630956,0.8642744036964,0.867954663137728,0.877955158175062,0.897367019277808,
0.90597650074626,0.90843761403847,0.909831549257518,0.911364091088334,0.913756465787837,
0.922220946046426,0.944802275419074,0.95250189492096,0.955923107500246,
0.958536786579955,0.961388948826537,0.966150409850912,0.981025765637848,
0.998392295653103,1.0029525356252,1.00474845045902,1.00623414369772,1.00791926860864,
1.01104118184762,1.02241662056397,1.04442112541473,1.04979707790695,1.05280145201634,
1.05538771208352,1.05860610285131,1.06531789688386,1.07482667917306,1.09400778017891,
1.09875486238431,1.10059770369467,1.10207878647515,1.10372980381599,1.10668617869406,
1.1212735270503,1.14167830590248,1.14637186445387,1.14921010743941,1.15182777682574,
1.15534023905504,1.16394194266049,1.17820731836293,1.19226971700874,1.19552429316274,
1.19725560607294,1.19858093669015,1.20002590475801,1.2019659721872,1.20634034158939,
1.21790188230871),.UNSPECIFIED.);
#1663=B_SPLINE_CURVE_WITH_KNOTS('',3,(#129164,#129165,#129166,#129167,#129168,
#129169,#129170,#129171,#129172,#129173,#129174,#129175,#129176,#129177,
#129178,#129179,#129180,#129181,#129182,#129183,#129184,#129185,#129186,
#129187,#129188,#129189,#129190,#129191,#129192,#129193,#129194,#129195,
#129196,#129197,#129198,#129199,#129200,#129201,#129202,#129203,#129204,
#129205,#129206,#129207,#129208,#129209,#129210,#129211,#129212,#129213,
#129214,#129215,#129216,#129217,#129218,#129219,#129220,#129221,#129222,
#129223,#129224,#129225,#129226,#129227,#129228,#129229,#129230,#129231,
#129232,#129233,#129234,#129235,#129236,#129237,#129238,#129239,#129240,
#129241,#129242,#129243,#129244,#129245,#129246,#129247,#129248,#129249,
#129250,#129251,#129252,#129253,#129254,#129255,#129256,#129257,#129258,
#129259,#129260,#129261,#129262,#129263,#129264,#129265,#129266,#129267,
#129268,#129269,#129270,#129271,#129272,#129273,#129274,#129275,#129276,
#129277,#129278,#129279,#129280,#129281,#129282,#129283,#129284,#129285,
#129286,#129287,#129288,#129289,#129290,#129291,#129292,#129293,#129294,
#129295,#129296,#129297,#129298,#129299,#129300,#129301,#129302,#129303,
#129304,#129305,#129306,#129307,#129308,#129309,#129310,#129311,#129312,
#129313,#129314,#129315,#129316,#129317,#129318,#129319,#129320,#129321,
#129322,#129323,#129324,#129325,#129326,#129327,#129328,#129329,#129330,
#129331,#129332,#129333,#129334,#129335,#129336,#129337),.UNSPECIFIED.,
 .F.,.F.,(4,2,2,2,2,2,2,2,2,2,2,2,2,2,2,2,2,2,2,2,2,2,2,2,2,2,2,2,2,2,2,
2,2,2,2,2,2,2,2,2,2,2,2,2,2,2,2,2,2,2,2,2,2,2,2,2,2,2,2,2,2,2,2,2,2,2,2,
2,2,2,2,2,2,2,2,2,2,2,2,2,2,2,2,2,2,2,4),(0.609294493087457,0.612279274065476,
0.61497192061227,0.618502815827184,0.626793786753854,0.640018988953453,
0.655625305147717,0.658796725165967,0.660543726057257,0.662080335124041,
0.664293274988974,0.670486473944873,0.68179004732075,0.700448315669616,
0.705315168785881,0.708250050099495,0.710957161248477,0.714597268008012,
0.723691275086161,0.739371403554182,0.751376313844737,0.754582274304652,
0.756336637342183,0.757871039088155,0.760068886138465,0.76613869369244,
0.777052709909105,0.796305799994951,0.801148381623591,0.804078446237653,
0.806787284056524,0.810439270506911,0.819625663961472,0.835622484328683,
0.848230270695418,0.850893023069629,0.852515373479983,0.854122598581708,
0.856713901661463,0.867591207402952,0.892867173331642,0.89733344193225,
0.900188491779084,0.902932052294452,0.906804016152967,0.917959726214802,
0.929939874734508,0.942933487951805,0.94618533305264,0.947949313116664,
0.949480837750616,0.951659156849383,0.957574444124615,0.968017960039134,
0.988040341506333,0.992828943200652,0.995748063367594,0.99846059597962,
1.00213919537037,1.01153908642404,1.02830423792746,1.0398852037876,1.04253440435527,
1.04415378920164,1.04576353760859,1.0483672901349,1.05951348088051,1.08427736603894,
1.08885034179558,1.09172635390582,1.09445781871163,1.09825854854641,1.10871823539971,
1.13038334860397,1.13650879204335,1.13877187099174,1.14030100385222,1.14201899391671,
1.14513920447827,1.15615698640013,1.1801774311948,1.18471024799207,1.18757814899122,
1.19031362350176,1.1941395743653,1.19983412647968,1.2183544972758),
 .UNSPECIFIED.);
#1664=B_SPLINE_CURVE_WITH_KNOTS('',3,(#129338,#129339,#129340,#129341,#129342,
#129343,#129344,#129345,#129346,#129347,#129348,#129349,#129350,#129351,
#129352,#129353,#129354,#129355,#129356,#129357,#129358,#129359,#129360,
#129361,#129362,#129363,#129364,#129365,#129366,#129367,#129368,#129369,
#129370,#129371,#129372,#129373,#129374,#129375,#129376,#129377,#129378,
#129379,#129380,#129381,#129382,#129383,#129384,#129385,#129386,#129387,
#129388,#129389,#129390,#129391,#129392,#129393,#129394,#129395,#129396,
#129397,#129398,#129399,#129400,#129401,#129402,#129403,#129404,#129405,
#129406,#129407,#129408,#129409,#129410,#129411,#129412,#129413,#129414,
#129415,#129416,#129417,#129418,#129419,#129420,#129421,#129422,#129423,
#129424,#129425,#129426,#129427,#129428,#129429,#129430,#129431,#129432,
#129433,#129434,#129435,#129436,#129437,#129438,#129439,#129440,#129441,
#129442,#129443,#129444,#129445,#129446,#129447,#129448,#129449,#129450,
#129451,#129452,#129453,#129454,#129455,#129456,#129457,#129458,#129459,
#129460,#129461,#129462,#129463,#129464,#129465,#129466,#129467,#129468,
#129469,#129470,#129471,#129472,#129473,#129474,#129475,#129476,#129477,
#129478,#129479,#129480,#129481,#129482,#129483,#129484,#129485,#129486,
#129487,#129488,#129489,#129490,#129491,#129492,#129493,#129494,#129495,
#129496,#129497,#129498,#129499,#129500,#129501,#129502,#129503,#129504,
#129505,#129506,#129507,#129508,#129509,#129510,#129511,#129512,#129513,
#129514,#129515),.UNSPECIFIED.,.F.,.F.,(4,2,2,2,2,2,2,2,2,2,2,2,2,2,2,2,
2,2,2,2,2,2,2,2,2,2,2,2,2,2,2,2,2,2,2,2,2,2,2,2,2,2,2,2,2,2,2,2,2,2,2,2,
2,2,2,2,2,2,2,2,2,2,2,2,2,2,2,2,2,2,2,2,2,2,2,2,2,2,2,2,2,2,2,2,2,2,2,2,
4),(4.48084807998542E-5,0.0151895777249643,0.0211597089994056,0.0241810351308087,
0.0270781628467691,0.0296805266355577,0.0330134375814879,0.0403420703475364,
0.0634508972498917,0.0719769345664564,0.0743741833310849,0.0759078615777264,
0.0774983741590798,0.0801658532645623,0.0948327763534422,0.108628642746622,
0.117993146897431,0.121599128960157,0.124231455826626,0.127035048151024,
0.131553364787702,0.153562173692234,0.163042257784255,0.168594117172197,
0.170685122280674,0.172165100115765,0.173871437850454,0.177005853269734,
0.192680303941157,0.206009550050221,0.214300926818803,0.217765564950306,
0.220377299650659,0.223237750965991,0.228039007803243,0.24694125143082,
0.258209233169335,0.264360434034748,0.266527086387937,0.26801828057052,
0.269688169226704,0.272734729901128,0.293979348286441,0.303918578330245,
0.310830813132952,0.314083363529147,0.316672281479533,0.319652574267506,
0.32490979924372,0.350959712738519,0.359787274778588,0.362207103561469,
0.363745325806985,0.365134213070399,0.367567889566214,0.375807187632045,
0.395573891358208,0.405650631215977,0.40933979037851,0.411985441904402,
0.414761326339755,0.419141909308159,0.4421368705191,0.451135727455969,0.456510915015384,
0.458577927971528,0.460054677603236,0.461773889507287,0.464969415388399,
0.478839018033031,0.493329402537119,0.502017403090592,0.505536464241162,
0.50815563162367,0.510992255872711,0.515675363887792,0.536284222426344,
0.546504997765943,0.552315476919564,0.554440061815629,0.555924742939173,
0.557613938883323,0.560668397200182,0.577529839932072,0.596420446495926,
0.600616890931166,0.603356196005889,0.605993806741988,0.609188119348819),
 .UNSPECIFIED.);
#1665=B_SPLINE_CURVE_WITH_KNOTS('',3,(#129520,#129521,#129522,#129523,#129524,
#129525,#129526,#129527,#129528,#129529,#129530,#129531,#129532,#129533,
#129534,#129535,#129536,#129537,#129538,#129539,#129540,#129541,#129542,
#129543,#129544,#129545,#129546,#129547,#129548,#129549,#129550,#129551,
#129552,#129553,#129554,#129555,#129556,#129557,#129558,#129559,#129560,
#129561,#129562,#129563,#129564,#129565,#129566,#129567,#129568,#129569,
#129570,#129571,#129572,#129573,#129574,#129575,#129576,#129577,#129578,
#129579,#129580,#129581,#129582,#129583,#129584,#129585,#129586,#129587,
#129588,#129589,#129590,#129591,#129592,#129593,#129594,#129595,#129596,
#129597,#129598,#129599,#129600,#129601,#129602,#129603,#129604,#129605,
#129606,#129607,#129608,#129609,#129610,#129611,#129612,#129613,#129614,
#129615,#129616,#129617,#129618,#129619,#129620,#129621,#129622,#129623,
#129624,#129625,#129626,#129627,#129628,#129629,#129630,#129631,#129632,
#129633,#129634,#129635,#129636,#129637,#129638,#129639,#129640,#129641,
#129642,#129643,#129644,#129645,#129646,#129647,#129648,#129649,#129650,
#129651,#129652,#129653,#129654,#129655,#129656,#129657,#129658,#129659,
#129660,#129661,#129662,#129663,#129664,#129665,#129666,#129667,#129668,
#129669,#129670,#129671,#129672,#129673,#129674,#129675,#129676,#129677,
#129678,#129679,#129680,#129681,#129682,#129683,#129684,#129685,#129686,
#129687,#129688,#129689,#129690,#129691),.UNSPECIFIED.,.F.,.F.,(4,2,2,2,
2,2,2,2,2,2,2,2,2,2,2,2,2,2,2,2,2,2,2,2,2,2,2,2,2,2,2,2,2,2,2,2,2,2,2,2,
2,2,2,2,2,2,2,2,2,2,2,2,2,2,2,2,2,2,2,2,2,2,2,2,2,2,2,2,2,2,2,2,2,2,2,2,
2,2,2,2,2,2,2,2,2,4),(0.00027441463337703,0.0227636344260558,0.0322427410889548,
0.0359313348477803,0.0386454365053149,0.0415608691984186,0.0463307052750516,
0.0665447975002483,0.0768652460854365,0.0827392509239614,0.0849122885035225,
0.086443149400746,0.0882099542434203,0.0914751140924374,0.104518576206399,
0.116544106461167,0.127622856500184,0.131487565135147,0.134229917503476,
0.137087068379059,0.141563916580247,0.166774405195101,0.177674564619549,
0.180266706225982,0.181874119018986,0.183496253788006,0.186158086626929,
0.198445734692305,0.214691712589056,0.223949729926721,0.227610891672681,
0.230321020449478,0.233247305120228,0.238071189693857,0.257608118769696,
0.268331010584425,0.274338721466226,0.276528746899259,0.278062024199386,
0.27982021575149,0.283044381765916,0.295530276535114,0.307737121188378,
0.319181811325464,0.323081586699972,0.325830046824822,0.328340183557665,
0.332461613406117,0.345746920269917,0.36046451453457,0.369508991325578,
0.371990971145363,0.373575722034662,0.375019587866653,0.377585796594849,
0.387019427809224,0.405546790550378,0.415387362640507,0.419119158255573,
0.421839786027067,0.424739208246939,0.429429073363312,0.450413828377309,
0.460308783189393,0.464259933572517,0.467307768497564,0.469010982618376,
0.470546401756773,0.472846809297149,0.479271700426983,0.500640134566339,
0.511052030554104,0.514848043354771,0.517578929586235,0.520456799323398,
0.525038297061851,0.549748520976427,0.560913927729103,0.563518437595197,
0.565128442483085,0.566747808622801,0.569396625300546,0.58094472891131,
0.597752195824288,0.604176596763572,0.609294493087457),.UNSPECIFIED.);
#1666=B_SPLINE_CURVE_WITH_KNOTS('',3,(#129692,#129693,#129694,#129695,#129696,
#129697,#129698,#129699,#129700,#129701,#129702,#129703,#129704,#129705,
#129706,#129707,#129708,#129709,#129710,#129711,#129712,#129713,#129714,
#129715,#129716,#129717,#129718,#129719,#129720,#129721,#129722,#129723,
#129724,#129725,#129726,#129727,#129728,#129729,#129730,#129731,#129732,
#129733,#129734,#129735,#129736,#129737,#129738,#129739,#129740,#129741,
#129742,#129743,#129744,#129745,#129746,#129747,#129748,#129749,#129750,
#129751,#129752,#129753,#129754,#129755,#129756,#129757,#129758,#129759,
#129760,#129761,#129762,#129763,#129764,#129765,#129766,#129767,#129768,
#129769,#129770,#129771,#129772,#129773,#129774,#129775,#129776,#129777,
#129778,#129779,#129780,#129781,#129782,#129783,#129784,#129785,#129786,
#129787,#129788,#129789,#129790,#129791,#129792,#129793,#129794,#129795,
#129796,#129797,#129798,#129799,#129800,#129801,#129802,#129803,#129804,
#129805,#129806,#129807,#129808,#129809,#129810,#129811,#129812,#129813,
#129814,#129815,#129816,#129817,#129818,#129819,#129820,#129821,#129822,
#129823,#129824,#129825,#129826,#129827,#129828,#129829,#129830,#129831,
#129832,#129833,#129834,#129835,#129836,#129837,#129838,#129839,#129840,
#129841,#129842,#129843,#129844,#129845,#129846,#129847,#129848,#129849,
#129850,#129851,#129852,#129853,#129854,#129855,#129856,#129857,#129858,
#129859,#129860,#129861,#129862,#129863,#129864,#129865,#129866,#129867),
 .UNSPECIFIED.,.F.,.F.,(4,2,2,2,2,2,2,2,2,2,2,2,2,2,2,2,2,2,2,2,2,2,2,2,
2,2,2,2,2,2,2,2,2,2,2,2,2,2,2,2,2,2,2,2,2,2,2,2,2,2,2,2,2,2,2,2,2,2,2,2,
2,2,2,2,2,2,2,2,2,2,2,2,2,2,2,2,2,2,2,2,2,2,2,2,2,2,2,4),(0.609188119348819,
0.618088851492723,0.633251114555404,0.646123396145481,0.649328424879929,
0.651049569329106,0.652525729076646,0.654588946612196,0.659937032324217,
0.668864420913284,0.692031038401225,0.696388585364891,0.699159732645307,
0.701807663723004,0.705511420767342,0.715723765954798,0.73618623161773,
0.743675524160358,0.746040354126816,0.747416559450016,0.748970029804227,
0.75146388487105,0.761423724940592,0.777623940814963,0.788967600956461,
0.79285090894607,0.795262921885291,0.797936912129993,0.801789426093628,
0.813514444614515,0.825109158173883,0.837991138658734,0.841196760179125,
0.842918011848968,0.844394116928159,0.846457059844592,0.851803317821929,
0.860725937879379,0.883902030814145,0.888258056202085,0.891028868527889,
0.893676917724308,0.897381577058123,0.907602576370799,0.928110941942554,
0.935551435755209,0.937912091513974,0.939287532172419,0.940841992354981,
0.94334062461135,0.953383857780236,0.96999816569416,0.972396809936449,0.981382967455826,
0.985030666058229,0.987669352280554,0.990458136533524,0.9949039347227,1.00026281686337,
1.01217754719982,1.03026941080494,1.03327206851665,1.03493281777466,1.03642727176729,
1.0386146786155,1.04494293428585,1.05679214336884,1.07487141672425,1.0796911322994,
1.08255510669432,1.08516547322749,1.08862146343895,1.09685403931589,1.11002083763632,
1.12593023907983,1.1290533738711,1.13075719629866,1.13223758013055,1.13433276094272,
1.13991693633654,1.1494881249364,1.17133428962439,1.17587548115476,1.17868344602129,
1.18131339927006,1.18490578156157,1.19416368997785,1.21816034869378),
 .UNSPECIFIED.);
#1667=B_SPLINE_CURVE_WITH_KNOTS('',3,(#129872,#129873,#129874,#129875,#129876,
#129877,#129878,#129879,#129880,#129881,#129882,#129883,#129884,#129885,
#129886,#129887,#129888,#129889,#129890,#129891,#129892,#129893,#129894,
#129895,#129896,#129897,#129898,#129899,#129900,#129901,#129902,#129903,
#129904,#129905,#129906,#129907,#129908,#129909,#129910,#129911,#129912,
#129913,#129914,#129915,#129916,#129917,#129918,#129919,#129920,#129921,
#129922,#129923,#129924,#129925,#129926,#129927,#129928,#129929,#129930,
#129931,#129932,#129933,#129934,#129935,#129936,#129937,#129938,#129939,
#129940,#129941,#129942,#129943,#129944,#129945,#129946,#129947,#129948,
#129949,#129950,#129951,#129952,#129953,#129954,#129955,#129956,#129957,
#129958,#129959,#129960,#129961,#129962,#129963,#129964,#129965,#129966,
#129967,#129968,#129969,#129970,#129971,#129972,#129973,#129974,#129975,
#129976,#129977,#129978,#129979,#129980,#129981,#129982,#129983,#129984,
#129985,#129986,#129987,#129988,#129989,#129990,#129991,#129992,#129993,
#129994,#129995,#129996,#129997,#129998,#129999,#130000,#130001,#130002,
#130003,#130004,#130005,#130006,#130007,#130008,#130009,#130010,#130011,
#130012,#130013,#130014,#130015,#130016,#130017,#130018,#130019,#130020,
#130021,#130022,#130023,#130024,#130025),.UNSPECIFIED.,.F.,.F.,(4,3,3,3,
3,3,3,3,3,3,3,3,3,3,3,3,3,3,3,3,3,3,3,3,3,3,3,3,3,3,3,3,3,3,3,3,3,3,3,3,
3,3,3,3,3,3,3,3,3,3,3,4),(-60.6402364208082,-60.4782147259492,-60.3931758543397,
-60.2672790840686,-60.1415709515627,-60.0159902828507,-59.8904761268088,
-59.7648709710315,-59.6392266695458,-59.5133279238666,-59.404570569114,
-59.2786776312088,-59.1529733209067,-59.0273964554494,-58.9018860749222,
-58.7762846146787,-58.6506439704419,-58.5247487641054,-58.4159652838882,
-58.2900772181433,-58.1643778917407,-58.0388061101619,-57.9133009019233,
-57.7877047030512,-57.6620693774554,-57.5361795087896,-57.4273599986625,
-57.3014681741924,-57.1757650286975,-57.0501893766061,-56.9246802552742,
-56.799080114101,-56.6734408239648,-56.5475470110616,-56.4387547134368,
-56.3128637271534,-56.1871614244939,-56.0615866179333,-55.9360783428843,
-55.8104790410212,-55.6848405876649,-55.558947595072,-55.450149428211,-55.3242589588329,
-55.1985571863574,-55.0729829220047,-54.9474751999556,-54.8218764627213,
-54.6962385812792,-54.5703461645474,-54.4615441429853,-54.3570525280441),
 .UNSPECIFIED.);
#1668=B_SPLINE_CURVE_WITH_KNOTS('',3,(#130026,#130027,#130028,#130029,#130030,
#130031,#130032,#130033,#130034,#130035,#130036,#130037,#130038,#130039,
#130040,#130041,#130042,#130043,#130044,#130045,#130046,#130047,#130048,
#130049,#130050,#130051,#130052,#130053,#130054,#130055,#130056,#130057,
#130058,#130059,#130060,#130061,#130062,#130063,#130064,#130065,#130066,
#130067,#130068,#130069,#130070,#130071,#130072,#130073,#130074,#130075,
#130076,#130077,#130078,#130079,#130080,#130081,#130082,#130083,#130084,
#130085,#130086,#130087,#130088,#130089,#130090,#130091,#130092,#130093,
#130094,#130095,#130096,#130097,#130098,#130099,#130100,#130101,#130102,
#130103,#130104,#130105,#130106,#130107,#130108,#130109,#130110,#130111,
#130112,#130113,#130114,#130115,#130116,#130117,#130118,#130119,#130120,
#130121,#130122,#130123,#130124,#130125,#130126,#130127,#130128,#130129,
#130130,#130131,#130132,#130133,#130134,#130135,#130136,#130137,#130138,
#130139,#130140,#130141,#130142,#130143,#130144,#130145,#130146,#130147,
#130148,#130149,#130150,#130151,#130152,#130153,#130154,#130155,#130156,
#130157,#130158,#130159,#130160,#130161,#130162,#130163,#130164,#130165,
#130166,#130167,#130168,#130169,#130170,#130171,#130172,#130173,#130174,
#130175,#130176,#130177,#130178,#130179,#130180,#130181,#130182,#130183,
#130184,#130185,#130186,#130187,#130188,#130189,#130190,#130191,#130192,
#130193,#130194,#130195,#130196,#130197,#130198,#130199,#130200,#130201,
#130202,#130203,#130204,#130205,#130206,#130207),.UNSPECIFIED.,.F.,.F.,
(4,2,2,2,2,2,2,2,2,2,2,2,2,2,2,2,2,2,2,2,2,2,2,2,2,2,2,2,2,2,2,2,2,2,2,
2,2,2,2,2,2,2,2,2,2,2,2,2,2,2,2,2,2,2,2,2,2,2,2,2,2,2,2,2,2,2,2,2,2,2,2,
2,2,2,2,2,2,2,2,2,2,2,2,2,2,2,2,2,2,2,4),(7.25993422053199E-5,0.00369566804877558,
0.00618834178124166,0.00773784430141063,0.00910319675066312,0.0106852833649096,
0.0133134497730082,0.0261054828078791,0.0331610911352754,0.0499936763290807,
0.0541386006359566,0.0568679278235674,0.0595129230942833,0.0627374444668784,
0.0713106167633259,0.0928459506236268,0.101174364557697,0.103555949911492,
0.105086420675871,0.106482637911173,0.108955522422688,0.11775688050675,
0.13701672551699,0.146986699811162,0.150663828661202,0.153307445971623,
0.156086993241243,0.160486090426006,0.183351853125453,0.192411579863944,
0.197809442806072,0.199879545556519,0.201356673666114,0.203074133590082,
0.206261389796618,0.218796887175313,0.233932428478149,0.243149431099175,
0.24673698031787,0.249366315129622,0.252176283103351,0.25672693241933,0.278483460683517,
0.288089925929344,0.293686878783432,0.295783774293984,0.297264473522018,
0.298967511369874,0.302086821858706,0.318146208316721,0.331233332100341,
0.339437081919361,0.342889099991582,0.345498979467513,0.34836486259968,
0.353194021885801,0.368906863329096,0.382483351759184,0.38929185470536,
0.391532460673219,0.393036074454538,0.394675843175733,0.39757754460442,
0.416584588979802,0.431515519003177,0.436852156073985,0.439818538441746,
0.442408801017214,0.445681024475371,0.452713461719678,0.476319414830594,
0.484901400945815,0.487302719149374,0.488837089916244,0.490426343316705,
0.493088216099066,0.507657015514054,0.522357079148755,0.531112464042791,
0.534640400318591,0.537260769989273,0.54009361677814,0.544758294763645,
0.568935359620865,0.576800092172742,0.581730853438571,0.583734128484157,
0.585203525830628,0.586961159003475,0.5904493867492,0.608920537561877),
 .UNSPECIFIED.);
#1669=B_SPLINE_CURVE_WITH_KNOTS('',3,(#130212,#130213,#130214,#130215,#130216,
#130217,#130218,#130219,#130220,#130221,#130222,#130223,#130224,#130225,
#130226,#130227,#130228,#130229,#130230,#130231,#130232,#130233,#130234,
#130235,#130236,#130237,#130238,#130239,#130240,#130241,#130242,#130243,
#130244,#130245,#130246,#130247,#130248,#130249,#130250,#130251,#130252,
#130253,#130254,#130255,#130256,#130257,#130258,#130259,#130260,#130261,
#130262,#130263,#130264,#130265,#130266,#130267,#130268,#130269,#130270,
#130271,#130272,#130273,#130274,#130275,#130276,#130277,#130278,#130279,
#130280,#130281,#130282,#130283,#130284,#130285,#130286,#130287,#130288,
#130289,#130290,#130291,#130292,#130293,#130294,#130295,#130296,#130297,
#130298,#130299,#130300,#130301,#130302,#130303,#130304,#130305,#130306,
#130307,#130308,#130309,#130310,#130311,#130312,#130313,#130314,#130315,
#130316,#130317,#130318,#130319,#130320,#130321,#130322,#130323,#130324,
#130325,#130326,#130327,#130328,#130329,#130330,#130331,#130332,#130333,
#130334,#130335,#130336,#130337,#130338,#130339,#130340,#130341,#130342,
#130343,#130344,#130345,#130346,#130347,#130348,#130349,#130350,#130351,
#130352,#130353,#130354,#130355,#130356,#130357,#130358,#130359,#130360,
#130361,#130362,#130363,#130364,#130365,#130366,#130367,#130368,#130369,
#130370,#130371,#130372,#130373,#130374,#130375,#130376,#130377,#130378,
#130379,#130380,#130381,#130382,#130383,#130384,#130385,#130386,#130387,
#130388,#130389,#130390,#130391,#130392,#130393,#130394,#130395,#130396,
#130397,#130398,#130399,#130400,#130401),.UNSPECIFIED.,.F.,.F.,(4,3,3,3,
3,3,3,3,3,3,3,3,3,3,3,3,3,3,3,3,3,3,3,3,3,3,3,3,3,3,3,3,3,3,3,3,3,3,3,3,
3,3,3,3,3,3,3,3,3,3,3,3,3,3,3,3,3,3,3,3,3,3,3,4),(-66.9234231424034,-66.7973292349505,
-66.6710781156156,-66.5447477367036,-66.4181217720289,-66.3248576010649,
-66.324807565694,-66.2088850243393,-66.1987599683357,-66.0729012718308,
-65.9471706622924,-65.8215075487528,-65.6957564473878,-65.5699676397352,
-65.4439289408944,-65.3362456643337,-65.3362022804683,-65.2195847317972,
-65.2101075849637,-65.0841968766125,-64.9584094730824,-64.8326849073244,
-64.706865627026,-64.5810048306654,-64.4548887683224,-64.3476423483233,
-64.3475969952426,-64.2314304079549,-64.2218574338031,-64.0963089413872,
-63.9708899769272,-63.8455392267311,-63.720098590772,-63.5946196851449,
-63.4688854072963,-63.3590377815925,-63.3589917100169,-63.2427560995522,
-63.2330689835492,-63.1073347979478,-62.9817280397894,-62.8561878182684,
-62.7305568863553,-62.6048869281379,-62.4789631013509,-62.3704315643027,
-62.3703864247911,-62.2540719067799,-62.2444736699696,-62.1187490531194,
-61.9931514396376,-61.8676199169368,-61.7419968992799,-61.6163344354188,
-61.4904172856392,-61.3818266163067,-61.3817811395654,-61.2665055674753,
-61.257325972207,-61.1330666724535,-61.0089048450847,-60.8848099234832,
-60.7606137535066,-60.6402378352237),.UNSPECIFIED.);
#1670=B_SPLINE_CURVE_WITH_KNOTS('',3,(#130402,#130403,#130404,#130405,#130406,
#130407,#130408,#130409,#130410,#130411,#130412,#130413,#130414,#130415,
#130416,#130417,#130418,#130419,#130420,#130421,#130422,#130423,#130424,
#130425,#130426,#130427,#130428,#130429,#130430,#130431,#130432,#130433,
#130434,#130435,#130436,#130437,#130438,#130439,#130440,#130441,#130442,
#130443,#130444,#130445,#130446,#130447,#130448,#130449,#130450,#130451,
#130452,#130453,#130454,#130455,#130456,#130457,#130458,#130459,#130460,
#130461,#130462,#130463,#130464,#130465,#130466,#130467,#130468,#130469,
#130470,#130471,#130472,#130473,#130474,#130475,#130476,#130477,#130478,
#130479,#130480,#130481,#130482,#130483,#130484,#130485,#130486,#130487,
#130488,#130489,#130490,#130491,#130492,#130493,#130494,#130495,#130496,
#130497,#130498,#130499,#130500,#130501,#130502,#130503,#130504,#130505,
#130506,#130507,#130508,#130509,#130510,#130511,#130512,#130513,#130514,
#130515,#130516,#130517,#130518,#130519,#130520,#130521,#130522,#130523,
#130524,#130525,#130526,#130527,#130528,#130529,#130530,#130531,#130532,
#130533,#130534,#130535,#130536,#130537,#130538,#130539,#130540,#130541,
#130542,#130543,#130544,#130545,#130546,#130547,#130548,#130549,#130550,
#130551,#130552,#130553,#130554,#130555,#130556,#130557,#130558,#130559,
#130560,#130561,#130562,#130563,#130564,#130565,#130566,#130567,#130568,
#130569,#130570,#130571,#130572,#130573,#130574,#130575,#130576,#130577,
#130578,#130579,#130580,#130581,#130582,#130583),.UNSPECIFIED.,.F.,.F.,
(4,2,2,2,2,2,2,2,2,2,2,2,2,2,2,2,2,2,2,2,2,2,2,2,2,2,2,2,2,2,2,2,2,2,2,
2,2,2,2,2,2,2,2,2,2,2,2,2,2,2,2,2,2,2,2,2,2,2,2,2,2,2,2,2,2,2,2,2,2,2,2,
2,2,2,2,2,2,2,2,2,2,2,2,2,2,2,2,2,2,2,4),(0.608920537561877,0.624256168821786,
0.629113545833075,0.631984807747575,0.634592672523624,0.638031779520276,
0.646148364536954,0.658998977436563,0.675381501983869,0.678505790283175,
0.680209709878118,0.681689799426814,0.683783962833883,0.689361458107024,
0.698913960843616,0.720802163427926,0.725338537781256,0.728145489516899,
0.730775776501109,0.734370663585568,0.74364943537995,0.758989794829869,
0.771231344264241,0.774406042415989,0.776120879293817,0.77759916748082,
0.779675436334702,0.785114454594341,0.794285845542122,0.816916219815622,
0.821348668097504,0.824135389091964,0.826776458273983,0.830434692948252,
0.840235884974788,0.858744218665279,0.868381253314547,0.870908487310343,
0.872469105255741,0.87402668594989,0.876544555470676,0.886961905685532,
0.909482481109093,0.915882818588326,0.919045664496742,0.921627181159771,
0.924671388852573,0.930422299408979,0.94305445112279,0.959548356727087,
0.965120913715681,0.967268595971487,0.968755837047758,0.970432241905588,
0.973512635765905,0.984535804865729,1.00817377297338,1.01295478777827,1.01581133191923,
1.01842447860032,1.02189854342733,1.03025811199955,1.04378644621304,1.05910718918934,
1.06224292418989,1.06395039714074,1.06543508638462,1.0675369240636,1.07314016936173,
1.08276533216519,1.10434385098459,1.10890314240192,1.11171865226943,1.1143538825839,
1.11795124642645,1.12721193308001,1.14247082217507,1.15484174720004,1.15802184143598,
1.15973787719428,1.16120698748422,1.1632603011753,1.16860217125017,1.17752424378311,
1.18797933217666,1.20152973972704,1.20554483227242,1.20796744875538,1.21041405025214,
1.21298593217112,1.21791947617356),.UNSPECIFIED.);
#1671=B_SPLINE_CURVE_WITH_KNOTS('',3,(#130589,#130590,#130591,#130592,#130593,
#130594,#130595,#130596,#130597,#130598,#130599,#130600,#130601,#130602,
#130603,#130604,#130605,#130606,#130607,#130608,#130609,#130610,#130611,
#130612,#130613,#130614,#130615,#130616,#130617,#130618,#130619,#130620,
#130621,#130622,#130623,#130624,#130625,#130626,#130627,#130628),
 .UNSPECIFIED.,.F.,.F.,(4,2,2,2,2,2,2,2,2,2,2,2,2,2,2,2,2,2,2,4),(-0.104760453105363,
-0.0994634724235555,-0.0968929368591775,-0.0954871930896152,-0.0939247039312219,
-0.0913394407810213,-0.0808838676492878,-0.0652008291509204,-0.0612243537920569,
-0.0588035558409778,-0.0561167224443349,-0.0521532597402351,-0.03944228777409,
-0.0260061456948558,-0.0234232455547038,-0.0218595630230891,-0.0202410662692351,
-0.0185042201956334,-0.0157590766080668,-1.33456115395515E-5),
 .UNSPECIFIED.);
#1672=B_SPLINE_CURVE_WITH_KNOTS('',3,(#130631,#130632,#130633,#130634,#130635,
#130636,#130637,#130638),.UNSPECIFIED.,.F.,.F.,(4,2,2,4),(-0.0123240142976081,
-0.00994052883850335,-0.00623763007844346,-1.5266722490738E-5),
 .UNSPECIFIED.);
#1673=B_SPLINE_CURVE_WITH_KNOTS('',3,(#130643,#130644,#130645,#130646,#130647,
#130648,#130649,#130650,#130651,#130652,#130653,#130654,#130655,#130656,
#130657,#130658,#130659,#130660,#130661,#130662,#130663,#130664,#130665,
#130666,#130667,#130668,#130669,#130670,#130671,#130672,#130673,#130674,
#130675,#130676,#130677,#130678,#130679,#130680,#130681,#130682,#130683,
#130684,#130685,#130686,#130687,#130688,#130689,#130690,#130691,#130692,
#130693,#130694,#130695,#130696,#130697,#130698,#130699,#130700,#130701,
#130702,#130703,#130704,#130705,#130706,#130707,#130708,#130709,#130710,
#130711,#130712,#130713,#130714,#130715,#130716,#130717,#130718,#130719,
#130720,#130721,#130722,#130723,#130724,#130725,#130726,#130727,#130728,
#130729,#130730,#130731,#130732,#130733,#130734,#130735,#130736,#130737,
#130738,#130739,#130740,#130741,#130742,#130743,#130744,#130745,#130746,
#130747,#130748,#130749,#130750,#130751,#130752,#130753,#130754,#130755,
#130756,#130757,#130758,#130759,#130760,#130761,#130762,#130763,#130764,
#130765,#130766,#130767,#130768,#130769,#130770,#130771,#130772,#130773,
#130774,#130775,#130776,#130777,#130778,#130779,#130780,#130781,#130782,
#130783,#130784,#130785,#130786,#130787,#130788,#130789,#130790,#130791,
#130792,#130793,#130794,#130795,#130796,#130797,#130798,#130799,#130800,
#130801,#130802,#130803,#130804,#130805,#130806,#130807,#130808),
 .UNSPECIFIED.,.F.,.F.,(4,2,2,2,2,2,2,2,2,2,2,2,2,2,2,2,2,2,2,2,2,2,2,2,
2,2,2,2,2,2,2,2,2,2,2,2,2,2,2,2,2,2,2,2,2,2,2,2,2,2,2,2,2,2,2,2,2,2,2,2,
2,2,2,2,2,2,2,2,2,2,2,2,2,2,2,2,2,2,2,2,2,2,4),(-0.571051559787927,-0.569996074513531,
-0.565671843249809,-0.560366882428473,-0.546557663273505,-0.539600185118641,
-0.537343957564249,-0.535840305815804,-0.534121793565648,-0.530741555086234,
-0.52597114521168,-0.516700251387653,-0.506185232178122,-0.502125052067211,
-0.499691568810702,-0.497019310272292,-0.493138314866569,-0.479934522013935,
-0.466858149278131,-0.464241332196048,-0.46267224585702,-0.461069704528704,
-0.458287920534849,-0.448560877492757,-0.432407578658465,-0.428491638974536,
-0.425840043368729,-0.423093042035003,-0.418789852070253,-0.413521171611082,
-0.399948314192901,-0.392630366694188,-0.390395974064222,-0.388895616885867,
-0.387167291862575,-0.383733032148312,-0.378851404193333,-0.36974050271539,
-0.359259111648477,-0.355200859325038,-0.352767892745599,-0.350095750197438,
-0.346214024981766,-0.332971962391731,-0.319942484826,-0.317322171459366,
-0.315752530832435,-0.314151231754787,-0.311374776483078,-0.301695541193718,
-0.285456510792349,-0.281550740964732,-0.278900956782245,-0.276151817980632,
-0.271836284421581,-0.266546170902295,-0.252832762870907,-0.245771822322346,
-0.243505809537544,-0.24201514600845,-0.240306329955738,-0.236981179840528,
-0.232322911665265,-0.214495799010595,-0.209340260128373,-0.206410138371564,
-0.203802567318848,-0.200375304828084,-0.191486995531469,-0.181599018465889,
-0.172438193643578,-0.170117338375145,-0.168618564225245,-0.16693542441401,
-0.163738236452623,-0.149178611996683,-0.137871258862018,-0.13425969181125,
-0.131631584954883,-0.128790949103628,-0.123968675471476,-0.11535376263171,
-0.104760453105363),.UNSPECIFIED.);
#1674=B_SPLINE_CURVE_WITH_KNOTS('',3,(#130810,#130811,#130812,#130813,#130814,
#130815,#130816,#130817,#130818,#130819),.UNSPECIFIED.,.F.,.F.,(4,3,3,4),
(15.363686816277,15.5113772250708,15.6590677938146,15.7079632679489),
 .UNSPECIFIED.);
#1675=B_SPLINE_CURVE_WITH_KNOTS('',3,(#130820,#130821,#130822,#130823,#130824,
#130825,#130826,#130827,#130828,#130829,#130830,#130831,#130832,#130833,
#130834,#130835,#130836,#130837,#130838,#130839,#130840,#130841,#130842,
#130843,#130844,#130845,#130846,#130847,#130848,#130849,#130850,#130851,
#130852,#130853,#130854,#130855,#130856,#130857,#130858,#130859,#130860,
#130861,#130862,#130863,#130864,#130865,#130866,#130867,#130868,#130869,
#130870,#130871,#130872,#130873,#130874,#130875,#130876,#130877,#130878,
#130879,#130880,#130881,#130882,#130883,#130884,#130885,#130886,#130887,
#130888,#130889,#130890,#130891,#130892,#130893,#130894,#130895,#130896,
#130897,#130898,#130899,#130900,#130901,#130902,#130903,#130904,#130905,
#130906,#130907,#130908,#130909,#130910,#130911,#130912,#130913,#130914,
#130915,#130916,#130917,#130918,#130919,#130920,#130921,#130922,#130923,
#130924,#130925,#130926,#130927,#130928,#130929,#130930,#130931,#130932,
#130933,#130934,#130935,#130936,#130937,#130938,#130939,#130940,#130941,
#130942,#130943,#130944,#130945,#130946,#130947,#130948,#130949,#130950,
#130951,#130952,#130953,#130954,#130955,#130956,#130957,#130958,#130959,
#130960,#130961,#130962,#130963,#130964,#130965,#130966,#130967,#130968,
#130969,#130970,#130971,#130972,#130973,#130974,#130975,#130976,#130977,
#130978,#130979,#130980,#130981,#130982,#130983,#130984,#130985,#130986,
#130987,#130988,#130989,#130990,#130991,#130992,#130993,#130994,#130995,
#130996,#130997,#130998,#130999,#131000,#131001,#131002,#131003),
 .UNSPECIFIED.,.F.,.F.,(4,3,3,3,3,3,3,3,3,3,3,3,3,3,3,3,3,3,3,3,3,3,3,3,
3,3,3,3,3,3,3,3,3,3,3,3,3,3,3,3,3,3,3,3,3,3,3,3,3,3,3,3,3,3,3,3,3,3,3,3,
3,4),(15.7079658912085,15.8280867104848,15.841693727571,15.9752153053394,
16.1086061050242,16.2433728485283,16.3768229870163,16.5122480330283,16.6373080334116,
16.6476730790403,16.6477295647726,16.7700944172117,16.7825272094377,16.9171733070631,
17.0516855888283,17.1861379983219,17.320704100207,17.4553370592189,17.5902314444273,
17.6362783642661,17.6363374995076,17.7582188619054,17.7707526904591,17.9050109173946,
18.0391283118763,18.1731798518975,18.3073399651891,18.4415634786314,18.5760484224978,
18.6248836494918,18.6249438490354,18.7468947738374,18.7595538646593,18.8940108554107,
19.0283293656656,19.1625838565757,19.296947748702,19.4313757768995,19.5660637510641,
19.6134889347175,19.6135478246836,19.7355858153476,19.7481484855373,19.882595273636,
20.0169040688695,20.1511493591163,20.2855049097021,20.4199250839303,20.5546060391902,
20.6020942199433,20.6021535687792,20.7241240926645,20.7367081159257,20.8711082220163,
21.0053694336211,21.1395663621798,21.2738728468049,21.4082434871058,21.5428748325272,
21.590699505169,21.5907589398938,21.647807050148),.UNSPECIFIED.);
#1676=B_SPLINE_CURVE_WITH_KNOTS('',3,(#131008,#131009,#131010,#131011,#131012,
#131013,#131014,#131015,#131016,#131017,#131018,#131019,#131020,#131021,
#131022,#131023,#131024,#131025,#131026,#131027,#131028,#131029,#131030,
#131031,#131032,#131033,#131034,#131035,#131036,#131037,#131038,#131039,
#131040,#131041,#131042,#131043,#131044,#131045,#131046,#131047,#131048,
#131049,#131050,#131051,#131052,#131053,#131054,#131055,#131056,#131057,
#131058,#131059,#131060,#131061,#131062,#131063,#131064,#131065,#131066,
#131067,#131068,#131069,#131070,#131071,#131072,#131073,#131074,#131075,
#131076,#131077,#131078,#131079,#131080,#131081,#131082,#131083,#131084,
#131085,#131086,#131087,#131088,#131089,#131090,#131091,#131092,#131093,
#131094,#131095,#131096,#131097,#131098,#131099,#131100,#131101,#131102,
#131103,#131104,#131105,#131106,#131107,#131108,#131109,#131110,#131111,
#131112,#131113,#131114,#131115,#131116,#131117,#131118,#131119,#131120,
#131121,#131122,#131123,#131124,#131125,#131126,#131127,#131128,#131129,
#131130,#131131,#131132,#131133,#131134,#131135,#131136,#131137,#131138,
#131139,#131140,#131141,#131142,#131143,#131144,#131145,#131146,#131147,
#131148,#131149,#131150,#131151,#131152,#131153,#131154,#131155,#131156,
#131157,#131158,#131159,#131160,#131161,#131162,#131163,#131164,#131165,
#131166,#131167,#131168,#131169,#131170,#131171,#131172,#131173,#131174,
#131175,#131176,#131177),.UNSPECIFIED.,.F.,.F.,(4,2,2,2,2,2,2,2,2,2,2,2,
2,2,2,2,2,2,2,2,2,2,2,2,2,2,2,2,2,2,2,2,2,2,2,2,2,2,2,2,2,2,2,2,2,2,2,2,
2,2,2,2,2,2,2,2,2,2,2,2,2,2,2,2,2,2,2,2,2,2,2,2,2,2,2,2,2,2,2,2,2,2,2,2,
4),(-1.03737585849936,-1.03227715523834,-1.02055288568758,-1.01644245472727,
-1.01373014153861,-1.01101680205915,-1.00690071747753,-0.994352282923678,
-0.984960736685868,-0.979882995409455,-0.978055814838689,-0.976563310812306,
-0.974805636634147,-0.971209682499858,-0.968429728397085,-0.957358599118677,
-0.945986508622834,-0.942371710140109,-0.939740803116181,-0.936896475627927,
-0.93206541560142,-0.925852120427952,-0.911239208908094,-0.906349691192717,
-0.90454776998583,-0.903059577463341,-0.901282804672542,-0.897577850157911,
-0.894672795136712,-0.882616161424283,-0.872445605120101,-0.868861969007884,
-0.866235418606352,-0.863378884640084,-0.858481184427325,-0.852142709930726,
-0.841290600394485,-0.83351811880258,-0.831243867809716,-0.829752134058528,
-0.828047921811842,-0.824745065367215,-0.822287816452621,-0.813387806769867,
-0.800191053957259,-0.796067738610522,-0.793353303175773,-0.790642555968347,
-0.786540028749658,-0.774878025917806,-0.760452124872451,-0.757980751988692,
-0.75659151167371,-0.755004723175957,-0.752300595641114,-0.743260406000457,
-0.725911196617614,-0.722156862002156,-0.719531349865557,-0.716741732065363,
-0.712206885972953,-0.709173042576224,-0.699616774568612,-0.687345091061038,
-0.684681469399271,-0.683102961308723,-0.681510893710357,-0.678780676240484,
-0.669514983211609,-0.652570346897138,-0.648759312230262,-0.646124914429003,
-0.643351560271103,-0.638904643213751,-0.626777927393997,-0.613798447382564,
-0.611174271553658,-0.609603710601596,-0.608002994647919,-0.605229896782282,
-0.595581753162721,-0.579294642172542,-0.575395519728214,-0.572746825441744,
-0.571051559787927),.UNSPECIFIED.);
#1677=B_SPLINE_CURVE_WITH_KNOTS('',3,(#131179,#131180,#131181,#131182,#131183,
#131184,#131185,#131186,#131187,#131188,#131189,#131190,#131191),
 .UNSPECIFIED.,.F.,.F.,(4,3,3,3,4),(21.6478070511627,21.7809366960148,21.796403000268,
21.9440994851842,21.9911485738921),.UNSPECIFIED.);
#1678=B_SPLINE_CURVE_WITH_KNOTS('',3,(#131192,#131193,#131194,#131195,#131196,
#131197,#131198,#131199,#131200,#131201,#131202,#131203,#131204,#131205,
#131206,#131207,#131208,#131209,#131210,#131211,#131212,#131213,#131214,
#131215,#131216,#131217,#131218,#131219,#131220,#131221,#131222,#131223,
#131224,#131225,#131226,#131227,#131228,#131229,#131230,#131231,#131232,
#131233,#131234,#131235,#131236,#131237,#131238,#131239,#131240,#131241,
#131242,#131243,#131244,#131245,#131246,#131247,#131248,#131249,#131250,
#131251,#131252,#131253,#131254,#131255,#131256,#131257,#131258,#131259,
#131260,#131261,#131262,#131263,#131264,#131265,#131266,#131267,#131268,
#131269,#131270,#131271,#131272,#131273,#131274,#131275,#131276,#131277,
#131278,#131279,#131280,#131281,#131282,#131283,#131284,#131285,#131286,
#131287,#131288,#131289,#131290,#131291,#131292,#131293,#131294,#131295,
#131296,#131297,#131298,#131299,#131300,#131301,#131302,#131303,#131304,
#131305,#131306,#131307,#131308,#131309,#131310,#131311,#131312,#131313,
#131314,#131315,#131316,#131317,#131318,#131319,#131320,#131321,#131322,
#131323,#131324,#131325,#131326,#131327,#131328,#131329,#131330,#131331,
#131332,#131333,#131334,#131335,#131336,#131337,#131338,#131339,#131340,
#131341,#131342,#131343,#131344,#131345,#131346,#131347,#131348,#131349,
#131350,#131351,#131352,#131353,#131354,#131355,#131356,#131357,#131358,
#131359,#131360,#131361,#131362,#131363,#131364,#131365,#131366,#131367,
#131368,#131369,#131370,#131371,#131372),.UNSPECIFIED.,.F.,.F.,(4,3,3,3,
3,3,3,3,3,3,3,3,3,3,3,3,3,3,3,3,3,3,3,3,3,3,3,3,3,3,3,3,3,3,3,3,3,3,3,3,
3,3,3,3,3,3,3,3,3,3,3,3,3,3,3,3,3,3,3,3,4),(21.9911485751285,22.1273195269264,
22.2636884434382,22.4001715837155,22.5369664127769,22.5793047903947,22.579364055752,
22.7013589250348,22.7139431476743,22.84836818408,22.9826547283351,23.1168773261226,
23.2512097396333,23.3856064910885,23.5202638907055,23.5679100756204,23.5679694139317,
23.6899550950555,23.7025432222845,23.8369629207288,23.9712440140535,24.105461062073,
24.2397878306671,24.3741788751869,24.5088305468898,24.5565153608462,24.5565747025817,
24.6785631409001,24.6911525273435,24.8255763143162,24.9598615539257,25.0940827951838,
25.2284137873522,25.3628090781897,25.4974649765261,25.5451206460719,25.545179966661,
25.667169268505,25.6797569161559,25.8141798014757,25.9484641365813,26.0826844728612,
26.2170145679853,26.3514089652749,26.4860639866976,26.5337259312976,26.5337852629189,
26.6557733512449,26.6683616485685,26.8027839659363,26.9370677194846,27.0712874621066,
27.2056169511046,27.3400107343051,27.4746651374359,27.5223312165234,27.5223905474788,
27.6433095975991,27.6553377119416,27.7930166516017,27.9306954395165),
 .UNSPECIFIED.);
#1679=B_SPLINE_CURVE_WITH_KNOTS('',3,(#131377,#131378,#131379,#131380,#131381,
#131382,#131383,#131384,#131385,#131386,#131387,#131388,#131389,#131390,
#131391,#131392,#131393,#131394,#131395,#131396,#131397,#131398,#131399,
#131400,#131401,#131402,#131403,#131404,#131405,#131406,#131407,#131408,
#131409,#131410,#131411,#131412,#131413,#131414,#131415,#131416,#131417,
#131418,#131419,#131420,#131421,#131422,#131423,#131424,#131425,#131426,
#131427,#131428,#131429,#131430,#131431,#131432,#131433,#131434,#131435,
#131436,#131437,#131438,#131439,#131440,#131441,#131442,#131443,#131444,
#131445,#131446,#131447,#131448,#131449,#131450,#131451,#131452,#131453,
#131454,#131455,#131456,#131457,#131458,#131459,#131460,#131461,#131462,
#131463,#131464,#131465,#131466,#131467,#131468,#131469,#131470,#131471,
#131472,#131473,#131474,#131475,#131476,#131477,#131478,#131479,#131480,
#131481,#131482,#131483,#131484,#131485,#131486,#131487,#131488,#131489,
#131490,#131491,#131492,#131493,#131494,#131495,#131496,#131497,#131498,
#131499,#131500,#131501,#131502,#131503,#131504,#131505,#131506,#131507,
#131508,#131509,#131510,#131511,#131512,#131513,#131514,#131515,#131516,
#131517,#131518,#131519,#131520,#131521,#131522,#131523,#131524,#131525,
#131526,#131527,#131528,#131529,#131530,#131531,#131532,#131533,#131534,
#131535,#131536,#131537,#131538,#131539,#131540,#131541,#131542,#131543,
#131544),.UNSPECIFIED.,.F.,.F.,(4,2,2,2,2,2,2,2,2,2,2,2,2,2,2,2,2,2,2,2,
2,2,2,2,2,2,2,2,2,2,2,2,2,2,2,2,2,2,2,2,2,2,2,2,2,2,2,2,2,2,2,2,2,2,2,2,
2,2,2,2,2,2,2,2,2,2,2,2,2,2,2,2,2,2,2,2,2,2,2,2,2,2,2,4),(-1.50364802285674,
-1.49545071073367,-1.49277784300415,-1.4911978096781,-1.48960844249668,
-1.4868897810579,-1.47496652604162,-1.46527405764246,-1.46221455472017,
-1.45765323723645,-1.45485936435662,-1.45223726314951,-1.44850103989386,
-1.43101940449241,-1.42204514007086,-1.41934910384597,-1.41776429307554,
-1.41637445893584,-1.41389802865572,-1.39954388678771,-1.3878576775268,
-1.38375301096247,-1.38104241125083,-1.37832923362657,-1.37421021101463,
-1.36048348501126,-1.35193918668256,-1.34852985676151,-1.34586995600447,
-1.34429248030542,-1.3427002150785,-1.3399675995032,-1.33063809196475,-1.31923800992053,
-1.31222954640053,-1.30902851719769,-1.30646340046811,-1.3033929521827,
-1.29725354033603,-1.28069048066722,-1.2761366571879,-1.27286413065123,
-1.2711658310835,-1.2696722879819,-1.26738524150891,-1.25930306649972,-1.2497418103615,
-1.23966884281241,-1.23613871611966,-1.23351969791668,-1.23064140754522,
-1.22562232784468,-1.20746943500652,-1.20278305642826,-1.19944442040429,
-1.19773360345223,-1.1962442974679,-1.1939857412558,-1.18645885958552,-1.17309565971293,
-1.16786154210746,-1.1635780667853,-1.16083471353968,-1.15818053209682,
-1.15424909030975,-1.13819563253312,-1.12839218039528,-1.12560185975233,
-1.12399763961541,-1.12242998135255,-1.11982066605514,-1.10534886412797,
-1.09505387622202,-1.09042292870394,-1.08761552173897,-1.0849690255242,
-1.08124896820758,-1.06363989104472,-1.0547287558928,-1.05203963558377,
-1.05045587143454,-1.04906446764604,-1.04658085487128,-1.03737585849936),
 .UNSPECIFIED.);
#1680=B_SPLINE_CURVE_WITH_KNOTS('',3,(#131546,#131547,#131548,#131549,#131550,
#131551,#131552,#131553,#131554,#131555,#131556,#131557),.UNSPECIFIED.,
 .F.,.F.,(4,2,2,2,2,4),(-0.025563779166194,-0.0218566744148999,-0.019367166493461,
-0.0166535805597176,-0.0127752645799051,-2.12926712384545E-6),
 .UNSPECIFIED.);
#1681=B_SPLINE_CURVE_WITH_KNOTS('',3,(#131558,#131559,#131560,#131561,#131562,
#131563,#131564,#131565,#131566,#131567,#131568,#131569,#131570,#131571,
#131572,#131573,#131574,#131575,#131576,#131577,#131578,#131579,#131580,
#131581,#131582,#131583,#131584,#131585,#131586,#131587,#131588,#131589,
#131590,#131591,#131592,#131593,#131594,#131595,#131596,#131597,#131598,
#131599,#131600,#131601,#131602,#131603,#131604,#131605,#131606,#131607,
#131608,#131609,#131610,#131611,#131612,#131613,#131614,#131615,#131616,
#131617,#131618,#131619,#131620,#131621,#131622,#131623,#131624,#131625,
#131626,#131627,#131628,#131629,#131630,#131631,#131632,#131633,#131634,
#131635,#131636,#131637,#131638,#131639,#131640,#131641,#131642,#131643,
#131644,#131645,#131646,#131647,#131648,#131649,#131650,#131651,#131652,
#131653,#131654,#131655,#131656,#131657,#131658,#131659,#131660,#131661,
#131662,#131663,#131664,#131665,#131666,#131667,#131668,#131669,#131670,
#131671,#131672,#131673,#131674,#131675,#131676,#131677,#131678,#131679,
#131680,#131681,#131682,#131683,#131684,#131685,#131686,#131687,#131688,
#131689,#131690,#131691,#131692,#131693,#131694,#131695,#131696,#131697,
#131698,#131699,#131700,#131701,#131702,#131703,#131704,#131705,#131706,
#131707,#131708,#131709,#131710,#131711,#131712,#131713,#131714,#131715,
#131716,#131717,#131718,#131719,#131720,#131721,#131722,#131723,#131724,
#131725,#131726,#131727,#131728,#131729,#131730,#131731,#131732,#131733,
#131734,#131735,#131736,#131737,#131738,#131739,#131740,#131741),
 .UNSPECIFIED.,.F.,.F.,(4,3,3,3,3,3,3,3,3,3,3,3,3,3,3,3,3,3,3,3,3,3,3,3,
3,3,3,3,3,3,3,3,3,3,3,3,3,3,3,3,3,3,3,3,3,3,3,3,3,3,3,3,3,3,3,3,3,3,3,3,
3,4),(28.2743338967306,28.4080562857905,28.450661125029,28.5109365017491,
28.5109958301788,28.6329844373678,28.6455726033673,28.7799953133922,28.9142794668526,
29.0484996156028,29.1828295161676,29.3172237145886,29.4518785331719,29.4995417869748,
29.4996011170081,29.6215895690841,29.634177836647,29.7686004930229,29.902884591277,
30.0371046834058,30.1714345257688,30.3058286650014,30.4404834236609,30.4881470722005,
30.4882064019962,30.6101949254426,30.6227831943049,30.757205924499,30.8914900977593,
31.0257102658872,31.1600401850117,31.2944344015414,31.429089237323,31.4767523574263,
31.4768116869338,31.5988002109329,31.6113884523335,31.7458111549967,31.8800953004658,
32.0143154406149,32.1486453317464,32.2830395202408,32.4176943282795,32.465357642652,
32.4654169723847,32.5874054772536,32.5999937338323,32.7344164325919,32.8687005739914,
33.0029207099153,33.1372505966289,33.2716447805881,33.4062995839727,33.4539629278777,
33.4540222575592,33.5760115235183,33.5886145888915,33.7230418399154,33.8573515080313,
33.9915876646927,34.1259133197487,34.2133098071407),.UNSPECIFIED.);
#1682=B_SPLINE_CURVE_WITH_KNOTS('',3,(#131746,#131747,#131748,#131749,#131750,
#131751,#131752,#131753,#131754,#131755,#131756,#131757,#131758,#131759,
#131760,#131761,#131762,#131763,#131764,#131765,#131766,#131767,#131768,
#131769,#131770,#131771,#131772,#131773,#131774,#131775,#131776,#131777,
#131778,#131779,#131780,#131781,#131782,#131783,#131784,#131785,#131786,
#131787,#131788,#131789,#131790,#131791,#131792,#131793,#131794,#131795,
#131796,#131797,#131798,#131799,#131800,#131801,#131802,#131803,#131804,
#131805,#131806,#131807,#131808,#131809,#131810,#131811,#131812,#131813,
#131814,#131815,#131816,#131817,#131818,#131819,#131820,#131821,#131822,
#131823,#131824,#131825,#131826,#131827,#131828,#131829,#131830,#131831,
#131832,#131833,#131834,#131835,#131836,#131837,#131838,#131839,#131840,
#131841,#131842,#131843,#131844,#131845,#131846,#131847,#131848,#131849,
#131850,#131851,#131852,#131853,#131854,#131855,#131856,#131857,#131858,
#131859,#131860,#131861,#131862,#131863,#131864,#131865,#131866,#131867,
#131868,#131869,#131870,#131871,#131872,#131873,#131874,#131875,#131876,
#131877,#131878,#131879,#131880,#131881,#131882,#131883,#131884,#131885,
#131886,#131887,#131888,#131889,#131890,#131891,#131892,#131893,#131894,
#131895,#131896,#131897,#131898,#131899,#131900,#131901,#131902,#131903,
#131904,#131905,#131906,#131907),.UNSPECIFIED.,.F.,.F.,(4,2,2,2,2,2,2,2,
2,2,2,2,2,2,2,2,2,2,2,2,2,2,2,2,2,2,2,2,2,2,2,2,2,2,2,2,2,2,2,2,2,2,2,2,
2,2,2,2,2,2,2,2,2,2,2,2,2,2,2,2,2,2,2,2,2,2,2,2,2,2,2,2,2,2,2,2,2,2,2,2,
4),(-1.96977677123554,-1.96786265403597,-1.96573321501472,-1.96167162230868,
-1.94590146179013,-1.93624742027908,-1.9334745428404,-1.93187453643428,
-1.9303051971168,-1.92768398226965,-1.91471533300402,-1.90557344281115,
-1.90262272335569,-1.89817551750715,-1.89540328859398,-1.8927707361987,
-1.8889638743168,-1.87199495010463,-1.86274083518687,-1.86001273426832,
-1.85842172337792,-1.85703669037491,-1.85458667364288,-1.84001187590523,
-1.82952706152445,-1.82490094155638,-1.82209559134509,-1.81945049171496,
-1.81573146694776,-1.79814113634482,-1.78923083908553,-1.78654279102156,
-1.78495986395928,-1.78356936486571,-1.78108766599658,-1.76678871844126,
-1.75507376823034,-1.75096608606115,-1.74825544400513,-1.74554367041334,
-1.7414297442648,-1.72755468915487,-1.71575230344817,-1.71308828805365,
-1.71151021381858,-1.70991931542362,-1.70719228954269,-1.6955058046255,
-1.682765676323,-1.67807983995417,-1.6752633309225,-1.67262312487704,-1.66893714685131,
-1.65111548551198,-1.6423288844496,-1.63965552390463,-1.63807550252748,
-1.63648647090955,-1.63376891181973,-1.62223508619449,-1.61229347065207,
-1.60772509028122,-1.60384174735595,-1.60116983478843,-1.59873784336122,
-1.59468322794104,-1.57980767462402,-1.56874828801468,-1.56615344533303,
-1.5645891350189,-1.56298240793629,-1.56017760053193,-1.54944854327282,
-1.53908352977955,-1.53589917031369,-1.53120962068263,-1.52839222095618,
-1.52575200079865,-1.52206738819631,-1.504231779604,-1.50364802285674),
 .UNSPECIFIED.);
#1683=B_SPLINE_CURVE_WITH_KNOTS('',3,(#131909,#131910,#131911,#131912,#131913,
#131914,#131915,#131916,#131917,#131918),.UNSPECIFIED.,.F.,.F.,(4,3,3,4),
(34.2133098076447,34.3479491574694,34.4425682131035,34.5575191894877),
 .UNSPECIFIED.);
#1684=B_SPLINE_CURVE_WITH_KNOTS('',3,(#131919,#131920,#131921,#131922,#131923,
#131924,#131925,#131926,#131927,#131928,#131929,#131930,#131931,#131932,
#131933,#131934,#131935,#131936,#131937,#131938,#131939,#131940,#131941,
#131942,#131943,#131944,#131945,#131946,#131947,#131948,#131949,#131950,
#131951,#131952,#131953,#131954,#131955,#131956,#131957,#131958,#131959,
#131960,#131961,#131962,#131963,#131964,#131965,#131966,#131967,#131968,
#131969,#131970,#131971,#131972,#131973,#131974,#131975,#131976,#131977,
#131978,#131979,#131980,#131981,#131982,#131983,#131984,#131985,#131986,
#131987,#131988,#131989,#131990,#131991,#131992,#131993,#131994,#131995,
#131996,#131997,#131998,#131999,#132000,#132001,#132002,#132003,#132004,
#132005,#132006,#132007,#132008,#132009,#132010,#132011,#132012,#132013,
#132014,#132015,#132016,#132017,#132018,#132019,#132020,#132021,#132022,
#132023,#132024,#132025,#132026,#132027,#132028,#132029,#132030,#132031,
#132032,#132033,#132034,#132035,#132036,#132037,#132038,#132039,#132040,
#132041,#132042,#132043,#132044,#132045,#132046,#132047,#132048,#132049,
#132050,#132051,#132052,#132053,#132054,#132055,#132056,#132057,#132058,
#132059,#132060,#132061,#132062,#132063,#132064,#132065,#132066,#132067,
#132068,#132069,#132070,#132071,#132072,#132073,#132074,#132075,#132076,
#132077,#132078,#132079,#132080,#132081,#132082,#132083,#132084,#132085,
#132086,#132087,#132088,#132089,#132090,#132091,#132092,#132093,#132094,
#132095,#132096),.UNSPECIFIED.,.F.,.F.,(4,3,3,3,3,3,3,3,3,3,3,3,3,3,3,3,
3,3,3,3,3,3,3,3,3,3,3,3,3,3,3,3,3,3,3,3,3,3,3,3,3,3,3,3,3,3,3,3,3,3,3,3,
3,3,3,3,3,3,3,4),(34.5575191904757,34.690284217135,34.8228676060756,34.9553479102442,
35.0879023753946,35.2204932902944,35.3533450541945,35.4311734983292,35.431232828011,
35.5532213403015,35.5658095944846,35.7002322983317,35.8345164449174,35.9687365861126,
36.1030664781748,36.2374606675342,36.3721154763276,36.4197787835549,36.4198381132273,
36.5418266270213,36.5544148808533,36.6888375858681,36.8231217336429,36.9573418760459,
37.0916717693317,37.2260659599253,37.3607207699536,37.4083840687806,37.4084433984502,
37.5304319119846,37.5430201654453,37.6774428698166,37.8117270169401,37.9459471586851,
38.0802770513101,38.2146712412402,38.3493260506096,38.3969893540064,38.3970486836801,
38.5190371970041,38.5316254507277,38.6660481551546,38.8003323023324,38.9345524441305,
39.0688823368061,39.2032765267856,39.3379313362016,39.3855946392321,39.3856539689042,
39.507642482419,39.5202307360884,39.6546534406534,39.788937587972,39.9231577299135,
40.0574876227346,40.191881812861,40.3265366224243,40.3741999244578,40.3742592541492,
40.4976061704439),.UNSPECIFIED.);
#1685=B_SPLINE_CURVE_WITH_KNOTS('',3,(#132101,#132102,#132103,#132104,#132105,
#132106,#132107,#132108,#132109,#132110,#132111,#132112,#132113,#132114,
#132115,#132116,#132117,#132118,#132119,#132120,#132121,#132122,#132123,
#132124,#132125,#132126,#132127,#132128,#132129,#132130,#132131,#132132,
#132133,#132134,#132135,#132136,#132137,#132138,#132139,#132140,#132141,
#132142,#132143,#132144,#132145,#132146,#132147,#132148,#132149,#132150,
#132151,#132152,#132153,#132154,#132155,#132156,#132157,#132158,#132159,
#132160,#132161,#132162,#132163,#132164,#132165,#132166,#132167,#132168,
#132169,#132170,#132171,#132172,#132173,#132174,#132175,#132176,#132177,
#132178,#132179,#132180,#132181,#132182,#132183,#132184,#132185,#132186,
#132187,#132188,#132189,#132190,#132191,#132192,#132193,#132194,#132195,
#132196,#132197,#132198,#132199,#132200,#132201,#132202,#132203,#132204,
#132205,#132206,#132207,#132208,#132209,#132210,#132211,#132212,#132213,
#132214,#132215,#132216,#132217,#132218,#132219,#132220,#132221,#132222,
#132223,#132224,#132225,#132226,#132227,#132228,#132229,#132230,#132231,
#132232,#132233,#132234,#132235,#132236,#132237,#132238,#132239,#132240,
#132241,#132242,#132243,#132244,#132245,#132246,#132247,#132248,#132249,
#132250,#132251,#132252,#132253,#132254,#132255,#132256,#132257,#132258,
#132259,#132260,#132261,#132262,#132263,#132264,#132265,#132266,#132267,
#132268),.UNSPECIFIED.,.F.,.F.,(4,2,2,2,2,2,2,2,2,2,2,2,2,2,2,2,2,2,2,2,
2,2,2,2,2,2,2,2,2,2,2,2,2,2,2,2,2,2,2,2,2,2,2,2,2,2,2,2,2,2,2,2,2,2,2,2,
2,2,2,2,2,2,2,2,2,2,2,2,2,2,2,2,2,2,2,2,2,2,2,2,2,2,2,4),(-0.466250456168778,
-0.462515734984742,-0.445730588883325,-0.441898784801489,-0.439261464619427,
-0.43649446551622,-0.432079883083639,-0.426617785213962,-0.411695311933343,
-0.405884200717412,-0.403766921177319,-0.402281904470734,-0.400491247456053,
-0.396703695157635,-0.393701511144969,-0.380802676507036,-0.379744070127349,
-0.37136004070281,-0.367951421616744,-0.365340143971343,-0.362433691182018,
-0.357257584904554,-0.345128280789277,-0.333639195686409,-0.330926536843941,
-0.329338295715798,-0.327756807175644,-0.325077505150332,-0.31624332656241,
-0.298525090081188,-0.294825365477072,-0.292182588200003,-0.289369692793726,
-0.284706163347405,-0.276161052143204,-0.260748214669335,-0.257709982467129,
-0.256056670720635,-0.254524067949552,-0.252096151517043,-0.249084719319112,
-0.242262141963782,-0.225319450037713,-0.221509134334388,-0.218875198296874,
-0.216102303772512,-0.21165606666655,-0.208706575661511,-0.199574142657068,
-0.18655181532208,-0.183931374029539,-0.18236174835175,-0.180760550509001,
-0.177984215355451,-0.168303944602996,-0.152076235965933,-0.148170541648297,
-0.145521082761926,-0.142772488508383,-0.138458287329498,-0.133170235914728,
-0.119468269465196,-0.112395851094886,-0.110129322150004,-0.108639050841957,
-0.106932174794059,-0.103613666894035,-0.0989681538229891,-0.0813009273757189,
-0.0760333798490178,-0.0730831562979099,-0.070480979211169,-0.0670945711654487,
-0.0585896908869579,-0.0402179526002847,-0.0372703646728362,-0.0356348908774732,
-0.0340912886790107,-0.0316043810609119,-0.0284936180620519,-0.0165415942135776,
-0.00491281277194659,-0.00217218770564259,-9.99999999529155E-7),
 .UNSPECIFIED.);
#1686=B_SPLINE_CURVE_WITH_KNOTS('',3,(#132270,#132271,#132272,#132273,#132274,
#132275,#132276,#132277,#132278,#132279),.UNSPECIFIED.,.F.,.F.,(4,2,2,2,
4),(-0.0255223692981158,-0.0128002959747665,-0.00436963811408314,-0.00196112391871313,
-3.26435750072084E-5),.UNSPECIFIED.);
#1687=B_SPLINE_CURVE_WITH_KNOTS('',3,(#132280,#132281,#132282,#132283,#132284,
#132285,#132286,#132287,#132288,#132289,#132290,#132291,#132292,#132293,
#132294,#132295,#132296,#132297,#132298,#132299,#132300,#132301,#132302,
#132303,#132304,#132305,#132306,#132307,#132308,#132309,#132310,#132311,
#132312,#132313,#132314,#132315,#132316,#132317,#132318,#132319,#132320,
#132321,#132322,#132323,#132324,#132325,#132326,#132327,#132328,#132329,
#132330,#132331,#132332,#132333,#132334,#132335,#132336,#132337,#132338,
#132339,#132340,#132341,#132342,#132343,#132344,#132345,#132346,#132347,
#132348,#132349,#132350,#132351,#132352,#132353,#132354,#132355,#132356,
#132357,#132358,#132359,#132360,#132361,#132362,#132363,#132364,#132365,
#132366,#132367,#132368,#132369,#132370,#132371,#132372,#132373,#132374,
#132375,#132376,#132377,#132378,#132379,#132380,#132381,#132382,#132383,
#132384,#132385,#132386,#132387,#132388,#132389,#132390,#132391,#132392,
#132393,#132394,#132395,#132396,#132397,#132398,#132399,#132400,#132401,
#132402,#132403,#132404,#132405,#132406,#132407,#132408,#132409,#132410,
#132411,#132412,#132413,#132414,#132415,#132416,#132417,#132418,#132419,
#132420,#132421,#132422,#132423,#132424,#132425,#132426,#132427,#132428,
#132429,#132430,#132431,#132432,#132433,#132434,#132435,#132436,#132437,
#132438,#132439,#132440,#132441,#132442,#132443,#132444,#132445,#132446,
#132447,#132448,#132449,#132450,#132451,#132452,#132453,#132454,#132455,
#132456,#132457,#132458,#132459,#132460),.UNSPECIFIED.,.F.,.F.,(4,3,3,3,
3,3,3,3,3,3,3,3,3,3,3,3,3,3,3,3,3,3,3,3,3,3,3,3,3,3,3,3,3,3,3,3,3,3,3,3,
3,3,3,3,3,3,3,3,3,3,3,3,3,3,3,3,3,3,3,3,4),(40.8407044966673,40.9798570562274,
41.1191799295957,41.2589299159688,41.3628052096836,41.3628645393561,41.484853052794,
41.4974413064647,41.631864010953,41.7661481581936,41.9003683000561,42.0346981927973,
42.1690923828433,42.3037471923262,42.3514104949093,42.3514698245815,42.4734583380527,
42.4860465917054,42.6204692962091,42.7547534434654,42.8889735853438,43.0233034781013,
43.1576976681637,43.2923524776632,43.340015780135,43.3400751098072,43.4620636232768,
43.4746518769183,43.6090745814091,43.7433587286522,43.8775788705174,44.0119087632615,
44.1463029533105,44.2809577627967,44.3286210653607,44.328680395033,44.4506689084891,
44.4632571621475,44.5976798666417,44.7319640138885,44.8661841557573,45.0005140485049,
45.1349082385574,45.2695630480469,45.3172263505865,45.3172856802588,45.4392741937587,
45.4518624473747,45.5862851518703,45.7205692991184,45.8547894409887,45.9891193337378,
46.1235135237919,46.258168333283,46.3058316358122,46.305890965474,46.4265984044318,
46.4384912255247,46.570943162863,46.7032833103682,46.779979472002),
 .UNSPECIFIED.);
#1688=B_SPLINE_CURVE_WITH_KNOTS('',3,(#132465,#132466,#132467,#132468,#132469,
#132470,#132471,#132472,#132473,#132474,#132475,#132476,#132477,#132478,
#132479,#132480,#132481,#132482,#132483,#132484,#132485,#132486,#132487,
#132488,#132489,#132490,#132491,#132492,#132493,#132494,#132495,#132496,
#132497,#132498,#132499,#132500,#132501,#132502,#132503,#132504,#132505,
#132506,#132507,#132508,#132509,#132510,#132511,#132512,#132513,#132514,
#132515,#132516,#132517,#132518,#132519,#132520,#132521,#132522,#132523,
#132524,#132525,#132526,#132527,#132528,#132529,#132530,#132531,#132532,
#132533,#132534,#132535,#132536,#132537,#132538,#132539,#132540,#132541,
#132542,#132543,#132544,#132545,#132546,#132547,#132548,#132549,#132550,
#132551,#132552,#132553,#132554,#132555,#132556,#132557,#132558,#132559,
#132560,#132561,#132562,#132563,#132564,#132565,#132566,#132567,#132568,
#132569,#132570,#132571,#132572,#132573,#132574,#132575,#132576,#132577,
#132578,#132579,#132580,#132581,#132582,#132583,#132584,#132585,#132586,
#132587,#132588,#132589,#132590,#132591,#132592,#132593,#132594,#132595,
#132596,#132597,#132598,#132599,#132600,#132601,#132602,#132603,#132604,
#132605,#132606,#132607,#132608,#132609,#132610,#132611,#132612,#132613,
#132614,#132615,#132616,#132617,#132618,#132619,#132620,#132621,#132622,
#132623,#132624,#132625,#132626,#132627,#132628,#132629,#132630,#132631,
#132632,#132633,#132634,#132635,#132636,#132637,#132638,#132639,#132640,
#132641,#132642),.UNSPECIFIED.,.F.,.F.,(4,2,2,2,2,2,2,2,2,2,2,2,2,2,2,2,
2,2,2,2,2,2,2,2,2,2,2,2,2,2,2,2,2,2,2,2,2,2,2,2,2,2,2,2,2,2,2,2,2,2,2,2,
2,2,2,2,2,2,2,2,2,2,2,2,2,2,2,2,2,2,2,2,2,2,2,2,2,2,2,2,2,2,2,2,2,2,2,2,
4),(-0.932467505666577,-0.921105747935325,-0.918464980990969,-0.916891263094845,
-0.915294612522539,-0.912540842579777,-0.903064502647796,-0.886491646128297,
-0.882630982376248,-0.879988922634601,-0.877229281849085,-0.872854982099366,
-0.867463089462418,-0.853055583516473,-0.846697212077067,-0.844528271891396,
-0.843037087162468,-0.841276045079259,-0.837659360607389,-0.834855485147031,
-0.823600553081565,-0.812466175294876,-0.808856495507244,-0.806226872714595,
-0.803381701482514,-0.798543225423195,-0.792315325976461,-0.777298511925181,
-0.772795788772797,-0.770841792240485,-0.769366823470256,-0.767483541907558,
-0.763119274852211,-0.756073949260172,-0.739626403985499,-0.735749220046827,
-0.733104484132722,-0.73034902637389,-0.725997334849761,-0.720644589936917,
-0.706509928809678,-0.699835539441193,-0.697648939116865,-0.696155466876677,
-0.694403840692854,-0.690840123623823,-0.685686308592639,-0.674754887130896,
-0.673290579482916,-0.665107060942649,-0.661718394897937,-0.659109506933057,
-0.656192603968386,-0.650958090906618,-0.647216733962562,-0.633123187275598,
-0.626403632275417,-0.624213135146824,-0.622719145109942,-0.620969547162416,
-0.617417166601867,-0.612287486355764,-0.601502005492716,-0.598569062292694,
-0.591338513711225,-0.588035249109525,-0.585440142582493,-0.58243727314326,
-0.57670842578075,-0.568669641253922,-0.554851921879872,-0.551644034815975,
-0.549957970928539,-0.548441872440278,-0.546107790659626,-0.536329351228345,
-0.519020815879315,-0.515261921928018,-0.512636098585077,-0.509848593466414,
-0.505323137240049,-0.502298051767117,-0.492785537236905,-0.480432238417921,
-0.477778735574285,-0.476202475660992,-0.474608669237597,-0.471868825860901,
-0.466250456168778),.UNSPECIFIED.);
#1689=B_SPLINE_CURVE_WITH_KNOTS('',3,(#132644,#132645,#132646,#132647,#132648,
#132649,#132650,#132651,#132652,#132653,#132654,#132655),.UNSPECIFIED.,
 .F.,.F.,(4,2,2,2,2,4),(-0.0255688444182446,-0.0240999659624579,-0.0225373436534429,
-0.019468758913173,-0.0127753173615656,-1.29626833824403E-5),
 .UNSPECIFIED.);
#1690=B_SPLINE_CURVE_WITH_KNOTS('',3,(#132656,#132657,#132658,#132659,#132660,
#132661,#132662,#132663,#132664,#132665,#132666,#132667,#132668,#132669,
#132670,#132671,#132672,#132673,#132674,#132675,#132676,#132677,#132678,
#132679,#132680,#132681,#132682,#132683,#132684,#132685,#132686,#132687,
#132688,#132689,#132690,#132691,#132692,#132693,#132694,#132695,#132696,
#132697,#132698,#132699,#132700,#132701,#132702,#132703,#132704,#132705,
#132706,#132707,#132708,#132709,#132710,#132711,#132712,#132713,#132714,
#132715,#132716,#132717,#132718,#132719,#132720,#132721,#132722,#132723,
#132724,#132725,#132726,#132727,#132728,#132729,#132730,#132731,#132732,
#132733,#132734,#132735,#132736,#132737,#132738,#132739,#132740,#132741,
#132742,#132743,#132744,#132745,#132746,#132747,#132748,#132749,#132750,
#132751,#132752,#132753,#132754,#132755,#132756,#132757,#132758,#132759,
#132760,#132761,#132762,#132763,#132764,#132765,#132766,#132767,#132768,
#132769,#132770,#132771,#132772,#132773,#132774,#132775,#132776,#132777,
#132778,#132779,#132780,#132781,#132782,#132783,#132784,#132785,#132786,
#132787,#132788,#132789,#132790,#132791,#132792,#132793,#132794,#132795,
#132796,#132797,#132798,#132799,#132800,#132801,#132802,#132803,#132804,
#132805,#132806,#132807,#132808,#132809,#132810,#132811,#132812,#132813,
#132814,#132815,#132816,#132817,#132818,#132819,#132820,#132821,#132822,
#132823,#132824,#132825,#132826,#132827,#132828,#132829,#132830,#132831,
#132832,#132833,#132834,#132835,#132836,#132837,#132838,#132839),
 .UNSPECIFIED.,.F.,.F.,(4,3,3,3,3,3,3,3,3,3,3,3,3,3,3,3,3,3,3,3,3,3,3,3,
3,3,3,3,3,3,3,3,3,3,3,3,3,3,3,3,3,3,3,3,3,3,3,3,3,3,3,3,3,3,3,3,3,3,3,3,
3,4),(47.1238898038469,47.2554184151012,47.2944369210379,47.2944962507101,
47.4164847641539,47.4290730178261,47.5634957223218,47.69777986957,47.8320000114401,
47.9663299041892,48.1007240942431,48.2353789037341,48.2830422062637,48.283101535936,
48.4050900493903,48.4176783030504,48.5521010075445,48.6863851547912,48.8206052966598,
48.9549351894075,49.08932937946,49.2239841889496,49.2716474914894,49.2717068211617,
49.3936953346274,49.4062835882727,49.5407062927633,49.6749904400066,49.8092105818717,
49.9435404746159,50.0779346646649,50.212589474151,50.2602527767151,50.2603121063873,
50.382300619854,50.3948888735117,50.5293115780158,50.6635957252724,50.7978158671509,
50.9321457599082,51.0665399499703,51.2011947594692,51.2488580619408,51.248917391613,
51.3709059050861,51.383494158721,51.5179168632087,51.6522010104491,51.7864211523116,
51.9207510450532,52.0551452350999,52.1898000445839,52.2374633471666,52.2375226768391,
52.359511650272,52.3721089837709,52.5065333880661,52.6456211692066,52.7798775652825,
52.914130819089,53.0485201510646,53.0628845114798),.UNSPECIFIED.);
#1691=B_SPLINE_CURVE_WITH_KNOTS('',3,(#132844,#132845,#132846,#132847,#132848,
#132849,#132850,#132851,#132852,#132853,#132854,#132855,#132856,#132857,
#132858,#132859,#132860,#132861,#132862,#132863,#132864,#132865,#132866,
#132867,#132868,#132869,#132870,#132871,#132872,#132873,#132874,#132875,
#132876,#132877,#132878,#132879,#132880,#132881,#132882,#132883,#132884,
#132885,#132886,#132887,#132888,#132889,#132890,#132891,#132892,#132893,
#132894,#132895,#132896,#132897,#132898,#132899,#132900,#132901,#132902,
#132903,#132904,#132905,#132906,#132907,#132908,#132909,#132910,#132911,
#132912,#132913,#132914,#132915,#132916,#132917,#132918,#132919,#132920,
#132921,#132922,#132923,#132924,#132925,#132926,#132927,#132928,#132929,
#132930,#132931,#132932,#132933,#132934,#132935,#132936,#132937,#132938,
#132939,#132940,#132941,#132942,#132943,#132944,#132945,#132946,#132947,
#132948,#132949,#132950,#132951,#132952,#132953,#132954,#132955,#132956,
#132957,#132958,#132959,#132960,#132961,#132962,#132963,#132964,#132965,
#132966,#132967,#132968,#132969,#132970,#132971,#132972,#132973,#132974,
#132975,#132976,#132977,#132978,#132979,#132980,#132981,#132982,#132983,
#132984,#132985,#132986,#132987,#132988,#132989,#132990,#132991,#132992,
#132993,#132994,#132995,#132996,#132997,#132998,#132999,#133000,#133001,
#133002,#133003,#133004,#133005,#133006,#133007,#133008,#133009,#133010,
#133011),.UNSPECIFIED.,.F.,.F.,(4,2,2,2,2,2,2,2,2,2,2,2,2,2,2,2,2,2,2,2,
2,2,2,2,2,2,2,2,2,2,2,2,2,2,2,2,2,2,2,2,2,2,2,2,2,2,2,2,2,2,2,2,2,2,2,2,
2,2,2,2,2,2,2,2,2,2,2,2,2,2,2,2,2,2,2,2,2,2,2,2,2,2,2,4),(-1.39870355738125,
-1.39709323051322,-1.39438139580999,-1.39166930499781,-1.38755669007251,
-1.3736047233822,-1.36520698520691,-1.36182875593005,-1.35918661641566,
-1.35761269078721,-1.35621499900328,-1.3536933908489,-1.33973391704012,
-1.32727511715368,-1.32338833003953,-1.320715499827,-1.31828358701918,-1.31423135284018,
-1.29931765007779,-1.2914916128012,-1.28684221459254,-1.28491723923631,
-1.28344349786372,-1.28153382378389,-1.2773037203214,-1.26076534078919,
-1.25511305432508,-1.25059007762816,-1.24780316922912,-1.24517725477441,
-1.2414171294668,-1.22410020745919,-1.21503416014965,-1.21232723971982,
-1.21074015558069,-1.20935169995419,-1.20688363802996,-1.19245399721653,
-1.18401330010431,-1.17810686102362,-1.17507431121453,-1.17248187027663,
-1.1692198109322,-1.16176295059518,-1.14882582466956,-1.14077648941288,
-1.13848465966282,-1.13699042889687,-1.13529414411419,-1.13203221812217,
-1.12750004796582,-1.11115007077001,-1.10485954630007,-1.10176524853483,
-1.09943519954046,-1.09637016545883,-1.09026444696507,-1.08135125504194,
-1.0678990417944,-1.06531879510893,-1.0637572124499,-1.06214661592754,-1.05932337689066,
-1.05562364911276,-1.04558879054432,-1.03391940752607,-1.02982178401969,
-1.02738263284155,-1.02471646795181,-1.02086990506828,-1.00800276375469,
-0.994426303294931,-0.991859322204321,-0.990453579502622,-0.988889461216315,
-0.986296795370386,-0.975354828504718,-0.960344432689713,-0.956302765445229,
-0.953872476545109,-0.951197830055049,-0.947300943870582,-0.933695294690738,
-0.932467505666577),.UNSPECIFIED.);
#1692=B_SPLINE_CURVE_WITH_KNOTS('',3,(#133013,#133014,#133015,#133016,#133017,
#133018,#133019,#133020,#133021,#133022,#133023,#133024,#133025,#133026,
#133027,#133028),.UNSPECIFIED.,.F.,.F.,(4,3,3,3,3,4),(53.0628845126283,
53.1975485052734,53.2260686323923,53.2261279621233,53.3579672512799,53.4070751110265),
 .UNSPECIFIED.);
#1693=B_SPLINE_CURVE_WITH_KNOTS('',3,(#133029,#133030,#133031,#133032,#133033,
#133034,#133035,#133036,#133037,#133038,#133039,#133040,#133041,#133042,
#133043,#133044,#133045,#133046,#133047,#133048,#133049,#133050,#133051,
#133052,#133053,#133054,#133055,#133056,#133057,#133058,#133059,#133060,
#133061,#133062,#133063,#133064,#133065,#133066,#133067,#133068,#133069,
#133070,#133071,#133072,#133073,#133074,#133075,#133076,#133077,#133078,
#133079,#133080,#133081,#133082,#133083,#133084,#133085,#133086,#133087,
#133088,#133089,#133090,#133091,#133092,#133093,#133094,#133095,#133096,
#133097,#133098,#133099,#133100,#133101,#133102,#133103,#133104,#133105,
#133106,#133107,#133108,#133109,#133110,#133111,#133112,#133113,#133114,
#133115,#133116,#133117,#133118,#133119,#133120,#133121,#133122,#133123,
#133124,#133125,#133126,#133127,#133128,#133129,#133130,#133131,#133132,
#133133,#133134,#133135,#133136,#133137,#133138,#133139,#133140,#133141,
#133142,#133143,#133144,#133145,#133146,#133147,#133148,#133149,#133150,
#133151,#133152,#133153,#133154,#133155,#133156,#133157,#133158,#133159,
#133160,#133161,#133162,#133163,#133164,#133165,#133166,#133167,#133168,
#133169,#133170,#133171,#133172,#133173,#133174,#133175,#133176,#133177,
#133178,#133179,#133180,#133181,#133182,#133183,#133184,#133185,#133186,
#133187,#133188,#133189,#133190,#133191,#133192,#133193,#133194,#133195,
#133196,#133197,#133198,#133199,#133200,#133201,#133202,#133203,#133204,
#133205,#133206,#133207,#133208,#133209,#133210,#133211,#133212),
 .UNSPECIFIED.,.F.,.F.,(4,3,3,3,3,3,3,3,3,3,3,3,3,3,3,3,3,3,3,3,3,3,3,3,
3,3,3,3,3,3,3,3,3,3,3,3,3,3,3,3,3,3,3,3,3,3,3,3,3,3,3,3,3,3,3,3,3,3,3,3,
3,4),(53.407075112124,53.5395748225813,53.6719291179904,53.8076153178973,
53.9400068534946,54.0773403855563,54.2013994567497,54.214673917618,54.2147332472902,
54.3367217607587,54.3493100143317,54.4837327187534,54.6180168659285,54.7522370077264,
54.8865669004053,55.0209610903902,55.1556158998146,55.2032792028438,55.2033385325175,
55.3253270457457,55.3379152995103,55.4723380038829,55.6066221510069,55.740842292752,
55.8751721853761,56.0095663753049,56.1442211846721,56.1918844880695,56.1919438177393,
56.3139323317598,56.3265205853932,56.4609432904251,56.595227438209,56.7294475806129,
56.8637774738881,56.9981716644641,57.132826474465,57.1804897732952,57.1805491029676,
57.3025376163047,57.3151258693894,57.4495485731948,57.5838327197582,57.7180528609505,
57.8523827530386,57.9867769424403,58.1214317513003,58.1690950585209,58.1691543882022,
58.2911428999394,58.3037311547547,58.438153858685,58.5724380053582,58.7066581466454,
58.8409880388054,58.975382228266,59.110037037165,59.1577003437467,59.157759673411,
59.2819978092843,59.2969476030988,59.3472480465758),.UNSPECIFIED.);
#1694=B_SPLINE_CURVE_WITH_KNOTS('',3,(#133217,#133218,#133219,#133220,#133221,
#133222,#133223,#133224,#133225,#133226,#133227,#133228,#133229,#133230,
#133231,#133232,#133233,#133234,#133235,#133236,#133237,#133238,#133239,
#133240,#133241,#133242,#133243,#133244,#133245,#133246,#133247,#133248,
#133249,#133250,#133251,#133252,#133253,#133254,#133255,#133256,#133257,
#133258,#133259,#133260,#133261,#133262,#133263,#133264,#133265,#133266,
#133267,#133268,#133269,#133270,#133271,#133272,#133273,#133274,#133275,
#133276,#133277,#133278,#133279,#133280,#133281,#133282,#133283,#133284,
#133285,#133286,#133287,#133288,#133289,#133290,#133291,#133292,#133293,
#133294,#133295,#133296,#133297,#133298,#133299,#133300,#133301,#133302,
#133303,#133304,#133305,#133306,#133307,#133308,#133309,#133310,#133311,
#133312,#133313,#133314,#133315,#133316,#133317,#133318,#133319,#133320,
#133321,#133322,#133323,#133324,#133325,#133326,#133327,#133328,#133329,
#133330,#133331,#133332,#133333,#133334,#133335,#133336,#133337,#133338,
#133339,#133340,#133341,#133342,#133343,#133344,#133345,#133346,#133347,
#133348,#133349,#133350,#133351,#133352,#133353,#133354,#133355,#133356,
#133357,#133358,#133359,#133360,#133361,#133362,#133363,#133364,#133365,
#133366,#133367,#133368,#133369,#133370,#133371,#133372,#133373,#133374,
#133375,#133376,#133377,#133378),.UNSPECIFIED.,.F.,.F.,(4,2,2,2,2,2,2,2,
2,2,2,2,2,2,2,2,2,2,2,2,2,2,2,2,2,2,2,2,2,2,2,2,2,2,2,2,2,2,2,2,2,2,2,2,
2,2,2,2,2,2,2,2,2,2,2,2,2,2,2,2,2,2,2,2,2,2,2,2,2,2,2,2,2,2,2,2,2,2,2,2,
4),(-1.86488544419714,-1.85365696410191,-1.84188530806308,-1.8377699615751,
-1.83505758284678,-1.83234651493028,-1.8282386120305,-1.81418462147493,
-1.80585531449291,-1.8024919954102,-1.79985847775436,-1.79828636155049,
-1.79668846069849,-1.79392749548157,-1.78371066127597,-1.77295238263045,
-1.76820227091544,-1.76420762745974,-1.76151660859604,-1.75910234343622,
-1.75516109849534,-1.73920378676322,-1.72934771433257,-1.7265523264965,
-1.72494746555782,-1.7233814331193,-1.72077835931069,-1.70757744503926,
-1.69442125350727,-1.69057828212119,-1.68791291387726,-1.68547335476776,
-1.68137238568769,-1.66958280630193,-1.65962674498408,-1.65594067604859,
-1.65312534435754,-1.65151645214735,-1.64995370372793,-1.64736731673291,
-1.63399597602187,-1.62098615509736,-1.61713967660845,-1.61447367123057,
-1.61203467117964,-1.60793749639567,-1.59632334200793,-1.58623232335227,
-1.58252183488291,-1.57969300110081,-1.57808136151013,-1.57652077683416,
-1.57394539094252,-1.56046890246613,-1.54766833468709,-1.54376518407776,
-1.54108971110237,-1.53866078594208,-1.53462673505591,-1.51951620823629,
-1.51179811411383,-1.50718683313568,-1.50526735100317,-1.50379363339642,
-1.50187868174028,-1.49839427370121,-1.48394776240774,-1.47570542619547,
-1.47106081549173,-1.46825151334881,-1.46560719826398,-1.46189699443107,
-1.44423356580635,-1.4353578376186,-1.43267345740897,-1.43109098872612,
-1.42969948523156,-1.4272135118021,-1.41294200199675,-1.40120451120901,
-1.39870355738125),.UNSPECIFIED.);
#1695=B_SPLINE_CURVE_WITH_KNOTS('',3,(#133380,#133381,#133382,#133383,#133384,
#133385,#133386,#133387,#133388,#133389,#133390,#133391),.UNSPECIFIED.,
 .F.,.F.,(4,2,2,2,2,4),(-0.0255459513154411,-0.0128046247359227,-0.00704877268430528,
-0.00400898693505774,-0.00198358349779247,-3.22321518027115E-5),
 .UNSPECIFIED.);
#1696=B_SPLINE_CURVE_WITH_KNOTS('',3,(#133392,#133393,#133394,#133395,#133396,
#133397,#133398,#133399,#133400,#133401,#133402,#133403,#133404,#133405,
#133406,#133407,#133408,#133409,#133410,#133411,#133412,#133413,#133414,
#133415,#133416,#133417,#133418,#133419,#133420,#133421,#133422,#133423,
#133424,#133425,#133426,#133427,#133428,#133429,#133430,#133431,#133432,
#133433,#133434,#133435,#133436,#133437,#133438,#133439,#133440,#133441,
#133442,#133443,#133444,#133445,#133446,#133447,#133448,#133449,#133450,
#133451,#133452,#133453,#133454,#133455,#133456,#133457,#133458,#133459,
#133460,#133461,#133462,#133463,#133464,#133465,#133466,#133467,#133468,
#133469,#133470,#133471,#133472,#133473,#133474,#133475,#133476,#133477,
#133478,#133479,#133480,#133481,#133482,#133483,#133484,#133485,#133486,
#133487,#133488,#133489,#133490,#133491,#133492,#133493,#133494,#133495,
#133496,#133497,#133498,#133499,#133500,#133501,#133502,#133503,#133504,
#133505,#133506,#133507,#133508,#133509,#133510,#133511,#133512,#133513,
#133514,#133515,#133516,#133517,#133518,#133519,#133520,#133521,#133522,
#133523,#133524,#133525,#133526,#133527,#133528,#133529,#133530,#133531,
#133532,#133533,#133534,#133535,#133536,#133537,#133538,#133539,#133540,
#133541,#133542,#133543,#133544,#133545,#133546,#133547,#133548,#133549,
#133550,#133551,#133552,#133553,#133554,#133555,#133556,#133557,#133558,
#133559,#133560,#133561,#133562,#133563,#133564,#133565,#133566,#133567,
#133568,#133569,#133570,#133571,#133572,#133573,#133574,#133575),
 .UNSPECIFIED.,.F.,.F.,(4,3,3,3,3,3,3,3,3,3,3,3,3,3,3,3,3,3,3,3,3,3,3,3,
3,3,3,3,3,3,3,3,3,3,3,3,3,3,3,3,3,3,3,3,3,3,3,3,3,3,3,3,3,3,3,3,3,3,3,3,
3,4),(59.6902604970919,59.833396490693,59.9768904150285,60.1083013831761,
60.1209187781749,60.1463056289724,60.1463649586525,60.2683534696589,60.2809417196825,
60.4153644181217,60.54964855935,60.6838686952516,60.8181985821629,60.9525927664475,
61.0872475703433,61.1349109141981,61.1349702439286,61.2569587469848,61.2695470095179,
61.4039697124623,61.5382538580817,61.6724739982504,61.8068038892084,61.9411980774173,
62.0758528850074,62.1235161994239,62.1235755289416,62.2455640740847,62.2581523224295,
62.3925750532376,62.5268592268259,62.6610793949968,62.7954093137422,62.9298035296484,
63.0644583644501,63.1121214846496,63.1121808144321,63.2341692995476,63.2467575308238,
63.3811801848166,63.5154642817972,63.6496843737593,63.7840142175936,63.9184083592464,
64.053063121709,64.1007267698753,64.1007860998983,64.222774553837,64.2353628755673,
64.3697855883676,64.504069743311,64.6382898922554,64.7726197911066,64.907013986709,
65.041668800863,65.089332055101,65.089391383594,65.2103712287251,65.2243357646258,
65.3570552955892,65.4932010943946,65.6293468932001),.UNSPECIFIED.);
#1697=B_SPLINE_CURVE_WITH_KNOTS('',3,(#133580,#133581,#133582,#133583,#133584,
#133585,#133586,#133587,#133588,#133589,#133590,#133591,#133592,#133593,
#133594,#133595,#133596,#133597,#133598,#133599,#133600,#133601,#133602,
#133603,#133604,#133605,#133606,#133607,#133608,#133609,#133610,#133611,
#133612,#133613,#133614,#133615,#133616,#133617,#133618,#133619,#133620,
#133621,#133622,#133623,#133624,#133625,#133626,#133627,#133628,#133629,
#133630,#133631,#133632,#133633,#133634,#133635,#133636,#133637,#133638,
#133639,#133640,#133641,#133642,#133643,#133644,#133645,#133646,#133647,
#133648,#133649,#133650,#133651,#133652,#133653,#133654,#133655,#133656,
#133657,#133658,#133659,#133660,#133661,#133662,#133663,#133664,#133665,
#133666,#133667,#133668,#133669,#133670,#133671,#133672,#133673,#133674,
#133675,#133676,#133677,#133678,#133679,#133680,#133681,#133682,#133683,
#133684,#133685,#133686,#133687,#133688,#133689,#133690,#133691,#133692,
#133693,#133694,#133695,#133696,#133697,#133698,#133699,#133700,#133701,
#133702,#133703,#133704,#133705,#133706,#133707,#133708,#133709,#133710,
#133711,#133712,#133713,#133714,#133715,#133716,#133717,#133718,#133719,
#133720,#133721,#133722,#133723,#133724,#133725,#133726,#133727,#133728,
#133729,#133730,#133731,#133732,#133733,#133734,#133735,#133736,#133737,
#133738,#133739,#133740,#133741,#133742,#133743,#133744,#133745,#133746,
#133747,#133748,#133749,#133750,#133751,#133752,#133753),.UNSPECIFIED.,
 .F.,.F.,(4,2,2,2,2,2,2,2,2,2,2,2,2,2,2,2,2,2,2,2,2,2,2,2,2,2,2,2,2,2,2,
2,2,2,2,2,2,2,2,2,2,2,2,2,2,2,2,2,2,2,2,2,2,2,2,2,2,2,2,2,2,2,2,2,2,2,2,
2,2,2,2,2,2,2,2,2,2,2,2,2,2,2,2,2,2,2,4),(-2.33098756212136,-2.32770212338009,
-2.31646610862759,-2.31383727485646,-2.31227335927866,-2.3106807241972,
-2.30794645461203,-2.29611141811926,-2.28637100161808,-2.28184644323665,
-2.27798786631659,-2.27531564131121,-2.27287179559994,-2.26876677381099,
-2.25479628646993,-2.24647852907023,-2.24311720114654,-2.24048372665527,
-2.23890820971872,-2.2373051432569,-2.2345233794621,-2.22405370772014,-2.21350214987303,
-2.21028520318969,-2.20556272023435,-2.20273890313631,-2.20010064510374,
-2.19643211268646,-2.17846101382362,-2.16973969810326,-2.16707419053712,
-2.16549600903019,-2.16390710980978,-2.16118601762735,-2.14955060040506,
-2.13967950270808,-2.13512859700862,-2.13125680230042,-2.12858867128916,
-2.12615767250019,-2.12209914607859,-2.11158873066677,-2.10236725326662,
-2.09755506665382,-2.09416608045372,-2.09244206899566,-2.09094186917777,
-2.08870398943557,-2.08144867600362,-2.0678575206045,-2.06258828831665,
-2.05828447768567,-2.05553756358227,-2.0528862316855,-2.04897089413123,
-2.03281880079352,-2.02309300260766,-2.02031147442211,-2.01870894554653,
-2.01713997775017,-2.01452258642402,-2.00149125823969,-1.98821011764705,
-1.98436174964467,-1.98169562380451,-1.97925727365408,-1.97516312319999,
-1.96082692639583,-1.95266821622917,-1.94934204921407,-1.94672994932158,
-1.94516230094211,-1.9437604087264,-1.94121343615269,-1.92520656097234,
-1.91642760513991,-1.91175119696534,-1.90893650509543,-1.90629567161495,
-1.90260492384512,-1.88481387908689,-1.87600911026292,-1.87333356871875,
-1.8717531447419,-1.87036068286077,-1.86786840001739,-1.86488544419714),
 .UNSPECIFIED.);
#1698=B_SPLINE_CURVE_WITH_KNOTS('',3,(#133755,#133756,#133757,#133758,#133759,
#133760,#133761,#133762),.UNSPECIFIED.,.F.,.F.,(4,2,2,4),(-0.025564683553867,
-0.0212145539685123,-0.0127726529739691,-2.44579138260531E-5),
 .UNSPECIFIED.);
#1699=B_SPLINE_CURVE_WITH_KNOTS('',3,(#133763,#133764,#133765,#133766,#133767,
#133768,#133769,#133770,#133771,#133772,#133773,#133774,#133775,#133776,
#133777,#133778,#133779,#133780,#133781,#133782,#133783,#133784,#133785,
#133786,#133787,#133788,#133789,#133790,#133791,#133792,#133793,#133794,
#133795,#133796,#133797,#133798,#133799,#133800,#133801,#133802,#133803,
#133804,#133805,#133806,#133807,#133808,#133809,#133810,#133811,#133812,
#133813,#133814,#133815,#133816,#133817,#133818,#133819,#133820,#133821,
#133822,#133823,#133824,#133825,#133826,#133827,#133828,#133829,#133830,
#133831,#133832,#133833,#133834,#133835,#133836,#133837,#133838,#133839,
#133840,#133841,#133842,#133843,#133844,#133845,#133846,#133847,#133848,
#133849,#133850,#133851,#133852,#133853,#133854,#133855,#133856,#133857,
#133858,#133859,#133860,#133861,#133862,#133863,#133864,#133865,#133866,
#133867,#133868,#133869,#133870,#133871,#133872,#133873,#133874,#133875,
#133876,#133877,#133878,#133879,#133880,#133881,#133882,#133883,#133884,
#133885,#133886,#133887,#133888,#133889,#133890,#133891,#133892,#133893,
#133894,#133895,#133896,#133897,#133898,#133899,#133900,#133901,#133902,
#133903,#133904,#133905,#133906,#133907,#133908,#133909,#133910,#133911,
#133912,#133913,#133914,#133915,#133916,#133917,#133918,#133919,#133920,
#133921,#133922,#133923,#133924,#133925,#133926,#133927,#133928,#133929,
#133930,#133931,#133932,#133933,#133934,#133935,#133936,#133937,#133938,
#133939,#133940,#133941,#133942,#133943),.UNSPECIFIED.,.F.,.F.,(4,3,3,3,
3,3,3,3,3,3,3,3,3,3,3,3,3,3,3,3,3,3,3,3,3,3,3,3,3,3,3,3,3,3,3,3,3,3,3,3,
3,3,3,3,3,3,3,3,3,3,3,3,3,3,3,3,3,3,3,3,4),(65.9734457253856,66.0779373403268,
66.0779966711752,66.1999849066616,66.2125730323752,66.3469953325592,66.4812790769259,
66.6154988183458,66.7498283179537,66.8842221186058,67.0188765491595,67.0665426255525,
67.0666019571481,67.1885901731476,67.2011789324032,67.3356018427714,67.469886191261,
67.6041065292935,67.7384366089515,67.8728309808017,68.0074859622503,68.0551479107782,
68.055207231863,68.1771974382781,68.1897850942651,68.3242088928125,68.4584941386067,
68.5927153806746,68.7270463656961,68.8614416447783,68.9960975246431,69.0437531960039,
69.0438125367751,69.1657985521766,69.1783861667009,69.3128057452608,69.4470867745264,
69.5813038141547,69.7156306567655,69.8500218230336,69.9846736860503,70.0323584812297,
70.0324178197249,70.1544052585737,70.1669971512239,70.3014224006743,70.4357090587619,
70.5699316714495,70.7042639534098,70.8386604884861,70.973317548102,71.0209637664554,
71.0210230350765,71.1430235684413,71.1556109739712,71.2900401917198,71.4243262573423,
71.558617078649,71.6929036281056,71.827384909386,71.9125675619089),
 .UNSPECIFIED.);
#1700=B_SPLINE_CURVE_WITH_KNOTS('',3,(#133946,#133947,#133948,#133949,#133950,
#133951,#133952,#133953,#133954,#133955,#133956,#133957,#133958,#133959,
#133960,#133961),.UNSPECIFIED.,.F.,.F.,(4,3,3,3,3,4),(71.9125675627573,
72.0095690516811,72.0096284787209,72.1412543016073,72.1828455385974,72.2566310313772),
 .UNSPECIFIED.);
#1701=B_SPLINE_CURVE_WITH_KNOTS('',3,(#133963,#133964,#133965,#133966,#133967,
#133968,#133969,#133970,#133971,#133972,#133973,#133974,#133975,#133976,
#133977,#133978,#133979,#133980,#133981,#133982,#133983,#133984,#133985,
#133986,#133987,#133988,#133989,#133990,#133991,#133992,#133993,#133994,
#133995,#133996,#133997,#133998,#133999,#134000,#134001,#134002,#134003,
#134004,#134005,#134006,#134007,#134008,#134009,#134010,#134011,#134012,
#134013,#134014,#134015,#134016,#134017,#134018,#134019,#134020,#134021,
#134022,#134023,#134024,#134025,#134026,#134027,#134028,#134029,#134030,
#134031,#134032,#134033,#134034,#134035,#134036,#134037,#134038,#134039,
#134040,#134041,#134042,#134043,#134044,#134045,#134046,#134047,#134048,
#134049,#134050,#134051,#134052,#134053,#134054,#134055,#134056,#134057,
#134058,#134059,#134060,#134061,#134062,#134063,#134064,#134065,#134066,
#134067,#134068,#134069,#134070,#134071,#134072,#134073,#134074,#134075,
#134076,#134077,#134078,#134079,#134080,#134081,#134082,#134083,#134084,
#134085,#134086,#134087,#134088,#134089,#134090,#134091,#134092,#134093,
#134094,#134095,#134096,#134097,#134098,#134099,#134100,#134101,#134102,
#134103,#134104,#134105,#134106,#134107,#134108,#134109,#134110,#134111,
#134112,#134113,#134114,#134115,#134116,#134117,#134118,#134119,#134120,
#134121,#134122,#134123,#134124,#134125,#134126,#134127,#134128),
 .UNSPECIFIED.,.F.,.F.,(4,3,3,3,3,3,3,3,3,3,3,3,3,3,3,3,3,3,3,3,3,3,3,3,
3,3,3,3,3,3,3,3,3,3,3,3,3,3,3,3,3,3,3,3,3,3,3,3,3,3,3,3,3,3,3,4),(72.2566310325653,
72.3894374467591,72.5221457062876,72.6549339998429,72.7877622859877,72.9208549495036,
72.9981743369069,72.9982336898363,73.1202228277463,73.1328364350279,73.2672849584092,
73.4015946806294,73.5358400918455,73.6701945703871,73.8046129814629,73.9392911666892,
73.9867796221326,73.9868385324179,74.108906242501,74.1214488825271,74.255905222884,
74.390223385728,74.5244778313572,74.6588421253742,74.793270814519,74.9279598270099,
74.9753849073583,74.9754450466518,75.0972621653067,75.1098516883196,75.2441047719449,
75.3782194139114,75.5122705854141,75.6464338624038,75.7806625836947,75.9151557208552,
75.963990192584,75.9640493770624,76.0861045734201,76.0988646685781,76.2335246164758,
76.3680442827096,76.5024976289655,76.6370551344828,76.7716739686609,76.9065461955451,
76.9525954778098,76.9526520815709,77.0740905315279,77.0857383232952,77.2186728465627,
77.351477171386,77.4843223777113,77.6171794272965,77.7502847484,77.8457368347758),
 .UNSPECIFIED.);
#1702=B_SPLINE_CURVE_WITH_KNOTS('',3,(#134132,#134133,#134134,#134135,#134136,
#134137,#134138,#134139,#134140,#134141,#134142,#134143,#134144,#134145,
#134146,#134147,#134148,#134149,#134150,#134151,#134152,#134153,#134154,
#134155,#134156,#134157,#134158,#134159,#134160,#134161,#134162,#134163,
#134164,#134165,#134166,#134167,#134168,#134169,#134170,#134171,#134172,
#134173,#134174,#134175,#134176,#134177,#134178,#134179,#134180,#134181,
#134182,#134183,#134184,#134185,#134186,#134187,#134188,#134189,#134190,
#134191,#134192,#134193,#134194,#134195,#134196,#134197,#134198,#134199,
#134200,#134201,#134202,#134203,#134204,#134205,#134206,#134207,#134208,
#134209,#134210,#134211,#134212,#134213,#134214,#134215,#134216,#134217,
#134218,#134219,#134220,#134221,#134222,#134223,#134224,#134225,#134226,
#134227,#134228,#134229,#134230,#134231,#134232,#134233,#134234,#134235,
#134236,#134237,#134238,#134239,#134240,#134241,#134242,#134243,#134244,
#134245,#134246,#134247,#134248,#134249,#134250,#134251,#134252,#134253,
#134254,#134255,#134256,#134257,#134258,#134259,#134260,#134261,#134262,
#134263,#134264,#134265,#134266,#134267,#134268,#134269,#134270,#134271,
#134272,#134273),.UNSPECIFIED.,.F.,.F.,(4,3,3,3,3,3,3,3,3,3,3,3,3,3,3,3,
3,3,3,3,3,3,3,3,3,3,3,3,3,3,3,3,3,3,3,3,3,3,3,3,3,3,3,3,3,3,3,4),(72.2566314741396,
72.4045609950112,72.5414579617111,72.5535140284593,72.6517127398032,72.651772204656,
72.7769482243648,72.7866266109606,72.9212659463293,73.0557645182426,73.1901963484967,
73.3247324131253,73.4593295146966,73.5865318565016,73.5941811307337,73.6415997214062,
73.6416565254697,73.7672874375975,73.7764261693097,73.9109853627333,74.0454085321108,
74.1797698262172,74.3142431103432,74.44878183488,74.5751854586477,74.5835822859716,
74.6314745352144,74.6315408462834,74.7551941928077,74.7648000454726,74.8978457776245,
75.0307559072255,75.1636079962241,75.2965913886114,75.429648976824,75.5630004736777,
75.6213694876214,75.6214251670971,75.748251875531,75.7596541443398,75.8976295032126,
76.0354124773744,76.1793867300085,76.3170070392934,76.4546118871423,76.5830703015199,
76.5923159523675,76.6113094879108),.UNSPECIFIED.);
#1703=B_SPLINE_CURVE_WITH_KNOTS('',3,(#134274,#134275,#134276,#134277,#134278,
#134279,#134280,#134281,#134282,#134283,#134284,#134285,#134286,#134287),
 .UNSPECIFIED.,.F.,.F.,(4,2,2,2,2,2,4),(-2.35651538611015,-2.35375456035493,
-2.3513626252777,-2.34892223761256,-2.3465069901102,-2.34248392432371,-2.33098756212136),
 .UNSPECIFIED.);
#1704=B_SPLINE_CURVE_WITH_KNOTS('',3,(#134290,#134291,#134292,#134293,#134294,
#134295,#134296,#134297,#134298,#134299,#134300,#134301,#134302,#134303,
#134304,#134305,#134306,#134307,#134308,#134309,#134310,#134311,#134312,
#134313,#134314,#134315,#134316,#134317,#134318,#134319,#134320,#134321,
#134322,#134323,#134324,#134325,#134326,#134327,#134328,#134329,#134330,
#134331,#134332,#134333,#134334,#134335,#134336,#134337,#134338,#134339,
#134340,#134341,#134342,#134343,#134344,#134345,#134346,#134347),
 .UNSPECIFIED.,.F.,.F.,(4,3,3,3,3,3,3,3,3,3,3,3,3,3,3,3,3,3,3,4),(63.947346022237,
64.0856677806405,64.2249239385586,64.3424808528907,64.468575806381,64.5944806171026,
64.7202560417844,64.8459626123754,64.971755226253,65.0975842562297,65.2236618847116,
65.3323651737044,65.4568633156543,65.5811766710722,65.7053691135383,65.8295042784497,
65.9537253005869,66.0779993018877,66.2024833656448,66.2363314693039),
 .UNSPECIFIED.);
#1705=B_SPLINE_CURVE_WITH_KNOTS('',3,(#134350,#134351,#134352,#134353,#134354,
#134355,#134356,#134357,#134358,#134359,#134360,#134361,#134362,#134363,
#134364,#134365,#134366,#134367,#134368,#134369,#134370,#134371,#134372,
#134373,#134374,#134375,#134376,#134377,#134378,#134379,#134380,#134381,
#134382,#134383),.UNSPECIFIED.,.F.,.F.,(4,3,3,3,3,3,3,3,3,3,3,4),(-68.3020181361455,
-68.1732359894119,-68.0445307062512,-67.9158529349099,-67.7871533887138,
-67.6582664075924,-67.5292846492219,-67.4000115996097,-67.3134128509198,
-67.1758788210711,-67.0392397108572,-66.9234304578509),.UNSPECIFIED.);
#1706=B_SPLINE_CURVE_WITH_KNOTS('',3,(#134673,#134674,#134675,#134676,#134677,
#134678,#134679,#134680,#134681,#134682,#134683,#134684,#134685,#134686,
#134687,#134688,#134689,#134690,#134691,#134692,#134693,#134694,#134695,
#134696,#134697,#134698),.UNSPECIFIED.,.F.,.F.,(4,2,2,2,2,2,2,2,2,2,2,2,
4),(0.105663848425438,0.141373353833559,0.175486205805465,0.215538764100116,
0.275546330497321,0.326160459620167,0.383983207715567,0.434851934495649,
0.488868806433905,0.539980848713981,0.589887233590854,0.654795876329018,
0.744278844687171),.UNSPECIFIED.);
#1707=B_SPLINE_CURVE_WITH_KNOTS('',3,(#134700,#134701,#134702,#134703,#134704,
#134705,#134706,#134707,#134708,#134709,#134710,#134711,#134712,#134713,
#134714,#134715,#134716,#134717,#134718,#134719,#134720,#134721,#134722,
#134723,#134724,#134725,#134726,#134727,#134728,#134729,#134730,#134731,
#134732,#134733,#134734,#134735,#134736,#134737,#134738,#134739,#134740,
#134741,#134742,#134743,#134744,#134745,#134746,#134747,#134748,#134749,
#134750,#134751,#134752,#134753,#134754,#134755,#134756,#134757,#134758,
#134759,#134760,#134761,#134762,#134763,#134764,#134765,#134766,#134767,
#134768,#134769,#134770,#134771,#134772,#134773,#134774,#134775),
 .UNSPECIFIED.,.F.,.F.,(4,3,3,3,3,3,3,3,3,3,3,3,3,3,3,3,3,3,3,3,3,3,3,3,
3,4),(-0.176229339719688,-0.16930135536687,-0.158068822610707,-0.153210440573506,
-0.14999874865766,-0.137539014752818,-0.130276774573411,-0.127219505533131,
-0.124662971108758,-0.112718638611185,-0.101066870224045,-0.0953479689548292,
-0.0930447645920619,-0.0906327597761066,-0.0794410933175649,-0.0687205266155614,
-0.0632054306857541,-0.060455489415314,-0.058082450533308,-0.0468942590722208,
-0.0358420032534035,-0.0306121296933921,-0.0277796741820399,-0.0172857919180543,
-0.00699398448747527,0.),.UNSPECIFIED.);
#1708=B_SPLINE_CURVE_WITH_KNOTS('',3,(#134776,#134777,#134778,#134779,#134780,
#134781),.UNSPECIFIED.,.F.,.F.,(4,2,4),(-0.0013480645929508,-0.000678455957808124,
-1.00000007721593E-6),.UNSPECIFIED.);
#1709=B_SPLINE_CURVE_WITH_KNOTS('',3,(#134782,#134783,#134784,#134785,#134786,
#134787,#134788,#134789,#134790,#134791,#134792,#134793),.UNSPECIFIED.,
 .F.,.F.,(4,2,2,2,2,4),(1.80267612534286E-5,0.030912223860268,0.0584819346422233,
0.0746239839028914,0.10502074371225,0.105663848425438),.UNSPECIFIED.);
#1710=B_SPLINE_CURVE_WITH_KNOTS('',3,(#134798,#134799,#134800,#134801),
 .UNSPECIFIED.,.F.,.F.,(4,4),(0.,0.00718622469090485),.UNSPECIFIED.);
#1711=B_SPLINE_CURVE_WITH_KNOTS('',3,(#134802,#134803,#134804,#134805,#134806,
#134807,#134808,#134809,#134810,#134811,#134812,#134813,#134814,#134815,
#134816,#134817,#134818,#134819,#134820,#134821,#134822,#134823,#134824,
#134825,#134826,#134827,#134828,#134829,#134830,#134831,#134832,#134833,
#134834,#134835,#134836,#134837,#134838,#134839,#134840,#134841,#134842,
#134843,#134844,#134845,#134846,#134847,#134848,#134849,#134850,#134851,
#134852,#134853,#134854,#134855,#134856,#134857,#134858,#134859,#134860,
#134861,#134862,#134863,#134864,#134865,#134866,#134867,#134868,#134869,
#134870,#134871,#134872,#134873,#134874,#134875,#134876,#134877),
 .UNSPECIFIED.,.F.,.F.,(4,3,3,3,3,3,3,3,3,3,3,3,3,3,3,3,3,3,3,3,3,3,3,3,
3,4),(-0.178587760439507,-0.171910820567902,-0.161828334105325,-0.158626626042432,
-0.155662350564125,-0.144861472649272,-0.140141558931839,-0.137336962197544,
-0.134642654294749,-0.123288481409911,-0.111857928729176,-0.105498830583136,
-0.103071300928935,-0.0912509288672889,-0.0798445627588778,-0.0745908481568186,
-0.07199198364724,-0.0695034129914027,-0.0574052630533521,-0.0453071131153016,
-0.0394332477820004,-0.0367368004707021,-0.0343156904617242,-0.0216249730003383,
-0.00901663940650531,0.),.UNSPECIFIED.);
#1712=B_SPLINE_CURVE_WITH_KNOTS('',3,(#135159,#135160,#135161,#135162,#135163,
#135164,#135165,#135166,#135167,#135168,#135169,#135170),.UNSPECIFIED.,
 .F.,.F.,(4,2,2,2,2,4),(-0.106753670550095,-0.0847951227008117,-0.0660598735029805,
-0.0401729541102252,-0.0191044959439433,0.),.UNSPECIFIED.);
#1713=SHAPE_REPRESENTATION_RELATIONSHIP('SRR','None',#135337,#1726);
#1714=SHAPE_REPRESENTATION_RELATIONSHIP('SRR','None',#135338,#1727);
#1715=SHAPE_REPRESENTATION_RELATIONSHIP('SRR','None',#135339,#1728);
#1716=SHAPE_REPRESENTATION_RELATIONSHIP('SRR','None',#135340,#1729);
#1717=SHAPE_REPRESENTATION_RELATIONSHIP('SRR','None',#135341,#1730);
#1718=SHAPE_REPRESENTATION_RELATIONSHIP('SRR','None',#135342,#1731);
#1719=SHAPE_REPRESENTATION_RELATIONSHIP('SRR','None',#135343,#1732);
#1720=SHAPE_REPRESENTATION_RELATIONSHIP('SRR','None',#135344,#1733);
#1721=SHAPE_REPRESENTATION_RELATIONSHIP('SRR','None',#135345,#1734);
#1722=SHAPE_REPRESENTATION_RELATIONSHIP('SRR','None',#135346,#1735);
#1723=SHAPE_REPRESENTATION_RELATIONSHIP('SRR','None',#135347,#1736);
#1724=SHAPE_REPRESENTATION_RELATIONSHIP('SRR','None',#135348,#1737);
#1725=SHAPE_REPRESENTATION_RELATIONSHIP('SRR','None',#135349,#1738);
#1726=ADVANCED_BREP_SHAPE_REPRESENTATION('',(#1752),#135269);
#1727=ADVANCED_BREP_SHAPE_REPRESENTATION('',(#1753),#135270);
#1728=ADVANCED_BREP_SHAPE_REPRESENTATION('',(#1754),#135271);
#1729=ADVANCED_BREP_SHAPE_REPRESENTATION('',(#1755),#135272);
#1730=ADVANCED_BREP_SHAPE_REPRESENTATION('',(#1756),#135273);
#1731=ADVANCED_BREP_SHAPE_REPRESENTATION('',(#1757),#135274);
#1732=ADVANCED_BREP_SHAPE_REPRESENTATION('',(#1758),#135275);
#1733=ADVANCED_BREP_SHAPE_REPRESENTATION('',(#1759),#135276);
#1734=ADVANCED_BREP_SHAPE_REPRESENTATION('',(#1760),#135277);
#1735=ADVANCED_BREP_SHAPE_REPRESENTATION('',(#1761),#135278);
#1736=ADVANCED_BREP_SHAPE_REPRESENTATION('',(#1762),#135279);
#1737=ADVANCED_BREP_SHAPE_REPRESENTATION('',(#1763),#135280);
#1738=ADVANCED_BREP_SHAPE_REPRESENTATION('',(#1764),#135281);
#1739=STYLED_ITEM('',(#135411),#1752);
#1740=STYLED_ITEM('',(#135412),#1753);
#1741=STYLED_ITEM('',(#135413),#1754);
#1742=STYLED_ITEM('',(#135414),#1755);
#1743=STYLED_ITEM('',(#135415),#1756);
#1744=STYLED_ITEM('',(#135416),#1757);
#1745=STYLED_ITEM('',(#135417),#1758);
#1746=STYLED_ITEM('',(#135418),#1759);
#1747=STYLED_ITEM('',(#135419),#1760);
#1748=STYLED_ITEM('',(#135420),#1761);
#1749=STYLED_ITEM('',(#135421),#1762);
#1750=STYLED_ITEM('',(#135422),#1763);
#1751=STYLED_ITEM('',(#135423),#1764);
#1752=MANIFOLD_SOLID_BREP('Body1',#32075);
#1753=MANIFOLD_SOLID_BREP('Body1',#32076);
#1754=MANIFOLD_SOLID_BREP('Body1',#32077);
#1755=MANIFOLD_SOLID_BREP('Body1',#32078);
#1756=MANIFOLD_SOLID_BREP('Body1',#32079);
#1757=MANIFOLD_SOLID_BREP('Body1',#32080);
#1758=MANIFOLD_SOLID_BREP('Body1',#32081);
#1759=MANIFOLD_SOLID_BREP('Body1',#32082);
#1760=MANIFOLD_SOLID_BREP('Body1',#32083);
#1761=MANIFOLD_SOLID_BREP('Body1',#32084);
#1762=MANIFOLD_SOLID_BREP('Body1',#32085);
#1763=MANIFOLD_SOLID_BREP('Body1',#32086);
#1764=MANIFOLD_SOLID_BREP('Body1',#32087);
#1765=CYLINDRICAL_SURFACE('',#32239,1.55);
#1766=CYLINDRICAL_SURFACE('',#32243,1.55);
#1767=CYLINDRICAL_SURFACE('',#32252,1.55);
#1768=CYLINDRICAL_SURFACE('',#32256,1.55);
#1769=CYLINDRICAL_SURFACE('',#32282,1.05);
#1770=CYLINDRICAL_SURFACE('',#32287,1.05);
#1771=CYLINDRICAL_SURFACE('',#32305,1.05);
#1772=CYLINDRICAL_SURFACE('',#32309,1.05);
#1773=CYLINDRICAL_SURFACE('',#32313,1.05);
#1774=CYLINDRICAL_SURFACE('',#32317,1.05);
#1775=CYLINDRICAL_SURFACE('',#32325,2.05);
#1776=CYLINDRICAL_SURFACE('',#32329,2.05);
#1777=CYLINDRICAL_SURFACE('',#32333,2.05);
#1778=CYLINDRICAL_SURFACE('',#32337,2.05);
#1779=CYLINDRICAL_SURFACE('',#32341,2.05);
#1780=CYLINDRICAL_SURFACE('',#32345,2.05);
#1781=CYLINDRICAL_SURFACE('',#32353,3.);
#1782=CYLINDRICAL_SURFACE('',#32358,3.);
#1783=CYLINDRICAL_SURFACE('',#32365,4.5);
#1784=CYLINDRICAL_SURFACE('',#32389,2.525);
#1785=CYLINDRICAL_SURFACE('',#32400,4.5);
#1786=CYLINDRICAL_SURFACE('',#32404,2.5);
#1787=CYLINDRICAL_SURFACE('',#32406,2.5);
#1788=CYLINDRICAL_SURFACE('',#32407,2.5);
#1789=CYLINDRICAL_SURFACE('',#32408,2.5);
#1790=CYLINDRICAL_SURFACE('',#32409,2.5);
#1791=CYLINDRICAL_SURFACE('',#32410,2.5);
#1792=CYLINDRICAL_SURFACE('',#32411,2.5);
#1793=CYLINDRICAL_SURFACE('',#32412,2.5);
#1794=CYLINDRICAL_SURFACE('',#32413,2.5);
#1795=CYLINDRICAL_SURFACE('',#32414,2.5);
#1796=CYLINDRICAL_SURFACE('',#32415,2.5);
#1797=CYLINDRICAL_SURFACE('',#32416,2.5);
#1798=CYLINDRICAL_SURFACE('',#32417,2.5);
#1799=CYLINDRICAL_SURFACE('',#32418,2.5);
#1800=CYLINDRICAL_SURFACE('',#32419,2.5);
#1801=CYLINDRICAL_SURFACE('',#32420,2.5);
#1802=CYLINDRICAL_SURFACE('',#32421,2.5);
#1803=CYLINDRICAL_SURFACE('',#32422,2.5);
#1804=CYLINDRICAL_SURFACE('',#32423,2.5);
#1805=CYLINDRICAL_SURFACE('',#32424,2.5);
#1806=CYLINDRICAL_SURFACE('',#32425,2.5);
#1807=CYLINDRICAL_SURFACE('',#32426,2.5);
#1808=CYLINDRICAL_SURFACE('',#32427,2.5);
#1809=CYLINDRICAL_SURFACE('',#32428,2.5);
#1810=CYLINDRICAL_SURFACE('',#32429,2.5);
#1811=CYLINDRICAL_SURFACE('',#32430,2.5);
#1812=CYLINDRICAL_SURFACE('',#32431,2.5);
#1813=CYLINDRICAL_SURFACE('',#32432,2.5);
#1814=CYLINDRICAL_SURFACE('',#32433,2.5);
#1815=CYLINDRICAL_SURFACE('',#32434,2.5);
#1816=CYLINDRICAL_SURFACE('',#32435,2.5);
#1817=CYLINDRICAL_SURFACE('',#32436,2.5);
#1818=CYLINDRICAL_SURFACE('',#32437,2.5);
#1819=CYLINDRICAL_SURFACE('',#32438,2.5);
#1820=CYLINDRICAL_SURFACE('',#32439,2.5);
#1821=CYLINDRICAL_SURFACE('',#32440,2.5);
#1822=CYLINDRICAL_SURFACE('',#32441,2.5);
#1823=CYLINDRICAL_SURFACE('',#32442,2.5);
#1824=CYLINDRICAL_SURFACE('',#32443,2.5);
#1825=CYLINDRICAL_SURFACE('',#32444,2.5);
#1826=CYLINDRICAL_SURFACE('',#32445,2.5);
#1827=CYLINDRICAL_SURFACE('',#32446,2.5);
#1828=CYLINDRICAL_SURFACE('',#32447,2.5);
#1829=CYLINDRICAL_SURFACE('',#32448,2.5);
#1830=CYLINDRICAL_SURFACE('',#32449,2.5);
#1831=CYLINDRICAL_SURFACE('',#32450,2.5);
#1832=CYLINDRICAL_SURFACE('',#32451,2.5);
#1833=CYLINDRICAL_SURFACE('',#32453,2.5);
#1834=CYLINDRICAL_SURFACE('',#32465,2.);
#1835=CYLINDRICAL_SURFACE('',#32472,2.);
#1836=CYLINDRICAL_SURFACE('',#32478,1.55);
#1837=CYLINDRICAL_SURFACE('',#32746,7.5);
#1838=CYLINDRICAL_SURFACE('',#32752,2.8);
#1839=CYLINDRICAL_SURFACE('',#32756,2.01);
#1840=CYLINDRICAL_SURFACE('',#33263,1.1);
#1841=CYLINDRICAL_SURFACE('',#33266,1.1);
#1842=CYLINDRICAL_SURFACE('',#33270,0.799999999999998);
#1843=CYLINDRICAL_SURFACE('',#33274,0.800000000000018);
#1844=CYLINDRICAL_SURFACE('',#33278,0.800000000000025);
#1845=CYLINDRICAL_SURFACE('',#33282,0.799999999999996);
#1846=CYLINDRICAL_SURFACE('',#33343,1.1);
#1847=CYLINDRICAL_SURFACE('',#33346,1.1);
#1848=CYLINDRICAL_SURFACE('',#33372,3.);
#1849=CYLINDRICAL_SURFACE('',#33376,3.);
#1850=CYLINDRICAL_SURFACE('',#33380,1.7);
#1851=CYLINDRICAL_SURFACE('',#33384,1.7);
#1852=CYLINDRICAL_SURFACE('',#33390,2.25);
#1853=CYLINDRICAL_SURFACE('',#33395,2.25);
#1854=CYLINDRICAL_SURFACE('',#33398,2.25);
#1855=CYLINDRICAL_SURFACE('',#33403,2.25);
#1856=CYLINDRICAL_SURFACE('',#33413,1.4635);
#1857=CYLINDRICAL_SURFACE('',#33415,1.4635);
#1858=CYLINDRICAL_SURFACE('',#33416,1.4635);
#1859=CYLINDRICAL_SURFACE('',#33417,1.4635);
#1860=CYLINDRICAL_SURFACE('',#33418,1.4635);
#1861=CYLINDRICAL_SURFACE('',#33419,1.4635);
#1862=CYLINDRICAL_SURFACE('',#33420,1.4635);
#1863=CYLINDRICAL_SURFACE('',#33421,1.4635);
#1864=CYLINDRICAL_SURFACE('',#33422,1.4635);
#1865=CYLINDRICAL_SURFACE('',#33423,1.17775);
#1866=CYLINDRICAL_SURFACE('',#33425,1.17775);
#1867=CYLINDRICAL_SURFACE('',#33426,1.17775);
#1868=CYLINDRICAL_SURFACE('',#33427,1.17775);
#1869=CYLINDRICAL_SURFACE('',#33428,1.17775);
#1870=CYLINDRICAL_SURFACE('',#33429,1.17775);
#1871=CYLINDRICAL_SURFACE('',#33430,1.17775);
#1872=CYLINDRICAL_SURFACE('',#33431,1.17775);
#1873=CYLINDRICAL_SURFACE('',#33432,1.17775);
#1874=CYLINDRICAL_SURFACE('',#33434,1.4635);
#1875=CYLINDRICAL_SURFACE('',#33450,0.816025403784426);
#1876=CYLINDRICAL_SURFACE('',#33452,0.816025403784426);
#1877=CYLINDRICAL_SURFACE('',#33454,0.816025403784426);
#1878=CYLINDRICAL_SURFACE('',#33456,0.816025403784426);
#1879=CYLINDRICAL_SURFACE('',#33458,0.816025403784426);
#1880=CYLINDRICAL_SURFACE('',#33460,0.816025403784426);
#1881=CYLINDRICAL_SURFACE('',#33497,1.05);
#1882=CYLINDRICAL_SURFACE('',#33505,1.05);
#1883=CYLINDRICAL_SURFACE('',#33518,1.55);
#1884=CYLINDRICAL_SURFACE('',#33522,1.55);
#1885=CYLINDRICAL_SURFACE('',#33528,3.);
#1886=CYLINDRICAL_SURFACE('',#33532,3.);
#1887=CYLINDRICAL_SURFACE('',#33538,1.7);
#1888=CYLINDRICAL_SURFACE('',#33540,1.7);
#1889=CYLINDRICAL_SURFACE('',#33545,2.015);
#1890=CYLINDRICAL_SURFACE('',#33556,1.4635);
#1891=CYLINDRICAL_SURFACE('',#33558,1.4635);
#1892=CYLINDRICAL_SURFACE('',#33559,1.4635);
#1893=CYLINDRICAL_SURFACE('',#33560,1.4635);
#1894=CYLINDRICAL_SURFACE('',#33561,1.4635);
#1895=CYLINDRICAL_SURFACE('',#33562,1.4635);
#1896=CYLINDRICAL_SURFACE('',#33563,1.4635);
#1897=CYLINDRICAL_SURFACE('',#33564,1.4635);
#1898=CYLINDRICAL_SURFACE('',#33565,1.4635);
#1899=CYLINDRICAL_SURFACE('',#33566,1.4635);
#1900=CYLINDRICAL_SURFACE('',#33567,1.4635);
#1901=CYLINDRICAL_SURFACE('',#33568,1.4635);
#1902=CYLINDRICAL_SURFACE('',#33569,1.4635);
#1903=CYLINDRICAL_SURFACE('',#33570,1.4635);
#1904=CYLINDRICAL_SURFACE('',#33571,1.4635);
#1905=CYLINDRICAL_SURFACE('',#33572,1.4635);
#1906=CYLINDRICAL_SURFACE('',#33573,1.4635);
#1907=CYLINDRICAL_SURFACE('',#33574,1.4635);
#1908=CYLINDRICAL_SURFACE('',#33575,1.4635);
#1909=CYLINDRICAL_SURFACE('',#33576,1.4635);
#1910=CYLINDRICAL_SURFACE('',#33577,1.4635);
#1911=CYLINDRICAL_SURFACE('',#33578,1.4635);
#1912=CYLINDRICAL_SURFACE('',#33579,1.4635);
#1913=CYLINDRICAL_SURFACE('',#33580,1.17775);
#1914=CYLINDRICAL_SURFACE('',#33582,1.17775);
#1915=CYLINDRICAL_SURFACE('',#33583,1.17775);
#1916=CYLINDRICAL_SURFACE('',#33584,1.17775);
#1917=CYLINDRICAL_SURFACE('',#33585,1.17775);
#1918=CYLINDRICAL_SURFACE('',#33586,1.17775);
#1919=CYLINDRICAL_SURFACE('',#33587,1.17775);
#1920=CYLINDRICAL_SURFACE('',#33588,1.17775);
#1921=CYLINDRICAL_SURFACE('',#33589,1.17775);
#1922=CYLINDRICAL_SURFACE('',#33590,1.17775);
#1923=CYLINDRICAL_SURFACE('',#33591,1.17775);
#1924=CYLINDRICAL_SURFACE('',#33592,1.17775);
#1925=CYLINDRICAL_SURFACE('',#33593,1.17775);
#1926=CYLINDRICAL_SURFACE('',#33594,1.17775);
#1927=CYLINDRICAL_SURFACE('',#33595,1.17775);
#1928=CYLINDRICAL_SURFACE('',#33596,1.17775);
#1929=CYLINDRICAL_SURFACE('',#33597,1.17775);
#1930=CYLINDRICAL_SURFACE('',#33598,1.17775);
#1931=CYLINDRICAL_SURFACE('',#33599,1.17775);
#1932=CYLINDRICAL_SURFACE('',#33600,1.17775);
#1933=CYLINDRICAL_SURFACE('',#33601,1.17775);
#1934=CYLINDRICAL_SURFACE('',#33602,1.17775);
#1935=CYLINDRICAL_SURFACE('',#33603,1.17775);
#1936=CYLINDRICAL_SURFACE('',#33604,1.17775);
#1937=CYLINDRICAL_SURFACE('',#33606,1.4635);
#1938=CYLINDRICAL_SURFACE('',#33626,2.75);
#1939=CYLINDRICAL_SURFACE('',#33819,1.39337567297406);
#1940=CYLINDRICAL_SURFACE('',#33821,1.39337567297406);
#1941=CYLINDRICAL_SURFACE('',#33823,1.39337567297406);
#1942=CYLINDRICAL_SURFACE('',#33825,1.39337567297406);
#1943=CYLINDRICAL_SURFACE('',#33827,1.39337567297406);
#1944=CYLINDRICAL_SURFACE('',#33829,1.39337567297406);
#1945=CYLINDRICAL_SURFACE('',#33857,1.4635);
#1946=CYLINDRICAL_SURFACE('',#33859,1.4635);
#1947=CYLINDRICAL_SURFACE('',#33860,1.4635);
#1948=CYLINDRICAL_SURFACE('',#33861,1.4635);
#1949=CYLINDRICAL_SURFACE('',#33862,1.4635);
#1950=CYLINDRICAL_SURFACE('',#33863,1.4635);
#1951=CYLINDRICAL_SURFACE('',#33864,1.4635);
#1952=CYLINDRICAL_SURFACE('',#33865,1.4635);
#1953=CYLINDRICAL_SURFACE('',#33866,1.4635);
#1954=CYLINDRICAL_SURFACE('',#33867,1.4635);
#1955=CYLINDRICAL_SURFACE('',#33868,1.4635);
#1956=CYLINDRICAL_SURFACE('',#33869,1.4635);
#1957=CYLINDRICAL_SURFACE('',#33870,1.4635);
#1958=CYLINDRICAL_SURFACE('',#33871,1.4635);
#1959=CYLINDRICAL_SURFACE('',#33872,1.4635);
#1960=CYLINDRICAL_SURFACE('',#33873,1.4635);
#1961=CYLINDRICAL_SURFACE('',#33874,1.4635);
#1962=CYLINDRICAL_SURFACE('',#33875,1.4635);
#1963=CYLINDRICAL_SURFACE('',#33876,1.4635);
#1964=CYLINDRICAL_SURFACE('',#33877,1.17775);
#1965=CYLINDRICAL_SURFACE('',#33879,1.17775);
#1966=CYLINDRICAL_SURFACE('',#33880,1.17775);
#1967=CYLINDRICAL_SURFACE('',#33881,1.17775);
#1968=CYLINDRICAL_SURFACE('',#33882,1.17775);
#1969=CYLINDRICAL_SURFACE('',#33883,1.17775);
#1970=CYLINDRICAL_SURFACE('',#33884,1.17775);
#1971=CYLINDRICAL_SURFACE('',#33885,1.17775);
#1972=CYLINDRICAL_SURFACE('',#33886,1.17775);
#1973=CYLINDRICAL_SURFACE('',#33887,1.17775);
#1974=CYLINDRICAL_SURFACE('',#33888,1.17775);
#1975=CYLINDRICAL_SURFACE('',#33889,1.17775);
#1976=CYLINDRICAL_SURFACE('',#33890,1.17775);
#1977=CYLINDRICAL_SURFACE('',#33891,1.17775);
#1978=CYLINDRICAL_SURFACE('',#33892,1.17775);
#1979=CYLINDRICAL_SURFACE('',#33893,1.17775);
#1980=CYLINDRICAL_SURFACE('',#33894,1.17775);
#1981=CYLINDRICAL_SURFACE('',#33895,1.17775);
#1982=CYLINDRICAL_SURFACE('',#33896,1.17775);
#1983=CYLINDRICAL_SURFACE('',#33897,1.17775);
#1984=CYLINDRICAL_SURFACE('',#33899,1.4635);
#1985=CYLINDRICAL_SURFACE('',#33919,2.75);
#1986=CYLINDRICAL_SURFACE('',#34112,1.39337567297406);
#1987=CYLINDRICAL_SURFACE('',#34114,1.39337567297406);
#1988=CYLINDRICAL_SURFACE('',#34116,1.39337567297406);
#1989=CYLINDRICAL_SURFACE('',#34118,1.39337567297406);
#1990=CYLINDRICAL_SURFACE('',#34120,1.39337567297406);
#1991=CYLINDRICAL_SURFACE('',#34122,1.39337567297406);
#1992=CYLINDRICAL_SURFACE('',#34150,0.96675);
#1993=CYLINDRICAL_SURFACE('',#34152,0.96675);
#1994=CYLINDRICAL_SURFACE('',#34153,0.96675);
#1995=CYLINDRICAL_SURFACE('',#34154,0.96675);
#1996=CYLINDRICAL_SURFACE('',#34155,0.96675);
#1997=CYLINDRICAL_SURFACE('',#34156,0.96675);
#1998=CYLINDRICAL_SURFACE('',#34157,0.96675);
#1999=CYLINDRICAL_SURFACE('',#34158,0.96675);
#2000=CYLINDRICAL_SURFACE('',#34159,0.96675);
#2001=CYLINDRICAL_SURFACE('',#34160,0.96675);
#2002=CYLINDRICAL_SURFACE('',#34161,0.96675);
#2003=CYLINDRICAL_SURFACE('',#34162,0.739000000000001);
#2004=CYLINDRICAL_SURFACE('',#34164,0.739000000000001);
#2005=CYLINDRICAL_SURFACE('',#34165,0.739000000000001);
#2006=CYLINDRICAL_SURFACE('',#34166,0.739000000000001);
#2007=CYLINDRICAL_SURFACE('',#34167,0.739000000000001);
#2008=CYLINDRICAL_SURFACE('',#34168,0.739000000000001);
#2009=CYLINDRICAL_SURFACE('',#34169,0.739000000000001);
#2010=CYLINDRICAL_SURFACE('',#34170,0.739000000000001);
#2011=CYLINDRICAL_SURFACE('',#34171,0.739000000000001);
#2012=CYLINDRICAL_SURFACE('',#34172,0.739000000000001);
#2013=CYLINDRICAL_SURFACE('',#34173,0.739000000000001);
#2014=CYLINDRICAL_SURFACE('',#34175,0.96675);
#2015=CYLINDRICAL_SURFACE('',#34191,1.9);
#2016=FACE_BOUND('',#5102,.T.);
#2017=FACE_BOUND('',#5103,.T.);
#2018=FACE_BOUND('',#5111,.T.);
#2019=FACE_BOUND('',#5112,.T.);
#2020=FACE_BOUND('',#5136,.T.);
#2021=FACE_BOUND('',#5137,.T.);
#2022=FACE_BOUND('',#5145,.T.);
#2023=FACE_BOUND('',#5146,.T.);
#2024=FACE_BOUND('',#5147,.T.);
#2025=FACE_BOUND('',#5148,.T.);
#2026=FACE_BOUND('',#5149,.T.);
#2027=FACE_BOUND('',#5150,.T.);
#2028=FACE_BOUND('',#5151,.T.);
#2029=FACE_BOUND('',#5152,.T.);
#2030=FACE_BOUND('',#5153,.T.);
#2031=FACE_BOUND('',#5154,.T.);
#2032=FACE_BOUND('',#5208,.T.);
#2033=FACE_BOUND('',#5211,.T.);
#2034=FACE_BOUND('',#5298,.T.);
#2035=FACE_BOUND('',#5300,.T.);
#2036=FACE_BOUND('',#5303,.T.);
#2037=FACE_BOUND('',#5476,.T.);
#2038=FACE_BOUND('',#5479,.T.);
#2039=FACE_BOUND('',#5480,.T.);
#2040=FACE_BOUND('',#5481,.T.);
#2041=FACE_BOUND('',#5482,.T.);
#2042=FACE_BOUND('',#5483,.T.);
#2043=FACE_BOUND('',#5484,.T.);
#2044=FACE_BOUND('',#5485,.T.);
#2045=FACE_BOUND('',#5486,.T.);
#2046=FACE_BOUND('',#5487,.T.);
#2047=FACE_BOUND('',#5488,.T.);
#2048=FACE_BOUND('',#5489,.T.);
#2049=FACE_BOUND('',#5490,.T.);
#2050=FACE_BOUND('',#5491,.T.);
#2051=FACE_BOUND('',#5492,.T.);
#2052=FACE_BOUND('',#5493,.T.);
#2053=FACE_BOUND('',#5494,.T.);
#2054=FACE_BOUND('',#5495,.T.);
#2055=FACE_BOUND('',#5496,.T.);
#2056=FACE_BOUND('',#5497,.T.);
#2057=FACE_BOUND('',#5498,.T.);
#2058=FACE_BOUND('',#5499,.T.);
#2059=FACE_BOUND('',#5500,.T.);
#2060=FACE_BOUND('',#5501,.T.);
#2061=FACE_BOUND('',#5502,.T.);
#2062=FACE_BOUND('',#5503,.T.);
#2063=FACE_BOUND('',#5504,.T.);
#2064=FACE_BOUND('',#5505,.T.);
#2065=FACE_BOUND('',#5506,.T.);
#2066=FACE_BOUND('',#5507,.T.);
#2067=FACE_BOUND('',#5508,.T.);
#2068=FACE_BOUND('',#5509,.T.);
#2069=FACE_BOUND('',#5510,.T.);
#2070=FACE_BOUND('',#5511,.T.);
#2071=FACE_BOUND('',#5512,.T.);
#2072=FACE_BOUND('',#5513,.T.);
#2073=FACE_BOUND('',#5514,.T.);
#2074=FACE_BOUND('',#5515,.T.);
#2075=FACE_BOUND('',#5518,.T.);
#2076=FACE_BOUND('',#5521,.T.);
#2077=FACE_BOUND('',#5523,.T.);
#2078=FACE_BOUND('',#5545,.T.);
#2079=FACE_BOUND('',#5561,.T.);
#2080=FACE_BOUND('',#5585,.T.);
#2081=FACE_BOUND('',#5639,.T.);
#2082=FACE_BOUND('',#5685,.T.);
#2083=FACE_BOUND('',#5718,.T.);
#2084=FACE_BOUND('',#5741,.T.);
#2085=FACE_BOUND('',#5774,.T.);
#2086=FACE_BOUND('',#5820,.T.);
#2087=FACE_BOUND('',#5874,.T.);
#2088=FACE_BOUND('',#5890,.T.);
#2089=FACE_BOUND('',#6329,.T.);
#2090=FACE_BOUND('',#6330,.T.);
#2091=FACE_BOUND('',#6331,.T.);
#2092=FACE_BOUND('',#6332,.T.);
#2093=FACE_BOUND('',#6333,.T.);
#2094=FACE_BOUND('',#6334,.T.);
#2095=FACE_BOUND('',#6335,.T.);
#2096=FACE_BOUND('',#6336,.T.);
#2097=FACE_BOUND('',#6337,.T.);
#2098=FACE_BOUND('',#6338,.T.);
#2099=FACE_BOUND('',#6339,.T.);
#2100=FACE_BOUND('',#6340,.T.);
#2101=FACE_BOUND('',#6341,.T.);
#2102=FACE_BOUND('',#6342,.T.);
#2103=FACE_BOUND('',#6343,.T.);
#2104=FACE_BOUND('',#6344,.T.);
#2105=FACE_BOUND('',#6345,.T.);
#2106=FACE_BOUND('',#6346,.T.);
#2107=FACE_BOUND('',#6347,.T.);
#2108=FACE_BOUND('',#6348,.T.);
#2109=FACE_BOUND('',#6349,.T.);
#2110=FACE_BOUND('',#6350,.T.);
#2111=FACE_BOUND('',#6351,.T.);
#2112=FACE_BOUND('',#6352,.T.);
#2113=FACE_BOUND('',#6353,.T.);
#2114=FACE_BOUND('',#6354,.T.);
#2115=FACE_BOUND('',#6355,.T.);
#2116=FACE_BOUND('',#6356,.T.);
#2117=FACE_BOUND('',#6357,.T.);
#2118=FACE_BOUND('',#6358,.T.);
#2119=FACE_BOUND('',#6359,.T.);
#2120=FACE_BOUND('',#6360,.T.);
#2121=FACE_BOUND('',#6361,.T.);
#2122=FACE_BOUND('',#6362,.T.);
#2123=FACE_BOUND('',#6363,.T.);
#2124=FACE_BOUND('',#6364,.T.);
#2125=FACE_BOUND('',#6365,.T.);
#2126=FACE_BOUND('',#6366,.T.);
#2127=FACE_BOUND('',#6367,.T.);
#2128=FACE_BOUND('',#6368,.T.);
#2129=FACE_BOUND('',#6369,.T.);
#2130=FACE_BOUND('',#6370,.T.);
#2131=FACE_BOUND('',#6371,.T.);
#2132=FACE_BOUND('',#6372,.T.);
#2133=FACE_BOUND('',#6373,.T.);
#2134=FACE_BOUND('',#6374,.T.);
#2135=FACE_BOUND('',#6375,.T.);
#2136=FACE_BOUND('',#6376,.T.);
#2137=FACE_BOUND('',#6377,.T.);
#2138=FACE_BOUND('',#6378,.T.);
#2139=FACE_BOUND('',#6379,.T.);
#2140=FACE_BOUND('',#6380,.T.);
#2141=FACE_BOUND('',#6381,.T.);
#2142=FACE_BOUND('',#6382,.T.);
#2143=FACE_BOUND('',#6383,.T.);
#2144=FACE_BOUND('',#6384,.T.);
#2145=FACE_BOUND('',#6385,.T.);
#2146=FACE_BOUND('',#6386,.T.);
#2147=FACE_BOUND('',#6387,.T.);
#2148=FACE_BOUND('',#6388,.T.);
#2149=FACE_BOUND('',#6389,.T.);
#2150=FACE_BOUND('',#6390,.T.);
#2151=FACE_BOUND('',#6391,.T.);
#2152=FACE_BOUND('',#6392,.T.);
#2153=FACE_BOUND('',#6393,.T.);
#2154=FACE_BOUND('',#6394,.T.);
#2155=FACE_BOUND('',#6395,.T.);
#2156=FACE_BOUND('',#6396,.T.);
#2157=FACE_BOUND('',#6397,.T.);
#2158=FACE_BOUND('',#6398,.T.);
#2159=FACE_BOUND('',#6399,.T.);
#2160=FACE_BOUND('',#6400,.T.);
#2161=FACE_BOUND('',#6401,.T.);
#2162=FACE_BOUND('',#6402,.T.);
#2163=FACE_BOUND('',#6403,.T.);
#2164=FACE_BOUND('',#6404,.T.);
#2165=FACE_BOUND('',#6405,.T.);
#2166=FACE_BOUND('',#6406,.T.);
#2167=FACE_BOUND('',#6407,.T.);
#2168=FACE_BOUND('',#6408,.T.);
#2169=FACE_BOUND('',#6409,.T.);
#2170=FACE_BOUND('',#6410,.T.);
#2171=FACE_BOUND('',#6411,.T.);
#2172=FACE_BOUND('',#6412,.T.);
#2173=FACE_BOUND('',#6413,.T.);
#2174=FACE_BOUND('',#6414,.T.);
#2175=FACE_BOUND('',#6415,.T.);
#2176=FACE_BOUND('',#6416,.T.);
#2177=FACE_BOUND('',#6417,.T.);
#2178=FACE_BOUND('',#6418,.T.);
#2179=FACE_BOUND('',#6419,.T.);
#2180=FACE_BOUND('',#6420,.T.);
#2181=FACE_BOUND('',#6421,.T.);
#2182=FACE_BOUND('',#6422,.T.);
#2183=FACE_BOUND('',#6423,.T.);
#2184=FACE_BOUND('',#6424,.T.);
#2185=FACE_BOUND('',#6425,.T.);
#2186=FACE_BOUND('',#6426,.T.);
#2187=FACE_BOUND('',#6427,.T.);
#2188=FACE_BOUND('',#6428,.T.);
#2189=FACE_BOUND('',#6429,.T.);
#2190=FACE_BOUND('',#6430,.T.);
#2191=FACE_BOUND('',#6431,.T.);
#2192=FACE_BOUND('',#6432,.T.);
#2193=FACE_BOUND('',#6434,.T.);
#2194=FACE_BOUND('',#6435,.T.);
#2195=FACE_BOUND('',#6494,.T.);
#2196=FACE_BOUND('',#6495,.T.);
#2197=FACE_BOUND('',#6498,.T.);
#2198=FACE_BOUND('',#6499,.T.);
#2199=FACE_BOUND('',#6504,.T.);
#2200=FACE_BOUND('',#6505,.T.);
#2201=FACE_BOUND('',#6506,.T.);
#2202=FACE_BOUND('',#6507,.T.);
#2203=FACE_BOUND('',#6508,.T.);
#2204=FACE_BOUND('',#6509,.T.);
#2205=FACE_BOUND('',#6510,.T.);
#2206=FACE_BOUND('',#6511,.T.);
#2207=FACE_BOUND('',#6512,.T.);
#2208=FACE_BOUND('',#6513,.T.);
#2209=FACE_BOUND('',#6514,.T.);
#2210=FACE_BOUND('',#6520,.T.);
#2211=FACE_BOUND('',#6521,.T.);
#2212=FACE_BOUND('',#6526,.T.);
#2213=FACE_BOUND('',#6529,.T.);
#2214=FACE_BOUND('',#6601,.T.);
#2215=FACE_BOUND('',#6605,.T.);
#2216=FACE_BOUND('',#6610,.T.);
#2217=FACE_BOUND('',#6614,.T.);
#2218=FACE_BOUND('',#6615,.T.);
#2219=FACE_BOUND('',#6616,.T.);
#2220=FACE_BOUND('',#6617,.T.);
#2221=FACE_BOUND('',#6618,.T.);
#2222=FACE_BOUND('',#6629,.T.);
#2223=FACE_BOUND('',#6631,.T.);
#2224=FACE_BOUND('',#6637,.T.);
#2225=FACE_BOUND('',#6638,.T.);
#2226=FACE_BOUND('',#6639,.T.);
#2227=FACE_BOUND('',#6701,.T.);
#2228=FACE_BOUND('',#6816,.T.);
#2229=FACE_BOUND('',#6889,.T.);
#2230=FACE_BOUND('',#7004,.T.);
#2231=FACE_BOUND('',#7059,.T.);
#2232=PLANE('',#32237);
#2233=PLANE('',#32250);
#2234=PLANE('',#32260);
#2235=PLANE('',#32261);
#2236=PLANE('',#32262);
#2237=PLANE('',#32263);
#2238=PLANE('',#32264);
#2239=PLANE('',#32265);
#2240=PLANE('',#32266);
#2241=PLANE('',#32267);
#2242=PLANE('',#32268);
#2243=PLANE('',#32269);
#2244=PLANE('',#32270);
#2245=PLANE('',#32271);
#2246=PLANE('',#32272);
#2247=PLANE('',#32273);
#2248=PLANE('',#32274);
#2249=PLANE('',#32275);
#2250=PLANE('',#32280);
#2251=PLANE('',#32295);
#2252=PLANE('',#32356);
#2253=PLANE('',#32357);
#2254=PLANE('',#32361);
#2255=PLANE('',#32363);
#2256=PLANE('',#32370);
#2257=PLANE('',#32371);
#2258=PLANE('',#32372);
#2259=PLANE('',#32373);
#2260=PLANE('',#32374);
#2261=PLANE('',#32375);
#2262=PLANE('',#32376);
#2263=PLANE('',#32377);
#2264=PLANE('',#32378);
#2265=PLANE('',#32379);
#2266=PLANE('',#32380);
#2267=PLANE('',#32381);
#2268=PLANE('',#32382);
#2269=PLANE('',#32383);
#2270=PLANE('',#32392);
#2271=PLANE('',#32396);
#2272=PLANE('',#32454);
#2273=PLANE('',#32456);
#2274=PLANE('',#32458);
#2275=PLANE('',#32459);
#2276=PLANE('',#32460);
#2277=PLANE('',#32461);
#2278=PLANE('',#32467);
#2279=PLANE('',#32470);
#2280=PLANE('',#32476);
#2281=PLANE('',#32491);
#2282=PLANE('',#32492);
#2283=PLANE('',#32493);
#2284=PLANE('',#32494);
#2285=PLANE('',#32495);
#2286=PLANE('',#32496);
#2287=PLANE('',#32497);
#2288=PLANE('',#32498);
#2289=PLANE('',#32499);
#2290=PLANE('',#32500);
#2291=PLANE('',#32501);
#2292=PLANE('',#32503);
#2293=PLANE('',#32505);
#2294=PLANE('',#32506);
#2295=PLANE('',#32508);
#2296=PLANE('',#32509);
#2297=PLANE('',#32511);
#2298=PLANE('',#32512);
#2299=PLANE('',#32514);
#2300=PLANE('',#32515);
#2301=PLANE('',#32517);
#2302=PLANE('',#32518);
#2303=PLANE('',#32520);
#2304=PLANE('',#32521);
#2305=PLANE('',#32523);
#2306=PLANE('',#32524);
#2307=PLANE('',#32526);
#2308=PLANE('',#32527);
#2309=PLANE('',#32529);
#2310=PLANE('',#32530);
#2311=PLANE('',#32532);
#2312=PLANE('',#32533);
#2313=PLANE('',#32535);
#2314=PLANE('',#32536);
#2315=PLANE('',#32538);
#2316=PLANE('',#32539);
#2317=PLANE('',#32541);
#2318=PLANE('',#32542);
#2319=PLANE('',#32544);
#2320=PLANE('',#32545);
#2321=PLANE('',#32547);
#2322=PLANE('',#32548);
#2323=PLANE('',#32550);
#2324=PLANE('',#32551);
#2325=PLANE('',#32553);
#2326=PLANE('',#32554);
#2327=PLANE('',#32556);
#2328=PLANE('',#32557);
#2329=PLANE('',#32559);
#2330=PLANE('',#32560);
#2331=PLANE('',#32562);
#2332=PLANE('',#32563);
#2333=PLANE('',#32565);
#2334=PLANE('',#32566);
#2335=PLANE('',#32568);
#2336=PLANE('',#32569);
#2337=PLANE('',#32571);
#2338=PLANE('',#32572);
#2339=PLANE('',#32574);
#2340=PLANE('',#32575);
#2341=PLANE('',#32577);
#2342=PLANE('',#32578);
#2343=PLANE('',#32580);
#2344=PLANE('',#32581);
#2345=PLANE('',#32583);
#2346=PLANE('',#32584);
#2347=PLANE('',#32586);
#2348=PLANE('',#32587);
#2349=PLANE('',#32589);
#2350=PLANE('',#32590);
#2351=PLANE('',#32592);
#2352=PLANE('',#32593);
#2353=PLANE('',#32595);
#2354=PLANE('',#32596);
#2355=PLANE('',#32598);
#2356=PLANE('',#32599);
#2357=PLANE('',#32601);
#2358=PLANE('',#32602);
#2359=PLANE('',#32604);
#2360=PLANE('',#32605);
#2361=PLANE('',#32607);
#2362=PLANE('',#32608);
#2363=PLANE('',#32610);
#2364=PLANE('',#32611);
#2365=PLANE('',#32613);
#2366=PLANE('',#32614);
#2367=PLANE('',#32617);
#2368=PLANE('',#32618);
#2369=PLANE('',#32621);
#2370=PLANE('',#32622);
#2371=PLANE('',#32624);
#2372=PLANE('',#32625);
#2373=PLANE('',#32627);
#2374=PLANE('',#32628);
#2375=PLANE('',#32630);
#2376=PLANE('',#32631);
#2377=PLANE('',#32633);
#2378=PLANE('',#32634);
#2379=PLANE('',#32636);
#2380=PLANE('',#32637);
#2381=PLANE('',#32639);
#2382=PLANE('',#32640);
#2383=PLANE('',#32642);
#2384=PLANE('',#32643);
#2385=PLANE('',#32645);
#2386=PLANE('',#32646);
#2387=PLANE('',#32648);
#2388=PLANE('',#32649);
#2389=PLANE('',#32651);
#2390=PLANE('',#32652);
#2391=PLANE('',#32654);
#2392=PLANE('',#32655);
#2393=PLANE('',#32657);
#2394=PLANE('',#32658);
#2395=PLANE('',#32660);
#2396=PLANE('',#32661);
#2397=PLANE('',#32663);
#2398=PLANE('',#32664);
#2399=PLANE('',#32666);
#2400=PLANE('',#32667);
#2401=PLANE('',#32669);
#2402=PLANE('',#32670);
#2403=PLANE('',#32672);
#2404=PLANE('',#32673);
#2405=PLANE('',#32675);
#2406=PLANE('',#32676);
#2407=PLANE('',#32678);
#2408=PLANE('',#32679);
#2409=PLANE('',#32681);
#2410=PLANE('',#32682);
#2411=PLANE('',#32684);
#2412=PLANE('',#32685);
#2413=PLANE('',#32687);
#2414=PLANE('',#32688);
#2415=PLANE('',#32690);
#2416=PLANE('',#32691);
#2417=PLANE('',#32693);
#2418=PLANE('',#32694);
#2419=PLANE('',#32696);
#2420=PLANE('',#32697);
#2421=PLANE('',#32699);
#2422=PLANE('',#32700);
#2423=PLANE('',#32702);
#2424=PLANE('',#32703);
#2425=PLANE('',#32705);
#2426=PLANE('',#32706);
#2427=PLANE('',#32708);
#2428=PLANE('',#32709);
#2429=PLANE('',#32711);
#2430=PLANE('',#32712);
#2431=PLANE('',#32714);
#2432=PLANE('',#32715);
#2433=PLANE('',#32717);
#2434=PLANE('',#32718);
#2435=PLANE('',#32720);
#2436=PLANE('',#32721);
#2437=PLANE('',#32723);
#2438=PLANE('',#32724);
#2439=PLANE('',#32726);
#2440=PLANE('',#32727);
#2441=PLANE('',#32729);
#2442=PLANE('',#32730);
#2443=PLANE('',#32732);
#2444=PLANE('',#32733);
#2445=PLANE('',#32735);
#2446=PLANE('',#32737);
#2447=PLANE('',#32742);
#2448=PLANE('',#32750);
#2449=PLANE('',#32754);
#2450=PLANE('',#32758);
#2451=PLANE('',#32759);
#2452=PLANE('',#32760);
#2453=PLANE('',#32761);
#2454=PLANE('',#32762);
#2455=PLANE('',#32763);
#2456=PLANE('',#32764);
#2457=PLANE('',#32765);
#2458=PLANE('',#32766);
#2459=PLANE('',#32767);
#2460=PLANE('',#32768);
#2461=PLANE('',#32769);
#2462=PLANE('',#32770);
#2463=PLANE('',#32771);
#2464=PLANE('',#32772);
#2465=PLANE('',#32773);
#2466=PLANE('',#32774);
#2467=PLANE('',#32775);
#2468=PLANE('',#32776);
#2469=PLANE('',#32777);
#2470=PLANE('',#32778);
#2471=PLANE('',#32779);
#2472=PLANE('',#32780);
#2473=PLANE('',#32781);
#2474=PLANE('',#32782);
#2475=PLANE('',#32783);
#2476=PLANE('',#32784);
#2477=PLANE('',#32785);
#2478=PLANE('',#32786);
#2479=PLANE('',#32787);
#2480=PLANE('',#32788);
#2481=PLANE('',#32789);
#2482=PLANE('',#32790);
#2483=PLANE('',#32791);
#2484=PLANE('',#32792);
#2485=PLANE('',#32793);
#2486=PLANE('',#32794);
#2487=PLANE('',#32795);
#2488=PLANE('',#32796);
#2489=PLANE('',#32797);
#2490=PLANE('',#32798);
#2491=PLANE('',#32799);
#2492=PLANE('',#32800);
#2493=PLANE('',#32801);
#2494=PLANE('',#32802);
#2495=PLANE('',#32803);
#2496=PLANE('',#32804);
#2497=PLANE('',#32805);
#2498=PLANE('',#32806);
#2499=PLANE('',#32807);
#2500=PLANE('',#32808);
#2501=PLANE('',#32809);
#2502=PLANE('',#32810);
#2503=PLANE('',#32811);
#2504=PLANE('',#32812);
#2505=PLANE('',#32813);
#2506=PLANE('',#32814);
#2507=PLANE('',#32815);
#2508=PLANE('',#32816);
#2509=PLANE('',#32817);
#2510=PLANE('',#32818);
#2511=PLANE('',#32819);
#2512=PLANE('',#32820);
#2513=PLANE('',#32821);
#2514=PLANE('',#32822);
#2515=PLANE('',#32823);
#2516=PLANE('',#32824);
#2517=PLANE('',#32825);
#2518=PLANE('',#32826);
#2519=PLANE('',#32827);
#2520=PLANE('',#32828);
#2521=PLANE('',#32829);
#2522=PLANE('',#32830);
#2523=PLANE('',#32831);
#2524=PLANE('',#32832);
#2525=PLANE('',#32833);
#2526=PLANE('',#32834);
#2527=PLANE('',#32835);
#2528=PLANE('',#32836);
#2529=PLANE('',#32837);
#2530=PLANE('',#32838);
#2531=PLANE('',#32839);
#2532=PLANE('',#32840);
#2533=PLANE('',#32841);
#2534=PLANE('',#32842);
#2535=PLANE('',#32843);
#2536=PLANE('',#32844);
#2537=PLANE('',#32845);
#2538=PLANE('',#32846);
#2539=PLANE('',#32847);
#2540=PLANE('',#32848);
#2541=PLANE('',#32849);
#2542=PLANE('',#32850);
#2543=PLANE('',#32851);
#2544=PLANE('',#32852);
#2545=PLANE('',#32853);
#2546=PLANE('',#32854);
#2547=PLANE('',#32855);
#2548=PLANE('',#32856);
#2549=PLANE('',#32857);
#2550=PLANE('',#32858);
#2551=PLANE('',#32859);
#2552=PLANE('',#32860);
#2553=PLANE('',#32861);
#2554=PLANE('',#32862);
#2555=PLANE('',#32863);
#2556=PLANE('',#32864);
#2557=PLANE('',#32865);
#2558=PLANE('',#32866);
#2559=PLANE('',#32867);
#2560=PLANE('',#32868);
#2561=PLANE('',#32869);
#2562=PLANE('',#32870);
#2563=PLANE('',#32871);
#2564=PLANE('',#32872);
#2565=PLANE('',#32873);
#2566=PLANE('',#32874);
#2567=PLANE('',#32875);
#2568=PLANE('',#32876);
#2569=PLANE('',#32877);
#2570=PLANE('',#32878);
#2571=PLANE('',#32879);
#2572=PLANE('',#32880);
#2573=PLANE('',#32881);
#2574=PLANE('',#32882);
#2575=PLANE('',#32883);
#2576=PLANE('',#32884);
#2577=PLANE('',#32885);
#2578=PLANE('',#32886);
#2579=PLANE('',#32887);
#2580=PLANE('',#32888);
#2581=PLANE('',#32889);
#2582=PLANE('',#32890);
#2583=PLANE('',#32891);
#2584=PLANE('',#32892);
#2585=PLANE('',#32893);
#2586=PLANE('',#32894);
#2587=PLANE('',#32895);
#2588=PLANE('',#32896);
#2589=PLANE('',#32897);
#2590=PLANE('',#32898);
#2591=PLANE('',#32899);
#2592=PLANE('',#32900);
#2593=PLANE('',#32901);
#2594=PLANE('',#32902);
#2595=PLANE('',#32903);
#2596=PLANE('',#32904);
#2597=PLANE('',#32905);
#2598=PLANE('',#32906);
#2599=PLANE('',#32907);
#2600=PLANE('',#32908);
#2601=PLANE('',#32909);
#2602=PLANE('',#32910);
#2603=PLANE('',#32911);
#2604=PLANE('',#32912);
#2605=PLANE('',#32913);
#2606=PLANE('',#32914);
#2607=PLANE('',#32915);
#2608=PLANE('',#32916);
#2609=PLANE('',#32917);
#2610=PLANE('',#32918);
#2611=PLANE('',#32919);
#2612=PLANE('',#32920);
#2613=PLANE('',#32921);
#2614=PLANE('',#32922);
#2615=PLANE('',#32923);
#2616=PLANE('',#32924);
#2617=PLANE('',#32925);
#2618=PLANE('',#32926);
#2619=PLANE('',#32927);
#2620=PLANE('',#32928);
#2621=PLANE('',#32929);
#2622=PLANE('',#32930);
#2623=PLANE('',#32931);
#2624=PLANE('',#32932);
#2625=PLANE('',#32933);
#2626=PLANE('',#32934);
#2627=PLANE('',#32935);
#2628=PLANE('',#32936);
#2629=PLANE('',#32937);
#2630=PLANE('',#32938);
#2631=PLANE('',#32939);
#2632=PLANE('',#32940);
#2633=PLANE('',#32941);
#2634=PLANE('',#32942);
#2635=PLANE('',#32943);
#2636=PLANE('',#32944);
#2637=PLANE('',#32945);
#2638=PLANE('',#32946);
#2639=PLANE('',#32947);
#2640=PLANE('',#32948);
#2641=PLANE('',#32949);
#2642=PLANE('',#32950);
#2643=PLANE('',#32951);
#2644=PLANE('',#32952);
#2645=PLANE('',#32953);
#2646=PLANE('',#32954);
#2647=PLANE('',#32955);
#2648=PLANE('',#32956);
#2649=PLANE('',#32957);
#2650=PLANE('',#32958);
#2651=PLANE('',#32959);
#2652=PLANE('',#32960);
#2653=PLANE('',#32961);
#2654=PLANE('',#32962);
#2655=PLANE('',#32963);
#2656=PLANE('',#32964);
#2657=PLANE('',#32965);
#2658=PLANE('',#32966);
#2659=PLANE('',#32967);
#2660=PLANE('',#32968);
#2661=PLANE('',#32969);
#2662=PLANE('',#32970);
#2663=PLANE('',#32971);
#2664=PLANE('',#32972);
#2665=PLANE('',#32973);
#2666=PLANE('',#32974);
#2667=PLANE('',#32975);
#2668=PLANE('',#32976);
#2669=PLANE('',#32977);
#2670=PLANE('',#32978);
#2671=PLANE('',#32979);
#2672=PLANE('',#32980);
#2673=PLANE('',#32981);
#2674=PLANE('',#32982);
#2675=PLANE('',#32983);
#2676=PLANE('',#32984);
#2677=PLANE('',#32985);
#2678=PLANE('',#32986);
#2679=PLANE('',#32987);
#2680=PLANE('',#32988);
#2681=PLANE('',#32989);
#2682=PLANE('',#32990);
#2683=PLANE('',#32991);
#2684=PLANE('',#32992);
#2685=PLANE('',#32993);
#2686=PLANE('',#32994);
#2687=PLANE('',#32995);
#2688=PLANE('',#32996);
#2689=PLANE('',#32997);
#2690=PLANE('',#32998);
#2691=PLANE('',#32999);
#2692=PLANE('',#33000);
#2693=PLANE('',#33001);
#2694=PLANE('',#33002);
#2695=PLANE('',#33003);
#2696=PLANE('',#33004);
#2697=PLANE('',#33005);
#2698=PLANE('',#33006);
#2699=PLANE('',#33007);
#2700=PLANE('',#33008);
#2701=PLANE('',#33009);
#2702=PLANE('',#33010);
#2703=PLANE('',#33011);
#2704=PLANE('',#33012);
#2705=PLANE('',#33013);
#2706=PLANE('',#33014);
#2707=PLANE('',#33015);
#2708=PLANE('',#33016);
#2709=PLANE('',#33017);
#2710=PLANE('',#33018);
#2711=PLANE('',#33019);
#2712=PLANE('',#33020);
#2713=PLANE('',#33021);
#2714=PLANE('',#33022);
#2715=PLANE('',#33023);
#2716=PLANE('',#33024);
#2717=PLANE('',#33025);
#2718=PLANE('',#33026);
#2719=PLANE('',#33027);
#2720=PLANE('',#33028);
#2721=PLANE('',#33029);
#2722=PLANE('',#33030);
#2723=PLANE('',#33031);
#2724=PLANE('',#33032);
#2725=PLANE('',#33033);
#2726=PLANE('',#33034);
#2727=PLANE('',#33035);
#2728=PLANE('',#33036);
#2729=PLANE('',#33037);
#2730=PLANE('',#33038);
#2731=PLANE('',#33039);
#2732=PLANE('',#33040);
#2733=PLANE('',#33041);
#2734=PLANE('',#33042);
#2735=PLANE('',#33043);
#2736=PLANE('',#33044);
#2737=PLANE('',#33045);
#2738=PLANE('',#33046);
#2739=PLANE('',#33047);
#2740=PLANE('',#33048);
#2741=PLANE('',#33049);
#2742=PLANE('',#33050);
#2743=PLANE('',#33051);
#2744=PLANE('',#33052);
#2745=PLANE('',#33053);
#2746=PLANE('',#33054);
#2747=PLANE('',#33055);
#2748=PLANE('',#33056);
#2749=PLANE('',#33057);
#2750=PLANE('',#33058);
#2751=PLANE('',#33059);
#2752=PLANE('',#33060);
#2753=PLANE('',#33061);
#2754=PLANE('',#33062);
#2755=PLANE('',#33063);
#2756=PLANE('',#33064);
#2757=PLANE('',#33065);
#2758=PLANE('',#33066);
#2759=PLANE('',#33067);
#2760=PLANE('',#33068);
#2761=PLANE('',#33069);
#2762=PLANE('',#33070);
#2763=PLANE('',#33071);
#2764=PLANE('',#33072);
#2765=PLANE('',#33073);
#2766=PLANE('',#33074);
#2767=PLANE('',#33075);
#2768=PLANE('',#33076);
#2769=PLANE('',#33077);
#2770=PLANE('',#33078);
#2771=PLANE('',#33079);
#2772=PLANE('',#33080);
#2773=PLANE('',#33081);
#2774=PLANE('',#33082);
#2775=PLANE('',#33083);
#2776=PLANE('',#33084);
#2777=PLANE('',#33085);
#2778=PLANE('',#33086);
#2779=PLANE('',#33087);
#2780=PLANE('',#33088);
#2781=PLANE('',#33089);
#2782=PLANE('',#33090);
#2783=PLANE('',#33091);
#2784=PLANE('',#33092);
#2785=PLANE('',#33093);
#2786=PLANE('',#33094);
#2787=PLANE('',#33095);
#2788=PLANE('',#33096);
#2789=PLANE('',#33097);
#2790=PLANE('',#33098);
#2791=PLANE('',#33099);
#2792=PLANE('',#33100);
#2793=PLANE('',#33101);
#2794=PLANE('',#33102);
#2795=PLANE('',#33103);
#2796=PLANE('',#33104);
#2797=PLANE('',#33105);
#2798=PLANE('',#33106);
#2799=PLANE('',#33107);
#2800=PLANE('',#33108);
#2801=PLANE('',#33109);
#2802=PLANE('',#33110);
#2803=PLANE('',#33111);
#2804=PLANE('',#33112);
#2805=PLANE('',#33113);
#2806=PLANE('',#33114);
#2807=PLANE('',#33115);
#2808=PLANE('',#33116);
#2809=PLANE('',#33117);
#2810=PLANE('',#33118);
#2811=PLANE('',#33119);
#2812=PLANE('',#33120);
#2813=PLANE('',#33121);
#2814=PLANE('',#33122);
#2815=PLANE('',#33123);
#2816=PLANE('',#33124);
#2817=PLANE('',#33125);
#2818=PLANE('',#33126);
#2819=PLANE('',#33127);
#2820=PLANE('',#33128);
#2821=PLANE('',#33129);
#2822=PLANE('',#33130);
#2823=PLANE('',#33131);
#2824=PLANE('',#33132);
#2825=PLANE('',#33133);
#2826=PLANE('',#33134);
#2827=PLANE('',#33135);
#2828=PLANE('',#33136);
#2829=PLANE('',#33137);
#2830=PLANE('',#33138);
#2831=PLANE('',#33139);
#2832=PLANE('',#33140);
#2833=PLANE('',#33141);
#2834=PLANE('',#33142);
#2835=PLANE('',#33143);
#2836=PLANE('',#33144);
#2837=PLANE('',#33145);
#2838=PLANE('',#33146);
#2839=PLANE('',#33147);
#2840=PLANE('',#33148);
#2841=PLANE('',#33149);
#2842=PLANE('',#33150);
#2843=PLANE('',#33151);
#2844=PLANE('',#33152);
#2845=PLANE('',#33153);
#2846=PLANE('',#33154);
#2847=PLANE('',#33155);
#2848=PLANE('',#33156);
#2849=PLANE('',#33157);
#2850=PLANE('',#33158);
#2851=PLANE('',#33159);
#2852=PLANE('',#33160);
#2853=PLANE('',#33161);
#2854=PLANE('',#33162);
#2855=PLANE('',#33163);
#2856=PLANE('',#33164);
#2857=PLANE('',#33165);
#2858=PLANE('',#33166);
#2859=PLANE('',#33167);
#2860=PLANE('',#33168);
#2861=PLANE('',#33169);
#2862=PLANE('',#33170);
#2863=PLANE('',#33171);
#2864=PLANE('',#33172);
#2865=PLANE('',#33173);
#2866=PLANE('',#33174);
#2867=PLANE('',#33175);
#2868=PLANE('',#33176);
#2869=PLANE('',#33177);
#2870=PLANE('',#33178);
#2871=PLANE('',#33179);
#2872=PLANE('',#33180);
#2873=PLANE('',#33181);
#2874=PLANE('',#33182);
#2875=PLANE('',#33183);
#2876=PLANE('',#33184);
#2877=PLANE('',#33185);
#2878=PLANE('',#33186);
#2879=PLANE('',#33187);
#2880=PLANE('',#33188);
#2881=PLANE('',#33189);
#2882=PLANE('',#33190);
#2883=PLANE('',#33191);
#2884=PLANE('',#33192);
#2885=PLANE('',#33193);
#2886=PLANE('',#33194);
#2887=PLANE('',#33195);
#2888=PLANE('',#33196);
#2889=PLANE('',#33197);
#2890=PLANE('',#33198);
#2891=PLANE('',#33199);
#2892=PLANE('',#33200);
#2893=PLANE('',#33201);
#2894=PLANE('',#33202);
#2895=PLANE('',#33203);
#2896=PLANE('',#33204);
#2897=PLANE('',#33205);
#2898=PLANE('',#33206);
#2899=PLANE('',#33207);
#2900=PLANE('',#33208);
#2901=PLANE('',#33209);
#2902=PLANE('',#33210);
#2903=PLANE('',#33211);
#2904=PLANE('',#33212);
#2905=PLANE('',#33213);
#2906=PLANE('',#33214);
#2907=PLANE('',#33215);
#2908=PLANE('',#33216);
#2909=PLANE('',#33217);
#2910=PLANE('',#33218);
#2911=PLANE('',#33219);
#2912=PLANE('',#33220);
#2913=PLANE('',#33221);
#2914=PLANE('',#33222);
#2915=PLANE('',#33223);
#2916=PLANE('',#33224);
#2917=PLANE('',#33225);
#2918=PLANE('',#33226);
#2919=PLANE('',#33227);
#2920=PLANE('',#33228);
#2921=PLANE('',#33229);
#2922=PLANE('',#33230);
#2923=PLANE('',#33231);
#2924=PLANE('',#33232);
#2925=PLANE('',#33233);
#2926=PLANE('',#33234);
#2927=PLANE('',#33235);
#2928=PLANE('',#33236);
#2929=PLANE('',#33237);
#2930=PLANE('',#33238);
#2931=PLANE('',#33239);
#2932=PLANE('',#33240);
#2933=PLANE('',#33241);
#2934=PLANE('',#33242);
#2935=PLANE('',#33243);
#2936=PLANE('',#33244);
#2937=PLANE('',#33245);
#2938=PLANE('',#33246);
#2939=PLANE('',#33247);
#2940=PLANE('',#33248);
#2941=PLANE('',#33249);
#2942=PLANE('',#33250);
#2943=PLANE('',#33251);
#2944=PLANE('',#33252);
#2945=PLANE('',#33253);
#2946=PLANE('',#33254);
#2947=PLANE('',#33255);
#2948=PLANE('',#33256);
#2949=PLANE('',#33257);
#2950=PLANE('',#33258);
#2951=PLANE('',#33259);
#2952=PLANE('',#33260);
#2953=PLANE('',#33261);
#2954=PLANE('',#33262);
#2955=PLANE('',#33269);
#2956=PLANE('',#33273);
#2957=PLANE('',#33277);
#2958=PLANE('',#33281);
#2959=PLANE('',#33285);
#2960=PLANE('',#33286);
#2961=PLANE('',#33288);
#2962=PLANE('',#33289);
#2963=PLANE('',#33290);
#2964=PLANE('',#33291);
#2965=PLANE('',#33292);
#2966=PLANE('',#33293);
#2967=PLANE('',#33294);
#2968=PLANE('',#33295);
#2969=PLANE('',#33296);
#2970=PLANE('',#33297);
#2971=PLANE('',#33298);
#2972=PLANE('',#33299);
#2973=PLANE('',#33300);
#2974=PLANE('',#33301);
#2975=PLANE('',#33302);
#2976=PLANE('',#33303);
#2977=PLANE('',#33304);
#2978=PLANE('',#33305);
#2979=PLANE('',#33306);
#2980=PLANE('',#33307);
#2981=PLANE('',#33308);
#2982=PLANE('',#33309);
#2983=PLANE('',#33310);
#2984=PLANE('',#33311);
#2985=PLANE('',#33312);
#2986=PLANE('',#33313);
#2987=PLANE('',#33314);
#2988=PLANE('',#33315);
#2989=PLANE('',#33316);
#2990=PLANE('',#33317);
#2991=PLANE('',#33318);
#2992=PLANE('',#33319);
#2993=PLANE('',#33320);
#2994=PLANE('',#33321);
#2995=PLANE('',#33322);
#2996=PLANE('',#33323);
#2997=PLANE('',#33324);
#2998=PLANE('',#33325);
#2999=PLANE('',#33326);
#3000=PLANE('',#33327);
#3001=PLANE('',#33328);
#3002=PLANE('',#33329);
#3003=PLANE('',#33330);
#3004=PLANE('',#33331);
#3005=PLANE('',#33332);
#3006=PLANE('',#33333);
#3007=PLANE('',#33334);
#3008=PLANE('',#33335);
#3009=PLANE('',#33336);
#3010=PLANE('',#33337);
#3011=PLANE('',#33338);
#3012=PLANE('',#33339);
#3013=PLANE('',#33340);
#3014=PLANE('',#33341);
#3015=PLANE('',#33342);
#3016=PLANE('',#33349);
#3017=PLANE('',#33350);
#3018=PLANE('',#33351);
#3019=PLANE('',#33352);
#3020=PLANE('',#33353);
#3021=PLANE('',#33354);
#3022=PLANE('',#33355);
#3023=PLANE('',#33356);
#3024=PLANE('',#33357);
#3025=PLANE('',#33358);
#3026=PLANE('',#33363);
#3027=PLANE('',#33371);
#3028=PLANE('',#33374);
#3029=PLANE('',#33378);
#3030=PLANE('',#33388);
#3031=PLANE('',#33389);
#3032=PLANE('',#33394);
#3033=PLANE('',#33397);
#3034=PLANE('',#33402);
#3035=PLANE('',#33405);
#3036=PLANE('',#33406);
#3037=PLANE('',#33407);
#3038=PLANE('',#33408);
#3039=PLANE('',#33409);
#3040=PLANE('',#33410);
#3041=PLANE('',#33411);
#3042=PLANE('',#33436);
#3043=PLANE('',#33439);
#3044=PLANE('',#33462);
#3045=PLANE('',#33463);
#3046=PLANE('',#33464);
#3047=PLANE('',#33465);
#3048=PLANE('',#33466);
#3049=PLANE('',#33467);
#3050=PLANE('',#33468);
#3051=PLANE('',#33469);
#3052=PLANE('',#33470);
#3053=PLANE('',#33471);
#3054=PLANE('',#33473);
#3055=PLANE('',#33475);
#3056=PLANE('',#33477);
#3057=PLANE('',#33479);
#3058=PLANE('',#33481);
#3059=PLANE('',#33484);
#3060=PLANE('',#33485);
#3061=PLANE('',#33486);
#3062=PLANE('',#33487);
#3063=PLANE('',#33492);
#3064=PLANE('',#33500);
#3065=PLANE('',#33508);
#3066=PLANE('',#33513);
#3067=PLANE('',#33534);
#3068=PLANE('',#33536);
#3069=PLANE('',#33547);
#3070=PLANE('',#33549);
#3071=PLANE('',#33550);
#3072=PLANE('',#33551);
#3073=PLANE('',#33552);
#3074=PLANE('',#33553);
#3075=PLANE('',#33554);
#3076=PLANE('',#33608);
#3077=PLANE('',#33611);
#3078=PLANE('',#33617);
#3079=PLANE('',#33621);
#3080=PLANE('',#33622);
#3081=PLANE('',#33624);
#3082=PLANE('',#33625);
#3083=PLANE('',#33701);
#3084=PLANE('',#33702);
#3085=PLANE('',#33703);
#3086=PLANE('',#33706);
#3087=PLANE('',#33707);
#3088=PLANE('',#33708);
#3089=PLANE('',#33709);
#3090=PLANE('',#33710);
#3091=PLANE('',#33711);
#3092=PLANE('',#33712);
#3093=PLANE('',#33713);
#3094=PLANE('',#33714);
#3095=PLANE('',#33715);
#3096=PLANE('',#33716);
#3097=PLANE('',#33717);
#3098=PLANE('',#33718);
#3099=PLANE('',#33719);
#3100=PLANE('',#33720);
#3101=PLANE('',#33721);
#3102=PLANE('',#33722);
#3103=PLANE('',#33723);
#3104=PLANE('',#33724);
#3105=PLANE('',#33725);
#3106=PLANE('',#33726);
#3107=PLANE('',#33727);
#3108=PLANE('',#33728);
#3109=PLANE('',#33729);
#3110=PLANE('',#33730);
#3111=PLANE('',#33731);
#3112=PLANE('',#33732);
#3113=PLANE('',#33733);
#3114=PLANE('',#33734);
#3115=PLANE('',#33735);
#3116=PLANE('',#33736);
#3117=PLANE('',#33737);
#3118=PLANE('',#33738);
#3119=PLANE('',#33739);
#3120=PLANE('',#33740);
#3121=PLANE('',#33741);
#3122=PLANE('',#33742);
#3123=PLANE('',#33743);
#3124=PLANE('',#33744);
#3125=PLANE('',#33745);
#3126=PLANE('',#33746);
#3127=PLANE('',#33747);
#3128=PLANE('',#33748);
#3129=PLANE('',#33749);
#3130=PLANE('',#33750);
#3131=PLANE('',#33751);
#3132=PLANE('',#33752);
#3133=PLANE('',#33753);
#3134=PLANE('',#33754);
#3135=PLANE('',#33755);
#3136=PLANE('',#33756);
#3137=PLANE('',#33757);
#3138=PLANE('',#33758);
#3139=PLANE('',#33759);
#3140=PLANE('',#33760);
#3141=PLANE('',#33761);
#3142=PLANE('',#33762);
#3143=PLANE('',#33763);
#3144=PLANE('',#33764);
#3145=PLANE('',#33765);
#3146=PLANE('',#33766);
#3147=PLANE('',#33767);
#3148=PLANE('',#33768);
#3149=PLANE('',#33769);
#3150=PLANE('',#33770);
#3151=PLANE('',#33771);
#3152=PLANE('',#33772);
#3153=PLANE('',#33773);
#3154=PLANE('',#33774);
#3155=PLANE('',#33775);
#3156=PLANE('',#33776);
#3157=PLANE('',#33777);
#3158=PLANE('',#33778);
#3159=PLANE('',#33779);
#3160=PLANE('',#33780);
#3161=PLANE('',#33781);
#3162=PLANE('',#33782);
#3163=PLANE('',#33783);
#3164=PLANE('',#33784);
#3165=PLANE('',#33785);
#3166=PLANE('',#33786);
#3167=PLANE('',#33787);
#3168=PLANE('',#33788);
#3169=PLANE('',#33789);
#3170=PLANE('',#33790);
#3171=PLANE('',#33791);
#3172=PLANE('',#33792);
#3173=PLANE('',#33793);
#3174=PLANE('',#33794);
#3175=PLANE('',#33795);
#3176=PLANE('',#33796);
#3177=PLANE('',#33797);
#3178=PLANE('',#33798);
#3179=PLANE('',#33799);
#3180=PLANE('',#33800);
#3181=PLANE('',#33801);
#3182=PLANE('',#33802);
#3183=PLANE('',#33803);
#3184=PLANE('',#33804);
#3185=PLANE('',#33805);
#3186=PLANE('',#33806);
#3187=PLANE('',#33807);
#3188=PLANE('',#33810);
#3189=PLANE('',#33831);
#3190=PLANE('',#33832);
#3191=PLANE('',#33833);
#3192=PLANE('',#33834);
#3193=PLANE('',#33835);
#3194=PLANE('',#33836);
#3195=PLANE('',#33837);
#3196=PLANE('',#33838);
#3197=PLANE('',#33839);
#3198=PLANE('',#33840);
#3199=PLANE('',#33842);
#3200=PLANE('',#33844);
#3201=PLANE('',#33846);
#3202=PLANE('',#33848);
#3203=PLANE('',#33850);
#3204=PLANE('',#33853);
#3205=PLANE('',#33854);
#3206=PLANE('',#33855);
#3207=PLANE('',#33901);
#3208=PLANE('',#33904);
#3209=PLANE('',#33910);
#3210=PLANE('',#33914);
#3211=PLANE('',#33915);
#3212=PLANE('',#33917);
#3213=PLANE('',#33918);
#3214=PLANE('',#33994);
#3215=PLANE('',#33995);
#3216=PLANE('',#33996);
#3217=PLANE('',#33999);
#3218=PLANE('',#34000);
#3219=PLANE('',#34001);
#3220=PLANE('',#34002);
#3221=PLANE('',#34003);
#3222=PLANE('',#34004);
#3223=PLANE('',#34005);
#3224=PLANE('',#34006);
#3225=PLANE('',#34007);
#3226=PLANE('',#34008);
#3227=PLANE('',#34009);
#3228=PLANE('',#34010);
#3229=PLANE('',#34011);
#3230=PLANE('',#34012);
#3231=PLANE('',#34013);
#3232=PLANE('',#34014);
#3233=PLANE('',#34015);
#3234=PLANE('',#34016);
#3235=PLANE('',#34017);
#3236=PLANE('',#34018);
#3237=PLANE('',#34019);
#3238=PLANE('',#34020);
#3239=PLANE('',#34021);
#3240=PLANE('',#34022);
#3241=PLANE('',#34023);
#3242=PLANE('',#34024);
#3243=PLANE('',#34025);
#3244=PLANE('',#34026);
#3245=PLANE('',#34027);
#3246=PLANE('',#34028);
#3247=PLANE('',#34029);
#3248=PLANE('',#34030);
#3249=PLANE('',#34031);
#3250=PLANE('',#34032);
#3251=PLANE('',#34033);
#3252=PLANE('',#34034);
#3253=PLANE('',#34035);
#3254=PLANE('',#34036);
#3255=PLANE('',#34037);
#3256=PLANE('',#34038);
#3257=PLANE('',#34039);
#3258=PLANE('',#34040);
#3259=PLANE('',#34041);
#3260=PLANE('',#34042);
#3261=PLANE('',#34043);
#3262=PLANE('',#34044);
#3263=PLANE('',#34045);
#3264=PLANE('',#34046);
#3265=PLANE('',#34047);
#3266=PLANE('',#34048);
#3267=PLANE('',#34049);
#3268=PLANE('',#34050);
#3269=PLANE('',#34051);
#3270=PLANE('',#34052);
#3271=PLANE('',#34053);
#3272=PLANE('',#34054);
#3273=PLANE('',#34055);
#3274=PLANE('',#34056);
#3275=PLANE('',#34057);
#3276=PLANE('',#34058);
#3277=PLANE('',#34059);
#3278=PLANE('',#34060);
#3279=PLANE('',#34061);
#3280=PLANE('',#34062);
#3281=PLANE('',#34063);
#3282=PLANE('',#34064);
#3283=PLANE('',#34065);
#3284=PLANE('',#34066);
#3285=PLANE('',#34067);
#3286=PLANE('',#34068);
#3287=PLANE('',#34069);
#3288=PLANE('',#34070);
#3289=PLANE('',#34071);
#3290=PLANE('',#34072);
#3291=PLANE('',#34073);
#3292=PLANE('',#34074);
#3293=PLANE('',#34075);
#3294=PLANE('',#34076);
#3295=PLANE('',#34077);
#3296=PLANE('',#34078);
#3297=PLANE('',#34079);
#3298=PLANE('',#34080);
#3299=PLANE('',#34081);
#3300=PLANE('',#34082);
#3301=PLANE('',#34083);
#3302=PLANE('',#34084);
#3303=PLANE('',#34085);
#3304=PLANE('',#34086);
#3305=PLANE('',#34087);
#3306=PLANE('',#34088);
#3307=PLANE('',#34089);
#3308=PLANE('',#34090);
#3309=PLANE('',#34091);
#3310=PLANE('',#34092);
#3311=PLANE('',#34093);
#3312=PLANE('',#34094);
#3313=PLANE('',#34095);
#3314=PLANE('',#34096);
#3315=PLANE('',#34097);
#3316=PLANE('',#34098);
#3317=PLANE('',#34099);
#3318=PLANE('',#34100);
#3319=PLANE('',#34103);
#3320=PLANE('',#34124);
#3321=PLANE('',#34125);
#3322=PLANE('',#34126);
#3323=PLANE('',#34127);
#3324=PLANE('',#34128);
#3325=PLANE('',#34129);
#3326=PLANE('',#34130);
#3327=PLANE('',#34131);
#3328=PLANE('',#34132);
#3329=PLANE('',#34133);
#3330=PLANE('',#34135);
#3331=PLANE('',#34137);
#3332=PLANE('',#34139);
#3333=PLANE('',#34141);
#3334=PLANE('',#34143);
#3335=PLANE('',#34146);
#3336=PLANE('',#34147);
#3337=PLANE('',#34148);
#3338=PLANE('',#34177);
#3339=PLANE('',#34183);
#3340=PLANE('',#34185);
#3341=PLANE('',#34189);
#3342=PLANE('',#34190);
#3343=PLANE('',#34194);
#3344=PLANE('',#34196);
#3345=PLANE('',#34199);
#3346=FACE_OUTER_BOUND('',#5100,.T.);
#3347=FACE_OUTER_BOUND('',#5101,.T.);
#3348=FACE_OUTER_BOUND('',#5104,.T.);
#3349=FACE_OUTER_BOUND('',#5105,.T.);
#3350=FACE_OUTER_BOUND('',#5106,.T.);
#3351=FACE_OUTER_BOUND('',#5107,.T.);
#3352=FACE_OUTER_BOUND('',#5108,.T.);
#3353=FACE_OUTER_BOUND('',#5109,.T.);
#3354=FACE_OUTER_BOUND('',#5110,.T.);
#3355=FACE_OUTER_BOUND('',#5113,.T.);
#3356=FACE_OUTER_BOUND('',#5114,.T.);
#3357=FACE_OUTER_BOUND('',#5115,.T.);
#3358=FACE_OUTER_BOUND('',#5116,.T.);
#3359=FACE_OUTER_BOUND('',#5117,.T.);
#3360=FACE_OUTER_BOUND('',#5118,.T.);
#3361=FACE_OUTER_BOUND('',#5119,.T.);
#3362=FACE_OUTER_BOUND('',#5120,.T.);
#3363=FACE_OUTER_BOUND('',#5121,.T.);
#3364=FACE_OUTER_BOUND('',#5122,.T.);
#3365=FACE_OUTER_BOUND('',#5123,.T.);
#3366=FACE_OUTER_BOUND('',#5124,.T.);
#3367=FACE_OUTER_BOUND('',#5125,.T.);
#3368=FACE_OUTER_BOUND('',#5126,.T.);
#3369=FACE_OUTER_BOUND('',#5127,.T.);
#3370=FACE_OUTER_BOUND('',#5128,.T.);
#3371=FACE_OUTER_BOUND('',#5129,.T.);
#3372=FACE_OUTER_BOUND('',#5130,.T.);
#3373=FACE_OUTER_BOUND('',#5131,.T.);
#3374=FACE_OUTER_BOUND('',#5132,.T.);
#3375=FACE_OUTER_BOUND('',#5133,.T.);
#3376=FACE_OUTER_BOUND('',#5134,.T.);
#3377=FACE_OUTER_BOUND('',#5135,.T.);
#3378=FACE_OUTER_BOUND('',#5138,.T.);
#3379=FACE_OUTER_BOUND('',#5139,.T.);
#3380=FACE_OUTER_BOUND('',#5140,.T.);
#3381=FACE_OUTER_BOUND('',#5141,.T.);
#3382=FACE_OUTER_BOUND('',#5142,.T.);
#3383=FACE_OUTER_BOUND('',#5143,.T.);
#3384=FACE_OUTER_BOUND('',#5144,.T.);
#3385=FACE_OUTER_BOUND('',#5155,.T.);
#3386=FACE_OUTER_BOUND('',#5156,.T.);
#3387=FACE_OUTER_BOUND('',#5157,.T.);
#3388=FACE_OUTER_BOUND('',#5158,.T.);
#3389=FACE_OUTER_BOUND('',#5159,.T.);
#3390=FACE_OUTER_BOUND('',#5160,.T.);
#3391=FACE_OUTER_BOUND('',#5161,.T.);
#3392=FACE_OUTER_BOUND('',#5162,.T.);
#3393=FACE_OUTER_BOUND('',#5163,.T.);
#3394=FACE_OUTER_BOUND('',#5164,.T.);
#3395=FACE_OUTER_BOUND('',#5165,.T.);
#3396=FACE_OUTER_BOUND('',#5166,.T.);
#3397=FACE_OUTER_BOUND('',#5167,.T.);
#3398=FACE_OUTER_BOUND('',#5168,.T.);
#3399=FACE_OUTER_BOUND('',#5169,.T.);
#3400=FACE_OUTER_BOUND('',#5170,.T.);
#3401=FACE_OUTER_BOUND('',#5171,.T.);
#3402=FACE_OUTER_BOUND('',#5172,.T.);
#3403=FACE_OUTER_BOUND('',#5173,.T.);
#3404=FACE_OUTER_BOUND('',#5174,.T.);
#3405=FACE_OUTER_BOUND('',#5175,.T.);
#3406=FACE_OUTER_BOUND('',#5176,.T.);
#3407=FACE_OUTER_BOUND('',#5177,.T.);
#3408=FACE_OUTER_BOUND('',#5178,.T.);
#3409=FACE_OUTER_BOUND('',#5179,.T.);
#3410=FACE_OUTER_BOUND('',#5180,.T.);
#3411=FACE_OUTER_BOUND('',#5181,.T.);
#3412=FACE_OUTER_BOUND('',#5182,.T.);
#3413=FACE_OUTER_BOUND('',#5183,.T.);
#3414=FACE_OUTER_BOUND('',#5184,.T.);
#3415=FACE_OUTER_BOUND('',#5185,.T.);
#3416=FACE_OUTER_BOUND('',#5186,.T.);
#3417=FACE_OUTER_BOUND('',#5187,.T.);
#3418=FACE_OUTER_BOUND('',#5188,.T.);
#3419=FACE_OUTER_BOUND('',#5189,.T.);
#3420=FACE_OUTER_BOUND('',#5190,.T.);
#3421=FACE_OUTER_BOUND('',#5191,.T.);
#3422=FACE_OUTER_BOUND('',#5192,.T.);
#3423=FACE_OUTER_BOUND('',#5193,.T.);
#3424=FACE_OUTER_BOUND('',#5194,.T.);
#3425=FACE_OUTER_BOUND('',#5195,.T.);
#3426=FACE_OUTER_BOUND('',#5196,.T.);
#3427=FACE_OUTER_BOUND('',#5197,.T.);
#3428=FACE_OUTER_BOUND('',#5198,.T.);
#3429=FACE_OUTER_BOUND('',#5199,.T.);
#3430=FACE_OUTER_BOUND('',#5200,.T.);
#3431=FACE_OUTER_BOUND('',#5201,.T.);
#3432=FACE_OUTER_BOUND('',#5202,.T.);
#3433=FACE_OUTER_BOUND('',#5203,.T.);
#3434=FACE_OUTER_BOUND('',#5204,.T.);
#3435=FACE_OUTER_BOUND('',#5205,.T.);
#3436=FACE_OUTER_BOUND('',#5206,.T.);
#3437=FACE_OUTER_BOUND('',#5207,.T.);
#3438=FACE_OUTER_BOUND('',#5209,.T.);
#3439=FACE_OUTER_BOUND('',#5210,.T.);
#3440=FACE_OUTER_BOUND('',#5212,.T.);
#3441=FACE_OUTER_BOUND('',#5213,.T.);
#3442=FACE_OUTER_BOUND('',#5214,.T.);
#3443=FACE_OUTER_BOUND('',#5215,.T.);
#3444=FACE_OUTER_BOUND('',#5216,.T.);
#3445=FACE_OUTER_BOUND('',#5217,.T.);
#3446=FACE_OUTER_BOUND('',#5218,.T.);
#3447=FACE_OUTER_BOUND('',#5219,.T.);
#3448=FACE_OUTER_BOUND('',#5220,.T.);
#3449=FACE_OUTER_BOUND('',#5221,.T.);
#3450=FACE_OUTER_BOUND('',#5222,.T.);
#3451=FACE_OUTER_BOUND('',#5223,.T.);
#3452=FACE_OUTER_BOUND('',#5224,.T.);
#3453=FACE_OUTER_BOUND('',#5225,.T.);
#3454=FACE_OUTER_BOUND('',#5226,.T.);
#3455=FACE_OUTER_BOUND('',#5227,.T.);
#3456=FACE_OUTER_BOUND('',#5228,.T.);
#3457=FACE_OUTER_BOUND('',#5229,.T.);
#3458=FACE_OUTER_BOUND('',#5230,.T.);
#3459=FACE_OUTER_BOUND('',#5231,.T.);
#3460=FACE_OUTER_BOUND('',#5232,.T.);
#3461=FACE_OUTER_BOUND('',#5233,.T.);
#3462=FACE_OUTER_BOUND('',#5234,.T.);
#3463=FACE_OUTER_BOUND('',#5235,.T.);
#3464=FACE_OUTER_BOUND('',#5236,.T.);
#3465=FACE_OUTER_BOUND('',#5237,.T.);
#3466=FACE_OUTER_BOUND('',#5238,.T.);
#3467=FACE_OUTER_BOUND('',#5239,.T.);
#3468=FACE_OUTER_BOUND('',#5240,.T.);
#3469=FACE_OUTER_BOUND('',#5241,.T.);
#3470=FACE_OUTER_BOUND('',#5242,.T.);
#3471=FACE_OUTER_BOUND('',#5243,.T.);
#3472=FACE_OUTER_BOUND('',#5244,.T.);
#3473=FACE_OUTER_BOUND('',#5245,.T.);
#3474=FACE_OUTER_BOUND('',#5246,.T.);
#3475=FACE_OUTER_BOUND('',#5247,.T.);
#3476=FACE_OUTER_BOUND('',#5248,.T.);
#3477=FACE_OUTER_BOUND('',#5249,.T.);
#3478=FACE_OUTER_BOUND('',#5250,.T.);
#3479=FACE_OUTER_BOUND('',#5251,.T.);
#3480=FACE_OUTER_BOUND('',#5252,.T.);
#3481=FACE_OUTER_BOUND('',#5253,.T.);
#3482=FACE_OUTER_BOUND('',#5254,.T.);
#3483=FACE_OUTER_BOUND('',#5255,.T.);
#3484=FACE_OUTER_BOUND('',#5256,.T.);
#3485=FACE_OUTER_BOUND('',#5257,.T.);
#3486=FACE_OUTER_BOUND('',#5258,.T.);
#3487=FACE_OUTER_BOUND('',#5259,.T.);
#3488=FACE_OUTER_BOUND('',#5260,.T.);
#3489=FACE_OUTER_BOUND('',#5261,.T.);
#3490=FACE_OUTER_BOUND('',#5262,.T.);
#3491=FACE_OUTER_BOUND('',#5263,.T.);
#3492=FACE_OUTER_BOUND('',#5264,.T.);
#3493=FACE_OUTER_BOUND('',#5265,.T.);
#3494=FACE_OUTER_BOUND('',#5266,.T.);
#3495=FACE_OUTER_BOUND('',#5267,.T.);
#3496=FACE_OUTER_BOUND('',#5268,.T.);
#3497=FACE_OUTER_BOUND('',#5269,.T.);
#3498=FACE_OUTER_BOUND('',#5270,.T.);
#3499=FACE_OUTER_BOUND('',#5271,.T.);
#3500=FACE_OUTER_BOUND('',#5272,.T.);
#3501=FACE_OUTER_BOUND('',#5273,.T.);
#3502=FACE_OUTER_BOUND('',#5274,.T.);
#3503=FACE_OUTER_BOUND('',#5275,.T.);
#3504=FACE_OUTER_BOUND('',#5276,.T.);
#3505=FACE_OUTER_BOUND('',#5277,.T.);
#3506=FACE_OUTER_BOUND('',#5278,.T.);
#3507=FACE_OUTER_BOUND('',#5279,.T.);
#3508=FACE_OUTER_BOUND('',#5280,.T.);
#3509=FACE_OUTER_BOUND('',#5281,.T.);
#3510=FACE_OUTER_BOUND('',#5282,.T.);
#3511=FACE_OUTER_BOUND('',#5283,.T.);
#3512=FACE_OUTER_BOUND('',#5284,.T.);
#3513=FACE_OUTER_BOUND('',#5285,.T.);
#3514=FACE_OUTER_BOUND('',#5286,.T.);
#3515=FACE_OUTER_BOUND('',#5287,.T.);
#3516=FACE_OUTER_BOUND('',#5288,.T.);
#3517=FACE_OUTER_BOUND('',#5289,.T.);
#3518=FACE_OUTER_BOUND('',#5290,.T.);
#3519=FACE_OUTER_BOUND('',#5291,.T.);
#3520=FACE_OUTER_BOUND('',#5292,.T.);
#3521=FACE_OUTER_BOUND('',#5293,.T.);
#3522=FACE_OUTER_BOUND('',#5294,.T.);
#3523=FACE_OUTER_BOUND('',#5295,.T.);
#3524=FACE_OUTER_BOUND('',#5296,.T.);
#3525=FACE_OUTER_BOUND('',#5297,.T.);
#3526=FACE_OUTER_BOUND('',#5299,.T.);
#3527=FACE_OUTER_BOUND('',#5301,.T.);
#3528=FACE_OUTER_BOUND('',#5302,.T.);
#3529=FACE_OUTER_BOUND('',#5304,.T.);
#3530=FACE_OUTER_BOUND('',#5305,.T.);
#3531=FACE_OUTER_BOUND('',#5306,.T.);
#3532=FACE_OUTER_BOUND('',#5307,.T.);
#3533=FACE_OUTER_BOUND('',#5308,.T.);
#3534=FACE_OUTER_BOUND('',#5309,.T.);
#3535=FACE_OUTER_BOUND('',#5310,.T.);
#3536=FACE_OUTER_BOUND('',#5311,.T.);
#3537=FACE_OUTER_BOUND('',#5312,.T.);
#3538=FACE_OUTER_BOUND('',#5313,.T.);
#3539=FACE_OUTER_BOUND('',#5314,.T.);
#3540=FACE_OUTER_BOUND('',#5315,.T.);
#3541=FACE_OUTER_BOUND('',#5316,.T.);
#3542=FACE_OUTER_BOUND('',#5317,.T.);
#3543=FACE_OUTER_BOUND('',#5318,.T.);
#3544=FACE_OUTER_BOUND('',#5319,.T.);
#3545=FACE_OUTER_BOUND('',#5320,.T.);
#3546=FACE_OUTER_BOUND('',#5321,.T.);
#3547=FACE_OUTER_BOUND('',#5322,.T.);
#3548=FACE_OUTER_BOUND('',#5323,.T.);
#3549=FACE_OUTER_BOUND('',#5324,.T.);
#3550=FACE_OUTER_BOUND('',#5325,.T.);
#3551=FACE_OUTER_BOUND('',#5326,.T.);
#3552=FACE_OUTER_BOUND('',#5327,.T.);
#3553=FACE_OUTER_BOUND('',#5328,.T.);
#3554=FACE_OUTER_BOUND('',#5329,.T.);
#3555=FACE_OUTER_BOUND('',#5330,.T.);
#3556=FACE_OUTER_BOUND('',#5331,.T.);
#3557=FACE_OUTER_BOUND('',#5332,.T.);
#3558=FACE_OUTER_BOUND('',#5333,.T.);
#3559=FACE_OUTER_BOUND('',#5334,.T.);
#3560=FACE_OUTER_BOUND('',#5335,.T.);
#3561=FACE_OUTER_BOUND('',#5336,.T.);
#3562=FACE_OUTER_BOUND('',#5337,.T.);
#3563=FACE_OUTER_BOUND('',#5338,.T.);
#3564=FACE_OUTER_BOUND('',#5339,.T.);
#3565=FACE_OUTER_BOUND('',#5340,.T.);
#3566=FACE_OUTER_BOUND('',#5341,.T.);
#3567=FACE_OUTER_BOUND('',#5342,.T.);
#3568=FACE_OUTER_BOUND('',#5343,.T.);
#3569=FACE_OUTER_BOUND('',#5344,.T.);
#3570=FACE_OUTER_BOUND('',#5345,.T.);
#3571=FACE_OUTER_BOUND('',#5346,.T.);
#3572=FACE_OUTER_BOUND('',#5347,.T.);
#3573=FACE_OUTER_BOUND('',#5348,.T.);
#3574=FACE_OUTER_BOUND('',#5349,.T.);
#3575=FACE_OUTER_BOUND('',#5350,.T.);
#3576=FACE_OUTER_BOUND('',#5351,.T.);
#3577=FACE_OUTER_BOUND('',#5352,.T.);
#3578=FACE_OUTER_BOUND('',#5353,.T.);
#3579=FACE_OUTER_BOUND('',#5354,.T.);
#3580=FACE_OUTER_BOUND('',#5355,.T.);
#3581=FACE_OUTER_BOUND('',#5356,.T.);
#3582=FACE_OUTER_BOUND('',#5357,.T.);
#3583=FACE_OUTER_BOUND('',#5358,.T.);
#3584=FACE_OUTER_BOUND('',#5359,.T.);
#3585=FACE_OUTER_BOUND('',#5360,.T.);
#3586=FACE_OUTER_BOUND('',#5361,.T.);
#3587=FACE_OUTER_BOUND('',#5362,.T.);
#3588=FACE_OUTER_BOUND('',#5363,.T.);
#3589=FACE_OUTER_BOUND('',#5364,.T.);
#3590=FACE_OUTER_BOUND('',#5365,.T.);
#3591=FACE_OUTER_BOUND('',#5366,.T.);
#3592=FACE_OUTER_BOUND('',#5367,.T.);
#3593=FACE_OUTER_BOUND('',#5368,.T.);
#3594=FACE_OUTER_BOUND('',#5369,.T.);
#3595=FACE_OUTER_BOUND('',#5370,.T.);
#3596=FACE_OUTER_BOUND('',#5371,.T.);
#3597=FACE_OUTER_BOUND('',#5372,.T.);
#3598=FACE_OUTER_BOUND('',#5373,.T.);
#3599=FACE_OUTER_BOUND('',#5374,.T.);
#3600=FACE_OUTER_BOUND('',#5375,.T.);
#3601=FACE_OUTER_BOUND('',#5376,.T.);
#3602=FACE_OUTER_BOUND('',#5377,.T.);
#3603=FACE_OUTER_BOUND('',#5378,.T.);
#3604=FACE_OUTER_BOUND('',#5379,.T.);
#3605=FACE_OUTER_BOUND('',#5380,.T.);
#3606=FACE_OUTER_BOUND('',#5381,.T.);
#3607=FACE_OUTER_BOUND('',#5382,.T.);
#3608=FACE_OUTER_BOUND('',#5383,.T.);
#3609=FACE_OUTER_BOUND('',#5384,.T.);
#3610=FACE_OUTER_BOUND('',#5385,.T.);
#3611=FACE_OUTER_BOUND('',#5386,.T.);
#3612=FACE_OUTER_BOUND('',#5387,.T.);
#3613=FACE_OUTER_BOUND('',#5388,.T.);
#3614=FACE_OUTER_BOUND('',#5389,.T.);
#3615=FACE_OUTER_BOUND('',#5390,.T.);
#3616=FACE_OUTER_BOUND('',#5391,.T.);
#3617=FACE_OUTER_BOUND('',#5392,.T.);
#3618=FACE_OUTER_BOUND('',#5393,.T.);
#3619=FACE_OUTER_BOUND('',#5394,.T.);
#3620=FACE_OUTER_BOUND('',#5395,.T.);
#3621=FACE_OUTER_BOUND('',#5396,.T.);
#3622=FACE_OUTER_BOUND('',#5397,.T.);
#3623=FACE_OUTER_BOUND('',#5398,.T.);
#3624=FACE_OUTER_BOUND('',#5399,.T.);
#3625=FACE_OUTER_BOUND('',#5400,.T.);
#3626=FACE_OUTER_BOUND('',#5401,.T.);
#3627=FACE_OUTER_BOUND('',#5402,.T.);
#3628=FACE_OUTER_BOUND('',#5403,.T.);
#3629=FACE_OUTER_BOUND('',#5404,.T.);
#3630=FACE_OUTER_BOUND('',#5405,.T.);
#3631=FACE_OUTER_BOUND('',#5406,.T.);
#3632=FACE_OUTER_BOUND('',#5407,.T.);
#3633=FACE_OUTER_BOUND('',#5408,.T.);
#3634=FACE_OUTER_BOUND('',#5409,.T.);
#3635=FACE_OUTER_BOUND('',#5410,.T.);
#3636=FACE_OUTER_BOUND('',#5411,.T.);
#3637=FACE_OUTER_BOUND('',#5412,.T.);
#3638=FACE_OUTER_BOUND('',#5413,.T.);
#3639=FACE_OUTER_BOUND('',#5414,.T.);
#3640=FACE_OUTER_BOUND('',#5415,.T.);
#3641=FACE_OUTER_BOUND('',#5416,.T.);
#3642=FACE_OUTER_BOUND('',#5417,.T.);
#3643=FACE_OUTER_BOUND('',#5418,.T.);
#3644=FACE_OUTER_BOUND('',#5419,.T.);
#3645=FACE_OUTER_BOUND('',#5420,.T.);
#3646=FACE_OUTER_BOUND('',#5421,.T.);
#3647=FACE_OUTER_BOUND('',#5422,.T.);
#3648=FACE_OUTER_BOUND('',#5423,.T.);
#3649=FACE_OUTER_BOUND('',#5424,.T.);
#3650=FACE_OUTER_BOUND('',#5425,.T.);
#3651=FACE_OUTER_BOUND('',#5426,.T.);
#3652=FACE_OUTER_BOUND('',#5427,.T.);
#3653=FACE_OUTER_BOUND('',#5428,.T.);
#3654=FACE_OUTER_BOUND('',#5429,.T.);
#3655=FACE_OUTER_BOUND('',#5430,.T.);
#3656=FACE_OUTER_BOUND('',#5431,.T.);
#3657=FACE_OUTER_BOUND('',#5432,.T.);
#3658=FACE_OUTER_BOUND('',#5433,.T.);
#3659=FACE_OUTER_BOUND('',#5434,.T.);
#3660=FACE_OUTER_BOUND('',#5435,.T.);
#3661=FACE_OUTER_BOUND('',#5436,.T.);
#3662=FACE_OUTER_BOUND('',#5437,.T.);
#3663=FACE_OUTER_BOUND('',#5438,.T.);
#3664=FACE_OUTER_BOUND('',#5439,.T.);
#3665=FACE_OUTER_BOUND('',#5440,.T.);
#3666=FACE_OUTER_BOUND('',#5441,.T.);
#3667=FACE_OUTER_BOUND('',#5442,.T.);
#3668=FACE_OUTER_BOUND('',#5443,.T.);
#3669=FACE_OUTER_BOUND('',#5444,.T.);
#3670=FACE_OUTER_BOUND('',#5445,.T.);
#3671=FACE_OUTER_BOUND('',#5446,.T.);
#3672=FACE_OUTER_BOUND('',#5447,.T.);
#3673=FACE_OUTER_BOUND('',#5448,.T.);
#3674=FACE_OUTER_BOUND('',#5449,.T.);
#3675=FACE_OUTER_BOUND('',#5450,.T.);
#3676=FACE_OUTER_BOUND('',#5451,.T.);
#3677=FACE_OUTER_BOUND('',#5452,.T.);
#3678=FACE_OUTER_BOUND('',#5453,.T.);
#3679=FACE_OUTER_BOUND('',#5454,.T.);
#3680=FACE_OUTER_BOUND('',#5455,.T.);
#3681=FACE_OUTER_BOUND('',#5456,.T.);
#3682=FACE_OUTER_BOUND('',#5457,.T.);
#3683=FACE_OUTER_BOUND('',#5458,.T.);
#3684=FACE_OUTER_BOUND('',#5459,.T.);
#3685=FACE_OUTER_BOUND('',#5460,.T.);
#3686=FACE_OUTER_BOUND('',#5461,.T.);
#3687=FACE_OUTER_BOUND('',#5462,.T.);
#3688=FACE_OUTER_BOUND('',#5463,.T.);
#3689=FACE_OUTER_BOUND('',#5464,.T.);
#3690=FACE_OUTER_BOUND('',#5465,.T.);
#3691=FACE_OUTER_BOUND('',#5466,.T.);
#3692=FACE_OUTER_BOUND('',#5467,.T.);
#3693=FACE_OUTER_BOUND('',#5468,.T.);
#3694=FACE_OUTER_BOUND('',#5469,.T.);
#3695=FACE_OUTER_BOUND('',#5470,.T.);
#3696=FACE_OUTER_BOUND('',#5471,.T.);
#3697=FACE_OUTER_BOUND('',#5472,.T.);
#3698=FACE_OUTER_BOUND('',#5473,.T.);
#3699=FACE_OUTER_BOUND('',#5474,.T.);
#3700=FACE_OUTER_BOUND('',#5475,.T.);
#3701=FACE_OUTER_BOUND('',#5477,.T.);
#3702=FACE_OUTER_BOUND('',#5478,.T.);
#3703=FACE_OUTER_BOUND('',#5516,.T.);
#3704=FACE_OUTER_BOUND('',#5517,.T.);
#3705=FACE_OUTER_BOUND('',#5519,.T.);
#3706=FACE_OUTER_BOUND('',#5520,.T.);
#3707=FACE_OUTER_BOUND('',#5522,.T.);
#3708=FACE_OUTER_BOUND('',#5524,.T.);
#3709=FACE_OUTER_BOUND('',#5525,.T.);
#3710=FACE_OUTER_BOUND('',#5526,.T.);
#3711=FACE_OUTER_BOUND('',#5527,.T.);
#3712=FACE_OUTER_BOUND('',#5528,.T.);
#3713=FACE_OUTER_BOUND('',#5529,.T.);
#3714=FACE_OUTER_BOUND('',#5530,.T.);
#3715=FACE_OUTER_BOUND('',#5531,.T.);
#3716=FACE_OUTER_BOUND('',#5532,.T.);
#3717=FACE_OUTER_BOUND('',#5533,.T.);
#3718=FACE_OUTER_BOUND('',#5534,.T.);
#3719=FACE_OUTER_BOUND('',#5535,.T.);
#3720=FACE_OUTER_BOUND('',#5536,.T.);
#3721=FACE_OUTER_BOUND('',#5537,.T.);
#3722=FACE_OUTER_BOUND('',#5538,.T.);
#3723=FACE_OUTER_BOUND('',#5539,.T.);
#3724=FACE_OUTER_BOUND('',#5540,.T.);
#3725=FACE_OUTER_BOUND('',#5541,.T.);
#3726=FACE_OUTER_BOUND('',#5542,.T.);
#3727=FACE_OUTER_BOUND('',#5543,.T.);
#3728=FACE_OUTER_BOUND('',#5544,.T.);
#3729=FACE_OUTER_BOUND('',#5546,.T.);
#3730=FACE_OUTER_BOUND('',#5547,.T.);
#3731=FACE_OUTER_BOUND('',#5548,.T.);
#3732=FACE_OUTER_BOUND('',#5549,.T.);
#3733=FACE_OUTER_BOUND('',#5550,.T.);
#3734=FACE_OUTER_BOUND('',#5551,.T.);
#3735=FACE_OUTER_BOUND('',#5552,.T.);
#3736=FACE_OUTER_BOUND('',#5553,.T.);
#3737=FACE_OUTER_BOUND('',#5554,.T.);
#3738=FACE_OUTER_BOUND('',#5555,.T.);
#3739=FACE_OUTER_BOUND('',#5556,.T.);
#3740=FACE_OUTER_BOUND('',#5557,.T.);
#3741=FACE_OUTER_BOUND('',#5558,.T.);
#3742=FACE_OUTER_BOUND('',#5559,.T.);
#3743=FACE_OUTER_BOUND('',#5560,.T.);
#3744=FACE_OUTER_BOUND('',#5562,.T.);
#3745=FACE_OUTER_BOUND('',#5563,.T.);
#3746=FACE_OUTER_BOUND('',#5564,.T.);
#3747=FACE_OUTER_BOUND('',#5565,.T.);
#3748=FACE_OUTER_BOUND('',#5566,.T.);
#3749=FACE_OUTER_BOUND('',#5567,.T.);
#3750=FACE_OUTER_BOUND('',#5568,.T.);
#3751=FACE_OUTER_BOUND('',#5569,.T.);
#3752=FACE_OUTER_BOUND('',#5570,.T.);
#3753=FACE_OUTER_BOUND('',#5571,.T.);
#3754=FACE_OUTER_BOUND('',#5572,.T.);
#3755=FACE_OUTER_BOUND('',#5573,.T.);
#3756=FACE_OUTER_BOUND('',#5574,.T.);
#3757=FACE_OUTER_BOUND('',#5575,.T.);
#3758=FACE_OUTER_BOUND('',#5576,.T.);
#3759=FACE_OUTER_BOUND('',#5577,.T.);
#3760=FACE_OUTER_BOUND('',#5578,.T.);
#3761=FACE_OUTER_BOUND('',#5579,.T.);
#3762=FACE_OUTER_BOUND('',#5580,.T.);
#3763=FACE_OUTER_BOUND('',#5581,.T.);
#3764=FACE_OUTER_BOUND('',#5582,.T.);
#3765=FACE_OUTER_BOUND('',#5583,.T.);
#3766=FACE_OUTER_BOUND('',#5584,.T.);
#3767=FACE_OUTER_BOUND('',#5586,.T.);
#3768=FACE_OUTER_BOUND('',#5587,.T.);
#3769=FACE_OUTER_BOUND('',#5588,.T.);
#3770=FACE_OUTER_BOUND('',#5589,.T.);
#3771=FACE_OUTER_BOUND('',#5590,.T.);
#3772=FACE_OUTER_BOUND('',#5591,.T.);
#3773=FACE_OUTER_BOUND('',#5592,.T.);
#3774=FACE_OUTER_BOUND('',#5593,.T.);
#3775=FACE_OUTER_BOUND('',#5594,.T.);
#3776=FACE_OUTER_BOUND('',#5595,.T.);
#3777=FACE_OUTER_BOUND('',#5596,.T.);
#3778=FACE_OUTER_BOUND('',#5597,.T.);
#3779=FACE_OUTER_BOUND('',#5598,.T.);
#3780=FACE_OUTER_BOUND('',#5599,.T.);
#3781=FACE_OUTER_BOUND('',#5600,.T.);
#3782=FACE_OUTER_BOUND('',#5601,.T.);
#3783=FACE_OUTER_BOUND('',#5602,.T.);
#3784=FACE_OUTER_BOUND('',#5603,.T.);
#3785=FACE_OUTER_BOUND('',#5604,.T.);
#3786=FACE_OUTER_BOUND('',#5605,.T.);
#3787=FACE_OUTER_BOUND('',#5606,.T.);
#3788=FACE_OUTER_BOUND('',#5607,.T.);
#3789=FACE_OUTER_BOUND('',#5608,.T.);
#3790=FACE_OUTER_BOUND('',#5609,.T.);
#3791=FACE_OUTER_BOUND('',#5610,.T.);
#3792=FACE_OUTER_BOUND('',#5611,.T.);
#3793=FACE_OUTER_BOUND('',#5612,.T.);
#3794=FACE_OUTER_BOUND('',#5613,.T.);
#3795=FACE_OUTER_BOUND('',#5614,.T.);
#3796=FACE_OUTER_BOUND('',#5615,.T.);
#3797=FACE_OUTER_BOUND('',#5616,.T.);
#3798=FACE_OUTER_BOUND('',#5617,.T.);
#3799=FACE_OUTER_BOUND('',#5618,.T.);
#3800=FACE_OUTER_BOUND('',#5619,.T.);
#3801=FACE_OUTER_BOUND('',#5620,.T.);
#3802=FACE_OUTER_BOUND('',#5621,.T.);
#3803=FACE_OUTER_BOUND('',#5622,.T.);
#3804=FACE_OUTER_BOUND('',#5623,.T.);
#3805=FACE_OUTER_BOUND('',#5624,.T.);
#3806=FACE_OUTER_BOUND('',#5625,.T.);
#3807=FACE_OUTER_BOUND('',#5626,.T.);
#3808=FACE_OUTER_BOUND('',#5627,.T.);
#3809=FACE_OUTER_BOUND('',#5628,.T.);
#3810=FACE_OUTER_BOUND('',#5629,.T.);
#3811=FACE_OUTER_BOUND('',#5630,.T.);
#3812=FACE_OUTER_BOUND('',#5631,.T.);
#3813=FACE_OUTER_BOUND('',#5632,.T.);
#3814=FACE_OUTER_BOUND('',#5633,.T.);
#3815=FACE_OUTER_BOUND('',#5634,.T.);
#3816=FACE_OUTER_BOUND('',#5635,.T.);
#3817=FACE_OUTER_BOUND('',#5636,.T.);
#3818=FACE_OUTER_BOUND('',#5637,.T.);
#3819=FACE_OUTER_BOUND('',#5638,.T.);
#3820=FACE_OUTER_BOUND('',#5640,.T.);
#3821=FACE_OUTER_BOUND('',#5641,.T.);
#3822=FACE_OUTER_BOUND('',#5642,.T.);
#3823=FACE_OUTER_BOUND('',#5643,.T.);
#3824=FACE_OUTER_BOUND('',#5644,.T.);
#3825=FACE_OUTER_BOUND('',#5645,.T.);
#3826=FACE_OUTER_BOUND('',#5646,.T.);
#3827=FACE_OUTER_BOUND('',#5647,.T.);
#3828=FACE_OUTER_BOUND('',#5648,.T.);
#3829=FACE_OUTER_BOUND('',#5649,.T.);
#3830=FACE_OUTER_BOUND('',#5650,.T.);
#3831=FACE_OUTER_BOUND('',#5651,.T.);
#3832=FACE_OUTER_BOUND('',#5652,.T.);
#3833=FACE_OUTER_BOUND('',#5653,.T.);
#3834=FACE_OUTER_BOUND('',#5654,.T.);
#3835=FACE_OUTER_BOUND('',#5655,.T.);
#3836=FACE_OUTER_BOUND('',#5656,.T.);
#3837=FACE_OUTER_BOUND('',#5657,.T.);
#3838=FACE_OUTER_BOUND('',#5658,.T.);
#3839=FACE_OUTER_BOUND('',#5659,.T.);
#3840=FACE_OUTER_BOUND('',#5660,.T.);
#3841=FACE_OUTER_BOUND('',#5661,.T.);
#3842=FACE_OUTER_BOUND('',#5662,.T.);
#3843=FACE_OUTER_BOUND('',#5663,.T.);
#3844=FACE_OUTER_BOUND('',#5664,.T.);
#3845=FACE_OUTER_BOUND('',#5665,.T.);
#3846=FACE_OUTER_BOUND('',#5666,.T.);
#3847=FACE_OUTER_BOUND('',#5667,.T.);
#3848=FACE_OUTER_BOUND('',#5668,.T.);
#3849=FACE_OUTER_BOUND('',#5669,.T.);
#3850=FACE_OUTER_BOUND('',#5670,.T.);
#3851=FACE_OUTER_BOUND('',#5671,.T.);
#3852=FACE_OUTER_BOUND('',#5672,.T.);
#3853=FACE_OUTER_BOUND('',#5673,.T.);
#3854=FACE_OUTER_BOUND('',#5674,.T.);
#3855=FACE_OUTER_BOUND('',#5675,.T.);
#3856=FACE_OUTER_BOUND('',#5676,.T.);
#3857=FACE_OUTER_BOUND('',#5677,.T.);
#3858=FACE_OUTER_BOUND('',#5678,.T.);
#3859=FACE_OUTER_BOUND('',#5679,.T.);
#3860=FACE_OUTER_BOUND('',#5680,.T.);
#3861=FACE_OUTER_BOUND('',#5681,.T.);
#3862=FACE_OUTER_BOUND('',#5682,.T.);
#3863=FACE_OUTER_BOUND('',#5683,.T.);
#3864=FACE_OUTER_BOUND('',#5684,.T.);
#3865=FACE_OUTER_BOUND('',#5686,.T.);
#3866=FACE_OUTER_BOUND('',#5687,.T.);
#3867=FACE_OUTER_BOUND('',#5688,.T.);
#3868=FACE_OUTER_BOUND('',#5689,.T.);
#3869=FACE_OUTER_BOUND('',#5690,.T.);
#3870=FACE_OUTER_BOUND('',#5691,.T.);
#3871=FACE_OUTER_BOUND('',#5692,.T.);
#3872=FACE_OUTER_BOUND('',#5693,.T.);
#3873=FACE_OUTER_BOUND('',#5694,.T.);
#3874=FACE_OUTER_BOUND('',#5695,.T.);
#3875=FACE_OUTER_BOUND('',#5696,.T.);
#3876=FACE_OUTER_BOUND('',#5697,.T.);
#3877=FACE_OUTER_BOUND('',#5698,.T.);
#3878=FACE_OUTER_BOUND('',#5699,.T.);
#3879=FACE_OUTER_BOUND('',#5700,.T.);
#3880=FACE_OUTER_BOUND('',#5701,.T.);
#3881=FACE_OUTER_BOUND('',#5702,.T.);
#3882=FACE_OUTER_BOUND('',#5703,.T.);
#3883=FACE_OUTER_BOUND('',#5704,.T.);
#3884=FACE_OUTER_BOUND('',#5705,.T.);
#3885=FACE_OUTER_BOUND('',#5706,.T.);
#3886=FACE_OUTER_BOUND('',#5707,.T.);
#3887=FACE_OUTER_BOUND('',#5708,.T.);
#3888=FACE_OUTER_BOUND('',#5709,.T.);
#3889=FACE_OUTER_BOUND('',#5710,.T.);
#3890=FACE_OUTER_BOUND('',#5711,.T.);
#3891=FACE_OUTER_BOUND('',#5712,.T.);
#3892=FACE_OUTER_BOUND('',#5713,.T.);
#3893=FACE_OUTER_BOUND('',#5714,.T.);
#3894=FACE_OUTER_BOUND('',#5715,.T.);
#3895=FACE_OUTER_BOUND('',#5716,.T.);
#3896=FACE_OUTER_BOUND('',#5717,.T.);
#3897=FACE_OUTER_BOUND('',#5719,.T.);
#3898=FACE_OUTER_BOUND('',#5720,.T.);
#3899=FACE_OUTER_BOUND('',#5721,.T.);
#3900=FACE_OUTER_BOUND('',#5722,.T.);
#3901=FACE_OUTER_BOUND('',#5723,.T.);
#3902=FACE_OUTER_BOUND('',#5724,.T.);
#3903=FACE_OUTER_BOUND('',#5725,.T.);
#3904=FACE_OUTER_BOUND('',#5726,.T.);
#3905=FACE_OUTER_BOUND('',#5727,.T.);
#3906=FACE_OUTER_BOUND('',#5728,.T.);
#3907=FACE_OUTER_BOUND('',#5729,.T.);
#3908=FACE_OUTER_BOUND('',#5730,.T.);
#3909=FACE_OUTER_BOUND('',#5731,.T.);
#3910=FACE_OUTER_BOUND('',#5732,.T.);
#3911=FACE_OUTER_BOUND('',#5733,.T.);
#3912=FACE_OUTER_BOUND('',#5734,.T.);
#3913=FACE_OUTER_BOUND('',#5735,.T.);
#3914=FACE_OUTER_BOUND('',#5736,.T.);
#3915=FACE_OUTER_BOUND('',#5737,.T.);
#3916=FACE_OUTER_BOUND('',#5738,.T.);
#3917=FACE_OUTER_BOUND('',#5739,.T.);
#3918=FACE_OUTER_BOUND('',#5740,.T.);
#3919=FACE_OUTER_BOUND('',#5742,.T.);
#3920=FACE_OUTER_BOUND('',#5743,.T.);
#3921=FACE_OUTER_BOUND('',#5744,.T.);
#3922=FACE_OUTER_BOUND('',#5745,.T.);
#3923=FACE_OUTER_BOUND('',#5746,.T.);
#3924=FACE_OUTER_BOUND('',#5747,.T.);
#3925=FACE_OUTER_BOUND('',#5748,.T.);
#3926=FACE_OUTER_BOUND('',#5749,.T.);
#3927=FACE_OUTER_BOUND('',#5750,.T.);
#3928=FACE_OUTER_BOUND('',#5751,.T.);
#3929=FACE_OUTER_BOUND('',#5752,.T.);
#3930=FACE_OUTER_BOUND('',#5753,.T.);
#3931=FACE_OUTER_BOUND('',#5754,.T.);
#3932=FACE_OUTER_BOUND('',#5755,.T.);
#3933=FACE_OUTER_BOUND('',#5756,.T.);
#3934=FACE_OUTER_BOUND('',#5757,.T.);
#3935=FACE_OUTER_BOUND('',#5758,.T.);
#3936=FACE_OUTER_BOUND('',#5759,.T.);
#3937=FACE_OUTER_BOUND('',#5760,.T.);
#3938=FACE_OUTER_BOUND('',#5761,.T.);
#3939=FACE_OUTER_BOUND('',#5762,.T.);
#3940=FACE_OUTER_BOUND('',#5763,.T.);
#3941=FACE_OUTER_BOUND('',#5764,.T.);
#3942=FACE_OUTER_BOUND('',#5765,.T.);
#3943=FACE_OUTER_BOUND('',#5766,.T.);
#3944=FACE_OUTER_BOUND('',#5767,.T.);
#3945=FACE_OUTER_BOUND('',#5768,.T.);
#3946=FACE_OUTER_BOUND('',#5769,.T.);
#3947=FACE_OUTER_BOUND('',#5770,.T.);
#3948=FACE_OUTER_BOUND('',#5771,.T.);
#3949=FACE_OUTER_BOUND('',#5772,.T.);
#3950=FACE_OUTER_BOUND('',#5773,.T.);
#3951=FACE_OUTER_BOUND('',#5775,.T.);
#3952=FACE_OUTER_BOUND('',#5776,.T.);
#3953=FACE_OUTER_BOUND('',#5777,.T.);
#3954=FACE_OUTER_BOUND('',#5778,.T.);
#3955=FACE_OUTER_BOUND('',#5779,.T.);
#3956=FACE_OUTER_BOUND('',#5780,.T.);
#3957=FACE_OUTER_BOUND('',#5781,.T.);
#3958=FACE_OUTER_BOUND('',#5782,.T.);
#3959=FACE_OUTER_BOUND('',#5783,.T.);
#3960=FACE_OUTER_BOUND('',#5784,.T.);
#3961=FACE_OUTER_BOUND('',#5785,.T.);
#3962=FACE_OUTER_BOUND('',#5786,.T.);
#3963=FACE_OUTER_BOUND('',#5787,.T.);
#3964=FACE_OUTER_BOUND('',#5788,.T.);
#3965=FACE_OUTER_BOUND('',#5789,.T.);
#3966=FACE_OUTER_BOUND('',#5790,.T.);
#3967=FACE_OUTER_BOUND('',#5791,.T.);
#3968=FACE_OUTER_BOUND('',#5792,.T.);
#3969=FACE_OUTER_BOUND('',#5793,.T.);
#3970=FACE_OUTER_BOUND('',#5794,.T.);
#3971=FACE_OUTER_BOUND('',#5795,.T.);
#3972=FACE_OUTER_BOUND('',#5796,.T.);
#3973=FACE_OUTER_BOUND('',#5797,.T.);
#3974=FACE_OUTER_BOUND('',#5798,.T.);
#3975=FACE_OUTER_BOUND('',#5799,.T.);
#3976=FACE_OUTER_BOUND('',#5800,.T.);
#3977=FACE_OUTER_BOUND('',#5801,.T.);
#3978=FACE_OUTER_BOUND('',#5802,.T.);
#3979=FACE_OUTER_BOUND('',#5803,.T.);
#3980=FACE_OUTER_BOUND('',#5804,.T.);
#3981=FACE_OUTER_BOUND('',#5805,.T.);
#3982=FACE_OUTER_BOUND('',#5806,.T.);
#3983=FACE_OUTER_BOUND('',#5807,.T.);
#3984=FACE_OUTER_BOUND('',#5808,.T.);
#3985=FACE_OUTER_BOUND('',#5809,.T.);
#3986=FACE_OUTER_BOUND('',#5810,.T.);
#3987=FACE_OUTER_BOUND('',#5811,.T.);
#3988=FACE_OUTER_BOUND('',#5812,.T.);
#3989=FACE_OUTER_BOUND('',#5813,.T.);
#3990=FACE_OUTER_BOUND('',#5814,.T.);
#3991=FACE_OUTER_BOUND('',#5815,.T.);
#3992=FACE_OUTER_BOUND('',#5816,.T.);
#3993=FACE_OUTER_BOUND('',#5817,.T.);
#3994=FACE_OUTER_BOUND('',#5818,.T.);
#3995=FACE_OUTER_BOUND('',#5819,.T.);
#3996=FACE_OUTER_BOUND('',#5821,.T.);
#3997=FACE_OUTER_BOUND('',#5822,.T.);
#3998=FACE_OUTER_BOUND('',#5823,.T.);
#3999=FACE_OUTER_BOUND('',#5824,.T.);
#4000=FACE_OUTER_BOUND('',#5825,.T.);
#4001=FACE_OUTER_BOUND('',#5826,.T.);
#4002=FACE_OUTER_BOUND('',#5827,.T.);
#4003=FACE_OUTER_BOUND('',#5828,.T.);
#4004=FACE_OUTER_BOUND('',#5829,.T.);
#4005=FACE_OUTER_BOUND('',#5830,.T.);
#4006=FACE_OUTER_BOUND('',#5831,.T.);
#4007=FACE_OUTER_BOUND('',#5832,.T.);
#4008=FACE_OUTER_BOUND('',#5833,.T.);
#4009=FACE_OUTER_BOUND('',#5834,.T.);
#4010=FACE_OUTER_BOUND('',#5835,.T.);
#4011=FACE_OUTER_BOUND('',#5836,.T.);
#4012=FACE_OUTER_BOUND('',#5837,.T.);
#4013=FACE_OUTER_BOUND('',#5838,.T.);
#4014=FACE_OUTER_BOUND('',#5839,.T.);
#4015=FACE_OUTER_BOUND('',#5840,.T.);
#4016=FACE_OUTER_BOUND('',#5841,.T.);
#4017=FACE_OUTER_BOUND('',#5842,.T.);
#4018=FACE_OUTER_BOUND('',#5843,.T.);
#4019=FACE_OUTER_BOUND('',#5844,.T.);
#4020=FACE_OUTER_BOUND('',#5845,.T.);
#4021=FACE_OUTER_BOUND('',#5846,.T.);
#4022=FACE_OUTER_BOUND('',#5847,.T.);
#4023=FACE_OUTER_BOUND('',#5848,.T.);
#4024=FACE_OUTER_BOUND('',#5849,.T.);
#4025=FACE_OUTER_BOUND('',#5850,.T.);
#4026=FACE_OUTER_BOUND('',#5851,.T.);
#4027=FACE_OUTER_BOUND('',#5852,.T.);
#4028=FACE_OUTER_BOUND('',#5853,.T.);
#4029=FACE_OUTER_BOUND('',#5854,.T.);
#4030=FACE_OUTER_BOUND('',#5855,.T.);
#4031=FACE_OUTER_BOUND('',#5856,.T.);
#4032=FACE_OUTER_BOUND('',#5857,.T.);
#4033=FACE_OUTER_BOUND('',#5858,.T.);
#4034=FACE_OUTER_BOUND('',#5859,.T.);
#4035=FACE_OUTER_BOUND('',#5860,.T.);
#4036=FACE_OUTER_BOUND('',#5861,.T.);
#4037=FACE_OUTER_BOUND('',#5862,.T.);
#4038=FACE_OUTER_BOUND('',#5863,.T.);
#4039=FACE_OUTER_BOUND('',#5864,.T.);
#4040=FACE_OUTER_BOUND('',#5865,.T.);
#4041=FACE_OUTER_BOUND('',#5866,.T.);
#4042=FACE_OUTER_BOUND('',#5867,.T.);
#4043=FACE_OUTER_BOUND('',#5868,.T.);
#4044=FACE_OUTER_BOUND('',#5869,.T.);
#4045=FACE_OUTER_BOUND('',#5870,.T.);
#4046=FACE_OUTER_BOUND('',#5871,.T.);
#4047=FACE_OUTER_BOUND('',#5872,.T.);
#4048=FACE_OUTER_BOUND('',#5873,.T.);
#4049=FACE_OUTER_BOUND('',#5875,.T.);
#4050=FACE_OUTER_BOUND('',#5876,.T.);
#4051=FACE_OUTER_BOUND('',#5877,.T.);
#4052=FACE_OUTER_BOUND('',#5878,.T.);
#4053=FACE_OUTER_BOUND('',#5879,.T.);
#4054=FACE_OUTER_BOUND('',#5880,.T.);
#4055=FACE_OUTER_BOUND('',#5881,.T.);
#4056=FACE_OUTER_BOUND('',#5882,.T.);
#4057=FACE_OUTER_BOUND('',#5883,.T.);
#4058=FACE_OUTER_BOUND('',#5884,.T.);
#4059=FACE_OUTER_BOUND('',#5885,.T.);
#4060=FACE_OUTER_BOUND('',#5886,.T.);
#4061=FACE_OUTER_BOUND('',#5887,.T.);
#4062=FACE_OUTER_BOUND('',#5888,.T.);
#4063=FACE_OUTER_BOUND('',#5889,.T.);
#4064=FACE_OUTER_BOUND('',#5891,.T.);
#4065=FACE_OUTER_BOUND('',#5892,.T.);
#4066=FACE_OUTER_BOUND('',#5893,.T.);
#4067=FACE_OUTER_BOUND('',#5894,.T.);
#4068=FACE_OUTER_BOUND('',#5895,.T.);
#4069=FACE_OUTER_BOUND('',#5896,.T.);
#4070=FACE_OUTER_BOUND('',#5897,.T.);
#4071=FACE_OUTER_BOUND('',#5898,.T.);
#4072=FACE_OUTER_BOUND('',#5899,.T.);
#4073=FACE_OUTER_BOUND('',#5900,.T.);
#4074=FACE_OUTER_BOUND('',#5901,.T.);
#4075=FACE_OUTER_BOUND('',#5902,.T.);
#4076=FACE_OUTER_BOUND('',#5903,.T.);
#4077=FACE_OUTER_BOUND('',#5904,.T.);
#4078=FACE_OUTER_BOUND('',#5905,.T.);
#4079=FACE_OUTER_BOUND('',#5906,.T.);
#4080=FACE_OUTER_BOUND('',#5907,.T.);
#4081=FACE_OUTER_BOUND('',#5908,.T.);
#4082=FACE_OUTER_BOUND('',#5909,.T.);
#4083=FACE_OUTER_BOUND('',#5910,.T.);
#4084=FACE_OUTER_BOUND('',#5911,.T.);
#4085=FACE_OUTER_BOUND('',#5912,.T.);
#4086=FACE_OUTER_BOUND('',#5913,.T.);
#4087=FACE_OUTER_BOUND('',#5914,.T.);
#4088=FACE_OUTER_BOUND('',#5915,.T.);
#4089=FACE_OUTER_BOUND('',#5916,.T.);
#4090=FACE_OUTER_BOUND('',#5917,.T.);
#4091=FACE_OUTER_BOUND('',#5918,.T.);
#4092=FACE_OUTER_BOUND('',#5919,.T.);
#4093=FACE_OUTER_BOUND('',#5920,.T.);
#4094=FACE_OUTER_BOUND('',#5921,.T.);
#4095=FACE_OUTER_BOUND('',#5922,.T.);
#4096=FACE_OUTER_BOUND('',#5923,.T.);
#4097=FACE_OUTER_BOUND('',#5924,.T.);
#4098=FACE_OUTER_BOUND('',#5925,.T.);
#4099=FACE_OUTER_BOUND('',#5926,.T.);
#4100=FACE_OUTER_BOUND('',#5927,.T.);
#4101=FACE_OUTER_BOUND('',#5928,.T.);
#4102=FACE_OUTER_BOUND('',#5929,.T.);
#4103=FACE_OUTER_BOUND('',#5930,.T.);
#4104=FACE_OUTER_BOUND('',#5931,.T.);
#4105=FACE_OUTER_BOUND('',#5932,.T.);
#4106=FACE_OUTER_BOUND('',#5933,.T.);
#4107=FACE_OUTER_BOUND('',#5934,.T.);
#4108=FACE_OUTER_BOUND('',#5935,.T.);
#4109=FACE_OUTER_BOUND('',#5936,.T.);
#4110=FACE_OUTER_BOUND('',#5937,.T.);
#4111=FACE_OUTER_BOUND('',#5938,.T.);
#4112=FACE_OUTER_BOUND('',#5939,.T.);
#4113=FACE_OUTER_BOUND('',#5940,.T.);
#4114=FACE_OUTER_BOUND('',#5941,.T.);
#4115=FACE_OUTER_BOUND('',#5942,.T.);
#4116=FACE_OUTER_BOUND('',#5943,.T.);
#4117=FACE_OUTER_BOUND('',#5944,.T.);
#4118=FACE_OUTER_BOUND('',#5945,.T.);
#4119=FACE_OUTER_BOUND('',#5946,.T.);
#4120=FACE_OUTER_BOUND('',#5947,.T.);
#4121=FACE_OUTER_BOUND('',#5948,.T.);
#4122=FACE_OUTER_BOUND('',#5949,.T.);
#4123=FACE_OUTER_BOUND('',#5950,.T.);
#4124=FACE_OUTER_BOUND('',#5951,.T.);
#4125=FACE_OUTER_BOUND('',#5952,.T.);
#4126=FACE_OUTER_BOUND('',#5953,.T.);
#4127=FACE_OUTER_BOUND('',#5954,.T.);
#4128=FACE_OUTER_BOUND('',#5955,.T.);
#4129=FACE_OUTER_BOUND('',#5956,.T.);
#4130=FACE_OUTER_BOUND('',#5957,.T.);
#4131=FACE_OUTER_BOUND('',#5958,.T.);
#4132=FACE_OUTER_BOUND('',#5959,.T.);
#4133=FACE_OUTER_BOUND('',#5960,.T.);
#4134=FACE_OUTER_BOUND('',#5961,.T.);
#4135=FACE_OUTER_BOUND('',#5962,.T.);
#4136=FACE_OUTER_BOUND('',#5963,.T.);
#4137=FACE_OUTER_BOUND('',#5964,.T.);
#4138=FACE_OUTER_BOUND('',#5965,.T.);
#4139=FACE_OUTER_BOUND('',#5966,.T.);
#4140=FACE_OUTER_BOUND('',#5967,.T.);
#4141=FACE_OUTER_BOUND('',#5968,.T.);
#4142=FACE_OUTER_BOUND('',#5969,.T.);
#4143=FACE_OUTER_BOUND('',#5970,.T.);
#4144=FACE_OUTER_BOUND('',#5971,.T.);
#4145=FACE_OUTER_BOUND('',#5972,.T.);
#4146=FACE_OUTER_BOUND('',#5973,.T.);
#4147=FACE_OUTER_BOUND('',#5974,.T.);
#4148=FACE_OUTER_BOUND('',#5975,.T.);
#4149=FACE_OUTER_BOUND('',#5976,.T.);
#4150=FACE_OUTER_BOUND('',#5977,.T.);
#4151=FACE_OUTER_BOUND('',#5978,.T.);
#4152=FACE_OUTER_BOUND('',#5979,.T.);
#4153=FACE_OUTER_BOUND('',#5980,.T.);
#4154=FACE_OUTER_BOUND('',#5981,.T.);
#4155=FACE_OUTER_BOUND('',#5982,.T.);
#4156=FACE_OUTER_BOUND('',#5983,.T.);
#4157=FACE_OUTER_BOUND('',#5984,.T.);
#4158=FACE_OUTER_BOUND('',#5985,.T.);
#4159=FACE_OUTER_BOUND('',#5986,.T.);
#4160=FACE_OUTER_BOUND('',#5987,.T.);
#4161=FACE_OUTER_BOUND('',#5988,.T.);
#4162=FACE_OUTER_BOUND('',#5989,.T.);
#4163=FACE_OUTER_BOUND('',#5990,.T.);
#4164=FACE_OUTER_BOUND('',#5991,.T.);
#4165=FACE_OUTER_BOUND('',#5992,.T.);
#4166=FACE_OUTER_BOUND('',#5993,.T.);
#4167=FACE_OUTER_BOUND('',#5994,.T.);
#4168=FACE_OUTER_BOUND('',#5995,.T.);
#4169=FACE_OUTER_BOUND('',#5996,.T.);
#4170=FACE_OUTER_BOUND('',#5997,.T.);
#4171=FACE_OUTER_BOUND('',#5998,.T.);
#4172=FACE_OUTER_BOUND('',#5999,.T.);
#4173=FACE_OUTER_BOUND('',#6000,.T.);
#4174=FACE_OUTER_BOUND('',#6001,.T.);
#4175=FACE_OUTER_BOUND('',#6002,.T.);
#4176=FACE_OUTER_BOUND('',#6003,.T.);
#4177=FACE_OUTER_BOUND('',#6004,.T.);
#4178=FACE_OUTER_BOUND('',#6005,.T.);
#4179=FACE_OUTER_BOUND('',#6006,.T.);
#4180=FACE_OUTER_BOUND('',#6007,.T.);
#4181=FACE_OUTER_BOUND('',#6008,.T.);
#4182=FACE_OUTER_BOUND('',#6009,.T.);
#4183=FACE_OUTER_BOUND('',#6010,.T.);
#4184=FACE_OUTER_BOUND('',#6011,.T.);
#4185=FACE_OUTER_BOUND('',#6012,.T.);
#4186=FACE_OUTER_BOUND('',#6013,.T.);
#4187=FACE_OUTER_BOUND('',#6014,.T.);
#4188=FACE_OUTER_BOUND('',#6015,.T.);
#4189=FACE_OUTER_BOUND('',#6016,.T.);
#4190=FACE_OUTER_BOUND('',#6017,.T.);
#4191=FACE_OUTER_BOUND('',#6018,.T.);
#4192=FACE_OUTER_BOUND('',#6019,.T.);
#4193=FACE_OUTER_BOUND('',#6020,.T.);
#4194=FACE_OUTER_BOUND('',#6021,.T.);
#4195=FACE_OUTER_BOUND('',#6022,.T.);
#4196=FACE_OUTER_BOUND('',#6023,.T.);
#4197=FACE_OUTER_BOUND('',#6024,.T.);
#4198=FACE_OUTER_BOUND('',#6025,.T.);
#4199=FACE_OUTER_BOUND('',#6026,.T.);
#4200=FACE_OUTER_BOUND('',#6027,.T.);
#4201=FACE_OUTER_BOUND('',#6028,.T.);
#4202=FACE_OUTER_BOUND('',#6029,.T.);
#4203=FACE_OUTER_BOUND('',#6030,.T.);
#4204=FACE_OUTER_BOUND('',#6031,.T.);
#4205=FACE_OUTER_BOUND('',#6032,.T.);
#4206=FACE_OUTER_BOUND('',#6033,.T.);
#4207=FACE_OUTER_BOUND('',#6034,.T.);
#4208=FACE_OUTER_BOUND('',#6035,.T.);
#4209=FACE_OUTER_BOUND('',#6036,.T.);
#4210=FACE_OUTER_BOUND('',#6037,.T.);
#4211=FACE_OUTER_BOUND('',#6038,.T.);
#4212=FACE_OUTER_BOUND('',#6039,.T.);
#4213=FACE_OUTER_BOUND('',#6040,.T.);
#4214=FACE_OUTER_BOUND('',#6041,.T.);
#4215=FACE_OUTER_BOUND('',#6042,.T.);
#4216=FACE_OUTER_BOUND('',#6043,.T.);
#4217=FACE_OUTER_BOUND('',#6044,.T.);
#4218=FACE_OUTER_BOUND('',#6045,.T.);
#4219=FACE_OUTER_BOUND('',#6046,.T.);
#4220=FACE_OUTER_BOUND('',#6047,.T.);
#4221=FACE_OUTER_BOUND('',#6048,.T.);
#4222=FACE_OUTER_BOUND('',#6049,.T.);
#4223=FACE_OUTER_BOUND('',#6050,.T.);
#4224=FACE_OUTER_BOUND('',#6051,.T.);
#4225=FACE_OUTER_BOUND('',#6052,.T.);
#4226=FACE_OUTER_BOUND('',#6053,.T.);
#4227=FACE_OUTER_BOUND('',#6054,.T.);
#4228=FACE_OUTER_BOUND('',#6055,.T.);
#4229=FACE_OUTER_BOUND('',#6056,.T.);
#4230=FACE_OUTER_BOUND('',#6057,.T.);
#4231=FACE_OUTER_BOUND('',#6058,.T.);
#4232=FACE_OUTER_BOUND('',#6059,.T.);
#4233=FACE_OUTER_BOUND('',#6060,.T.);
#4234=FACE_OUTER_BOUND('',#6061,.T.);
#4235=FACE_OUTER_BOUND('',#6062,.T.);
#4236=FACE_OUTER_BOUND('',#6063,.T.);
#4237=FACE_OUTER_BOUND('',#6064,.T.);
#4238=FACE_OUTER_BOUND('',#6065,.T.);
#4239=FACE_OUTER_BOUND('',#6066,.T.);
#4240=FACE_OUTER_BOUND('',#6067,.T.);
#4241=FACE_OUTER_BOUND('',#6068,.T.);
#4242=FACE_OUTER_BOUND('',#6069,.T.);
#4243=FACE_OUTER_BOUND('',#6070,.T.);
#4244=FACE_OUTER_BOUND('',#6071,.T.);
#4245=FACE_OUTER_BOUND('',#6072,.T.);
#4246=FACE_OUTER_BOUND('',#6073,.T.);
#4247=FACE_OUTER_BOUND('',#6074,.T.);
#4248=FACE_OUTER_BOUND('',#6075,.T.);
#4249=FACE_OUTER_BOUND('',#6076,.T.);
#4250=FACE_OUTER_BOUND('',#6077,.T.);
#4251=FACE_OUTER_BOUND('',#6078,.T.);
#4252=FACE_OUTER_BOUND('',#6079,.T.);
#4253=FACE_OUTER_BOUND('',#6080,.T.);
#4254=FACE_OUTER_BOUND('',#6081,.T.);
#4255=FACE_OUTER_BOUND('',#6082,.T.);
#4256=FACE_OUTER_BOUND('',#6083,.T.);
#4257=FACE_OUTER_BOUND('',#6084,.T.);
#4258=FACE_OUTER_BOUND('',#6085,.T.);
#4259=FACE_OUTER_BOUND('',#6086,.T.);
#4260=FACE_OUTER_BOUND('',#6087,.T.);
#4261=FACE_OUTER_BOUND('',#6088,.T.);
#4262=FACE_OUTER_BOUND('',#6089,.T.);
#4263=FACE_OUTER_BOUND('',#6090,.T.);
#4264=FACE_OUTER_BOUND('',#6091,.T.);
#4265=FACE_OUTER_BOUND('',#6092,.T.);
#4266=FACE_OUTER_BOUND('',#6093,.T.);
#4267=FACE_OUTER_BOUND('',#6094,.T.);
#4268=FACE_OUTER_BOUND('',#6095,.T.);
#4269=FACE_OUTER_BOUND('',#6096,.T.);
#4270=FACE_OUTER_BOUND('',#6097,.T.);
#4271=FACE_OUTER_BOUND('',#6098,.T.);
#4272=FACE_OUTER_BOUND('',#6099,.T.);
#4273=FACE_OUTER_BOUND('',#6100,.T.);
#4274=FACE_OUTER_BOUND('',#6101,.T.);
#4275=FACE_OUTER_BOUND('',#6102,.T.);
#4276=FACE_OUTER_BOUND('',#6103,.T.);
#4277=FACE_OUTER_BOUND('',#6104,.T.);
#4278=FACE_OUTER_BOUND('',#6105,.T.);
#4279=FACE_OUTER_BOUND('',#6106,.T.);
#4280=FACE_OUTER_BOUND('',#6107,.T.);
#4281=FACE_OUTER_BOUND('',#6108,.T.);
#4282=FACE_OUTER_BOUND('',#6109,.T.);
#4283=FACE_OUTER_BOUND('',#6110,.T.);
#4284=FACE_OUTER_BOUND('',#6111,.T.);
#4285=FACE_OUTER_BOUND('',#6112,.T.);
#4286=FACE_OUTER_BOUND('',#6113,.T.);
#4287=FACE_OUTER_BOUND('',#6114,.T.);
#4288=FACE_OUTER_BOUND('',#6115,.T.);
#4289=FACE_OUTER_BOUND('',#6116,.T.);
#4290=FACE_OUTER_BOUND('',#6117,.T.);
#4291=FACE_OUTER_BOUND('',#6118,.T.);
#4292=FACE_OUTER_BOUND('',#6119,.T.);
#4293=FACE_OUTER_BOUND('',#6120,.T.);
#4294=FACE_OUTER_BOUND('',#6121,.T.);
#4295=FACE_OUTER_BOUND('',#6122,.T.);
#4296=FACE_OUTER_BOUND('',#6123,.T.);
#4297=FACE_OUTER_BOUND('',#6124,.T.);
#4298=FACE_OUTER_BOUND('',#6125,.T.);
#4299=FACE_OUTER_BOUND('',#6126,.T.);
#4300=FACE_OUTER_BOUND('',#6127,.T.);
#4301=FACE_OUTER_BOUND('',#6128,.T.);
#4302=FACE_OUTER_BOUND('',#6129,.T.);
#4303=FACE_OUTER_BOUND('',#6130,.T.);
#4304=FACE_OUTER_BOUND('',#6131,.T.);
#4305=FACE_OUTER_BOUND('',#6132,.T.);
#4306=FACE_OUTER_BOUND('',#6133,.T.);
#4307=FACE_OUTER_BOUND('',#6134,.T.);
#4308=FACE_OUTER_BOUND('',#6135,.T.);
#4309=FACE_OUTER_BOUND('',#6136,.T.);
#4310=FACE_OUTER_BOUND('',#6137,.T.);
#4311=FACE_OUTER_BOUND('',#6138,.T.);
#4312=FACE_OUTER_BOUND('',#6139,.T.);
#4313=FACE_OUTER_BOUND('',#6140,.T.);
#4314=FACE_OUTER_BOUND('',#6141,.T.);
#4315=FACE_OUTER_BOUND('',#6142,.T.);
#4316=FACE_OUTER_BOUND('',#6143,.T.);
#4317=FACE_OUTER_BOUND('',#6144,.T.);
#4318=FACE_OUTER_BOUND('',#6145,.T.);
#4319=FACE_OUTER_BOUND('',#6146,.T.);
#4320=FACE_OUTER_BOUND('',#6147,.T.);
#4321=FACE_OUTER_BOUND('',#6148,.T.);
#4322=FACE_OUTER_BOUND('',#6149,.T.);
#4323=FACE_OUTER_BOUND('',#6150,.T.);
#4324=FACE_OUTER_BOUND('',#6151,.T.);
#4325=FACE_OUTER_BOUND('',#6152,.T.);
#4326=FACE_OUTER_BOUND('',#6153,.T.);
#4327=FACE_OUTER_BOUND('',#6154,.T.);
#4328=FACE_OUTER_BOUND('',#6155,.T.);
#4329=FACE_OUTER_BOUND('',#6156,.T.);
#4330=FACE_OUTER_BOUND('',#6157,.T.);
#4331=FACE_OUTER_BOUND('',#6158,.T.);
#4332=FACE_OUTER_BOUND('',#6159,.T.);
#4333=FACE_OUTER_BOUND('',#6160,.T.);
#4334=FACE_OUTER_BOUND('',#6161,.T.);
#4335=FACE_OUTER_BOUND('',#6162,.T.);
#4336=FACE_OUTER_BOUND('',#6163,.T.);
#4337=FACE_OUTER_BOUND('',#6164,.T.);
#4338=FACE_OUTER_BOUND('',#6165,.T.);
#4339=FACE_OUTER_BOUND('',#6166,.T.);
#4340=FACE_OUTER_BOUND('',#6167,.T.);
#4341=FACE_OUTER_BOUND('',#6168,.T.);
#4342=FACE_OUTER_BOUND('',#6169,.T.);
#4343=FACE_OUTER_BOUND('',#6170,.T.);
#4344=FACE_OUTER_BOUND('',#6171,.T.);
#4345=FACE_OUTER_BOUND('',#6172,.T.);
#4346=FACE_OUTER_BOUND('',#6173,.T.);
#4347=FACE_OUTER_BOUND('',#6174,.T.);
#4348=FACE_OUTER_BOUND('',#6175,.T.);
#4349=FACE_OUTER_BOUND('',#6176,.T.);
#4350=FACE_OUTER_BOUND('',#6177,.T.);
#4351=FACE_OUTER_BOUND('',#6178,.T.);
#4352=FACE_OUTER_BOUND('',#6179,.T.);
#4353=FACE_OUTER_BOUND('',#6180,.T.);
#4354=FACE_OUTER_BOUND('',#6181,.T.);
#4355=FACE_OUTER_BOUND('',#6182,.T.);
#4356=FACE_OUTER_BOUND('',#6183,.T.);
#4357=FACE_OUTER_BOUND('',#6184,.T.);
#4358=FACE_OUTER_BOUND('',#6185,.T.);
#4359=FACE_OUTER_BOUND('',#6186,.T.);
#4360=FACE_OUTER_BOUND('',#6187,.T.);
#4361=FACE_OUTER_BOUND('',#6188,.T.);
#4362=FACE_OUTER_BOUND('',#6189,.T.);
#4363=FACE_OUTER_BOUND('',#6190,.T.);
#4364=FACE_OUTER_BOUND('',#6191,.T.);
#4365=FACE_OUTER_BOUND('',#6192,.T.);
#4366=FACE_OUTER_BOUND('',#6193,.T.);
#4367=FACE_OUTER_BOUND('',#6194,.T.);
#4368=FACE_OUTER_BOUND('',#6195,.T.);
#4369=FACE_OUTER_BOUND('',#6196,.T.);
#4370=FACE_OUTER_BOUND('',#6197,.T.);
#4371=FACE_OUTER_BOUND('',#6198,.T.);
#4372=FACE_OUTER_BOUND('',#6199,.T.);
#4373=FACE_OUTER_BOUND('',#6200,.T.);
#4374=FACE_OUTER_BOUND('',#6201,.T.);
#4375=FACE_OUTER_BOUND('',#6202,.T.);
#4376=FACE_OUTER_BOUND('',#6203,.T.);
#4377=FACE_OUTER_BOUND('',#6204,.T.);
#4378=FACE_OUTER_BOUND('',#6205,.T.);
#4379=FACE_OUTER_BOUND('',#6206,.T.);
#4380=FACE_OUTER_BOUND('',#6207,.T.);
#4381=FACE_OUTER_BOUND('',#6208,.T.);
#4382=FACE_OUTER_BOUND('',#6209,.T.);
#4383=FACE_OUTER_BOUND('',#6210,.T.);
#4384=FACE_OUTER_BOUND('',#6211,.T.);
#4385=FACE_OUTER_BOUND('',#6212,.T.);
#4386=FACE_OUTER_BOUND('',#6213,.T.);
#4387=FACE_OUTER_BOUND('',#6214,.T.);
#4388=FACE_OUTER_BOUND('',#6215,.T.);
#4389=FACE_OUTER_BOUND('',#6216,.T.);
#4390=FACE_OUTER_BOUND('',#6217,.T.);
#4391=FACE_OUTER_BOUND('',#6218,.T.);
#4392=FACE_OUTER_BOUND('',#6219,.T.);
#4393=FACE_OUTER_BOUND('',#6220,.T.);
#4394=FACE_OUTER_BOUND('',#6221,.T.);
#4395=FACE_OUTER_BOUND('',#6222,.T.);
#4396=FACE_OUTER_BOUND('',#6223,.T.);
#4397=FACE_OUTER_BOUND('',#6224,.T.);
#4398=FACE_OUTER_BOUND('',#6225,.T.);
#4399=FACE_OUTER_BOUND('',#6226,.T.);
#4400=FACE_OUTER_BOUND('',#6227,.T.);
#4401=FACE_OUTER_BOUND('',#6228,.T.);
#4402=FACE_OUTER_BOUND('',#6229,.T.);
#4403=FACE_OUTER_BOUND('',#6230,.T.);
#4404=FACE_OUTER_BOUND('',#6231,.T.);
#4405=FACE_OUTER_BOUND('',#6232,.T.);
#4406=FACE_OUTER_BOUND('',#6233,.T.);
#4407=FACE_OUTER_BOUND('',#6234,.T.);
#4408=FACE_OUTER_BOUND('',#6235,.T.);
#4409=FACE_OUTER_BOUND('',#6236,.T.);
#4410=FACE_OUTER_BOUND('',#6237,.T.);
#4411=FACE_OUTER_BOUND('',#6238,.T.);
#4412=FACE_OUTER_BOUND('',#6239,.T.);
#4413=FACE_OUTER_BOUND('',#6240,.T.);
#4414=FACE_OUTER_BOUND('',#6241,.T.);
#4415=FACE_OUTER_BOUND('',#6242,.T.);
#4416=FACE_OUTER_BOUND('',#6243,.T.);
#4417=FACE_OUTER_BOUND('',#6244,.T.);
#4418=FACE_OUTER_BOUND('',#6245,.T.);
#4419=FACE_OUTER_BOUND('',#6246,.T.);
#4420=FACE_OUTER_BOUND('',#6247,.T.);
#4421=FACE_OUTER_BOUND('',#6248,.T.);
#4422=FACE_OUTER_BOUND('',#6249,.T.);
#4423=FACE_OUTER_BOUND('',#6250,.T.);
#4424=FACE_OUTER_BOUND('',#6251,.T.);
#4425=FACE_OUTER_BOUND('',#6252,.T.);
#4426=FACE_OUTER_BOUND('',#6253,.T.);
#4427=FACE_OUTER_BOUND('',#6254,.T.);
#4428=FACE_OUTER_BOUND('',#6255,.T.);
#4429=FACE_OUTER_BOUND('',#6256,.T.);
#4430=FACE_OUTER_BOUND('',#6257,.T.);
#4431=FACE_OUTER_BOUND('',#6258,.T.);
#4432=FACE_OUTER_BOUND('',#6259,.T.);
#4433=FACE_OUTER_BOUND('',#6260,.T.);
#4434=FACE_OUTER_BOUND('',#6261,.T.);
#4435=FACE_OUTER_BOUND('',#6262,.T.);
#4436=FACE_OUTER_BOUND('',#6263,.T.);
#4437=FACE_OUTER_BOUND('',#6264,.T.);
#4438=FACE_OUTER_BOUND('',#6265,.T.);
#4439=FACE_OUTER_BOUND('',#6266,.T.);
#4440=FACE_OUTER_BOUND('',#6267,.T.);
#4441=FACE_OUTER_BOUND('',#6268,.T.);
#4442=FACE_OUTER_BOUND('',#6269,.T.);
#4443=FACE_OUTER_BOUND('',#6270,.T.);
#4444=FACE_OUTER_BOUND('',#6271,.T.);
#4445=FACE_OUTER_BOUND('',#6272,.T.);
#4446=FACE_OUTER_BOUND('',#6273,.T.);
#4447=FACE_OUTER_BOUND('',#6274,.T.);
#4448=FACE_OUTER_BOUND('',#6275,.T.);
#4449=FACE_OUTER_BOUND('',#6276,.T.);
#4450=FACE_OUTER_BOUND('',#6277,.T.);
#4451=FACE_OUTER_BOUND('',#6278,.T.);
#4452=FACE_OUTER_BOUND('',#6279,.T.);
#4453=FACE_OUTER_BOUND('',#6280,.T.);
#4454=FACE_OUTER_BOUND('',#6281,.T.);
#4455=FACE_OUTER_BOUND('',#6282,.T.);
#4456=FACE_OUTER_BOUND('',#6283,.T.);
#4457=FACE_OUTER_BOUND('',#6284,.T.);
#4458=FACE_OUTER_BOUND('',#6285,.T.);
#4459=FACE_OUTER_BOUND('',#6286,.T.);
#4460=FACE_OUTER_BOUND('',#6287,.T.);
#4461=FACE_OUTER_BOUND('',#6288,.T.);
#4462=FACE_OUTER_BOUND('',#6289,.T.);
#4463=FACE_OUTER_BOUND('',#6290,.T.);
#4464=FACE_OUTER_BOUND('',#6291,.T.);
#4465=FACE_OUTER_BOUND('',#6292,.T.);
#4466=FACE_OUTER_BOUND('',#6293,.T.);
#4467=FACE_OUTER_BOUND('',#6294,.T.);
#4468=FACE_OUTER_BOUND('',#6295,.T.);
#4469=FACE_OUTER_BOUND('',#6296,.T.);
#4470=FACE_OUTER_BOUND('',#6297,.T.);
#4471=FACE_OUTER_BOUND('',#6298,.T.);
#4472=FACE_OUTER_BOUND('',#6299,.T.);
#4473=FACE_OUTER_BOUND('',#6300,.T.);
#4474=FACE_OUTER_BOUND('',#6301,.T.);
#4475=FACE_OUTER_BOUND('',#6302,.T.);
#4476=FACE_OUTER_BOUND('',#6303,.T.);
#4477=FACE_OUTER_BOUND('',#6304,.T.);
#4478=FACE_OUTER_BOUND('',#6305,.T.);
#4479=FACE_OUTER_BOUND('',#6306,.T.);
#4480=FACE_OUTER_BOUND('',#6307,.T.);
#4481=FACE_OUTER_BOUND('',#6308,.T.);
#4482=FACE_OUTER_BOUND('',#6309,.T.);
#4483=FACE_OUTER_BOUND('',#6310,.T.);
#4484=FACE_OUTER_BOUND('',#6311,.T.);
#4485=FACE_OUTER_BOUND('',#6312,.T.);
#4486=FACE_OUTER_BOUND('',#6313,.T.);
#4487=FACE_OUTER_BOUND('',#6314,.T.);
#4488=FACE_OUTER_BOUND('',#6315,.T.);
#4489=FACE_OUTER_BOUND('',#6316,.T.);
#4490=FACE_OUTER_BOUND('',#6317,.T.);
#4491=FACE_OUTER_BOUND('',#6318,.T.);
#4492=FACE_OUTER_BOUND('',#6319,.T.);
#4493=FACE_OUTER_BOUND('',#6320,.T.);
#4494=FACE_OUTER_BOUND('',#6321,.T.);
#4495=FACE_OUTER_BOUND('',#6322,.T.);
#4496=FACE_OUTER_BOUND('',#6323,.T.);
#4497=FACE_OUTER_BOUND('',#6324,.T.);
#4498=FACE_OUTER_BOUND('',#6325,.T.);
#4499=FACE_OUTER_BOUND('',#6326,.T.);
#4500=FACE_OUTER_BOUND('',#6327,.T.);
#4501=FACE_OUTER_BOUND('',#6328,.T.);
#4502=FACE_OUTER_BOUND('',#6433,.T.);
#4503=FACE_OUTER_BOUND('',#6436,.T.);
#4504=FACE_OUTER_BOUND('',#6437,.T.);
#4505=FACE_OUTER_BOUND('',#6438,.T.);
#4506=FACE_OUTER_BOUND('',#6439,.T.);
#4507=FACE_OUTER_BOUND('',#6440,.T.);
#4508=FACE_OUTER_BOUND('',#6441,.T.);
#4509=FACE_OUTER_BOUND('',#6442,.T.);
#4510=FACE_OUTER_BOUND('',#6443,.T.);
#4511=FACE_OUTER_BOUND('',#6444,.T.);
#4512=FACE_OUTER_BOUND('',#6445,.T.);
#4513=FACE_OUTER_BOUND('',#6446,.T.);
#4514=FACE_OUTER_BOUND('',#6447,.T.);
#4515=FACE_OUTER_BOUND('',#6448,.T.);
#4516=FACE_OUTER_BOUND('',#6449,.T.);
#4517=FACE_OUTER_BOUND('',#6450,.T.);
#4518=FACE_OUTER_BOUND('',#6451,.T.);
#4519=FACE_OUTER_BOUND('',#6452,.T.);
#4520=FACE_OUTER_BOUND('',#6453,.T.);
#4521=FACE_OUTER_BOUND('',#6454,.T.);
#4522=FACE_OUTER_BOUND('',#6455,.T.);
#4523=FACE_OUTER_BOUND('',#6456,.T.);
#4524=FACE_OUTER_BOUND('',#6457,.T.);
#4525=FACE_OUTER_BOUND('',#6458,.T.);
#4526=FACE_OUTER_BOUND('',#6459,.T.);
#4527=FACE_OUTER_BOUND('',#6460,.T.);
#4528=FACE_OUTER_BOUND('',#6461,.T.);
#4529=FACE_OUTER_BOUND('',#6462,.T.);
#4530=FACE_OUTER_BOUND('',#6463,.T.);
#4531=FACE_OUTER_BOUND('',#6464,.T.);
#4532=FACE_OUTER_BOUND('',#6465,.T.);
#4533=FACE_OUTER_BOUND('',#6466,.T.);
#4534=FACE_OUTER_BOUND('',#6467,.T.);
#4535=FACE_OUTER_BOUND('',#6468,.T.);
#4536=FACE_OUTER_BOUND('',#6469,.T.);
#4537=FACE_OUTER_BOUND('',#6470,.T.);
#4538=FACE_OUTER_BOUND('',#6471,.T.);
#4539=FACE_OUTER_BOUND('',#6472,.T.);
#4540=FACE_OUTER_BOUND('',#6473,.T.);
#4541=FACE_OUTER_BOUND('',#6474,.T.);
#4542=FACE_OUTER_BOUND('',#6475,.T.);
#4543=FACE_OUTER_BOUND('',#6476,.T.);
#4544=FACE_OUTER_BOUND('',#6477,.T.);
#4545=FACE_OUTER_BOUND('',#6478,.T.);
#4546=FACE_OUTER_BOUND('',#6479,.T.);
#4547=FACE_OUTER_BOUND('',#6480,.T.);
#4548=FACE_OUTER_BOUND('',#6481,.T.);
#4549=FACE_OUTER_BOUND('',#6482,.T.);
#4550=FACE_OUTER_BOUND('',#6483,.T.);
#4551=FACE_OUTER_BOUND('',#6484,.T.);
#4552=FACE_OUTER_BOUND('',#6485,.T.);
#4553=FACE_OUTER_BOUND('',#6486,.T.);
#4554=FACE_OUTER_BOUND('',#6487,.T.);
#4555=FACE_OUTER_BOUND('',#6488,.T.);
#4556=FACE_OUTER_BOUND('',#6489,.T.);
#4557=FACE_OUTER_BOUND('',#6490,.T.);
#4558=FACE_OUTER_BOUND('',#6491,.T.);
#4559=FACE_OUTER_BOUND('',#6492,.T.);
#4560=FACE_OUTER_BOUND('',#6493,.T.);
#4561=FACE_OUTER_BOUND('',#6496,.T.);
#4562=FACE_OUTER_BOUND('',#6497,.T.);
#4563=FACE_OUTER_BOUND('',#6500,.T.);
#4564=FACE_OUTER_BOUND('',#6501,.T.);
#4565=FACE_OUTER_BOUND('',#6502,.T.);
#4566=FACE_OUTER_BOUND('',#6503,.T.);
#4567=FACE_OUTER_BOUND('',#6515,.T.);
#4568=FACE_OUTER_BOUND('',#6516,.T.);
#4569=FACE_OUTER_BOUND('',#6517,.T.);
#4570=FACE_OUTER_BOUND('',#6518,.T.);
#4571=FACE_OUTER_BOUND('',#6519,.T.);
#4572=FACE_OUTER_BOUND('',#6522,.T.);
#4573=FACE_OUTER_BOUND('',#6523,.T.);
#4574=FACE_OUTER_BOUND('',#6524,.T.);
#4575=FACE_OUTER_BOUND('',#6525,.T.);
#4576=FACE_OUTER_BOUND('',#6527,.T.);
#4577=FACE_OUTER_BOUND('',#6528,.T.);
#4578=FACE_OUTER_BOUND('',#6530,.T.);
#4579=FACE_OUTER_BOUND('',#6531,.T.);
#4580=FACE_OUTER_BOUND('',#6532,.T.);
#4581=FACE_OUTER_BOUND('',#6533,.T.);
#4582=FACE_OUTER_BOUND('',#6534,.T.);
#4583=FACE_OUTER_BOUND('',#6535,.T.);
#4584=FACE_OUTER_BOUND('',#6536,.T.);
#4585=FACE_OUTER_BOUND('',#6537,.T.);
#4586=FACE_OUTER_BOUND('',#6538,.T.);
#4587=FACE_OUTER_BOUND('',#6539,.T.);
#4588=FACE_OUTER_BOUND('',#6540,.T.);
#4589=FACE_OUTER_BOUND('',#6541,.T.);
#4590=FACE_OUTER_BOUND('',#6542,.T.);
#4591=FACE_OUTER_BOUND('',#6543,.T.);
#4592=FACE_OUTER_BOUND('',#6544,.T.);
#4593=FACE_OUTER_BOUND('',#6545,.T.);
#4594=FACE_OUTER_BOUND('',#6546,.T.);
#4595=FACE_OUTER_BOUND('',#6547,.T.);
#4596=FACE_OUTER_BOUND('',#6548,.T.);
#4597=FACE_OUTER_BOUND('',#6549,.T.);
#4598=FACE_OUTER_BOUND('',#6550,.T.);
#4599=FACE_OUTER_BOUND('',#6551,.T.);
#4600=FACE_OUTER_BOUND('',#6552,.T.);
#4601=FACE_OUTER_BOUND('',#6553,.T.);
#4602=FACE_OUTER_BOUND('',#6554,.T.);
#4603=FACE_OUTER_BOUND('',#6555,.T.);
#4604=FACE_OUTER_BOUND('',#6556,.T.);
#4605=FACE_OUTER_BOUND('',#6557,.T.);
#4606=FACE_OUTER_BOUND('',#6558,.T.);
#4607=FACE_OUTER_BOUND('',#6559,.T.);
#4608=FACE_OUTER_BOUND('',#6560,.T.);
#4609=FACE_OUTER_BOUND('',#6561,.T.);
#4610=FACE_OUTER_BOUND('',#6562,.T.);
#4611=FACE_OUTER_BOUND('',#6563,.T.);
#4612=FACE_OUTER_BOUND('',#6564,.T.);
#4613=FACE_OUTER_BOUND('',#6565,.T.);
#4614=FACE_OUTER_BOUND('',#6566,.T.);
#4615=FACE_OUTER_BOUND('',#6567,.T.);
#4616=FACE_OUTER_BOUND('',#6568,.T.);
#4617=FACE_OUTER_BOUND('',#6569,.T.);
#4618=FACE_OUTER_BOUND('',#6570,.T.);
#4619=FACE_OUTER_BOUND('',#6571,.T.);
#4620=FACE_OUTER_BOUND('',#6572,.T.);
#4621=FACE_OUTER_BOUND('',#6573,.T.);
#4622=FACE_OUTER_BOUND('',#6574,.T.);
#4623=FACE_OUTER_BOUND('',#6575,.T.);
#4624=FACE_OUTER_BOUND('',#6576,.T.);
#4625=FACE_OUTER_BOUND('',#6577,.T.);
#4626=FACE_OUTER_BOUND('',#6578,.T.);
#4627=FACE_OUTER_BOUND('',#6579,.T.);
#4628=FACE_OUTER_BOUND('',#6580,.T.);
#4629=FACE_OUTER_BOUND('',#6581,.T.);
#4630=FACE_OUTER_BOUND('',#6582,.T.);
#4631=FACE_OUTER_BOUND('',#6583,.T.);
#4632=FACE_OUTER_BOUND('',#6584,.T.);
#4633=FACE_OUTER_BOUND('',#6585,.T.);
#4634=FACE_OUTER_BOUND('',#6586,.T.);
#4635=FACE_OUTER_BOUND('',#6587,.T.);
#4636=FACE_OUTER_BOUND('',#6588,.T.);
#4637=FACE_OUTER_BOUND('',#6589,.T.);
#4638=FACE_OUTER_BOUND('',#6590,.T.);
#4639=FACE_OUTER_BOUND('',#6591,.T.);
#4640=FACE_OUTER_BOUND('',#6592,.T.);
#4641=FACE_OUTER_BOUND('',#6593,.T.);
#4642=FACE_OUTER_BOUND('',#6594,.T.);
#4643=FACE_OUTER_BOUND('',#6595,.T.);
#4644=FACE_OUTER_BOUND('',#6596,.T.);
#4645=FACE_OUTER_BOUND('',#6597,.T.);
#4646=FACE_OUTER_BOUND('',#6598,.T.);
#4647=FACE_OUTER_BOUND('',#6599,.T.);
#4648=FACE_OUTER_BOUND('',#6600,.T.);
#4649=FACE_OUTER_BOUND('',#6602,.T.);
#4650=FACE_OUTER_BOUND('',#6603,.T.);
#4651=FACE_OUTER_BOUND('',#6604,.T.);
#4652=FACE_OUTER_BOUND('',#6606,.T.);
#4653=FACE_OUTER_BOUND('',#6607,.T.);
#4654=FACE_OUTER_BOUND('',#6608,.T.);
#4655=FACE_OUTER_BOUND('',#6609,.T.);
#4656=FACE_OUTER_BOUND('',#6611,.T.);
#4657=FACE_OUTER_BOUND('',#6612,.T.);
#4658=FACE_OUTER_BOUND('',#6613,.T.);
#4659=FACE_OUTER_BOUND('',#6619,.T.);
#4660=FACE_OUTER_BOUND('',#6620,.T.);
#4661=FACE_OUTER_BOUND('',#6621,.T.);
#4662=FACE_OUTER_BOUND('',#6622,.T.);
#4663=FACE_OUTER_BOUND('',#6623,.T.);
#4664=FACE_OUTER_BOUND('',#6624,.T.);
#4665=FACE_OUTER_BOUND('',#6625,.T.);
#4666=FACE_OUTER_BOUND('',#6626,.T.);
#4667=FACE_OUTER_BOUND('',#6627,.T.);
#4668=FACE_OUTER_BOUND('',#6628,.T.);
#4669=FACE_OUTER_BOUND('',#6630,.T.);
#4670=FACE_OUTER_BOUND('',#6632,.T.);
#4671=FACE_OUTER_BOUND('',#6633,.T.);
#4672=FACE_OUTER_BOUND('',#6634,.T.);
#4673=FACE_OUTER_BOUND('',#6635,.T.);
#4674=FACE_OUTER_BOUND('',#6636,.T.);
#4675=FACE_OUTER_BOUND('',#6640,.T.);
#4676=FACE_OUTER_BOUND('',#6641,.T.);
#4677=FACE_OUTER_BOUND('',#6642,.T.);
#4678=FACE_OUTER_BOUND('',#6643,.T.);
#4679=FACE_OUTER_BOUND('',#6644,.T.);
#4680=FACE_OUTER_BOUND('',#6645,.T.);
#4681=FACE_OUTER_BOUND('',#6646,.T.);
#4682=FACE_OUTER_BOUND('',#6647,.T.);
#4683=FACE_OUTER_BOUND('',#6648,.T.);
#4684=FACE_OUTER_BOUND('',#6649,.T.);
#4685=FACE_OUTER_BOUND('',#6650,.T.);
#4686=FACE_OUTER_BOUND('',#6651,.T.);
#4687=FACE_OUTER_BOUND('',#6652,.T.);
#4688=FACE_OUTER_BOUND('',#6653,.T.);
#4689=FACE_OUTER_BOUND('',#6654,.T.);
#4690=FACE_OUTER_BOUND('',#6655,.T.);
#4691=FACE_OUTER_BOUND('',#6656,.T.);
#4692=FACE_OUTER_BOUND('',#6657,.T.);
#4693=FACE_OUTER_BOUND('',#6658,.T.);
#4694=FACE_OUTER_BOUND('',#6659,.T.);
#4695=FACE_OUTER_BOUND('',#6660,.T.);
#4696=FACE_OUTER_BOUND('',#6661,.T.);
#4697=FACE_OUTER_BOUND('',#6662,.T.);
#4698=FACE_OUTER_BOUND('',#6663,.T.);
#4699=FACE_OUTER_BOUND('',#6664,.T.);
#4700=FACE_OUTER_BOUND('',#6665,.T.);
#4701=FACE_OUTER_BOUND('',#6666,.T.);
#4702=FACE_OUTER_BOUND('',#6667,.T.);
#4703=FACE_OUTER_BOUND('',#6668,.T.);
#4704=FACE_OUTER_BOUND('',#6669,.T.);
#4705=FACE_OUTER_BOUND('',#6670,.T.);
#4706=FACE_OUTER_BOUND('',#6671,.T.);
#4707=FACE_OUTER_BOUND('',#6672,.T.);
#4708=FACE_OUTER_BOUND('',#6673,.T.);
#4709=FACE_OUTER_BOUND('',#6674,.T.);
#4710=FACE_OUTER_BOUND('',#6675,.T.);
#4711=FACE_OUTER_BOUND('',#6676,.T.);
#4712=FACE_OUTER_BOUND('',#6677,.T.);
#4713=FACE_OUTER_BOUND('',#6678,.T.);
#4714=FACE_OUTER_BOUND('',#6679,.T.);
#4715=FACE_OUTER_BOUND('',#6680,.T.);
#4716=FACE_OUTER_BOUND('',#6681,.T.);
#4717=FACE_OUTER_BOUND('',#6682,.T.);
#4718=FACE_OUTER_BOUND('',#6683,.T.);
#4719=FACE_OUTER_BOUND('',#6684,.T.);
#4720=FACE_OUTER_BOUND('',#6685,.T.);
#4721=FACE_OUTER_BOUND('',#6686,.T.);
#4722=FACE_OUTER_BOUND('',#6687,.T.);
#4723=FACE_OUTER_BOUND('',#6688,.T.);
#4724=FACE_OUTER_BOUND('',#6689,.T.);
#4725=FACE_OUTER_BOUND('',#6690,.T.);
#4726=FACE_OUTER_BOUND('',#6691,.T.);
#4727=FACE_OUTER_BOUND('',#6692,.T.);
#4728=FACE_OUTER_BOUND('',#6693,.T.);
#4729=FACE_OUTER_BOUND('',#6694,.T.);
#4730=FACE_OUTER_BOUND('',#6695,.T.);
#4731=FACE_OUTER_BOUND('',#6696,.T.);
#4732=FACE_OUTER_BOUND('',#6697,.T.);
#4733=FACE_OUTER_BOUND('',#6698,.T.);
#4734=FACE_OUTER_BOUND('',#6699,.T.);
#4735=FACE_OUTER_BOUND('',#6700,.T.);
#4736=FACE_OUTER_BOUND('',#6702,.T.);
#4737=FACE_OUTER_BOUND('',#6703,.T.);
#4738=FACE_OUTER_BOUND('',#6704,.T.);
#4739=FACE_OUTER_BOUND('',#6705,.T.);
#4740=FACE_OUTER_BOUND('',#6706,.T.);
#4741=FACE_OUTER_BOUND('',#6707,.T.);
#4742=FACE_OUTER_BOUND('',#6708,.T.);
#4743=FACE_OUTER_BOUND('',#6709,.T.);
#4744=FACE_OUTER_BOUND('',#6710,.T.);
#4745=FACE_OUTER_BOUND('',#6711,.T.);
#4746=FACE_OUTER_BOUND('',#6712,.T.);
#4747=FACE_OUTER_BOUND('',#6713,.T.);
#4748=FACE_OUTER_BOUND('',#6714,.T.);
#4749=FACE_OUTER_BOUND('',#6715,.T.);
#4750=FACE_OUTER_BOUND('',#6716,.T.);
#4751=FACE_OUTER_BOUND('',#6717,.T.);
#4752=FACE_OUTER_BOUND('',#6718,.T.);
#4753=FACE_OUTER_BOUND('',#6719,.T.);
#4754=FACE_OUTER_BOUND('',#6720,.T.);
#4755=FACE_OUTER_BOUND('',#6721,.T.);
#4756=FACE_OUTER_BOUND('',#6722,.T.);
#4757=FACE_OUTER_BOUND('',#6723,.T.);
#4758=FACE_OUTER_BOUND('',#6724,.T.);
#4759=FACE_OUTER_BOUND('',#6725,.T.);
#4760=FACE_OUTER_BOUND('',#6726,.T.);
#4761=FACE_OUTER_BOUND('',#6727,.T.);
#4762=FACE_OUTER_BOUND('',#6728,.T.);
#4763=FACE_OUTER_BOUND('',#6729,.T.);
#4764=FACE_OUTER_BOUND('',#6730,.T.);
#4765=FACE_OUTER_BOUND('',#6731,.T.);
#4766=FACE_OUTER_BOUND('',#6732,.T.);
#4767=FACE_OUTER_BOUND('',#6733,.T.);
#4768=FACE_OUTER_BOUND('',#6734,.T.);
#4769=FACE_OUTER_BOUND('',#6735,.T.);
#4770=FACE_OUTER_BOUND('',#6736,.T.);
#4771=FACE_OUTER_BOUND('',#6737,.T.);
#4772=FACE_OUTER_BOUND('',#6738,.T.);
#4773=FACE_OUTER_BOUND('',#6739,.T.);
#4774=FACE_OUTER_BOUND('',#6740,.T.);
#4775=FACE_OUTER_BOUND('',#6741,.T.);
#4776=FACE_OUTER_BOUND('',#6742,.T.);
#4777=FACE_OUTER_BOUND('',#6743,.T.);
#4778=FACE_OUTER_BOUND('',#6744,.T.);
#4779=FACE_OUTER_BOUND('',#6745,.T.);
#4780=FACE_OUTER_BOUND('',#6746,.T.);
#4781=FACE_OUTER_BOUND('',#6747,.T.);
#4782=FACE_OUTER_BOUND('',#6748,.T.);
#4783=FACE_OUTER_BOUND('',#6749,.T.);
#4784=FACE_OUTER_BOUND('',#6750,.T.);
#4785=FACE_OUTER_BOUND('',#6751,.T.);
#4786=FACE_OUTER_BOUND('',#6752,.T.);
#4787=FACE_OUTER_BOUND('',#6753,.T.);
#4788=FACE_OUTER_BOUND('',#6754,.T.);
#4789=FACE_OUTER_BOUND('',#6755,.T.);
#4790=FACE_OUTER_BOUND('',#6756,.T.);
#4791=FACE_OUTER_BOUND('',#6757,.T.);
#4792=FACE_OUTER_BOUND('',#6758,.T.);
#4793=FACE_OUTER_BOUND('',#6759,.T.);
#4794=FACE_OUTER_BOUND('',#6760,.T.);
#4795=FACE_OUTER_BOUND('',#6761,.T.);
#4796=FACE_OUTER_BOUND('',#6762,.T.);
#4797=FACE_OUTER_BOUND('',#6763,.T.);
#4798=FACE_OUTER_BOUND('',#6764,.T.);
#4799=FACE_OUTER_BOUND('',#6765,.T.);
#4800=FACE_OUTER_BOUND('',#6766,.T.);
#4801=FACE_OUTER_BOUND('',#6767,.T.);
#4802=FACE_OUTER_BOUND('',#6768,.T.);
#4803=FACE_OUTER_BOUND('',#6769,.T.);
#4804=FACE_OUTER_BOUND('',#6770,.T.);
#4805=FACE_OUTER_BOUND('',#6771,.T.);
#4806=FACE_OUTER_BOUND('',#6772,.T.);
#4807=FACE_OUTER_BOUND('',#6773,.T.);
#4808=FACE_OUTER_BOUND('',#6774,.T.);
#4809=FACE_OUTER_BOUND('',#6775,.T.);
#4810=FACE_OUTER_BOUND('',#6776,.T.);
#4811=FACE_OUTER_BOUND('',#6777,.T.);
#4812=FACE_OUTER_BOUND('',#6778,.T.);
#4813=FACE_OUTER_BOUND('',#6779,.T.);
#4814=FACE_OUTER_BOUND('',#6780,.T.);
#4815=FACE_OUTER_BOUND('',#6781,.T.);
#4816=FACE_OUTER_BOUND('',#6782,.T.);
#4817=FACE_OUTER_BOUND('',#6783,.T.);
#4818=FACE_OUTER_BOUND('',#6784,.T.);
#4819=FACE_OUTER_BOUND('',#6785,.T.);
#4820=FACE_OUTER_BOUND('',#6786,.T.);
#4821=FACE_OUTER_BOUND('',#6787,.T.);
#4822=FACE_OUTER_BOUND('',#6788,.T.);
#4823=FACE_OUTER_BOUND('',#6789,.T.);
#4824=FACE_OUTER_BOUND('',#6790,.T.);
#4825=FACE_OUTER_BOUND('',#6791,.T.);
#4826=FACE_OUTER_BOUND('',#6792,.T.);
#4827=FACE_OUTER_BOUND('',#6793,.T.);
#4828=FACE_OUTER_BOUND('',#6794,.T.);
#4829=FACE_OUTER_BOUND('',#6795,.T.);
#4830=FACE_OUTER_BOUND('',#6796,.T.);
#4831=FACE_OUTER_BOUND('',#6797,.T.);
#4832=FACE_OUTER_BOUND('',#6798,.T.);
#4833=FACE_OUTER_BOUND('',#6799,.T.);
#4834=FACE_OUTER_BOUND('',#6800,.T.);
#4835=FACE_OUTER_BOUND('',#6801,.T.);
#4836=FACE_OUTER_BOUND('',#6802,.T.);
#4837=FACE_OUTER_BOUND('',#6803,.T.);
#4838=FACE_OUTER_BOUND('',#6804,.T.);
#4839=FACE_OUTER_BOUND('',#6805,.T.);
#4840=FACE_OUTER_BOUND('',#6806,.T.);
#4841=FACE_OUTER_BOUND('',#6807,.T.);
#4842=FACE_OUTER_BOUND('',#6808,.T.);
#4843=FACE_OUTER_BOUND('',#6809,.T.);
#4844=FACE_OUTER_BOUND('',#6810,.T.);
#4845=FACE_OUTER_BOUND('',#6811,.T.);
#4846=FACE_OUTER_BOUND('',#6812,.T.);
#4847=FACE_OUTER_BOUND('',#6813,.T.);
#4848=FACE_OUTER_BOUND('',#6814,.T.);
#4849=FACE_OUTER_BOUND('',#6815,.T.);
#4850=FACE_OUTER_BOUND('',#6817,.T.);
#4851=FACE_OUTER_BOUND('',#6818,.T.);
#4852=FACE_OUTER_BOUND('',#6819,.T.);
#4853=FACE_OUTER_BOUND('',#6820,.T.);
#4854=FACE_OUTER_BOUND('',#6821,.T.);
#4855=FACE_OUTER_BOUND('',#6822,.T.);
#4856=FACE_OUTER_BOUND('',#6823,.T.);
#4857=FACE_OUTER_BOUND('',#6824,.T.);
#4858=FACE_OUTER_BOUND('',#6825,.T.);
#4859=FACE_OUTER_BOUND('',#6826,.T.);
#4860=FACE_OUTER_BOUND('',#6827,.T.);
#4861=FACE_OUTER_BOUND('',#6828,.T.);
#4862=FACE_OUTER_BOUND('',#6829,.T.);
#4863=FACE_OUTER_BOUND('',#6830,.T.);
#4864=FACE_OUTER_BOUND('',#6831,.T.);
#4865=FACE_OUTER_BOUND('',#6832,.T.);
#4866=FACE_OUTER_BOUND('',#6833,.T.);
#4867=FACE_OUTER_BOUND('',#6834,.T.);
#4868=FACE_OUTER_BOUND('',#6835,.T.);
#4869=FACE_OUTER_BOUND('',#6836,.T.);
#4870=FACE_OUTER_BOUND('',#6837,.T.);
#4871=FACE_OUTER_BOUND('',#6838,.T.);
#4872=FACE_OUTER_BOUND('',#6839,.T.);
#4873=FACE_OUTER_BOUND('',#6840,.T.);
#4874=FACE_OUTER_BOUND('',#6841,.T.);
#4875=FACE_OUTER_BOUND('',#6842,.T.);
#4876=FACE_OUTER_BOUND('',#6843,.T.);
#4877=FACE_OUTER_BOUND('',#6844,.T.);
#4878=FACE_OUTER_BOUND('',#6845,.T.);
#4879=FACE_OUTER_BOUND('',#6846,.T.);
#4880=FACE_OUTER_BOUND('',#6847,.T.);
#4881=FACE_OUTER_BOUND('',#6848,.T.);
#4882=FACE_OUTER_BOUND('',#6849,.T.);
#4883=FACE_OUTER_BOUND('',#6850,.T.);
#4884=FACE_OUTER_BOUND('',#6851,.T.);
#4885=FACE_OUTER_BOUND('',#6852,.T.);
#4886=FACE_OUTER_BOUND('',#6853,.T.);
#4887=FACE_OUTER_BOUND('',#6854,.T.);
#4888=FACE_OUTER_BOUND('',#6855,.T.);
#4889=FACE_OUTER_BOUND('',#6856,.T.);
#4890=FACE_OUTER_BOUND('',#6857,.T.);
#4891=FACE_OUTER_BOUND('',#6858,.T.);
#4892=FACE_OUTER_BOUND('',#6859,.T.);
#4893=FACE_OUTER_BOUND('',#6860,.T.);
#4894=FACE_OUTER_BOUND('',#6861,.T.);
#4895=FACE_OUTER_BOUND('',#6862,.T.);
#4896=FACE_OUTER_BOUND('',#6863,.T.);
#4897=FACE_OUTER_BOUND('',#6864,.T.);
#4898=FACE_OUTER_BOUND('',#6865,.T.);
#4899=FACE_OUTER_BOUND('',#6866,.T.);
#4900=FACE_OUTER_BOUND('',#6867,.T.);
#4901=FACE_OUTER_BOUND('',#6868,.T.);
#4902=FACE_OUTER_BOUND('',#6869,.T.);
#4903=FACE_OUTER_BOUND('',#6870,.T.);
#4904=FACE_OUTER_BOUND('',#6871,.T.);
#4905=FACE_OUTER_BOUND('',#6872,.T.);
#4906=FACE_OUTER_BOUND('',#6873,.T.);
#4907=FACE_OUTER_BOUND('',#6874,.T.);
#4908=FACE_OUTER_BOUND('',#6875,.T.);
#4909=FACE_OUTER_BOUND('',#6876,.T.);
#4910=FACE_OUTER_BOUND('',#6877,.T.);
#4911=FACE_OUTER_BOUND('',#6878,.T.);
#4912=FACE_OUTER_BOUND('',#6879,.T.);
#4913=FACE_OUTER_BOUND('',#6880,.T.);
#4914=FACE_OUTER_BOUND('',#6881,.T.);
#4915=FACE_OUTER_BOUND('',#6882,.T.);
#4916=FACE_OUTER_BOUND('',#6883,.T.);
#4917=FACE_OUTER_BOUND('',#6884,.T.);
#4918=FACE_OUTER_BOUND('',#6885,.T.);
#4919=FACE_OUTER_BOUND('',#6886,.T.);
#4920=FACE_OUTER_BOUND('',#6887,.T.);
#4921=FACE_OUTER_BOUND('',#6888,.T.);
#4922=FACE_OUTER_BOUND('',#6890,.T.);
#4923=FACE_OUTER_BOUND('',#6891,.T.);
#4924=FACE_OUTER_BOUND('',#6892,.T.);
#4925=FACE_OUTER_BOUND('',#6893,.T.);
#4926=FACE_OUTER_BOUND('',#6894,.T.);
#4927=FACE_OUTER_BOUND('',#6895,.T.);
#4928=FACE_OUTER_BOUND('',#6896,.T.);
#4929=FACE_OUTER_BOUND('',#6897,.T.);
#4930=FACE_OUTER_BOUND('',#6898,.T.);
#4931=FACE_OUTER_BOUND('',#6899,.T.);
#4932=FACE_OUTER_BOUND('',#6900,.T.);
#4933=FACE_OUTER_BOUND('',#6901,.T.);
#4934=FACE_OUTER_BOUND('',#6902,.T.);
#4935=FACE_OUTER_BOUND('',#6903,.T.);
#4936=FACE_OUTER_BOUND('',#6904,.T.);
#4937=FACE_OUTER_BOUND('',#6905,.T.);
#4938=FACE_OUTER_BOUND('',#6906,.T.);
#4939=FACE_OUTER_BOUND('',#6907,.T.);
#4940=FACE_OUTER_BOUND('',#6908,.T.);
#4941=FACE_OUTER_BOUND('',#6909,.T.);
#4942=FACE_OUTER_BOUND('',#6910,.T.);
#4943=FACE_OUTER_BOUND('',#6911,.T.);
#4944=FACE_OUTER_BOUND('',#6912,.T.);
#4945=FACE_OUTER_BOUND('',#6913,.T.);
#4946=FACE_OUTER_BOUND('',#6914,.T.);
#4947=FACE_OUTER_BOUND('',#6915,.T.);
#4948=FACE_OUTER_BOUND('',#6916,.T.);
#4949=FACE_OUTER_BOUND('',#6917,.T.);
#4950=FACE_OUTER_BOUND('',#6918,.T.);
#4951=FACE_OUTER_BOUND('',#6919,.T.);
#4952=FACE_OUTER_BOUND('',#6920,.T.);
#4953=FACE_OUTER_BOUND('',#6921,.T.);
#4954=FACE_OUTER_BOUND('',#6922,.T.);
#4955=FACE_OUTER_BOUND('',#6923,.T.);
#4956=FACE_OUTER_BOUND('',#6924,.T.);
#4957=FACE_OUTER_BOUND('',#6925,.T.);
#4958=FACE_OUTER_BOUND('',#6926,.T.);
#4959=FACE_OUTER_BOUND('',#6927,.T.);
#4960=FACE_OUTER_BOUND('',#6928,.T.);
#4961=FACE_OUTER_BOUND('',#6929,.T.);
#4962=FACE_OUTER_BOUND('',#6930,.T.);
#4963=FACE_OUTER_BOUND('',#6931,.T.);
#4964=FACE_OUTER_BOUND('',#6932,.T.);
#4965=FACE_OUTER_BOUND('',#6933,.T.);
#4966=FACE_OUTER_BOUND('',#6934,.T.);
#4967=FACE_OUTER_BOUND('',#6935,.T.);
#4968=FACE_OUTER_BOUND('',#6936,.T.);
#4969=FACE_OUTER_BOUND('',#6937,.T.);
#4970=FACE_OUTER_BOUND('',#6938,.T.);
#4971=FACE_OUTER_BOUND('',#6939,.T.);
#4972=FACE_OUTER_BOUND('',#6940,.T.);
#4973=FACE_OUTER_BOUND('',#6941,.T.);
#4974=FACE_OUTER_BOUND('',#6942,.T.);
#4975=FACE_OUTER_BOUND('',#6943,.T.);
#4976=FACE_OUTER_BOUND('',#6944,.T.);
#4977=FACE_OUTER_BOUND('',#6945,.T.);
#4978=FACE_OUTER_BOUND('',#6946,.T.);
#4979=FACE_OUTER_BOUND('',#6947,.T.);
#4980=FACE_OUTER_BOUND('',#6948,.T.);
#4981=FACE_OUTER_BOUND('',#6949,.T.);
#4982=FACE_OUTER_BOUND('',#6950,.T.);
#4983=FACE_OUTER_BOUND('',#6951,.T.);
#4984=FACE_OUTER_BOUND('',#6952,.T.);
#4985=FACE_OUTER_BOUND('',#6953,.T.);
#4986=FACE_OUTER_BOUND('',#6954,.T.);
#4987=FACE_OUTER_BOUND('',#6955,.T.);
#4988=FACE_OUTER_BOUND('',#6956,.T.);
#4989=FACE_OUTER_BOUND('',#6957,.T.);
#4990=FACE_OUTER_BOUND('',#6958,.T.);
#4991=FACE_OUTER_BOUND('',#6959,.T.);
#4992=FACE_OUTER_BOUND('',#6960,.T.);
#4993=FACE_OUTER_BOUND('',#6961,.T.);
#4994=FACE_OUTER_BOUND('',#6962,.T.);
#4995=FACE_OUTER_BOUND('',#6963,.T.);
#4996=FACE_OUTER_BOUND('',#6964,.T.);
#4997=FACE_OUTER_BOUND('',#6965,.T.);
#4998=FACE_OUTER_BOUND('',#6966,.T.);
#4999=FACE_OUTER_BOUND('',#6967,.T.);
#5000=FACE_OUTER_BOUND('',#6968,.T.);
#5001=FACE_OUTER_BOUND('',#6969,.T.);
#5002=FACE_OUTER_BOUND('',#6970,.T.);
#5003=FACE_OUTER_BOUND('',#6971,.T.);
#5004=FACE_OUTER_BOUND('',#6972,.T.);
#5005=FACE_OUTER_BOUND('',#6973,.T.);
#5006=FACE_OUTER_BOUND('',#6974,.T.);
#5007=FACE_OUTER_BOUND('',#6975,.T.);
#5008=FACE_OUTER_BOUND('',#6976,.T.);
#5009=FACE_OUTER_BOUND('',#6977,.T.);
#5010=FACE_OUTER_BOUND('',#6978,.T.);
#5011=FACE_OUTER_BOUND('',#6979,.T.);
#5012=FACE_OUTER_BOUND('',#6980,.T.);
#5013=FACE_OUTER_BOUND('',#6981,.T.);
#5014=FACE_OUTER_BOUND('',#6982,.T.);
#5015=FACE_OUTER_BOUND('',#6983,.T.);
#5016=FACE_OUTER_BOUND('',#6984,.T.);
#5017=FACE_OUTER_BOUND('',#6985,.T.);
#5018=FACE_OUTER_BOUND('',#6986,.T.);
#5019=FACE_OUTER_BOUND('',#6987,.T.);
#5020=FACE_OUTER_BOUND('',#6988,.T.);
#5021=FACE_OUTER_BOUND('',#6989,.T.);
#5022=FACE_OUTER_BOUND('',#6990,.T.);
#5023=FACE_OUTER_BOUND('',#6991,.T.);
#5024=FACE_OUTER_BOUND('',#6992,.T.);
#5025=FACE_OUTER_BOUND('',#6993,.T.);
#5026=FACE_OUTER_BOUND('',#6994,.T.);
#5027=FACE_OUTER_BOUND('',#6995,.T.);
#5028=FACE_OUTER_BOUND('',#6996,.T.);
#5029=FACE_OUTER_BOUND('',#6997,.T.);
#5030=FACE_OUTER_BOUND('',#6998,.T.);
#5031=FACE_OUTER_BOUND('',#6999,.T.);
#5032=FACE_OUTER_BOUND('',#7000,.T.);
#5033=FACE_OUTER_BOUND('',#7001,.T.);
#5034=FACE_OUTER_BOUND('',#7002,.T.);
#5035=FACE_OUTER_BOUND('',#7003,.T.);
#5036=FACE_OUTER_BOUND('',#7005,.T.);
#5037=FACE_OUTER_BOUND('',#7006,.T.);
#5038=FACE_OUTER_BOUND('',#7007,.T.);
#5039=FACE_OUTER_BOUND('',#7008,.T.);
#5040=FACE_OUTER_BOUND('',#7009,.T.);
#5041=FACE_OUTER_BOUND('',#7010,.T.);
#5042=FACE_OUTER_BOUND('',#7011,.T.);
#5043=FACE_OUTER_BOUND('',#7012,.T.);
#5044=FACE_OUTER_BOUND('',#7013,.T.);
#5045=FACE_OUTER_BOUND('',#7014,.T.);
#5046=FACE_OUTER_BOUND('',#7015,.T.);
#5047=FACE_OUTER_BOUND('',#7016,.T.);
#5048=FACE_OUTER_BOUND('',#7017,.T.);
#5049=FACE_OUTER_BOUND('',#7018,.T.);
#5050=FACE_OUTER_BOUND('',#7019,.T.);
#5051=FACE_OUTER_BOUND('',#7020,.T.);
#5052=FACE_OUTER_BOUND('',#7021,.T.);
#5053=FACE_OUTER_BOUND('',#7022,.T.);
#5054=FACE_OUTER_BOUND('',#7023,.T.);
#5055=FACE_OUTER_BOUND('',#7024,.T.);
#5056=FACE_OUTER_BOUND('',#7025,.T.);
#5057=FACE_OUTER_BOUND('',#7026,.T.);
#5058=FACE_OUTER_BOUND('',#7027,.T.);
#5059=FACE_OUTER_BOUND('',#7028,.T.);
#5060=FACE_OUTER_BOUND('',#7029,.T.);
#5061=FACE_OUTER_BOUND('',#7030,.T.);
#5062=FACE_OUTER_BOUND('',#7031,.T.);
#5063=FACE_OUTER_BOUND('',#7032,.T.);
#5064=FACE_OUTER_BOUND('',#7033,.T.);
#5065=FACE_OUTER_BOUND('',#7034,.T.);
#5066=FACE_OUTER_BOUND('',#7035,.T.);
#5067=FACE_OUTER_BOUND('',#7036,.T.);
#5068=FACE_OUTER_BOUND('',#7037,.T.);
#5069=FACE_OUTER_BOUND('',#7038,.T.);
#5070=FACE_OUTER_BOUND('',#7039,.T.);
#5071=FACE_OUTER_BOUND('',#7040,.T.);
#5072=FACE_OUTER_BOUND('',#7041,.T.);
#5073=FACE_OUTER_BOUND('',#7042,.T.);
#5074=FACE_OUTER_BOUND('',#7043,.T.);
#5075=FACE_OUTER_BOUND('',#7044,.T.);
#5076=FACE_OUTER_BOUND('',#7045,.T.);
#5077=FACE_OUTER_BOUND('',#7046,.T.);
#5078=FACE_OUTER_BOUND('',#7047,.T.);
#5079=FACE_OUTER_BOUND('',#7048,.T.);
#5080=FACE_OUTER_BOUND('',#7049,.T.);
#5081=FACE_OUTER_BOUND('',#7050,.T.);
#5082=FACE_OUTER_BOUND('',#7051,.T.);
#5083=FACE_OUTER_BOUND('',#7052,.T.);
#5084=FACE_OUTER_BOUND('',#7053,.T.);
#5085=FACE_OUTER_BOUND('',#7054,.T.);
#5086=FACE_OUTER_BOUND('',#7055,.T.);
#5087=FACE_OUTER_BOUND('',#7056,.T.);
#5088=FACE_OUTER_BOUND('',#7057,.T.);
#5089=FACE_OUTER_BOUND('',#7058,.T.);
#5090=FACE_OUTER_BOUND('',#7060,.T.);
#5091=FACE_OUTER_BOUND('',#7061,.T.);
#5092=FACE_OUTER_BOUND('',#7062,.T.);
#5093=FACE_OUTER_BOUND('',#7063,.T.);
#5094=FACE_OUTER_BOUND('',#7064,.T.);
#5095=FACE_OUTER_BOUND('',#7065,.T.);
#5096=FACE_OUTER_BOUND('',#7066,.T.);
#5097=FACE_OUTER_BOUND('',#7067,.T.);
#5098=FACE_OUTER_BOUND('',#7068,.T.);
#5099=FACE_OUTER_BOUND('',#7069,.T.);
#5100=EDGE_LOOP('',(#20976,#20977,#20978,#20979));
#5101=EDGE_LOOP('',(#20980,#20981,#20982,#20983,#20984,#20985,#20986,#20987,
#20988,#20989,#20990,#20991,#20992,#20993,#20994,#20995));
#5102=EDGE_LOOP('',(#20996));
#5103=EDGE_LOOP('',(#20997));
#5104=EDGE_LOOP('',(#20998,#20999,#21000,#21001));
#5105=EDGE_LOOP('',(#21002,#21003,#21004,#21005));
#5106=EDGE_LOOP('',(#21006,#21007,#21008,#21009));
#5107=EDGE_LOOP('',(#21010,#21011,#21012));
#5108=EDGE_LOOP('',(#21013,#21014,#21015));
#5109=EDGE_LOOP('',(#21016,#21017,#21018,#21019));
#5110=EDGE_LOOP('',(#21020,#21021,#21022,#21023,#21024,#21025,#21026,#21027,
#21028,#21029,#21030,#21031,#21032,#21033,#21034,#21035));
#5111=EDGE_LOOP('',(#21036));
#5112=EDGE_LOOP('',(#21037));
#5113=EDGE_LOOP('',(#21038,#21039,#21040,#21041));
#5114=EDGE_LOOP('',(#21042,#21043,#21044,#21045));
#5115=EDGE_LOOP('',(#21046,#21047,#21048,#21049));
#5116=EDGE_LOOP('',(#21050,#21051,#21052));
#5117=EDGE_LOOP('',(#21053,#21054,#21055));
#5118=EDGE_LOOP('',(#21056,#21057,#21058,#21059));
#5119=EDGE_LOOP('',(#21060,#21061,#21062,#21063));
#5120=EDGE_LOOP('',(#21064,#21065,#21066,#21067));
#5121=EDGE_LOOP('',(#21068,#21069,#21070,#21071));
#5122=EDGE_LOOP('',(#21072,#21073,#21074,#21075));
#5123=EDGE_LOOP('',(#21076,#21077,#21078,#21079));
#5124=EDGE_LOOP('',(#21080,#21081,#21082,#21083));
#5125=EDGE_LOOP('',(#21084,#21085,#21086,#21087));
#5126=EDGE_LOOP('',(#21088,#21089,#21090,#21091));
#5127=EDGE_LOOP('',(#21092,#21093,#21094,#21095));
#5128=EDGE_LOOP('',(#21096,#21097,#21098,#21099));
#5129=EDGE_LOOP('',(#21100,#21101,#21102,#21103));
#5130=EDGE_LOOP('',(#21104,#21105,#21106,#21107));
#5131=EDGE_LOOP('',(#21108,#21109,#21110,#21111));
#5132=EDGE_LOOP('',(#21112,#21113,#21114,#21115));
#5133=EDGE_LOOP('',(#21116,#21117,#21118,#21119));
#5134=EDGE_LOOP('',(#21120,#21121,#21122,#21123));
#5135=EDGE_LOOP('',(#21124,#21125,#21126,#21127));
#5136=EDGE_LOOP('',(#21128));
#5137=EDGE_LOOP('',(#21129));
#5138=EDGE_LOOP('',(#21130,#21131,#21132,#21133,#21134));
#5139=EDGE_LOOP('',(#21135,#21136,#21137,#21138));
#5140=EDGE_LOOP('',(#21139,#21140,#21141,#21142,#21143));
#5141=EDGE_LOOP('',(#21144,#21145,#21146,#21147));
#5142=EDGE_LOOP('',(#21148,#21149,#21150,#21151));
#5143=EDGE_LOOP('',(#21152,#21153,#21154,#21155));
#5144=EDGE_LOOP('',(#21156,#21157,#21158,#21159));
#5145=EDGE_LOOP('',(#21160));
#5146=EDGE_LOOP('',(#21161));
#5147=EDGE_LOOP('',(#21162));
#5148=EDGE_LOOP('',(#21163));
#5149=EDGE_LOOP('',(#21164));
#5150=EDGE_LOOP('',(#21165));
#5151=EDGE_LOOP('',(#21166));
#5152=EDGE_LOOP('',(#21167));
#5153=EDGE_LOOP('',(#21168));
#5154=EDGE_LOOP('',(#21169));
#5155=EDGE_LOOP('',(#21170,#21171,#21172,#21173));
#5156=EDGE_LOOP('',(#21174,#21175,#21176,#21177));
#5157=EDGE_LOOP('',(#21178,#21179,#21180,#21181));
#5158=EDGE_LOOP('',(#21182,#21183,#21184,#21185));
#5159=EDGE_LOOP('',(#21186,#21187,#21188,#21189));
#5160=EDGE_LOOP('',(#21190,#21191,#21192,#21193));
#5161=EDGE_LOOP('',(#21194,#21195,#21196,#21197));
#5162=EDGE_LOOP('',(#21198,#21199,#21200));
#5163=EDGE_LOOP('',(#21201,#21202,#21203));
#5164=EDGE_LOOP('',(#21204,#21205,#21206));
#5165=EDGE_LOOP('',(#21207,#21208,#21209));
#5166=EDGE_LOOP('',(#21210,#21211,#21212,#21213));
#5167=EDGE_LOOP('',(#21214,#21215,#21216,#21217));
#5168=EDGE_LOOP('',(#21218,#21219,#21220,#21221));
#5169=EDGE_LOOP('',(#21222,#21223,#21224,#21225));
#5170=EDGE_LOOP('',(#21226,#21227,#21228,#21229));
#5171=EDGE_LOOP('',(#21230,#21231,#21232,#21233));
#5172=EDGE_LOOP('',(#21234,#21235,#21236,#21237));
#5173=EDGE_LOOP('',(#21238,#21239,#21240,#21241));
#5174=EDGE_LOOP('',(#21242,#21243,#21244,#21245));
#5175=EDGE_LOOP('',(#21246,#21247,#21248,#21249));
#5176=EDGE_LOOP('',(#21250,#21251,#21252,#21253));
#5177=EDGE_LOOP('',(#21254,#21255,#21256,#21257));
#5178=EDGE_LOOP('',(#21258,#21259,#21260));
#5179=EDGE_LOOP('',(#21261,#21262,#21263));
#5180=EDGE_LOOP('',(#21264,#21265,#21266));
#5181=EDGE_LOOP('',(#21267,#21268,#21269));
#5182=EDGE_LOOP('',(#21270,#21271,#21272));
#5183=EDGE_LOOP('',(#21273,#21274,#21275));
#5184=EDGE_LOOP('',(#21276,#21277,#21278,#21279));
#5185=EDGE_LOOP('',(#21280,#21281,#21282,#21283,#21284,#21285));
#5186=EDGE_LOOP('',(#21286,#21287,#21288,#21289,#21290,#21291,#21292,#21293,
#21294,#21295));
#5187=EDGE_LOOP('',(#21296,#21297,#21298,#21299));
#5188=EDGE_LOOP('',(#21300,#21301,#21302,#21303));
#5189=EDGE_LOOP('',(#21304,#21305,#21306,#21307));
#5190=EDGE_LOOP('',(#21308,#21309,#21310,#21311,#21312,#21313,#21314,#21315));
#5191=EDGE_LOOP('',(#21316,#21317,#21318,#21319));
#5192=EDGE_LOOP('',(#21320,#21321,#21322,#21323));
#5193=EDGE_LOOP('',(#21324,#21325,#21326,#21327));
#5194=EDGE_LOOP('',(#21328,#21329,#21330,#21331));
#5195=EDGE_LOOP('',(#21332,#21333,#21334,#21335,#21336,#21337));
#5196=EDGE_LOOP('',(#21338,#21339,#21340,#21341,#21342,#21343,#21344,#21345,
#21346));
#5197=EDGE_LOOP('',(#21347,#21348,#21349,#21350));
#5198=EDGE_LOOP('',(#21351,#21352,#21353,#21354));
#5199=EDGE_LOOP('',(#21355,#21356,#21357,#21358));
#5200=EDGE_LOOP('',(#21359,#21360,#21361,#21362));
#5201=EDGE_LOOP('',(#21363,#21364,#21365,#21366));
#5202=EDGE_LOOP('',(#21367,#21368,#21369,#21370,#21371,#21372,#21373,#21374,
#21375));
#5203=EDGE_LOOP('',(#21376,#21377,#21378,#21379));
#5204=EDGE_LOOP('',(#21380,#21381,#21382,#21383,#21384,#21385,#21386,#21387,
#21388,#21389));
#5205=EDGE_LOOP('',(#21390,#21391,#21392,#21393,#21394));
#5206=EDGE_LOOP('',(#21395,#21396,#21397,#21398,#21399,#21400));
#5207=EDGE_LOOP('',(#21401));
#5208=EDGE_LOOP('',(#21402));
#5209=EDGE_LOOP('',(#21403,#21404,#21405,#21406,#21407));
#5210=EDGE_LOOP('',(#21408));
#5211=EDGE_LOOP('',(#21409));
#5212=EDGE_LOOP('',(#21410,#21411,#21412,#21413));
#5213=EDGE_LOOP('',(#21414,#21415,#21416,#21417));
#5214=EDGE_LOOP('',(#21418,#21419,#21420,#21421));
#5215=EDGE_LOOP('',(#21422,#21423,#21424,#21425,#21426,#21427,#21428,#21429,
#21430,#21431));
#5216=EDGE_LOOP('',(#21432,#21433,#21434,#21435,#21436));
#5217=EDGE_LOOP('',(#21437,#21438,#21439,#21440));
#5218=EDGE_LOOP('',(#21441,#21442,#21443,#21444,#21445,#21446));
#5219=EDGE_LOOP('',(#21447,#21448,#21449,#21450,#21451));
#5220=EDGE_LOOP('',(#21452,#21453,#21454,#21455,#21456));
#5221=EDGE_LOOP('',(#21457,#21458,#21459,#21460,#21461,#21462));
#5222=EDGE_LOOP('',(#21463,#21464,#21465,#21466,#21467));
#5223=EDGE_LOOP('',(#21468,#21469,#21470,#21471,#21472,#21473));
#5224=EDGE_LOOP('',(#21474,#21475,#21476,#21477,#21478,#21479));
#5225=EDGE_LOOP('',(#21480,#21481,#21482,#21483,#21484));
#5226=EDGE_LOOP('',(#21485,#21486,#21487,#21488,#21489,#21490,#21491));
#5227=EDGE_LOOP('',(#21492,#21493,#21494,#21495,#21496));
#5228=EDGE_LOOP('',(#21497,#21498,#21499,#21500,#21501));
#5229=EDGE_LOOP('',(#21502,#21503,#21504,#21505,#21506,#21507));
#5230=EDGE_LOOP('',(#21508,#21509,#21510,#21511));
#5231=EDGE_LOOP('',(#21512,#21513,#21514,#21515,#21516,#21517));
#5232=EDGE_LOOP('',(#21518,#21519,#21520,#21521,#21522));
#5233=EDGE_LOOP('',(#21523,#21524,#21525,#21526));
#5234=EDGE_LOOP('',(#21527,#21528,#21529,#21530,#21531,#21532));
#5235=EDGE_LOOP('',(#21533,#21534,#21535,#21536,#21537));
#5236=EDGE_LOOP('',(#21538,#21539,#21540,#21541,#21542,#21543,#21544));
#5237=EDGE_LOOP('',(#21545,#21546,#21547,#21548,#21549,#21550));
#5238=EDGE_LOOP('',(#21551,#21552,#21553,#21554));
#5239=EDGE_LOOP('',(#21555,#21556,#21557,#21558,#21559,#21560,#21561));
#5240=EDGE_LOOP('',(#21562,#21563,#21564,#21565,#21566));
#5241=EDGE_LOOP('',(#21567,#21568,#21569,#21570));
#5242=EDGE_LOOP('',(#21571,#21572,#21573,#21574,#21575,#21576));
#5243=EDGE_LOOP('',(#21577,#21578,#21579,#21580));
#5244=EDGE_LOOP('',(#21581,#21582,#21583,#21584,#21585));
#5245=EDGE_LOOP('',(#21586,#21587,#21588,#21589,#21590,#21591));
#5246=EDGE_LOOP('',(#21592,#21593,#21594,#21595,#21596));
#5247=EDGE_LOOP('',(#21597,#21598,#21599,#21600,#21601));
#5248=EDGE_LOOP('',(#21602,#21603,#21604,#21605,#21606,#21607,#21608));
#5249=EDGE_LOOP('',(#21609,#21610,#21611,#21612,#21613));
#5250=EDGE_LOOP('',(#21614,#21615,#21616,#21617,#21618,#21619));
#5251=EDGE_LOOP('',(#21620,#21621,#21622,#21623));
#5252=EDGE_LOOP('',(#21624,#21625,#21626,#21627,#21628,#21629));
#5253=EDGE_LOOP('',(#21630,#21631,#21632,#21633,#21634));
#5254=EDGE_LOOP('',(#21635,#21636,#21637,#21638,#21639,#21640));
#5255=EDGE_LOOP('',(#21641,#21642,#21643,#21644,#21645));
#5256=EDGE_LOOP('',(#21646,#21647,#21648,#21649,#21650,#21651,#21652,#21653,
#21654));
#5257=EDGE_LOOP('',(#21655,#21656,#21657,#21658,#21659));
#5258=EDGE_LOOP('',(#21660,#21661,#21662,#21663,#21664,#21665));
#5259=EDGE_LOOP('',(#21666,#21667,#21668,#21669));
#5260=EDGE_LOOP('',(#21670,#21671,#21672,#21673,#21674));
#5261=EDGE_LOOP('',(#21675,#21676,#21677,#21678,#21679,#21680,#21681,#21682,
#21683));
#5262=EDGE_LOOP('',(#21684,#21685,#21686,#21687,#21688,#21689,#21690,#21691));
#5263=EDGE_LOOP('',(#21692,#21693));
#5264=EDGE_LOOP('',(#21694,#21695));
#5265=EDGE_LOOP('',(#21696,#21697,#21698,#21699));
#5266=EDGE_LOOP('',(#21700,#21701,#21702,#21703));
#5267=EDGE_LOOP('',(#21704,#21705,#21706,#21707,#21708));
#5268=EDGE_LOOP('',(#21709,#21710,#21711,#21712,#21713));
#5269=EDGE_LOOP('',(#21714,#21715,#21716,#21717,#21718,#21719,#21720,#21721,
#21722));
#5270=EDGE_LOOP('',(#21723,#21724,#21725,#21726,#21727,#21728));
#5271=EDGE_LOOP('',(#21729,#21730,#21731,#21732,#21733,#21734));
#5272=EDGE_LOOP('',(#21735,#21736,#21737,#21738,#21739,#21740));
#5273=EDGE_LOOP('',(#21741,#21742,#21743,#21744,#21745,#21746,#21747));
#5274=EDGE_LOOP('',(#21748,#21749,#21750,#21751));
#5275=EDGE_LOOP('',(#21752,#21753,#21754,#21755,#21756,#21757,#21758,#21759,
#21760,#21761));
#5276=EDGE_LOOP('',(#21762,#21763,#21764,#21765,#21766,#21767,#21768,#21769,
#21770,#21771));
#5277=EDGE_LOOP('',(#21772,#21773,#21774,#21775,#21776,#21777,#21778,#21779,
#21780));
#5278=EDGE_LOOP('',(#21781,#21782,#21783,#21784,#21785,#21786,#21787,#21788));
#5279=EDGE_LOOP('',(#21789,#21790,#21791,#21792,#21793,#21794,#21795,#21796,
#21797,#21798));
#5280=EDGE_LOOP('',(#21799,#21800,#21801,#21802,#21803,#21804,#21805,#21806,
#21807,#21808,#21809));
#5281=EDGE_LOOP('',(#21810,#21811,#21812,#21813,#21814,#21815,#21816,#21817,
#21818,#21819));
#5282=EDGE_LOOP('',(#21820,#21821,#21822,#21823,#21824,#21825,#21826,#21827,
#21828,#21829));
#5283=EDGE_LOOP('',(#21830,#21831,#21832,#21833,#21834,#21835,#21836,#21837,
#21838,#21839,#21840,#21841));
#5284=EDGE_LOOP('',(#21842,#21843,#21844,#21845,#21846,#21847,#21848,#21849,
#21850,#21851,#21852));
#5285=EDGE_LOOP('',(#21853,#21854,#21855,#21856));
#5286=EDGE_LOOP('',(#21857,#21858,#21859,#21860,#21861,#21862,#21863,#21864,
#21865,#21866,#21867,#21868));
#5287=EDGE_LOOP('',(#21869,#21870,#21871,#21872,#21873,#21874,#21875,#21876));
#5288=EDGE_LOOP('',(#21877,#21878,#21879,#21880,#21881,#21882,#21883,#21884,
#21885));
#5289=EDGE_LOOP('',(#21886,#21887,#21888,#21889,#21890,#21891,#21892,#21893,
#21894));
#5290=EDGE_LOOP('',(#21895,#21896,#21897,#21898,#21899,#21900,#21901,#21902,
#21903));
#5291=EDGE_LOOP('',(#21904,#21905,#21906,#21907,#21908,#21909));
#5292=EDGE_LOOP('',(#21910,#21911,#21912,#21913,#21914,#21915,#21916,#21917,
#21918,#21919));
#5293=EDGE_LOOP('',(#21920,#21921,#21922,#21923,#21924,#21925,#21926,#21927,
#21928,#21929));
#5294=EDGE_LOOP('',(#21930,#21931,#21932,#21933));
#5295=EDGE_LOOP('',(#21934));
#5296=EDGE_LOOP('',(#21935,#21936,#21937,#21938));
#5297=EDGE_LOOP('',(#21939,#21940,#21941,#21942));
#5298=EDGE_LOOP('',(#21943,#21944,#21945,#21946));
#5299=EDGE_LOOP('',(#21947));
#5300=EDGE_LOOP('',(#21948));
#5301=EDGE_LOOP('',(#21949,#21950,#21951,#21952));
#5302=EDGE_LOOP('',(#21953));
#5303=EDGE_LOOP('',(#21954));
#5304=EDGE_LOOP('',(#21955,#21956,#21957,#21958));
#5305=EDGE_LOOP('',(#21959,#21960,#21961,#21962));
#5306=EDGE_LOOP('',(#21963));
#5307=EDGE_LOOP('',(#21964,#21965,#21966,#21967,#21968,#21969,#21970,#21971,
#21972,#21973,#21974,#21975,#21976,#21977,#21978,#21979,#21980,#21981,#21982,
#21983,#21984,#21985,#21986));
#5308=EDGE_LOOP('',(#21987,#21988,#21989,#21990));
#5309=EDGE_LOOP('',(#21991,#21992,#21993,#21994));
#5310=EDGE_LOOP('',(#21995,#21996,#21997,#21998));
#5311=EDGE_LOOP('',(#21999,#22000,#22001,#22002));
#5312=EDGE_LOOP('',(#22003,#22004,#22005,#22006));
#5313=EDGE_LOOP('',(#22007,#22008,#22009,#22010));
#5314=EDGE_LOOP('',(#22011,#22012,#22013,#22014));
#5315=EDGE_LOOP('',(#22015,#22016,#22017,#22018));
#5316=EDGE_LOOP('',(#22019,#22020,#22021,#22022));
#5317=EDGE_LOOP('',(#22023,#22024,#22025,#22026));
#5318=EDGE_LOOP('',(#22027,#22028,#22029));
#5319=EDGE_LOOP('',(#22030,#22031,#22032));
#5320=EDGE_LOOP('',(#22033,#22034,#22035,#22036));
#5321=EDGE_LOOP('',(#22037,#22038,#22039));
#5322=EDGE_LOOP('',(#22040,#22041,#22042,#22043));
#5323=EDGE_LOOP('',(#22044,#22045,#22046));
#5324=EDGE_LOOP('',(#22047,#22048,#22049,#22050));
#5325=EDGE_LOOP('',(#22051,#22052,#22053));
#5326=EDGE_LOOP('',(#22054,#22055,#22056,#22057));
#5327=EDGE_LOOP('',(#22058,#22059,#22060));
#5328=EDGE_LOOP('',(#22061,#22062,#22063,#22064));
#5329=EDGE_LOOP('',(#22065,#22066,#22067));
#5330=EDGE_LOOP('',(#22068,#22069,#22070,#22071));
#5331=EDGE_LOOP('',(#22072,#22073,#22074));
#5332=EDGE_LOOP('',(#22075,#22076,#22077,#22078));
#5333=EDGE_LOOP('',(#22079,#22080,#22081));
#5334=EDGE_LOOP('',(#22082,#22083,#22084,#22085));
#5335=EDGE_LOOP('',(#22086,#22087,#22088));
#5336=EDGE_LOOP('',(#22089,#22090,#22091,#22092));
#5337=EDGE_LOOP('',(#22093,#22094,#22095));
#5338=EDGE_LOOP('',(#22096,#22097,#22098,#22099));
#5339=EDGE_LOOP('',(#22100,#22101,#22102));
#5340=EDGE_LOOP('',(#22103,#22104,#22105,#22106));
#5341=EDGE_LOOP('',(#22107,#22108,#22109));
#5342=EDGE_LOOP('',(#22110,#22111,#22112,#22113));
#5343=EDGE_LOOP('',(#22114,#22115,#22116));
#5344=EDGE_LOOP('',(#22117,#22118,#22119,#22120));
#5345=EDGE_LOOP('',(#22121,#22122,#22123));
#5346=EDGE_LOOP('',(#22124,#22125,#22126,#22127));
#5347=EDGE_LOOP('',(#22128,#22129,#22130));
#5348=EDGE_LOOP('',(#22131,#22132,#22133,#22134));
#5349=EDGE_LOOP('',(#22135,#22136,#22137));
#5350=EDGE_LOOP('',(#22138,#22139,#22140,#22141));
#5351=EDGE_LOOP('',(#22142,#22143,#22144));
#5352=EDGE_LOOP('',(#22145,#22146,#22147,#22148));
#5353=EDGE_LOOP('',(#22149,#22150,#22151));
#5354=EDGE_LOOP('',(#22152,#22153,#22154,#22155));
#5355=EDGE_LOOP('',(#22156,#22157,#22158));
#5356=EDGE_LOOP('',(#22159,#22160,#22161,#22162));
#5357=EDGE_LOOP('',(#22163,#22164,#22165));
#5358=EDGE_LOOP('',(#22166,#22167,#22168,#22169));
#5359=EDGE_LOOP('',(#22170,#22171,#22172));
#5360=EDGE_LOOP('',(#22173,#22174,#22175,#22176));
#5361=EDGE_LOOP('',(#22177,#22178,#22179));
#5362=EDGE_LOOP('',(#22180,#22181,#22182,#22183));
#5363=EDGE_LOOP('',(#22184,#22185,#22186));
#5364=EDGE_LOOP('',(#22187,#22188,#22189,#22190));
#5365=EDGE_LOOP('',(#22191,#22192,#22193));
#5366=EDGE_LOOP('',(#22194,#22195,#22196,#22197));
#5367=EDGE_LOOP('',(#22198,#22199,#22200));
#5368=EDGE_LOOP('',(#22201,#22202,#22203,#22204));
#5369=EDGE_LOOP('',(#22205,#22206,#22207));
#5370=EDGE_LOOP('',(#22208,#22209,#22210,#22211));
#5371=EDGE_LOOP('',(#22212,#22213,#22214));
#5372=EDGE_LOOP('',(#22215,#22216,#22217,#22218));
#5373=EDGE_LOOP('',(#22219,#22220,#22221));
#5374=EDGE_LOOP('',(#22222,#22223,#22224,#22225));
#5375=EDGE_LOOP('',(#22226,#22227,#22228));
#5376=EDGE_LOOP('',(#22229,#22230,#22231,#22232));
#5377=EDGE_LOOP('',(#22233,#22234,#22235));
#5378=EDGE_LOOP('',(#22236,#22237,#22238,#22239));
#5379=EDGE_LOOP('',(#22240,#22241,#22242));
#5380=EDGE_LOOP('',(#22243,#22244,#22245,#22246));
#5381=EDGE_LOOP('',(#22247,#22248,#22249));
#5382=EDGE_LOOP('',(#22250,#22251,#22252,#22253));
#5383=EDGE_LOOP('',(#22254,#22255,#22256));
#5384=EDGE_LOOP('',(#22257,#22258,#22259,#22260));
#5385=EDGE_LOOP('',(#22261,#22262,#22263));
#5386=EDGE_LOOP('',(#22264,#22265,#22266,#22267));
#5387=EDGE_LOOP('',(#22268,#22269,#22270));
#5388=EDGE_LOOP('',(#22271,#22272,#22273,#22274));
#5389=EDGE_LOOP('',(#22275,#22276,#22277));
#5390=EDGE_LOOP('',(#22278,#22279,#22280,#22281));
#5391=EDGE_LOOP('',(#22282,#22283,#22284));
#5392=EDGE_LOOP('',(#22285,#22286,#22287,#22288));
#5393=EDGE_LOOP('',(#22289,#22290,#22291,#22292));
#5394=EDGE_LOOP('',(#22293,#22294,#22295,#22296));
#5395=EDGE_LOOP('',(#22297,#22298,#22299,#22300));
#5396=EDGE_LOOP('',(#22301,#22302,#22303,#22304));
#5397=EDGE_LOOP('',(#22305,#22306,#22307));
#5398=EDGE_LOOP('',(#22308,#22309,#22310,#22311));
#5399=EDGE_LOOP('',(#22312,#22313,#22314));
#5400=EDGE_LOOP('',(#22315,#22316,#22317,#22318));
#5401=EDGE_LOOP('',(#22319,#22320,#22321));
#5402=EDGE_LOOP('',(#22322,#22323,#22324,#22325));
#5403=EDGE_LOOP('',(#22326,#22327,#22328));
#5404=EDGE_LOOP('',(#22329,#22330,#22331,#22332));
#5405=EDGE_LOOP('',(#22333,#22334,#22335));
#5406=EDGE_LOOP('',(#22336,#22337,#22338,#22339));
#5407=EDGE_LOOP('',(#22340,#22341,#22342));
#5408=EDGE_LOOP('',(#22343,#22344,#22345,#22346));
#5409=EDGE_LOOP('',(#22347,#22348,#22349));
#5410=EDGE_LOOP('',(#22350,#22351,#22352,#22353));
#5411=EDGE_LOOP('',(#22354,#22355,#22356));
#5412=EDGE_LOOP('',(#22357,#22358,#22359,#22360));
#5413=EDGE_LOOP('',(#22361,#22362,#22363));
#5414=EDGE_LOOP('',(#22364,#22365,#22366,#22367));
#5415=EDGE_LOOP('',(#22368,#22369,#22370));
#5416=EDGE_LOOP('',(#22371,#22372,#22373,#22374));
#5417=EDGE_LOOP('',(#22375,#22376,#22377));
#5418=EDGE_LOOP('',(#22378,#22379,#22380,#22381));
#5419=EDGE_LOOP('',(#22382,#22383,#22384));
#5420=EDGE_LOOP('',(#22385,#22386,#22387,#22388));
#5421=EDGE_LOOP('',(#22389,#22390,#22391));
#5422=EDGE_LOOP('',(#22392,#22393,#22394,#22395));
#5423=EDGE_LOOP('',(#22396,#22397,#22398));
#5424=EDGE_LOOP('',(#22399,#22400,#22401,#22402));
#5425=EDGE_LOOP('',(#22403,#22404,#22405));
#5426=EDGE_LOOP('',(#22406,#22407,#22408,#22409));
#5427=EDGE_LOOP('',(#22410,#22411,#22412));
#5428=EDGE_LOOP('',(#22413,#22414,#22415,#22416));
#5429=EDGE_LOOP('',(#22417,#22418,#22419));
#5430=EDGE_LOOP('',(#22420,#22421,#22422,#22423));
#5431=EDGE_LOOP('',(#22424,#22425,#22426));
#5432=EDGE_LOOP('',(#22427,#22428,#22429,#22430));
#5433=EDGE_LOOP('',(#22431,#22432,#22433));
#5434=EDGE_LOOP('',(#22434,#22435,#22436,#22437));
#5435=EDGE_LOOP('',(#22438,#22439,#22440));
#5436=EDGE_LOOP('',(#22441,#22442,#22443,#22444));
#5437=EDGE_LOOP('',(#22445,#22446,#22447));
#5438=EDGE_LOOP('',(#22448,#22449,#22450,#22451));
#5439=EDGE_LOOP('',(#22452,#22453,#22454));
#5440=EDGE_LOOP('',(#22455,#22456,#22457,#22458));
#5441=EDGE_LOOP('',(#22459,#22460,#22461));
#5442=EDGE_LOOP('',(#22462,#22463,#22464,#22465));
#5443=EDGE_LOOP('',(#22466,#22467,#22468));
#5444=EDGE_LOOP('',(#22469,#22470,#22471,#22472));
#5445=EDGE_LOOP('',(#22473,#22474,#22475));
#5446=EDGE_LOOP('',(#22476,#22477,#22478,#22479));
#5447=EDGE_LOOP('',(#22480,#22481,#22482));
#5448=EDGE_LOOP('',(#22483,#22484,#22485,#22486));
#5449=EDGE_LOOP('',(#22487,#22488,#22489));
#5450=EDGE_LOOP('',(#22490,#22491,#22492,#22493));
#5451=EDGE_LOOP('',(#22494,#22495,#22496));
#5452=EDGE_LOOP('',(#22497,#22498,#22499,#22500));
#5453=EDGE_LOOP('',(#22501,#22502,#22503));
#5454=EDGE_LOOP('',(#22504,#22505,#22506,#22507));
#5455=EDGE_LOOP('',(#22508,#22509,#22510));
#5456=EDGE_LOOP('',(#22511,#22512,#22513,#22514));
#5457=EDGE_LOOP('',(#22515,#22516,#22517));
#5458=EDGE_LOOP('',(#22518,#22519,#22520,#22521));
#5459=EDGE_LOOP('',(#22522,#22523,#22524));
#5460=EDGE_LOOP('',(#22525,#22526,#22527,#22528));
#5461=EDGE_LOOP('',(#22529,#22530,#22531));
#5462=EDGE_LOOP('',(#22532,#22533,#22534,#22535));
#5463=EDGE_LOOP('',(#22536,#22537,#22538));
#5464=EDGE_LOOP('',(#22539,#22540,#22541,#22542));
#5465=EDGE_LOOP('',(#22543,#22544,#22545));
#5466=EDGE_LOOP('',(#22546,#22547,#22548,#22549));
#5467=EDGE_LOOP('',(#22550,#22551,#22552));
#5468=EDGE_LOOP('',(#22553,#22554,#22555,#22556));
#5469=EDGE_LOOP('',(#22557,#22558,#22559));
#5470=EDGE_LOOP('',(#22560,#22561,#22562,#22563));
#5471=EDGE_LOOP('',(#22564,#22565,#22566));
#5472=EDGE_LOOP('',(#22567,#22568,#22569));
#5473=EDGE_LOOP('',(#22570,#22571,#22572));
#5474=EDGE_LOOP('',(#22573,#22574,#22575,#22576));
#5475=EDGE_LOOP('',(#22577));
#5476=EDGE_LOOP('',(#22578));
#5477=EDGE_LOOP('',(#22579,#22580,#22581,#22582));
#5478=EDGE_LOOP('',(#22583,#22584,#22585,#22586,#22587,#22588,#22589,#22590,
#22591,#22592,#22593,#22594));
#5479=EDGE_LOOP('',(#22595,#22596,#22597,#22598,#22599,#22600,#22601,#22602,
#22603,#22604,#22605,#22606,#22607,#22608,#22609,#22610,#22611,#22612,#22613,
#22614,#22615,#22616,#22617,#22618,#22619));
#5480=EDGE_LOOP('',(#22620,#22621,#22622,#22623));
#5481=EDGE_LOOP('',(#22624,#22625,#22626,#22627));
#5482=EDGE_LOOP('',(#22628,#22629,#22630,#22631));
#5483=EDGE_LOOP('',(#22632,#22633,#22634,#22635));
#5484=EDGE_LOOP('',(#22636,#22637,#22638,#22639));
#5485=EDGE_LOOP('',(#22640,#22641,#22642,#22643));
#5486=EDGE_LOOP('',(#22644,#22645,#22646,#22647));
#5487=EDGE_LOOP('',(#22648,#22649,#22650,#22651));
#5488=EDGE_LOOP('',(#22652,#22653,#22654,#22655));
#5489=EDGE_LOOP('',(#22656,#22657,#22658,#22659));
#5490=EDGE_LOOP('',(#22660,#22661,#22662,#22663));
#5491=EDGE_LOOP('',(#22664,#22665,#22666,#22667));
#5492=EDGE_LOOP('',(#22668,#22669,#22670,#22671));
#5493=EDGE_LOOP('',(#22672,#22673,#22674,#22675));
#5494=EDGE_LOOP('',(#22676,#22677,#22678,#22679));
#5495=EDGE_LOOP('',(#22680,#22681,#22682,#22683));
#5496=EDGE_LOOP('',(#22684,#22685,#22686,#22687));
#5497=EDGE_LOOP('',(#22688,#22689,#22690,#22691));
#5498=EDGE_LOOP('',(#22692,#22693,#22694,#22695));
#5499=EDGE_LOOP('',(#22696,#22697,#22698,#22699));
#5500=EDGE_LOOP('',(#22700,#22701,#22702,#22703));
#5501=EDGE_LOOP('',(#22704,#22705,#22706,#22707));
#5502=EDGE_LOOP('',(#22708,#22709,#22710,#22711));
#5503=EDGE_LOOP('',(#22712,#22713,#22714,#22715));
#5504=EDGE_LOOP('',(#22716,#22717,#22718,#22719));
#5505=EDGE_LOOP('',(#22720,#22721,#22722,#22723));
#5506=EDGE_LOOP('',(#22724,#22725,#22726,#22727));
#5507=EDGE_LOOP('',(#22728,#22729,#22730,#22731));
#5508=EDGE_LOOP('',(#22732,#22733,#22734,#22735));
#5509=EDGE_LOOP('',(#22736,#22737,#22738,#22739));
#5510=EDGE_LOOP('',(#22740,#22741,#22742,#22743));
#5511=EDGE_LOOP('',(#22744,#22745,#22746,#22747));
#5512=EDGE_LOOP('',(#22748,#22749,#22750,#22751));
#5513=EDGE_LOOP('',(#22752,#22753,#22754,#22755));
#5514=EDGE_LOOP('',(#22756,#22757,#22758,#22759));
#5515=EDGE_LOOP('',(#22760,#22761,#22762,#22763));
#5516=EDGE_LOOP('',(#22764,#22765,#22766,#22767));
#5517=EDGE_LOOP('',(#22768));
#5518=EDGE_LOOP('',(#22769));
#5519=EDGE_LOOP('',(#22770,#22771,#22772,#22773));
#5520=EDGE_LOOP('',(#22774));
#5521=EDGE_LOOP('',(#22775));
#5522=EDGE_LOOP('',(#22776,#22777,#22778,#22779));
#5523=EDGE_LOOP('',(#22780,#22781));
#5524=EDGE_LOOP('',(#22782,#22783,#22784,#22785));
#5525=EDGE_LOOP('',(#22786,#22787,#22788,#22789));
#5526=EDGE_LOOP('',(#22790,#22791,#22792,#22793));
#5527=EDGE_LOOP('',(#22794,#22795,#22796,#22797));
#5528=EDGE_LOOP('',(#22798,#22799,#22800,#22801));
#5529=EDGE_LOOP('',(#22802,#22803,#22804,#22805));
#5530=EDGE_LOOP('',(#22806,#22807,#22808,#22809));
#5531=EDGE_LOOP('',(#22810,#22811,#22812,#22813));
#5532=EDGE_LOOP('',(#22814,#22815,#22816,#22817));
#5533=EDGE_LOOP('',(#22818,#22819,#22820,#22821));
#5534=EDGE_LOOP('',(#22822,#22823,#22824,#22825));
#5535=EDGE_LOOP('',(#22826,#22827,#22828,#22829));
#5536=EDGE_LOOP('',(#22830,#22831,#22832,#22833));
#5537=EDGE_LOOP('',(#22834,#22835,#22836,#22837));
#5538=EDGE_LOOP('',(#22838,#22839,#22840,#22841));
#5539=EDGE_LOOP('',(#22842,#22843,#22844,#22845));
#5540=EDGE_LOOP('',(#22846,#22847,#22848,#22849));
#5541=EDGE_LOOP('',(#22850,#22851,#22852,#22853));
#5542=EDGE_LOOP('',(#22854,#22855,#22856,#22857));
#5543=EDGE_LOOP('',(#22858,#22859,#22860,#22861));
#5544=EDGE_LOOP('',(#22862,#22863,#22864,#22865,#22866,#22867,#22868,#22869,
#22870,#22871,#22872,#22873));
#5545=EDGE_LOOP('',(#22874,#22875,#22876,#22877,#22878,#22879,#22880,#22881));
#5546=EDGE_LOOP('',(#22882,#22883,#22884,#22885));
#5547=EDGE_LOOP('',(#22886,#22887,#22888,#22889));
#5548=EDGE_LOOP('',(#22890,#22891,#22892,#22893));
#5549=EDGE_LOOP('',(#22894,#22895,#22896,#22897));
#5550=EDGE_LOOP('',(#22898,#22899,#22900,#22901));
#5551=EDGE_LOOP('',(#22902,#22903,#22904,#22905));
#5552=EDGE_LOOP('',(#22906,#22907,#22908,#22909));
#5553=EDGE_LOOP('',(#22910,#22911,#22912,#22913));
#5554=EDGE_LOOP('',(#22914,#22915,#22916,#22917));
#5555=EDGE_LOOP('',(#22918,#22919,#22920,#22921));
#5556=EDGE_LOOP('',(#22922,#22923,#22924,#22925));
#5557=EDGE_LOOP('',(#22926,#22927,#22928,#22929));
#5558=EDGE_LOOP('',(#22930,#22931,#22932,#22933));
#5559=EDGE_LOOP('',(#22934,#22935,#22936,#22937));
#5560=EDGE_LOOP('',(#22938,#22939,#22940,#22941,#22942,#22943,#22944,#22945,
#22946,#22947,#22948));
#5561=EDGE_LOOP('',(#22949,#22950,#22951));
#5562=EDGE_LOOP('',(#22952,#22953,#22954));
#5563=EDGE_LOOP('',(#22955,#22956,#22957,#22958,#22959,#22960,#22961,#22962));
#5564=EDGE_LOOP('',(#22963,#22964,#22965,#22966));
#5565=EDGE_LOOP('',(#22967,#22968,#22969,#22970));
#5566=EDGE_LOOP('',(#22971,#22972,#22973,#22974));
#5567=EDGE_LOOP('',(#22975,#22976,#22977,#22978));
#5568=EDGE_LOOP('',(#22979,#22980,#22981,#22982));
#5569=EDGE_LOOP('',(#22983,#22984,#22985,#22986));
#5570=EDGE_LOOP('',(#22987,#22988,#22989,#22990));
#5571=EDGE_LOOP('',(#22991,#22992,#22993,#22994));
#5572=EDGE_LOOP('',(#22995,#22996,#22997,#22998));
#5573=EDGE_LOOP('',(#22999,#23000,#23001,#23002));
#5574=EDGE_LOOP('',(#23003,#23004,#23005,#23006));
#5575=EDGE_LOOP('',(#23007,#23008,#23009,#23010));
#5576=EDGE_LOOP('',(#23011,#23012,#23013,#23014));
#5577=EDGE_LOOP('',(#23015,#23016,#23017,#23018));
#5578=EDGE_LOOP('',(#23019,#23020,#23021,#23022));
#5579=EDGE_LOOP('',(#23023,#23024,#23025,#23026));
#5580=EDGE_LOOP('',(#23027,#23028,#23029,#23030));
#5581=EDGE_LOOP('',(#23031,#23032,#23033,#23034));
#5582=EDGE_LOOP('',(#23035,#23036,#23037,#23038));
#5583=EDGE_LOOP('',(#23039,#23040,#23041,#23042));
#5584=EDGE_LOOP('',(#23043,#23044,#23045,#23046,#23047,#23048,#23049,#23050,
#23051,#23052,#23053,#23054));
#5585=EDGE_LOOP('',(#23055,#23056,#23057,#23058,#23059,#23060,#23061,#23062));
#5586=EDGE_LOOP('',(#23063,#23064,#23065,#23066));
#5587=EDGE_LOOP('',(#23067,#23068,#23069,#23070));
#5588=EDGE_LOOP('',(#23071,#23072,#23073,#23074));
#5589=EDGE_LOOP('',(#23075,#23076,#23077,#23078));
#5590=EDGE_LOOP('',(#23079,#23080,#23081,#23082));
#5591=EDGE_LOOP('',(#23083,#23084,#23085,#23086));
#5592=EDGE_LOOP('',(#23087,#23088,#23089,#23090));
#5593=EDGE_LOOP('',(#23091,#23092,#23093,#23094));
#5594=EDGE_LOOP('',(#23095,#23096,#23097,#23098));
#5595=EDGE_LOOP('',(#23099,#23100,#23101,#23102));
#5596=EDGE_LOOP('',(#23103,#23104,#23105,#23106));
#5597=EDGE_LOOP('',(#23107,#23108,#23109,#23110));
#5598=EDGE_LOOP('',(#23111,#23112,#23113,#23114));
#5599=EDGE_LOOP('',(#23115,#23116,#23117,#23118));
#5600=EDGE_LOOP('',(#23119,#23120,#23121,#23122));
#5601=EDGE_LOOP('',(#23123,#23124,#23125,#23126));
#5602=EDGE_LOOP('',(#23127,#23128,#23129,#23130));
#5603=EDGE_LOOP('',(#23131,#23132,#23133,#23134));
#5604=EDGE_LOOP('',(#23135,#23136,#23137,#23138));
#5605=EDGE_LOOP('',(#23139,#23140,#23141,#23142));
#5606=EDGE_LOOP('',(#23143,#23144,#23145,#23146));
#5607=EDGE_LOOP('',(#23147,#23148,#23149,#23150));
#5608=EDGE_LOOP('',(#23151,#23152,#23153,#23154));
#5609=EDGE_LOOP('',(#23155,#23156,#23157,#23158));
#5610=EDGE_LOOP('',(#23159,#23160,#23161,#23162));
#5611=EDGE_LOOP('',(#23163,#23164,#23165,#23166));
#5612=EDGE_LOOP('',(#23167,#23168,#23169,#23170));
#5613=EDGE_LOOP('',(#23171,#23172,#23173,#23174));
#5614=EDGE_LOOP('',(#23175,#23176,#23177,#23178));
#5615=EDGE_LOOP('',(#23179,#23180,#23181,#23182));
#5616=EDGE_LOOP('',(#23183,#23184,#23185,#23186,#23187,#23188,#23189,#23190,
#23191,#23192,#23193,#23194,#23195,#23196,#23197,#23198,#23199,#23200,#23201,
#23202,#23203,#23204,#23205,#23206,#23207,#23208,#23209,#23210,#23211,#23212));
#5617=EDGE_LOOP('',(#23213,#23214,#23215,#23216,#23217,#23218,#23219,#23220));
#5618=EDGE_LOOP('',(#23221,#23222,#23223,#23224));
#5619=EDGE_LOOP('',(#23225,#23226,#23227,#23228));
#5620=EDGE_LOOP('',(#23229,#23230,#23231,#23232));
#5621=EDGE_LOOP('',(#23233,#23234,#23235,#23236));
#5622=EDGE_LOOP('',(#23237,#23238,#23239,#23240));
#5623=EDGE_LOOP('',(#23241,#23242,#23243,#23244));
#5624=EDGE_LOOP('',(#23245,#23246,#23247,#23248));
#5625=EDGE_LOOP('',(#23249,#23250,#23251,#23252));
#5626=EDGE_LOOP('',(#23253,#23254,#23255,#23256));
#5627=EDGE_LOOP('',(#23257,#23258,#23259,#23260));
#5628=EDGE_LOOP('',(#23261,#23262,#23263,#23264));
#5629=EDGE_LOOP('',(#23265,#23266,#23267,#23268));
#5630=EDGE_LOOP('',(#23269,#23270,#23271,#23272));
#5631=EDGE_LOOP('',(#23273,#23274,#23275,#23276));
#5632=EDGE_LOOP('',(#23277,#23278,#23279,#23280));
#5633=EDGE_LOOP('',(#23281,#23282,#23283,#23284));
#5634=EDGE_LOOP('',(#23285,#23286,#23287,#23288));
#5635=EDGE_LOOP('',(#23289,#23290,#23291,#23292));
#5636=EDGE_LOOP('',(#23293,#23294,#23295,#23296));
#5637=EDGE_LOOP('',(#23297,#23298,#23299,#23300));
#5638=EDGE_LOOP('',(#23301,#23302,#23303,#23304,#23305,#23306,#23307,#23308,
#23309,#23310,#23311,#23312));
#5639=EDGE_LOOP('',(#23313,#23314,#23315,#23316,#23317,#23318,#23319,#23320));
#5640=EDGE_LOOP('',(#23321,#23322,#23323,#23324));
#5641=EDGE_LOOP('',(#23325,#23326,#23327,#23328));
#5642=EDGE_LOOP('',(#23329,#23330,#23331,#23332));
#5643=EDGE_LOOP('',(#23333,#23334,#23335,#23336));
#5644=EDGE_LOOP('',(#23337,#23338,#23339,#23340));
#5645=EDGE_LOOP('',(#23341,#23342,#23343,#23344));
#5646=EDGE_LOOP('',(#23345,#23346,#23347,#23348));
#5647=EDGE_LOOP('',(#23349,#23350,#23351,#23352));
#5648=EDGE_LOOP('',(#23353,#23354,#23355,#23356));
#5649=EDGE_LOOP('',(#23357,#23358,#23359,#23360));
#5650=EDGE_LOOP('',(#23361,#23362,#23363,#23364));
#5651=EDGE_LOOP('',(#23365,#23366,#23367,#23368));
#5652=EDGE_LOOP('',(#23369,#23370,#23371,#23372));
#5653=EDGE_LOOP('',(#23373,#23374,#23375,#23376));
#5654=EDGE_LOOP('',(#23377,#23378,#23379,#23380));
#5655=EDGE_LOOP('',(#23381,#23382,#23383,#23384));
#5656=EDGE_LOOP('',(#23385,#23386,#23387,#23388));
#5657=EDGE_LOOP('',(#23389,#23390,#23391,#23392));
#5658=EDGE_LOOP('',(#23393,#23394,#23395,#23396));
#5659=EDGE_LOOP('',(#23397,#23398,#23399,#23400));
#5660=EDGE_LOOP('',(#23401,#23402,#23403,#23404));
#5661=EDGE_LOOP('',(#23405,#23406,#23407,#23408));
#5662=EDGE_LOOP('',(#23409,#23410,#23411,#23412,#23413,#23414,#23415,#23416,
#23417,#23418,#23419,#23420,#23421,#23422,#23423,#23424,#23425,#23426,#23427,
#23428,#23429,#23430));
#5663=EDGE_LOOP('',(#23431,#23432,#23433,#23434,#23435,#23436,#23437,#23438));
#5664=EDGE_LOOP('',(#23439,#23440,#23441,#23442));
#5665=EDGE_LOOP('',(#23443,#23444,#23445,#23446));
#5666=EDGE_LOOP('',(#23447,#23448,#23449,#23450));
#5667=EDGE_LOOP('',(#23451,#23452,#23453,#23454));
#5668=EDGE_LOOP('',(#23455,#23456,#23457,#23458));
#5669=EDGE_LOOP('',(#23459,#23460,#23461,#23462));
#5670=EDGE_LOOP('',(#23463,#23464,#23465,#23466));
#5671=EDGE_LOOP('',(#23467,#23468,#23469,#23470));
#5672=EDGE_LOOP('',(#23471,#23472,#23473,#23474));
#5673=EDGE_LOOP('',(#23475,#23476,#23477,#23478));
#5674=EDGE_LOOP('',(#23479,#23480,#23481,#23482));
#5675=EDGE_LOOP('',(#23483,#23484,#23485,#23486));
#5676=EDGE_LOOP('',(#23487,#23488,#23489,#23490));
#5677=EDGE_LOOP('',(#23491,#23492,#23493,#23494));
#5678=EDGE_LOOP('',(#23495,#23496,#23497,#23498));
#5679=EDGE_LOOP('',(#23499,#23500,#23501,#23502));
#5680=EDGE_LOOP('',(#23503,#23504,#23505,#23506));
#5681=EDGE_LOOP('',(#23507,#23508,#23509,#23510));
#5682=EDGE_LOOP('',(#23511,#23512,#23513,#23514));
#5683=EDGE_LOOP('',(#23515,#23516,#23517,#23518));
#5684=EDGE_LOOP('',(#23519,#23520,#23521,#23522,#23523,#23524,#23525,#23526,
#23527,#23528,#23529,#23530));
#5685=EDGE_LOOP('',(#23531,#23532,#23533,#23534,#23535,#23536,#23537,#23538));
#5686=EDGE_LOOP('',(#23539,#23540,#23541,#23542));
#5687=EDGE_LOOP('',(#23543,#23544,#23545,#23546));
#5688=EDGE_LOOP('',(#23547,#23548,#23549,#23550));
#5689=EDGE_LOOP('',(#23551,#23552,#23553,#23554));
#5690=EDGE_LOOP('',(#23555,#23556,#23557,#23558));
#5691=EDGE_LOOP('',(#23559,#23560,#23561,#23562));
#5692=EDGE_LOOP('',(#23563,#23564,#23565,#23566));
#5693=EDGE_LOOP('',(#23567,#23568,#23569,#23570));
#5694=EDGE_LOOP('',(#23571,#23572,#23573,#23574));
#5695=EDGE_LOOP('',(#23575,#23576,#23577,#23578,#23579,#23580,#23581,#23582,
#23583));
#5696=EDGE_LOOP('',(#23584,#23585,#23586,#23587,#23588,#23589,#23590,#23591));
#5697=EDGE_LOOP('',(#23592,#23593,#23594,#23595));
#5698=EDGE_LOOP('',(#23596,#23597,#23598,#23599));
#5699=EDGE_LOOP('',(#23600,#23601,#23602,#23603));
#5700=EDGE_LOOP('',(#23604,#23605,#23606,#23607));
#5701=EDGE_LOOP('',(#23608,#23609,#23610,#23611));
#5702=EDGE_LOOP('',(#23612,#23613,#23614,#23615));
#5703=EDGE_LOOP('',(#23616,#23617,#23618,#23619));
#5704=EDGE_LOOP('',(#23620,#23621,#23622,#23623));
#5705=EDGE_LOOP('',(#23624,#23625,#23626,#23627));
#5706=EDGE_LOOP('',(#23628,#23629,#23630,#23631));
#5707=EDGE_LOOP('',(#23632,#23633,#23634,#23635));
#5708=EDGE_LOOP('',(#23636,#23637,#23638,#23639));
#5709=EDGE_LOOP('',(#23640,#23641,#23642,#23643));
#5710=EDGE_LOOP('',(#23644,#23645,#23646,#23647));
#5711=EDGE_LOOP('',(#23648,#23649,#23650,#23651));
#5712=EDGE_LOOP('',(#23652,#23653,#23654,#23655));
#5713=EDGE_LOOP('',(#23656,#23657,#23658,#23659));
#5714=EDGE_LOOP('',(#23660,#23661,#23662,#23663));
#5715=EDGE_LOOP('',(#23664,#23665,#23666,#23667));
#5716=EDGE_LOOP('',(#23668,#23669,#23670,#23671));
#5717=EDGE_LOOP('',(#23672,#23673,#23674,#23675,#23676,#23677,#23678,#23679,
#23680,#23681,#23682,#23683));
#5718=EDGE_LOOP('',(#23684,#23685,#23686,#23687,#23688,#23689,#23690,#23691));
#5719=EDGE_LOOP('',(#23692,#23693,#23694,#23695,#23696,#23697,#23698,#23699));
#5720=EDGE_LOOP('',(#23700,#23701,#23702,#23703));
#5721=EDGE_LOOP('',(#23704,#23705,#23706,#23707));
#5722=EDGE_LOOP('',(#23708,#23709,#23710,#23711));
#5723=EDGE_LOOP('',(#23712,#23713,#23714,#23715));
#5724=EDGE_LOOP('',(#23716,#23717,#23718,#23719));
#5725=EDGE_LOOP('',(#23720,#23721,#23722,#23723));
#5726=EDGE_LOOP('',(#23724,#23725,#23726,#23727));
#5727=EDGE_LOOP('',(#23728,#23729,#23730,#23731));
#5728=EDGE_LOOP('',(#23732,#23733,#23734,#23735));
#5729=EDGE_LOOP('',(#23736,#23737,#23738,#23739));
#5730=EDGE_LOOP('',(#23740,#23741,#23742,#23743));
#5731=EDGE_LOOP('',(#23744,#23745,#23746,#23747));
#5732=EDGE_LOOP('',(#23748,#23749,#23750,#23751));
#5733=EDGE_LOOP('',(#23752,#23753,#23754,#23755));
#5734=EDGE_LOOP('',(#23756,#23757,#23758,#23759));
#5735=EDGE_LOOP('',(#23760,#23761,#23762,#23763));
#5736=EDGE_LOOP('',(#23764,#23765,#23766,#23767));
#5737=EDGE_LOOP('',(#23768,#23769,#23770,#23771));
#5738=EDGE_LOOP('',(#23772,#23773,#23774,#23775));
#5739=EDGE_LOOP('',(#23776,#23777,#23778,#23779));
#5740=EDGE_LOOP('',(#23780,#23781,#23782,#23783,#23784,#23785,#23786,#23787,
#23788,#23789,#23790,#23791));
#5741=EDGE_LOOP('',(#23792,#23793,#23794,#23795,#23796,#23797,#23798,#23799));
#5742=EDGE_LOOP('',(#23800,#23801,#23802,#23803));
#5743=EDGE_LOOP('',(#23804,#23805,#23806,#23807));
#5744=EDGE_LOOP('',(#23808,#23809,#23810,#23811));
#5745=EDGE_LOOP('',(#23812,#23813,#23814,#23815));
#5746=EDGE_LOOP('',(#23816,#23817,#23818,#23819));
#5747=EDGE_LOOP('',(#23820,#23821,#23822,#23823));
#5748=EDGE_LOOP('',(#23824,#23825,#23826,#23827));
#5749=EDGE_LOOP('',(#23828,#23829,#23830,#23831));
#5750=EDGE_LOOP('',(#23832,#23833,#23834,#23835));
#5751=EDGE_LOOP('',(#23836,#23837,#23838,#23839,#23840,#23841,#23842,#23843,
#23844));
#5752=EDGE_LOOP('',(#23845,#23846,#23847,#23848,#23849,#23850,#23851,#23852));
#5753=EDGE_LOOP('',(#23853,#23854,#23855,#23856));
#5754=EDGE_LOOP('',(#23857,#23858,#23859,#23860));
#5755=EDGE_LOOP('',(#23861,#23862,#23863,#23864));
#5756=EDGE_LOOP('',(#23865,#23866,#23867,#23868));
#5757=EDGE_LOOP('',(#23869,#23870,#23871,#23872));
#5758=EDGE_LOOP('',(#23873,#23874,#23875,#23876));
#5759=EDGE_LOOP('',(#23877,#23878,#23879,#23880));
#5760=EDGE_LOOP('',(#23881,#23882,#23883,#23884));
#5761=EDGE_LOOP('',(#23885,#23886,#23887,#23888));
#5762=EDGE_LOOP('',(#23889,#23890,#23891,#23892));
#5763=EDGE_LOOP('',(#23893,#23894,#23895,#23896));
#5764=EDGE_LOOP('',(#23897,#23898,#23899,#23900));
#5765=EDGE_LOOP('',(#23901,#23902,#23903,#23904));
#5766=EDGE_LOOP('',(#23905,#23906,#23907,#23908));
#5767=EDGE_LOOP('',(#23909,#23910,#23911,#23912));
#5768=EDGE_LOOP('',(#23913,#23914,#23915,#23916));
#5769=EDGE_LOOP('',(#23917,#23918,#23919,#23920));
#5770=EDGE_LOOP('',(#23921,#23922,#23923,#23924));
#5771=EDGE_LOOP('',(#23925,#23926,#23927,#23928));
#5772=EDGE_LOOP('',(#23929,#23930,#23931,#23932));
#5773=EDGE_LOOP('',(#23933,#23934,#23935,#23936,#23937,#23938,#23939,#23940,
#23941,#23942,#23943,#23944));
#5774=EDGE_LOOP('',(#23945,#23946,#23947,#23948,#23949,#23950,#23951,#23952));
#5775=EDGE_LOOP('',(#23953,#23954,#23955,#23956));
#5776=EDGE_LOOP('',(#23957,#23958,#23959,#23960));
#5777=EDGE_LOOP('',(#23961,#23962,#23963,#23964));
#5778=EDGE_LOOP('',(#23965,#23966,#23967,#23968));
#5779=EDGE_LOOP('',(#23969,#23970,#23971,#23972));
#5780=EDGE_LOOP('',(#23973,#23974,#23975,#23976));
#5781=EDGE_LOOP('',(#23977,#23978,#23979,#23980));
#5782=EDGE_LOOP('',(#23981,#23982,#23983,#23984));
#5783=EDGE_LOOP('',(#23985,#23986,#23987,#23988));
#5784=EDGE_LOOP('',(#23989,#23990,#23991,#23992));
#5785=EDGE_LOOP('',(#23993,#23994,#23995,#23996));
#5786=EDGE_LOOP('',(#23997,#23998,#23999,#24000));
#5787=EDGE_LOOP('',(#24001,#24002,#24003,#24004));
#5788=EDGE_LOOP('',(#24005,#24006,#24007,#24008));
#5789=EDGE_LOOP('',(#24009,#24010,#24011,#24012));
#5790=EDGE_LOOP('',(#24013,#24014,#24015,#24016));
#5791=EDGE_LOOP('',(#24017,#24018,#24019,#24020));
#5792=EDGE_LOOP('',(#24021,#24022,#24023,#24024));
#5793=EDGE_LOOP('',(#24025,#24026,#24027,#24028));
#5794=EDGE_LOOP('',(#24029,#24030,#24031,#24032));
#5795=EDGE_LOOP('',(#24033,#24034,#24035,#24036));
#5796=EDGE_LOOP('',(#24037,#24038,#24039,#24040));
#5797=EDGE_LOOP('',(#24041,#24042,#24043,#24044,#24045,#24046,#24047,#24048,
#24049,#24050,#24051,#24052,#24053,#24054,#24055,#24056,#24057,#24058,#24059,
#24060,#24061,#24062));
#5798=EDGE_LOOP('',(#24063,#24064,#24065,#24066,#24067,#24068,#24069,#24070));
#5799=EDGE_LOOP('',(#24071,#24072,#24073,#24074));
#5800=EDGE_LOOP('',(#24075,#24076,#24077,#24078));
#5801=EDGE_LOOP('',(#24079,#24080,#24081,#24082));
#5802=EDGE_LOOP('',(#24083,#24084,#24085,#24086));
#5803=EDGE_LOOP('',(#24087,#24088,#24089,#24090));
#5804=EDGE_LOOP('',(#24091,#24092,#24093,#24094));
#5805=EDGE_LOOP('',(#24095,#24096,#24097,#24098));
#5806=EDGE_LOOP('',(#24099,#24100,#24101,#24102));
#5807=EDGE_LOOP('',(#24103,#24104,#24105,#24106));
#5808=EDGE_LOOP('',(#24107,#24108,#24109,#24110));
#5809=EDGE_LOOP('',(#24111,#24112,#24113,#24114));
#5810=EDGE_LOOP('',(#24115,#24116,#24117,#24118));
#5811=EDGE_LOOP('',(#24119,#24120,#24121,#24122));
#5812=EDGE_LOOP('',(#24123,#24124,#24125,#24126));
#5813=EDGE_LOOP('',(#24127,#24128,#24129,#24130));
#5814=EDGE_LOOP('',(#24131,#24132,#24133,#24134));
#5815=EDGE_LOOP('',(#24135,#24136,#24137,#24138));
#5816=EDGE_LOOP('',(#24139,#24140,#24141,#24142));
#5817=EDGE_LOOP('',(#24143,#24144,#24145,#24146));
#5818=EDGE_LOOP('',(#24147,#24148,#24149,#24150));
#5819=EDGE_LOOP('',(#24151,#24152,#24153,#24154,#24155,#24156,#24157,#24158,
#24159,#24160,#24161,#24162));
#5820=EDGE_LOOP('',(#24163,#24164,#24165,#24166,#24167,#24168,#24169,#24170));
#5821=EDGE_LOOP('',(#24171,#24172,#24173,#24174));
#5822=EDGE_LOOP('',(#24175,#24176,#24177,#24178));
#5823=EDGE_LOOP('',(#24179,#24180,#24181,#24182));
#5824=EDGE_LOOP('',(#24183,#24184,#24185,#24186));
#5825=EDGE_LOOP('',(#24187,#24188,#24189,#24190));
#5826=EDGE_LOOP('',(#24191,#24192,#24193,#24194));
#5827=EDGE_LOOP('',(#24195,#24196,#24197,#24198));
#5828=EDGE_LOOP('',(#24199,#24200,#24201,#24202));
#5829=EDGE_LOOP('',(#24203,#24204,#24205,#24206));
#5830=EDGE_LOOP('',(#24207,#24208,#24209,#24210));
#5831=EDGE_LOOP('',(#24211,#24212,#24213,#24214));
#5832=EDGE_LOOP('',(#24215,#24216,#24217,#24218));
#5833=EDGE_LOOP('',(#24219,#24220,#24221,#24222));
#5834=EDGE_LOOP('',(#24223,#24224,#24225,#24226));
#5835=EDGE_LOOP('',(#24227,#24228,#24229,#24230));
#5836=EDGE_LOOP('',(#24231,#24232,#24233,#24234));
#5837=EDGE_LOOP('',(#24235,#24236,#24237,#24238));
#5838=EDGE_LOOP('',(#24239,#24240,#24241,#24242));
#5839=EDGE_LOOP('',(#24243,#24244,#24245,#24246));
#5840=EDGE_LOOP('',(#24247,#24248,#24249,#24250));
#5841=EDGE_LOOP('',(#24251,#24252,#24253,#24254));
#5842=EDGE_LOOP('',(#24255,#24256,#24257,#24258));
#5843=EDGE_LOOP('',(#24259,#24260,#24261,#24262));
#5844=EDGE_LOOP('',(#24263,#24264,#24265,#24266));
#5845=EDGE_LOOP('',(#24267,#24268,#24269,#24270));
#5846=EDGE_LOOP('',(#24271,#24272,#24273,#24274));
#5847=EDGE_LOOP('',(#24275,#24276,#24277,#24278));
#5848=EDGE_LOOP('',(#24279,#24280,#24281,#24282));
#5849=EDGE_LOOP('',(#24283,#24284,#24285,#24286));
#5850=EDGE_LOOP('',(#24287,#24288,#24289,#24290));
#5851=EDGE_LOOP('',(#24291,#24292,#24293,#24294,#24295,#24296,#24297,#24298,
#24299,#24300,#24301,#24302,#24303,#24304,#24305,#24306,#24307,#24308,#24309,
#24310,#24311,#24312,#24313,#24314,#24315,#24316,#24317,#24318,#24319,#24320));
#5852=EDGE_LOOP('',(#24321,#24322,#24323,#24324,#24325,#24326,#24327,#24328));
#5853=EDGE_LOOP('',(#24329,#24330,#24331,#24332));
#5854=EDGE_LOOP('',(#24333,#24334,#24335,#24336));
#5855=EDGE_LOOP('',(#24337,#24338,#24339,#24340));
#5856=EDGE_LOOP('',(#24341,#24342,#24343,#24344));
#5857=EDGE_LOOP('',(#24345,#24346,#24347,#24348));
#5858=EDGE_LOOP('',(#24349,#24350,#24351,#24352));
#5859=EDGE_LOOP('',(#24353,#24354,#24355,#24356));
#5860=EDGE_LOOP('',(#24357,#24358,#24359,#24360));
#5861=EDGE_LOOP('',(#24361,#24362,#24363,#24364));
#5862=EDGE_LOOP('',(#24365,#24366,#24367,#24368));
#5863=EDGE_LOOP('',(#24369,#24370,#24371,#24372));
#5864=EDGE_LOOP('',(#24373,#24374,#24375,#24376));
#5865=EDGE_LOOP('',(#24377,#24378,#24379,#24380));
#5866=EDGE_LOOP('',(#24381,#24382,#24383,#24384));
#5867=EDGE_LOOP('',(#24385,#24386,#24387,#24388));
#5868=EDGE_LOOP('',(#24389,#24390,#24391,#24392));
#5869=EDGE_LOOP('',(#24393,#24394,#24395,#24396));
#5870=EDGE_LOOP('',(#24397,#24398,#24399,#24400));
#5871=EDGE_LOOP('',(#24401,#24402,#24403,#24404));
#5872=EDGE_LOOP('',(#24405,#24406,#24407,#24408));
#5873=EDGE_LOOP('',(#24409,#24410,#24411,#24412,#24413,#24414,#24415,#24416,
#24417,#24418,#24419,#24420));
#5874=EDGE_LOOP('',(#24421,#24422,#24423,#24424,#24425,#24426,#24427,#24428));
#5875=EDGE_LOOP('',(#24429,#24430,#24431,#24432));
#5876=EDGE_LOOP('',(#24433,#24434,#24435,#24436));
#5877=EDGE_LOOP('',(#24437,#24438,#24439,#24440));
#5878=EDGE_LOOP('',(#24441,#24442,#24443,#24444));
#5879=EDGE_LOOP('',(#24445,#24446,#24447,#24448));
#5880=EDGE_LOOP('',(#24449,#24450,#24451,#24452));
#5881=EDGE_LOOP('',(#24453,#24454,#24455,#24456));
#5882=EDGE_LOOP('',(#24457,#24458,#24459,#24460));
#5883=EDGE_LOOP('',(#24461,#24462,#24463,#24464));
#5884=EDGE_LOOP('',(#24465,#24466,#24467,#24468));
#5885=EDGE_LOOP('',(#24469,#24470,#24471,#24472));
#5886=EDGE_LOOP('',(#24473,#24474,#24475,#24476));
#5887=EDGE_LOOP('',(#24477,#24478,#24479,#24480));
#5888=EDGE_LOOP('',(#24481,#24482,#24483,#24484));
#5889=EDGE_LOOP('',(#24485,#24486,#24487,#24488,#24489,#24490,#24491,#24492,
#24493,#24494,#24495));
#5890=EDGE_LOOP('',(#24496,#24497,#24498));
#5891=EDGE_LOOP('',(#24499,#24500,#24501));
#5892=EDGE_LOOP('',(#24502,#24503,#24504,#24505,#24506,#24507,#24508,#24509));
#5893=EDGE_LOOP('',(#24510,#24511,#24512,#24513));
#5894=EDGE_LOOP('',(#24514,#24515,#24516,#24517));
#5895=EDGE_LOOP('',(#24518,#24519,#24520,#24521));
#5896=EDGE_LOOP('',(#24522,#24523,#24524,#24525));
#5897=EDGE_LOOP('',(#24526,#24527,#24528,#24529));
#5898=EDGE_LOOP('',(#24530,#24531,#24532,#24533));
#5899=EDGE_LOOP('',(#24534,#24535,#24536,#24537));
#5900=EDGE_LOOP('',(#24538,#24539,#24540,#24541));
#5901=EDGE_LOOP('',(#24542,#24543,#24544,#24545));
#5902=EDGE_LOOP('',(#24546,#24547,#24548,#24549));
#5903=EDGE_LOOP('',(#24550,#24551,#24552,#24553));
#5904=EDGE_LOOP('',(#24554,#24555,#24556,#24557));
#5905=EDGE_LOOP('',(#24558,#24559,#24560,#24561));
#5906=EDGE_LOOP('',(#24562,#24563,#24564,#24565));
#5907=EDGE_LOOP('',(#24566,#24567,#24568,#24569));
#5908=EDGE_LOOP('',(#24570,#24571,#24572,#24573));
#5909=EDGE_LOOP('',(#24574,#24575,#24576,#24577));
#5910=EDGE_LOOP('',(#24578,#24579,#24580,#24581));
#5911=EDGE_LOOP('',(#24582,#24583,#24584,#24585));
#5912=EDGE_LOOP('',(#24586,#24587,#24588,#24589));
#5913=EDGE_LOOP('',(#24590,#24591,#24592,#24593));
#5914=EDGE_LOOP('',(#24594,#24595,#24596,#24597));
#5915=EDGE_LOOP('',(#24598,#24599,#24600,#24601));
#5916=EDGE_LOOP('',(#24602,#24603,#24604,#24605));
#5917=EDGE_LOOP('',(#24606,#24607,#24608,#24609));
#5918=EDGE_LOOP('',(#24610,#24611,#24612,#24613));
#5919=EDGE_LOOP('',(#24614,#24615,#24616,#24617));
#5920=EDGE_LOOP('',(#24618,#24619,#24620,#24621));
#5921=EDGE_LOOP('',(#24622,#24623,#24624,#24625));
#5922=EDGE_LOOP('',(#24626,#24627,#24628,#24629));
#5923=EDGE_LOOP('',(#24630,#24631,#24632,#24633));
#5924=EDGE_LOOP('',(#24634,#24635,#24636,#24637));
#5925=EDGE_LOOP('',(#24638,#24639,#24640,#24641));
#5926=EDGE_LOOP('',(#24642,#24643,#24644,#24645));
#5927=EDGE_LOOP('',(#24646,#24647,#24648,#24649));
#5928=EDGE_LOOP('',(#24650,#24651,#24652,#24653));
#5929=EDGE_LOOP('',(#24654,#24655,#24656,#24657));
#5930=EDGE_LOOP('',(#24658,#24659,#24660,#24661));
#5931=EDGE_LOOP('',(#24662,#24663,#24664,#24665));
#5932=EDGE_LOOP('',(#24666,#24667,#24668,#24669));
#5933=EDGE_LOOP('',(#24670,#24671,#24672,#24673));
#5934=EDGE_LOOP('',(#24674,#24675,#24676,#24677));
#5935=EDGE_LOOP('',(#24678,#24679,#24680,#24681));
#5936=EDGE_LOOP('',(#24682,#24683,#24684,#24685));
#5937=EDGE_LOOP('',(#24686,#24687,#24688,#24689));
#5938=EDGE_LOOP('',(#24690,#24691,#24692,#24693));
#5939=EDGE_LOOP('',(#24694,#24695,#24696,#24697));
#5940=EDGE_LOOP('',(#24698,#24699,#24700,#24701));
#5941=EDGE_LOOP('',(#24702,#24703,#24704,#24705));
#5942=EDGE_LOOP('',(#24706,#24707,#24708,#24709));
#5943=EDGE_LOOP('',(#24710,#24711,#24712,#24713));
#5944=EDGE_LOOP('',(#24714,#24715,#24716,#24717));
#5945=EDGE_LOOP('',(#24718,#24719,#24720,#24721));
#5946=EDGE_LOOP('',(#24722,#24723,#24724,#24725));
#5947=EDGE_LOOP('',(#24726,#24727,#24728,#24729));
#5948=EDGE_LOOP('',(#24730,#24731,#24732,#24733));
#5949=EDGE_LOOP('',(#24734,#24735,#24736,#24737));
#5950=EDGE_LOOP('',(#24738,#24739,#24740,#24741));
#5951=EDGE_LOOP('',(#24742,#24743,#24744,#24745));
#5952=EDGE_LOOP('',(#24746,#24747,#24748,#24749));
#5953=EDGE_LOOP('',(#24750,#24751,#24752,#24753));
#5954=EDGE_LOOP('',(#24754,#24755,#24756,#24757));
#5955=EDGE_LOOP('',(#24758,#24759,#24760,#24761));
#5956=EDGE_LOOP('',(#24762,#24763,#24764,#24765));
#5957=EDGE_LOOP('',(#24766,#24767,#24768,#24769));
#5958=EDGE_LOOP('',(#24770,#24771,#24772,#24773));
#5959=EDGE_LOOP('',(#24774,#24775,#24776,#24777));
#5960=EDGE_LOOP('',(#24778,#24779,#24780,#24781));
#5961=EDGE_LOOP('',(#24782,#24783,#24784,#24785));
#5962=EDGE_LOOP('',(#24786,#24787,#24788,#24789));
#5963=EDGE_LOOP('',(#24790,#24791,#24792,#24793));
#5964=EDGE_LOOP('',(#24794,#24795,#24796,#24797));
#5965=EDGE_LOOP('',(#24798,#24799,#24800,#24801));
#5966=EDGE_LOOP('',(#24802,#24803,#24804,#24805));
#5967=EDGE_LOOP('',(#24806,#24807,#24808,#24809));
#5968=EDGE_LOOP('',(#24810,#24811,#24812,#24813));
#5969=EDGE_LOOP('',(#24814,#24815,#24816,#24817));
#5970=EDGE_LOOP('',(#24818,#24819,#24820,#24821));
#5971=EDGE_LOOP('',(#24822,#24823,#24824,#24825));
#5972=EDGE_LOOP('',(#24826,#24827,#24828,#24829));
#5973=EDGE_LOOP('',(#24830,#24831,#24832,#24833));
#5974=EDGE_LOOP('',(#24834,#24835,#24836,#24837));
#5975=EDGE_LOOP('',(#24838,#24839,#24840,#24841));
#5976=EDGE_LOOP('',(#24842,#24843,#24844,#24845));
#5977=EDGE_LOOP('',(#24846,#24847,#24848,#24849));
#5978=EDGE_LOOP('',(#24850,#24851,#24852,#24853));
#5979=EDGE_LOOP('',(#24854,#24855,#24856,#24857));
#5980=EDGE_LOOP('',(#24858,#24859,#24860,#24861));
#5981=EDGE_LOOP('',(#24862,#24863,#24864,#24865));
#5982=EDGE_LOOP('',(#24866,#24867,#24868,#24869));
#5983=EDGE_LOOP('',(#24870,#24871,#24872,#24873));
#5984=EDGE_LOOP('',(#24874,#24875,#24876,#24877));
#5985=EDGE_LOOP('',(#24878,#24879,#24880,#24881));
#5986=EDGE_LOOP('',(#24882,#24883,#24884,#24885));
#5987=EDGE_LOOP('',(#24886,#24887,#24888,#24889));
#5988=EDGE_LOOP('',(#24890,#24891,#24892,#24893));
#5989=EDGE_LOOP('',(#24894,#24895,#24896,#24897));
#5990=EDGE_LOOP('',(#24898,#24899,#24900,#24901));
#5991=EDGE_LOOP('',(#24902,#24903,#24904,#24905));
#5992=EDGE_LOOP('',(#24906,#24907,#24908,#24909));
#5993=EDGE_LOOP('',(#24910,#24911,#24912,#24913));
#5994=EDGE_LOOP('',(#24914,#24915,#24916,#24917));
#5995=EDGE_LOOP('',(#24918,#24919,#24920,#24921));
#5996=EDGE_LOOP('',(#24922,#24923,#24924,#24925));
#5997=EDGE_LOOP('',(#24926,#24927,#24928,#24929));
#5998=EDGE_LOOP('',(#24930,#24931,#24932,#24933));
#5999=EDGE_LOOP('',(#24934,#24935,#24936,#24937));
#6000=EDGE_LOOP('',(#24938,#24939,#24940,#24941));
#6001=EDGE_LOOP('',(#24942,#24943,#24944,#24945));
#6002=EDGE_LOOP('',(#24946,#24947,#24948,#24949));
#6003=EDGE_LOOP('',(#24950,#24951,#24952,#24953));
#6004=EDGE_LOOP('',(#24954,#24955,#24956,#24957));
#6005=EDGE_LOOP('',(#24958,#24959,#24960,#24961));
#6006=EDGE_LOOP('',(#24962,#24963,#24964,#24965));
#6007=EDGE_LOOP('',(#24966,#24967,#24968,#24969));
#6008=EDGE_LOOP('',(#24970,#24971,#24972,#24973));
#6009=EDGE_LOOP('',(#24974,#24975,#24976,#24977));
#6010=EDGE_LOOP('',(#24978,#24979,#24980,#24981));
#6011=EDGE_LOOP('',(#24982,#24983,#24984,#24985));
#6012=EDGE_LOOP('',(#24986,#24987,#24988,#24989));
#6013=EDGE_LOOP('',(#24990,#24991,#24992,#24993));
#6014=EDGE_LOOP('',(#24994,#24995,#24996,#24997));
#6015=EDGE_LOOP('',(#24998,#24999,#25000,#25001));
#6016=EDGE_LOOP('',(#25002,#25003,#25004,#25005));
#6017=EDGE_LOOP('',(#25006,#25007,#25008,#25009));
#6018=EDGE_LOOP('',(#25010,#25011,#25012,#25013));
#6019=EDGE_LOOP('',(#25014,#25015,#25016,#25017));
#6020=EDGE_LOOP('',(#25018,#25019,#25020,#25021));
#6021=EDGE_LOOP('',(#25022,#25023,#25024,#25025));
#6022=EDGE_LOOP('',(#25026,#25027,#25028,#25029));
#6023=EDGE_LOOP('',(#25030,#25031,#25032,#25033));
#6024=EDGE_LOOP('',(#25034,#25035,#25036,#25037));
#6025=EDGE_LOOP('',(#25038,#25039,#25040,#25041));
#6026=EDGE_LOOP('',(#25042,#25043,#25044,#25045));
#6027=EDGE_LOOP('',(#25046,#25047,#25048,#25049));
#6028=EDGE_LOOP('',(#25050,#25051,#25052,#25053));
#6029=EDGE_LOOP('',(#25054,#25055,#25056,#25057));
#6030=EDGE_LOOP('',(#25058,#25059,#25060,#25061));
#6031=EDGE_LOOP('',(#25062,#25063,#25064,#25065));
#6032=EDGE_LOOP('',(#25066,#25067,#25068,#25069));
#6033=EDGE_LOOP('',(#25070,#25071,#25072,#25073));
#6034=EDGE_LOOP('',(#25074,#25075,#25076,#25077));
#6035=EDGE_LOOP('',(#25078,#25079,#25080,#25081));
#6036=EDGE_LOOP('',(#25082,#25083,#25084,#25085));
#6037=EDGE_LOOP('',(#25086,#25087,#25088,#25089));
#6038=EDGE_LOOP('',(#25090,#25091,#25092,#25093));
#6039=EDGE_LOOP('',(#25094,#25095,#25096,#25097));
#6040=EDGE_LOOP('',(#25098,#25099,#25100,#25101));
#6041=EDGE_LOOP('',(#25102,#25103,#25104,#25105));
#6042=EDGE_LOOP('',(#25106,#25107,#25108,#25109));
#6043=EDGE_LOOP('',(#25110,#25111,#25112,#25113));
#6044=EDGE_LOOP('',(#25114,#25115,#25116,#25117));
#6045=EDGE_LOOP('',(#25118,#25119,#25120,#25121));
#6046=EDGE_LOOP('',(#25122,#25123,#25124,#25125));
#6047=EDGE_LOOP('',(#25126,#25127,#25128,#25129));
#6048=EDGE_LOOP('',(#25130,#25131,#25132,#25133));
#6049=EDGE_LOOP('',(#25134,#25135,#25136,#25137));
#6050=EDGE_LOOP('',(#25138,#25139,#25140,#25141));
#6051=EDGE_LOOP('',(#25142,#25143,#25144,#25145));
#6052=EDGE_LOOP('',(#25146,#25147,#25148,#25149));
#6053=EDGE_LOOP('',(#25150,#25151,#25152,#25153));
#6054=EDGE_LOOP('',(#25154,#25155,#25156,#25157));
#6055=EDGE_LOOP('',(#25158,#25159,#25160,#25161));
#6056=EDGE_LOOP('',(#25162,#25163,#25164,#25165));
#6057=EDGE_LOOP('',(#25166,#25167,#25168,#25169));
#6058=EDGE_LOOP('',(#25170,#25171,#25172,#25173));
#6059=EDGE_LOOP('',(#25174,#25175,#25176,#25177));
#6060=EDGE_LOOP('',(#25178,#25179,#25180,#25181));
#6061=EDGE_LOOP('',(#25182,#25183,#25184,#25185));
#6062=EDGE_LOOP('',(#25186,#25187,#25188,#25189));
#6063=EDGE_LOOP('',(#25190,#25191,#25192,#25193));
#6064=EDGE_LOOP('',(#25194,#25195,#25196,#25197));
#6065=EDGE_LOOP('',(#25198,#25199,#25200,#25201));
#6066=EDGE_LOOP('',(#25202,#25203,#25204,#25205));
#6067=EDGE_LOOP('',(#25206,#25207,#25208,#25209));
#6068=EDGE_LOOP('',(#25210,#25211,#25212,#25213));
#6069=EDGE_LOOP('',(#25214,#25215,#25216,#25217));
#6070=EDGE_LOOP('',(#25218,#25219,#25220,#25221));
#6071=EDGE_LOOP('',(#25222,#25223,#25224,#25225));
#6072=EDGE_LOOP('',(#25226,#25227,#25228,#25229));
#6073=EDGE_LOOP('',(#25230,#25231,#25232,#25233));
#6074=EDGE_LOOP('',(#25234,#25235,#25236,#25237));
#6075=EDGE_LOOP('',(#25238,#25239,#25240,#25241));
#6076=EDGE_LOOP('',(#25242,#25243,#25244,#25245));
#6077=EDGE_LOOP('',(#25246,#25247,#25248,#25249));
#6078=EDGE_LOOP('',(#25250,#25251,#25252,#25253));
#6079=EDGE_LOOP('',(#25254,#25255,#25256,#25257));
#6080=EDGE_LOOP('',(#25258,#25259,#25260,#25261));
#6081=EDGE_LOOP('',(#25262,#25263,#25264,#25265));
#6082=EDGE_LOOP('',(#25266,#25267,#25268,#25269));
#6083=EDGE_LOOP('',(#25270,#25271,#25272,#25273));
#6084=EDGE_LOOP('',(#25274,#25275,#25276,#25277));
#6085=EDGE_LOOP('',(#25278,#25279,#25280,#25281));
#6086=EDGE_LOOP('',(#25282,#25283,#25284,#25285));
#6087=EDGE_LOOP('',(#25286,#25287,#25288,#25289));
#6088=EDGE_LOOP('',(#25290,#25291,#25292,#25293));
#6089=EDGE_LOOP('',(#25294,#25295,#25296,#25297));
#6090=EDGE_LOOP('',(#25298,#25299,#25300,#25301));
#6091=EDGE_LOOP('',(#25302,#25303,#25304,#25305));
#6092=EDGE_LOOP('',(#25306,#25307,#25308,#25309));
#6093=EDGE_LOOP('',(#25310,#25311,#25312,#25313));
#6094=EDGE_LOOP('',(#25314,#25315,#25316,#25317));
#6095=EDGE_LOOP('',(#25318,#25319,#25320,#25321));
#6096=EDGE_LOOP('',(#25322,#25323,#25324,#25325));
#6097=EDGE_LOOP('',(#25326,#25327,#25328,#25329));
#6098=EDGE_LOOP('',(#25330,#25331,#25332,#25333));
#6099=EDGE_LOOP('',(#25334,#25335,#25336,#25337));
#6100=EDGE_LOOP('',(#25338,#25339,#25340,#25341));
#6101=EDGE_LOOP('',(#25342,#25343,#25344,#25345));
#6102=EDGE_LOOP('',(#25346,#25347,#25348,#25349));
#6103=EDGE_LOOP('',(#25350,#25351,#25352,#25353));
#6104=EDGE_LOOP('',(#25354,#25355,#25356,#25357));
#6105=EDGE_LOOP('',(#25358,#25359,#25360,#25361));
#6106=EDGE_LOOP('',(#25362,#25363,#25364,#25365));
#6107=EDGE_LOOP('',(#25366,#25367,#25368,#25369));
#6108=EDGE_LOOP('',(#25370,#25371,#25372,#25373));
#6109=EDGE_LOOP('',(#25374,#25375,#25376,#25377));
#6110=EDGE_LOOP('',(#25378,#25379,#25380,#25381));
#6111=EDGE_LOOP('',(#25382,#25383,#25384,#25385));
#6112=EDGE_LOOP('',(#25386,#25387,#25388,#25389));
#6113=EDGE_LOOP('',(#25390,#25391,#25392,#25393));
#6114=EDGE_LOOP('',(#25394,#25395,#25396,#25397));
#6115=EDGE_LOOP('',(#25398,#25399,#25400,#25401));
#6116=EDGE_LOOP('',(#25402,#25403,#25404,#25405));
#6117=EDGE_LOOP('',(#25406,#25407,#25408,#25409));
#6118=EDGE_LOOP('',(#25410,#25411,#25412,#25413));
#6119=EDGE_LOOP('',(#25414,#25415,#25416,#25417));
#6120=EDGE_LOOP('',(#25418,#25419,#25420,#25421));
#6121=EDGE_LOOP('',(#25422,#25423,#25424,#25425));
#6122=EDGE_LOOP('',(#25426,#25427,#25428,#25429));
#6123=EDGE_LOOP('',(#25430,#25431,#25432,#25433));
#6124=EDGE_LOOP('',(#25434,#25435,#25436,#25437));
#6125=EDGE_LOOP('',(#25438,#25439,#25440,#25441));
#6126=EDGE_LOOP('',(#25442,#25443,#25444,#25445));
#6127=EDGE_LOOP('',(#25446,#25447,#25448,#25449));
#6128=EDGE_LOOP('',(#25450,#25451,#25452,#25453));
#6129=EDGE_LOOP('',(#25454,#25455,#25456,#25457));
#6130=EDGE_LOOP('',(#25458,#25459,#25460,#25461));
#6131=EDGE_LOOP('',(#25462,#25463,#25464,#25465));
#6132=EDGE_LOOP('',(#25466,#25467,#25468,#25469));
#6133=EDGE_LOOP('',(#25470,#25471,#25472,#25473));
#6134=EDGE_LOOP('',(#25474,#25475,#25476,#25477));
#6135=EDGE_LOOP('',(#25478,#25479,#25480,#25481));
#6136=EDGE_LOOP('',(#25482,#25483,#25484,#25485));
#6137=EDGE_LOOP('',(#25486,#25487,#25488,#25489));
#6138=EDGE_LOOP('',(#25490,#25491,#25492,#25493));
#6139=EDGE_LOOP('',(#25494,#25495,#25496,#25497));
#6140=EDGE_LOOP('',(#25498,#25499,#25500,#25501));
#6141=EDGE_LOOP('',(#25502,#25503,#25504,#25505));
#6142=EDGE_LOOP('',(#25506,#25507,#25508,#25509));
#6143=EDGE_LOOP('',(#25510,#25511,#25512,#25513));
#6144=EDGE_LOOP('',(#25514,#25515,#25516,#25517));
#6145=EDGE_LOOP('',(#25518,#25519,#25520,#25521));
#6146=EDGE_LOOP('',(#25522,#25523,#25524,#25525));
#6147=EDGE_LOOP('',(#25526,#25527,#25528,#25529));
#6148=EDGE_LOOP('',(#25530,#25531,#25532,#25533));
#6149=EDGE_LOOP('',(#25534,#25535,#25536,#25537));
#6150=EDGE_LOOP('',(#25538,#25539,#25540,#25541));
#6151=EDGE_LOOP('',(#25542,#25543,#25544,#25545));
#6152=EDGE_LOOP('',(#25546,#25547,#25548,#25549));
#6153=EDGE_LOOP('',(#25550,#25551,#25552,#25553));
#6154=EDGE_LOOP('',(#25554,#25555,#25556,#25557));
#6155=EDGE_LOOP('',(#25558,#25559,#25560,#25561));
#6156=EDGE_LOOP('',(#25562,#25563,#25564,#25565));
#6157=EDGE_LOOP('',(#25566,#25567,#25568,#25569));
#6158=EDGE_LOOP('',(#25570,#25571,#25572,#25573));
#6159=EDGE_LOOP('',(#25574,#25575,#25576,#25577));
#6160=EDGE_LOOP('',(#25578,#25579,#25580,#25581));
#6161=EDGE_LOOP('',(#25582,#25583,#25584,#25585));
#6162=EDGE_LOOP('',(#25586,#25587,#25588,#25589));
#6163=EDGE_LOOP('',(#25590,#25591,#25592,#25593));
#6164=EDGE_LOOP('',(#25594,#25595,#25596,#25597));
#6165=EDGE_LOOP('',(#25598,#25599,#25600,#25601));
#6166=EDGE_LOOP('',(#25602,#25603,#25604,#25605));
#6167=EDGE_LOOP('',(#25606,#25607,#25608,#25609));
#6168=EDGE_LOOP('',(#25610,#25611,#25612,#25613));
#6169=EDGE_LOOP('',(#25614,#25615,#25616,#25617));
#6170=EDGE_LOOP('',(#25618,#25619,#25620,#25621));
#6171=EDGE_LOOP('',(#25622,#25623,#25624,#25625));
#6172=EDGE_LOOP('',(#25626,#25627,#25628,#25629));
#6173=EDGE_LOOP('',(#25630,#25631,#25632,#25633));
#6174=EDGE_LOOP('',(#25634,#25635,#25636,#25637));
#6175=EDGE_LOOP('',(#25638,#25639,#25640,#25641));
#6176=EDGE_LOOP('',(#25642,#25643,#25644,#25645));
#6177=EDGE_LOOP('',(#25646,#25647,#25648,#25649));
#6178=EDGE_LOOP('',(#25650,#25651,#25652,#25653));
#6179=EDGE_LOOP('',(#25654,#25655,#25656,#25657));
#6180=EDGE_LOOP('',(#25658,#25659,#25660,#25661));
#6181=EDGE_LOOP('',(#25662,#25663,#25664,#25665));
#6182=EDGE_LOOP('',(#25666,#25667,#25668,#25669));
#6183=EDGE_LOOP('',(#25670,#25671,#25672,#25673));
#6184=EDGE_LOOP('',(#25674,#25675,#25676,#25677));
#6185=EDGE_LOOP('',(#25678,#25679,#25680,#25681));
#6186=EDGE_LOOP('',(#25682,#25683,#25684,#25685));
#6187=EDGE_LOOP('',(#25686,#25687,#25688,#25689));
#6188=EDGE_LOOP('',(#25690,#25691,#25692,#25693));
#6189=EDGE_LOOP('',(#25694,#25695,#25696,#25697));
#6190=EDGE_LOOP('',(#25698,#25699,#25700,#25701));
#6191=EDGE_LOOP('',(#25702,#25703,#25704,#25705));
#6192=EDGE_LOOP('',(#25706,#25707,#25708,#25709));
#6193=EDGE_LOOP('',(#25710,#25711,#25712,#25713));
#6194=EDGE_LOOP('',(#25714,#25715,#25716,#25717));
#6195=EDGE_LOOP('',(#25718,#25719,#25720,#25721));
#6196=EDGE_LOOP('',(#25722,#25723,#25724,#25725));
#6197=EDGE_LOOP('',(#25726,#25727,#25728,#25729));
#6198=EDGE_LOOP('',(#25730,#25731,#25732,#25733));
#6199=EDGE_LOOP('',(#25734,#25735,#25736,#25737));
#6200=EDGE_LOOP('',(#25738,#25739,#25740,#25741));
#6201=EDGE_LOOP('',(#25742,#25743,#25744,#25745));
#6202=EDGE_LOOP('',(#25746,#25747,#25748,#25749));
#6203=EDGE_LOOP('',(#25750,#25751,#25752,#25753));
#6204=EDGE_LOOP('',(#25754,#25755,#25756,#25757));
#6205=EDGE_LOOP('',(#25758,#25759,#25760,#25761));
#6206=EDGE_LOOP('',(#25762,#25763,#25764,#25765));
#6207=EDGE_LOOP('',(#25766,#25767,#25768,#25769));
#6208=EDGE_LOOP('',(#25770,#25771,#25772,#25773));
#6209=EDGE_LOOP('',(#25774,#25775,#25776,#25777));
#6210=EDGE_LOOP('',(#25778,#25779,#25780,#25781));
#6211=EDGE_LOOP('',(#25782,#25783,#25784,#25785));
#6212=EDGE_LOOP('',(#25786,#25787,#25788,#25789));
#6213=EDGE_LOOP('',(#25790,#25791,#25792,#25793));
#6214=EDGE_LOOP('',(#25794,#25795,#25796,#25797));
#6215=EDGE_LOOP('',(#25798,#25799,#25800,#25801));
#6216=EDGE_LOOP('',(#25802,#25803,#25804,#25805));
#6217=EDGE_LOOP('',(#25806,#25807,#25808,#25809));
#6218=EDGE_LOOP('',(#25810,#25811,#25812,#25813));
#6219=EDGE_LOOP('',(#25814,#25815,#25816,#25817));
#6220=EDGE_LOOP('',(#25818,#25819,#25820,#25821));
#6221=EDGE_LOOP('',(#25822,#25823,#25824,#25825));
#6222=EDGE_LOOP('',(#25826,#25827,#25828,#25829));
#6223=EDGE_LOOP('',(#25830,#25831,#25832,#25833));
#6224=EDGE_LOOP('',(#25834,#25835,#25836,#25837));
#6225=EDGE_LOOP('',(#25838,#25839,#25840,#25841));
#6226=EDGE_LOOP('',(#25842,#25843,#25844,#25845));
#6227=EDGE_LOOP('',(#25846,#25847,#25848,#25849));
#6228=EDGE_LOOP('',(#25850,#25851,#25852,#25853));
#6229=EDGE_LOOP('',(#25854,#25855,#25856,#25857));
#6230=EDGE_LOOP('',(#25858,#25859,#25860,#25861));
#6231=EDGE_LOOP('',(#25862,#25863,#25864,#25865));
#6232=EDGE_LOOP('',(#25866,#25867,#25868,#25869));
#6233=EDGE_LOOP('',(#25870,#25871,#25872,#25873));
#6234=EDGE_LOOP('',(#25874,#25875,#25876,#25877));
#6235=EDGE_LOOP('',(#25878,#25879,#25880,#25881));
#6236=EDGE_LOOP('',(#25882,#25883,#25884,#25885));
#6237=EDGE_LOOP('',(#25886,#25887,#25888,#25889));
#6238=EDGE_LOOP('',(#25890,#25891,#25892,#25893));
#6239=EDGE_LOOP('',(#25894,#25895,#25896,#25897));
#6240=EDGE_LOOP('',(#25898,#25899,#25900,#25901));
#6241=EDGE_LOOP('',(#25902,#25903,#25904,#25905));
#6242=EDGE_LOOP('',(#25906,#25907,#25908,#25909));
#6243=EDGE_LOOP('',(#25910,#25911,#25912,#25913));
#6244=EDGE_LOOP('',(#25914,#25915,#25916,#25917));
#6245=EDGE_LOOP('',(#25918,#25919,#25920,#25921));
#6246=EDGE_LOOP('',(#25922,#25923,#25924,#25925));
#6247=EDGE_LOOP('',(#25926,#25927,#25928,#25929));
#6248=EDGE_LOOP('',(#25930,#25931,#25932,#25933));
#6249=EDGE_LOOP('',(#25934,#25935,#25936,#25937));
#6250=EDGE_LOOP('',(#25938,#25939,#25940,#25941));
#6251=EDGE_LOOP('',(#25942,#25943,#25944,#25945));
#6252=EDGE_LOOP('',(#25946,#25947,#25948,#25949));
#6253=EDGE_LOOP('',(#25950,#25951,#25952,#25953));
#6254=EDGE_LOOP('',(#25954,#25955,#25956,#25957));
#6255=EDGE_LOOP('',(#25958,#25959,#25960,#25961));
#6256=EDGE_LOOP('',(#25962,#25963,#25964,#25965));
#6257=EDGE_LOOP('',(#25966,#25967,#25968,#25969));
#6258=EDGE_LOOP('',(#25970,#25971,#25972,#25973));
#6259=EDGE_LOOP('',(#25974,#25975,#25976,#25977));
#6260=EDGE_LOOP('',(#25978,#25979,#25980,#25981));
#6261=EDGE_LOOP('',(#25982,#25983,#25984,#25985));
#6262=EDGE_LOOP('',(#25986,#25987,#25988,#25989));
#6263=EDGE_LOOP('',(#25990,#25991,#25992,#25993));
#6264=EDGE_LOOP('',(#25994,#25995,#25996,#25997));
#6265=EDGE_LOOP('',(#25998,#25999,#26000,#26001));
#6266=EDGE_LOOP('',(#26002,#26003,#26004,#26005));
#6267=EDGE_LOOP('',(#26006,#26007,#26008,#26009));
#6268=EDGE_LOOP('',(#26010,#26011,#26012,#26013));
#6269=EDGE_LOOP('',(#26014,#26015,#26016,#26017));
#6270=EDGE_LOOP('',(#26018,#26019,#26020,#26021));
#6271=EDGE_LOOP('',(#26022,#26023,#26024,#26025));
#6272=EDGE_LOOP('',(#26026,#26027,#26028,#26029));
#6273=EDGE_LOOP('',(#26030,#26031,#26032,#26033));
#6274=EDGE_LOOP('',(#26034,#26035,#26036,#26037));
#6275=EDGE_LOOP('',(#26038,#26039,#26040,#26041));
#6276=EDGE_LOOP('',(#26042,#26043,#26044,#26045));
#6277=EDGE_LOOP('',(#26046,#26047,#26048,#26049));
#6278=EDGE_LOOP('',(#26050,#26051,#26052,#26053));
#6279=EDGE_LOOP('',(#26054,#26055,#26056,#26057));
#6280=EDGE_LOOP('',(#26058,#26059,#26060,#26061));
#6281=EDGE_LOOP('',(#26062,#26063,#26064,#26065));
#6282=EDGE_LOOP('',(#26066,#26067,#26068,#26069));
#6283=EDGE_LOOP('',(#26070,#26071,#26072,#26073));
#6284=EDGE_LOOP('',(#26074,#26075,#26076,#26077));
#6285=EDGE_LOOP('',(#26078,#26079,#26080,#26081));
#6286=EDGE_LOOP('',(#26082,#26083,#26084,#26085));
#6287=EDGE_LOOP('',(#26086,#26087,#26088,#26089));
#6288=EDGE_LOOP('',(#26090,#26091,#26092,#26093));
#6289=EDGE_LOOP('',(#26094,#26095,#26096,#26097));
#6290=EDGE_LOOP('',(#26098,#26099,#26100,#26101));
#6291=EDGE_LOOP('',(#26102,#26103,#26104,#26105));
#6292=EDGE_LOOP('',(#26106,#26107,#26108,#26109));
#6293=EDGE_LOOP('',(#26110,#26111,#26112,#26113));
#6294=EDGE_LOOP('',(#26114,#26115,#26116,#26117));
#6295=EDGE_LOOP('',(#26118,#26119,#26120,#26121));
#6296=EDGE_LOOP('',(#26122,#26123,#26124,#26125));
#6297=EDGE_LOOP('',(#26126,#26127,#26128,#26129));
#6298=EDGE_LOOP('',(#26130,#26131,#26132,#26133));
#6299=EDGE_LOOP('',(#26134,#26135,#26136,#26137));
#6300=EDGE_LOOP('',(#26138,#26139,#26140,#26141));
#6301=EDGE_LOOP('',(#26142,#26143,#26144,#26145));
#6302=EDGE_LOOP('',(#26146,#26147,#26148,#26149));
#6303=EDGE_LOOP('',(#26150,#26151,#26152,#26153));
#6304=EDGE_LOOP('',(#26154,#26155,#26156,#26157));
#6305=EDGE_LOOP('',(#26158,#26159,#26160,#26161));
#6306=EDGE_LOOP('',(#26162,#26163,#26164,#26165));
#6307=EDGE_LOOP('',(#26166,#26167,#26168,#26169));
#6308=EDGE_LOOP('',(#26170,#26171,#26172,#26173));
#6309=EDGE_LOOP('',(#26174,#26175,#26176,#26177));
#6310=EDGE_LOOP('',(#26178,#26179,#26180,#26181));
#6311=EDGE_LOOP('',(#26182,#26183,#26184,#26185));
#6312=EDGE_LOOP('',(#26186,#26187,#26188,#26189));
#6313=EDGE_LOOP('',(#26190,#26191,#26192,#26193));
#6314=EDGE_LOOP('',(#26194,#26195,#26196,#26197));
#6315=EDGE_LOOP('',(#26198,#26199,#26200,#26201));
#6316=EDGE_LOOP('',(#26202,#26203,#26204,#26205));
#6317=EDGE_LOOP('',(#26206,#26207,#26208,#26209));
#6318=EDGE_LOOP('',(#26210,#26211,#26212,#26213));
#6319=EDGE_LOOP('',(#26214,#26215,#26216,#26217));
#6320=EDGE_LOOP('',(#26218,#26219,#26220,#26221));
#6321=EDGE_LOOP('',(#26222,#26223,#26224,#26225));
#6322=EDGE_LOOP('',(#26226,#26227,#26228,#26229));
#6323=EDGE_LOOP('',(#26230,#26231,#26232,#26233));
#6324=EDGE_LOOP('',(#26234,#26235,#26236,#26237));
#6325=EDGE_LOOP('',(#26238,#26239,#26240,#26241));
#6326=EDGE_LOOP('',(#26242,#26243,#26244,#26245));
#6327=EDGE_LOOP('',(#26246,#26247,#26248,#26249));
#6328=EDGE_LOOP('',(#26250,#26251,#26252,#26253,#26254,#26255,#26256,#26257));
#6329=EDGE_LOOP('',(#26258,#26259,#26260,#26261,#26262,#26263,#26264,#26265,
#26266,#26267,#26268,#26269));
#6330=EDGE_LOOP('',(#26270,#26271,#26272,#26273,#26274,#26275,#26276,#26277,
#26278,#26279,#26280,#26281,#26282,#26283,#26284,#26285,#26286,#26287,#26288,
#26289,#26290,#26291,#26292,#26293,#26294,#26295,#26296,#26297,#26298,#26299));
#6331=EDGE_LOOP('',(#26300,#26301,#26302,#26303,#26304,#26305,#26306,#26307,
#26308,#26309,#26310,#26311));
#6332=EDGE_LOOP('',(#26312,#26313,#26314,#26315,#26316,#26317,#26318,#26319,
#26320));
#6333=EDGE_LOOP('',(#26321,#26322,#26323,#26324,#26325,#26326,#26327,#26328,
#26329,#26330,#26331,#26332));
#6334=EDGE_LOOP('',(#26333,#26334,#26335,#26336,#26337,#26338,#26339,#26340,
#26341));
#6335=EDGE_LOOP('',(#26342,#26343,#26344,#26345,#26346,#26347,#26348,#26349,
#26350,#26351,#26352,#26353));
#6336=EDGE_LOOP('',(#26354,#26355,#26356,#26357,#26358,#26359,#26360,#26361,
#26362,#26363,#26364,#26365,#26366,#26367,#26368,#26369,#26370,#26371,#26372,
#26373,#26374,#26375,#26376,#26377,#26378,#26379,#26380,#26381,#26382,#26383));
#6337=EDGE_LOOP('',(#26384,#26385,#26386,#26387));
#6338=EDGE_LOOP('',(#26388,#26389,#26390,#26391));
#6339=EDGE_LOOP('',(#26392,#26393,#26394,#26395));
#6340=EDGE_LOOP('',(#26396,#26397,#26398,#26399));
#6341=EDGE_LOOP('',(#26400,#26401,#26402,#26403));
#6342=EDGE_LOOP('',(#26404,#26405,#26406,#26407));
#6343=EDGE_LOOP('',(#26408,#26409,#26410,#26411));
#6344=EDGE_LOOP('',(#26412,#26413,#26414,#26415));
#6345=EDGE_LOOP('',(#26416,#26417,#26418,#26419));
#6346=EDGE_LOOP('',(#26420,#26421,#26422,#26423));
#6347=EDGE_LOOP('',(#26424,#26425,#26426,#26427));
#6348=EDGE_LOOP('',(#26428,#26429,#26430,#26431));
#6349=EDGE_LOOP('',(#26432,#26433,#26434,#26435));
#6350=EDGE_LOOP('',(#26436,#26437,#26438,#26439));
#6351=EDGE_LOOP('',(#26440,#26441,#26442,#26443));
#6352=EDGE_LOOP('',(#26444,#26445,#26446,#26447));
#6353=EDGE_LOOP('',(#26448,#26449,#26450,#26451));
#6354=EDGE_LOOP('',(#26452,#26453,#26454,#26455));
#6355=EDGE_LOOP('',(#26456,#26457,#26458,#26459));
#6356=EDGE_LOOP('',(#26460,#26461,#26462,#26463));
#6357=EDGE_LOOP('',(#26464,#26465,#26466,#26467));
#6358=EDGE_LOOP('',(#26468,#26469,#26470,#26471));
#6359=EDGE_LOOP('',(#26472,#26473,#26474,#26475));
#6360=EDGE_LOOP('',(#26476,#26477,#26478,#26479));
#6361=EDGE_LOOP('',(#26480,#26481,#26482,#26483));
#6362=EDGE_LOOP('',(#26484,#26485,#26486,#26487));
#6363=EDGE_LOOP('',(#26488,#26489,#26490,#26491));
#6364=EDGE_LOOP('',(#26492,#26493,#26494,#26495));
#6365=EDGE_LOOP('',(#26496,#26497,#26498,#26499));
#6366=EDGE_LOOP('',(#26500,#26501,#26502,#26503));
#6367=EDGE_LOOP('',(#26504,#26505,#26506,#26507));
#6368=EDGE_LOOP('',(#26508,#26509,#26510,#26511));
#6369=EDGE_LOOP('',(#26512,#26513,#26514,#26515));
#6370=EDGE_LOOP('',(#26516,#26517,#26518,#26519));
#6371=EDGE_LOOP('',(#26520,#26521,#26522,#26523));
#6372=EDGE_LOOP('',(#26524,#26525,#26526,#26527));
#6373=EDGE_LOOP('',(#26528,#26529,#26530,#26531));
#6374=EDGE_LOOP('',(#26532,#26533,#26534,#26535));
#6375=EDGE_LOOP('',(#26536,#26537,#26538,#26539));
#6376=EDGE_LOOP('',(#26540,#26541,#26542,#26543));
#6377=EDGE_LOOP('',(#26544,#26545,#26546,#26547));
#6378=EDGE_LOOP('',(#26548,#26549,#26550,#26551));
#6379=EDGE_LOOP('',(#26552,#26553,#26554,#26555));
#6380=EDGE_LOOP('',(#26556,#26557,#26558,#26559));
#6381=EDGE_LOOP('',(#26560,#26561,#26562,#26563));
#6382=EDGE_LOOP('',(#26564,#26565,#26566,#26567));
#6383=EDGE_LOOP('',(#26568,#26569,#26570,#26571));
#6384=EDGE_LOOP('',(#26572,#26573,#26574,#26575));
#6385=EDGE_LOOP('',(#26576,#26577,#26578,#26579));
#6386=EDGE_LOOP('',(#26580,#26581,#26582,#26583));
#6387=EDGE_LOOP('',(#26584,#26585,#26586,#26587));
#6388=EDGE_LOOP('',(#26588,#26589,#26590,#26591));
#6389=EDGE_LOOP('',(#26592,#26593,#26594,#26595));
#6390=EDGE_LOOP('',(#26596,#26597,#26598,#26599));
#6391=EDGE_LOOP('',(#26600,#26601,#26602,#26603));
#6392=EDGE_LOOP('',(#26604,#26605,#26606,#26607));
#6393=EDGE_LOOP('',(#26608,#26609,#26610,#26611));
#6394=EDGE_LOOP('',(#26612,#26613,#26614,#26615));
#6395=EDGE_LOOP('',(#26616,#26617,#26618,#26619));
#6396=EDGE_LOOP('',(#26620,#26621,#26622,#26623));
#6397=EDGE_LOOP('',(#26624,#26625,#26626,#26627));
#6398=EDGE_LOOP('',(#26628,#26629,#26630,#26631));
#6399=EDGE_LOOP('',(#26632,#26633,#26634,#26635));
#6400=EDGE_LOOP('',(#26636,#26637,#26638,#26639));
#6401=EDGE_LOOP('',(#26640,#26641,#26642,#26643));
#6402=EDGE_LOOP('',(#26644,#26645,#26646,#26647));
#6403=EDGE_LOOP('',(#26648,#26649,#26650,#26651));
#6404=EDGE_LOOP('',(#26652,#26653,#26654,#26655));
#6405=EDGE_LOOP('',(#26656,#26657,#26658,#26659));
#6406=EDGE_LOOP('',(#26660,#26661,#26662,#26663));
#6407=EDGE_LOOP('',(#26664,#26665,#26666,#26667));
#6408=EDGE_LOOP('',(#26668,#26669,#26670,#26671));
#6409=EDGE_LOOP('',(#26672,#26673,#26674,#26675));
#6410=EDGE_LOOP('',(#26676,#26677,#26678,#26679));
#6411=EDGE_LOOP('',(#26680,#26681,#26682,#26683));
#6412=EDGE_LOOP('',(#26684,#26685,#26686,#26687));
#6413=EDGE_LOOP('',(#26688,#26689,#26690,#26691));
#6414=EDGE_LOOP('',(#26692,#26693,#26694,#26695));
#6415=EDGE_LOOP('',(#26696,#26697,#26698,#26699));
#6416=EDGE_LOOP('',(#26700,#26701,#26702,#26703));
#6417=EDGE_LOOP('',(#26704,#26705,#26706,#26707));
#6418=EDGE_LOOP('',(#26708,#26709,#26710,#26711));
#6419=EDGE_LOOP('',(#26712,#26713,#26714,#26715));
#6420=EDGE_LOOP('',(#26716,#26717,#26718,#26719));
#6421=EDGE_LOOP('',(#26720,#26721,#26722,#26723));
#6422=EDGE_LOOP('',(#26724));
#6423=EDGE_LOOP('',(#26725));
#6424=EDGE_LOOP('',(#26726,#26727,#26728,#26729,#26730,#26731,#26732,#26733,
#26734,#26735,#26736));
#6425=EDGE_LOOP('',(#26737,#26738,#26739,#26740,#26741,#26742,#26743,#26744,
#26745,#26746,#26747,#26748));
#6426=EDGE_LOOP('',(#26749,#26750,#26751,#26752,#26753,#26754,#26755,#26756,
#26757,#26758,#26759,#26760,#26761,#26762,#26763,#26764,#26765,#26766,#26767,
#26768,#26769,#26770));
#6427=EDGE_LOOP('',(#26771,#26772,#26773,#26774,#26775,#26776,#26777,#26778,
#26779,#26780,#26781,#26782));
#6428=EDGE_LOOP('',(#26783,#26784,#26785,#26786,#26787,#26788,#26789,#26790,
#26791,#26792,#26793,#26794));
#6429=EDGE_LOOP('',(#26795,#26796,#26797,#26798,#26799,#26800,#26801,#26802,
#26803,#26804,#26805,#26806,#26807,#26808,#26809,#26810,#26811,#26812,#26813,
#26814,#26815,#26816));
#6430=EDGE_LOOP('',(#26817,#26818,#26819,#26820,#26821,#26822,#26823,#26824,
#26825,#26826,#26827,#26828));
#6431=EDGE_LOOP('',(#26829,#26830,#26831,#26832,#26833,#26834,#26835,#26836,
#26837,#26838,#26839));
#6432=EDGE_LOOP('',(#26840,#26841,#26842,#26843,#26844,#26845,#26846,#26847,
#26848,#26849,#26850,#26851));
#6433=EDGE_LOOP('',(#26852,#26853,#26854,#26855,#26856,#26857,#26858,#26859));
#6434=EDGE_LOOP('',(#26860));
#6435=EDGE_LOOP('',(#26861));
#6436=EDGE_LOOP('',(#26862,#26863,#26864,#26865));
#6437=EDGE_LOOP('',(#26866,#26867,#26868,#26869));
#6438=EDGE_LOOP('',(#26870,#26871,#26872,#26873));
#6439=EDGE_LOOP('',(#26874,#26875,#26876,#26877));
#6440=EDGE_LOOP('',(#26878,#26879,#26880,#26881));
#6441=EDGE_LOOP('',(#26882,#26883,#26884,#26885));
#6442=EDGE_LOOP('',(#26886,#26887,#26888,#26889));
#6443=EDGE_LOOP('',(#26890,#26891,#26892,#26893));
#6444=EDGE_LOOP('',(#26894,#26895,#26896,#26897));
#6445=EDGE_LOOP('',(#26898,#26899,#26900,#26901));
#6446=EDGE_LOOP('',(#26902,#26903,#26904,#26905));
#6447=EDGE_LOOP('',(#26906,#26907,#26908,#26909));
#6448=EDGE_LOOP('',(#26910,#26911,#26912,#26913));
#6449=EDGE_LOOP('',(#26914,#26915,#26916,#26917));
#6450=EDGE_LOOP('',(#26918,#26919,#26920,#26921));
#6451=EDGE_LOOP('',(#26922,#26923,#26924,#26925));
#6452=EDGE_LOOP('',(#26926,#26927,#26928,#26929));
#6453=EDGE_LOOP('',(#26930,#26931,#26932,#26933));
#6454=EDGE_LOOP('',(#26934,#26935,#26936,#26937));
#6455=EDGE_LOOP('',(#26938,#26939,#26940,#26941));
#6456=EDGE_LOOP('',(#26942,#26943,#26944,#26945));
#6457=EDGE_LOOP('',(#26946,#26947,#26948,#26949));
#6458=EDGE_LOOP('',(#26950,#26951,#26952,#26953));
#6459=EDGE_LOOP('',(#26954,#26955,#26956,#26957));
#6460=EDGE_LOOP('',(#26958,#26959,#26960,#26961));
#6461=EDGE_LOOP('',(#26962,#26963,#26964,#26965));
#6462=EDGE_LOOP('',(#26966,#26967,#26968,#26969));
#6463=EDGE_LOOP('',(#26970,#26971,#26972,#26973));
#6464=EDGE_LOOP('',(#26974,#26975,#26976,#26977));
#6465=EDGE_LOOP('',(#26978,#26979,#26980,#26981));
#6466=EDGE_LOOP('',(#26982,#26983,#26984,#26985));
#6467=EDGE_LOOP('',(#26986,#26987,#26988,#26989));
#6468=EDGE_LOOP('',(#26990,#26991,#26992,#26993));
#6469=EDGE_LOOP('',(#26994,#26995,#26996,#26997));
#6470=EDGE_LOOP('',(#26998,#26999,#27000,#27001));
#6471=EDGE_LOOP('',(#27002,#27003,#27004,#27005));
#6472=EDGE_LOOP('',(#27006,#27007,#27008,#27009));
#6473=EDGE_LOOP('',(#27010,#27011,#27012,#27013));
#6474=EDGE_LOOP('',(#27014,#27015,#27016,#27017));
#6475=EDGE_LOOP('',(#27018,#27019,#27020,#27021));
#6476=EDGE_LOOP('',(#27022,#27023,#27024,#27025));
#6477=EDGE_LOOP('',(#27026,#27027,#27028,#27029));
#6478=EDGE_LOOP('',(#27030,#27031,#27032,#27033));
#6479=EDGE_LOOP('',(#27034,#27035,#27036,#27037));
#6480=EDGE_LOOP('',(#27038,#27039,#27040,#27041));
#6481=EDGE_LOOP('',(#27042,#27043,#27044,#27045));
#6482=EDGE_LOOP('',(#27046,#27047,#27048,#27049));
#6483=EDGE_LOOP('',(#27050,#27051,#27052,#27053));
#6484=EDGE_LOOP('',(#27054,#27055,#27056,#27057));
#6485=EDGE_LOOP('',(#27058,#27059,#27060,#27061));
#6486=EDGE_LOOP('',(#27062,#27063,#27064,#27065));
#6487=EDGE_LOOP('',(#27066,#27067,#27068,#27069));
#6488=EDGE_LOOP('',(#27070,#27071,#27072,#27073));
#6489=EDGE_LOOP('',(#27074,#27075,#27076,#27077));
#6490=EDGE_LOOP('',(#27078,#27079,#27080,#27081));
#6491=EDGE_LOOP('',(#27082,#27083,#27084,#27085));
#6492=EDGE_LOOP('',(#27086,#27087,#27088,#27089));
#6493=EDGE_LOOP('',(#27090,#27091,#27092,#27093));
#6494=EDGE_LOOP('',(#27094));
#6495=EDGE_LOOP('',(#27095));
#6496=EDGE_LOOP('',(#27096,#27097,#27098,#27099));
#6497=EDGE_LOOP('',(#27100,#27101,#27102,#27103));
#6498=EDGE_LOOP('',(#27104));
#6499=EDGE_LOOP('',(#27105));
#6500=EDGE_LOOP('',(#27106,#27107,#27108,#27109));
#6501=EDGE_LOOP('',(#27110,#27111,#27112,#27113));
#6502=EDGE_LOOP('',(#27114,#27115,#27116,#27117));
#6503=EDGE_LOOP('',(#27118,#27119,#27120,#27121));
#6504=EDGE_LOOP('',(#27122,#27123,#27124,#27125));
#6505=EDGE_LOOP('',(#27126,#27127,#27128,#27129));
#6506=EDGE_LOOP('',(#27130,#27131,#27132,#27133));
#6507=EDGE_LOOP('',(#27134,#27135,#27136,#27137));
#6508=EDGE_LOOP('',(#27138,#27139,#27140,#27141));
#6509=EDGE_LOOP('',(#27142,#27143,#27144,#27145));
#6510=EDGE_LOOP('',(#27146,#27147,#27148,#27149));
#6511=EDGE_LOOP('',(#27150,#27151,#27152,#27153));
#6512=EDGE_LOOP('',(#27154,#27155,#27156,#27157));
#6513=EDGE_LOOP('',(#27158,#27159,#27160,#27161));
#6514=EDGE_LOOP('',(#27162,#27163,#27164,#27165));
#6515=EDGE_LOOP('',(#27166,#27167,#27168,#27169));
#6516=EDGE_LOOP('',(#27170,#27171,#27172,#27173,#27174,#27175,#27176,#27177));
#6517=EDGE_LOOP('',(#27178,#27179,#27180,#27181,#27182,#27183,#27184,#27185));
#6518=EDGE_LOOP('',(#27186,#27187,#27188,#27189));
#6519=EDGE_LOOP('',(#27190,#27191,#27192,#27193,#27194,#27195,#27196,#27197));
#6520=EDGE_LOOP('',(#27198,#27199,#27200,#27201));
#6521=EDGE_LOOP('',(#27202,#27203,#27204,#27205));
#6522=EDGE_LOOP('',(#27206,#27207,#27208,#27209));
#6523=EDGE_LOOP('',(#27210,#27211,#27212,#27213,#27214,#27215,#27216,#27217,
#27218,#27219,#27220,#27221,#27222,#27223,#27224,#27225));
#6524=EDGE_LOOP('',(#27226,#27227,#27228,#27229));
#6525=EDGE_LOOP('',(#27230,#27231));
#6526=EDGE_LOOP('',(#27232));
#6527=EDGE_LOOP('',(#27233,#27234,#27235,#27236));
#6528=EDGE_LOOP('',(#27237,#27238));
#6529=EDGE_LOOP('',(#27239));
#6530=EDGE_LOOP('',(#27240,#27241,#27242,#27243,#27244,#27245));
#6531=EDGE_LOOP('',(#27246,#27247,#27248,#27249,#27250,#27251));
#6532=EDGE_LOOP('',(#27252,#27253,#27254,#27255,#27256,#27257,#27258,#27259));
#6533=EDGE_LOOP('',(#27260,#27261,#27262,#27263));
#6534=EDGE_LOOP('',(#27264,#27265,#27266,#27267,#27268,#27269));
#6535=EDGE_LOOP('',(#27270,#27271,#27272,#27273));
#6536=EDGE_LOOP('',(#27274,#27275,#27276,#27277));
#6537=EDGE_LOOP('',(#27278,#27279,#27280,#27281));
#6538=EDGE_LOOP('',(#27282,#27283,#27284,#27285,#27286,#27287));
#6539=EDGE_LOOP('',(#27288,#27289,#27290,#27291));
#6540=EDGE_LOOP('',(#27292,#27293,#27294,#27295));
#6541=EDGE_LOOP('',(#27296,#27297,#27298,#27299,#27300,#27301,#27302,#27303,
#27304,#27305,#27306,#27307,#27308,#27309,#27310,#27311,#27312,#27313,#27314,
#27315,#27316,#27317));
#6542=EDGE_LOOP('',(#27318,#27319,#27320,#27321));
#6543=EDGE_LOOP('',(#27322,#27323,#27324,#27325));
#6544=EDGE_LOOP('',(#27326,#27327,#27328,#27329,#27330,#27331,#27332,#27333));
#6545=EDGE_LOOP('',(#27334,#27335,#27336,#27337));
#6546=EDGE_LOOP('',(#27338,#27339,#27340,#27341));
#6547=EDGE_LOOP('',(#27342,#27343,#27344,#27345));
#6548=EDGE_LOOP('',(#27346,#27347,#27348,#27349));
#6549=EDGE_LOOP('',(#27350,#27351,#27352,#27353));
#6550=EDGE_LOOP('',(#27354,#27355,#27356,#27357));
#6551=EDGE_LOOP('',(#27358,#27359,#27360,#27361,#27362,#27363));
#6552=EDGE_LOOP('',(#27364,#27365,#27366,#27367,#27368));
#6553=EDGE_LOOP('',(#27369,#27370,#27371,#27372));
#6554=EDGE_LOOP('',(#27373,#27374,#27375,#27376,#27377));
#6555=EDGE_LOOP('',(#27378,#27379,#27380,#27381,#27382,#27383));
#6556=EDGE_LOOP('',(#27384,#27385,#27386,#27387));
#6557=EDGE_LOOP('',(#27388,#27389,#27390,#27391));
#6558=EDGE_LOOP('',(#27392,#27393,#27394,#27395));
#6559=EDGE_LOOP('',(#27396,#27397,#27398,#27399));
#6560=EDGE_LOOP('',(#27400,#27401,#27402,#27403,#27404));
#6561=EDGE_LOOP('',(#27405,#27406,#27407,#27408));
#6562=EDGE_LOOP('',(#27409,#27410,#27411,#27412));
#6563=EDGE_LOOP('',(#27413,#27414,#27415,#27416,#27417));
#6564=EDGE_LOOP('',(#27418,#27419,#27420,#27421));
#6565=EDGE_LOOP('',(#27422,#27423,#27424,#27425));
#6566=EDGE_LOOP('',(#27426,#27427,#27428,#27429));
#6567=EDGE_LOOP('',(#27430,#27431,#27432,#27433,#27434));
#6568=EDGE_LOOP('',(#27435,#27436,#27437,#27438,#27439,#27440,#27441,#27442,
#27443,#27444,#27445,#27446,#27447,#27448,#27449,#27450,#27451,#27452,#27453,
#27454,#27455,#27456,#27457,#27458,#27459,#27460,#27461));
#6569=EDGE_LOOP('',(#27462,#27463,#27464,#27465,#27466,#27467));
#6570=EDGE_LOOP('',(#27468,#27469,#27470,#27471,#27472,#27473,#27474,#27475,
#27476,#27477,#27478,#27479,#27480,#27481,#27482,#27483,#27484,#27485,#27486,
#27487,#27488,#27489,#27490,#27491,#27492,#27493));
#6571=EDGE_LOOP('',(#27494,#27495,#27496,#27497,#27498,#27499,#27500,#27501,
#27502,#27503,#27504,#27505,#27506,#27507,#27508,#27509,#27510,#27511,#27512,
#27513,#27514));
#6572=EDGE_LOOP('',(#27515,#27516,#27517,#27518));
#6573=EDGE_LOOP('',(#27519,#27520,#27521,#27522));
#6574=EDGE_LOOP('',(#27523,#27524,#27525,#27526));
#6575=EDGE_LOOP('',(#27527,#27528,#27529,#27530));
#6576=EDGE_LOOP('',(#27531,#27532,#27533,#27534));
#6577=EDGE_LOOP('',(#27535,#27536,#27537,#27538));
#6578=EDGE_LOOP('',(#27539,#27540,#27541,#27542,#27543,#27544,#27545,#27546));
#6579=EDGE_LOOP('',(#27547,#27548,#27549,#27550,#27551,#27552,#27553,#27554));
#6580=EDGE_LOOP('',(#27555,#27556,#27557,#27558,#27559,#27560,#27561,#27562));
#6581=EDGE_LOOP('',(#27563,#27564));
#6582=EDGE_LOOP('',(#27565,#27566));
#6583=EDGE_LOOP('',(#27567,#27568));
#6584=EDGE_LOOP('',(#27569,#27570));
#6585=EDGE_LOOP('',(#27571,#27572));
#6586=EDGE_LOOP('',(#27573,#27574));
#6587=EDGE_LOOP('',(#27575,#27576));
#6588=EDGE_LOOP('',(#27577,#27578));
#6589=EDGE_LOOP('',(#27579,#27580));
#6590=EDGE_LOOP('',(#27581,#27582));
#6591=EDGE_LOOP('',(#27583,#27584));
#6592=EDGE_LOOP('',(#27585,#27586));
#6593=EDGE_LOOP('',(#27587,#27588,#27589,#27590,#27591,#27592,#27593,#27594));
#6594=EDGE_LOOP('',(#27595,#27596,#27597,#27598,#27599,#27600,#27601,#27602));
#6595=EDGE_LOOP('',(#27603,#27604,#27605,#27606,#27607,#27608,#27609,#27610));
#6596=EDGE_LOOP('',(#27611,#27612,#27613,#27614,#27615,#27616,#27617,#27618));
#6597=EDGE_LOOP('',(#27619));
#6598=EDGE_LOOP('',(#27620,#27621,#27622,#27623,#27624,#27625,#27626));
#6599=EDGE_LOOP('',(#27627,#27628,#27629,#27630,#27631,#27632,#27633));
#6600=EDGE_LOOP('',(#27634));
#6601=EDGE_LOOP('',(#27635));
#6602=EDGE_LOOP('',(#27636,#27637,#27638,#27639));
#6603=EDGE_LOOP('',(#27640,#27641,#27642,#27643,#27644));
#6604=EDGE_LOOP('',(#27645,#27646,#27647,#27648));
#6605=EDGE_LOOP('',(#27649));
#6606=EDGE_LOOP('',(#27650,#27651,#27652,#27653));
#6607=EDGE_LOOP('',(#27654,#27655,#27656,#27657));
#6608=EDGE_LOOP('',(#27658,#27659,#27660,#27661,#27662));
#6609=EDGE_LOOP('',(#27663,#27664,#27665,#27666));
#6610=EDGE_LOOP('',(#27667));
#6611=EDGE_LOOP('',(#27668,#27669,#27670,#27671));
#6612=EDGE_LOOP('',(#27672,#27673,#27674,#27675));
#6613=EDGE_LOOP('',(#27676,#27677,#27678,#27679,#27680,#27681,#27682,#27683));
#6614=EDGE_LOOP('',(#27684));
#6615=EDGE_LOOP('',(#27685));
#6616=EDGE_LOOP('',(#27686));
#6617=EDGE_LOOP('',(#27687));
#6618=EDGE_LOOP('',(#27688));
#6619=EDGE_LOOP('',(#27689,#27690,#27691,#27692));
#6620=EDGE_LOOP('',(#27693,#27694,#27695,#27696));
#6621=EDGE_LOOP('',(#27697,#27698,#27699,#27700));
#6622=EDGE_LOOP('',(#27701,#27702,#27703));
#6623=EDGE_LOOP('',(#27704,#27705,#27706));
#6624=EDGE_LOOP('',(#27707,#27708,#27709,#27710));
#6625=EDGE_LOOP('',(#27711,#27712,#27713,#27714));
#6626=EDGE_LOOP('',(#27715,#27716,#27717,#27718));
#6627=EDGE_LOOP('',(#27719,#27720,#27721,#27722));
#6628=EDGE_LOOP('',(#27723));
#6629=EDGE_LOOP('',(#27724));
#6630=EDGE_LOOP('',(#27725));
#6631=EDGE_LOOP('',(#27726));
#6632=EDGE_LOOP('',(#27727,#27728,#27729,#27730));
#6633=EDGE_LOOP('',(#27731,#27732,#27733,#27734));
#6634=EDGE_LOOP('',(#27735,#27736,#27737,#27738));
#6635=EDGE_LOOP('',(#27739,#27740,#27741,#27742));
#6636=EDGE_LOOP('',(#27743,#27744,#27745,#27746,#27747,#27748,#27749,#27750));
#6637=EDGE_LOOP('',(#27751));
#6638=EDGE_LOOP('',(#27752));
#6639=EDGE_LOOP('',(#27753));
#6640=EDGE_LOOP('',(#27754,#27755,#27756,#27757));
#6641=EDGE_LOOP('',(#27758,#27759,#27760,#27761));
#6642=EDGE_LOOP('',(#27762,#27763,#27764,#27765));
#6643=EDGE_LOOP('',(#27766,#27767,#27768,#27769));
#6644=EDGE_LOOP('',(#27770,#27771,#27772,#27773));
#6645=EDGE_LOOP('',(#27774,#27775,#27776,#27777));
#6646=EDGE_LOOP('',(#27778,#27779,#27780,#27781));
#6647=EDGE_LOOP('',(#27782,#27783,#27784,#27785));
#6648=EDGE_LOOP('',(#27786,#27787,#27788,#27789));
#6649=EDGE_LOOP('',(#27790,#27791,#27792,#27793));
#6650=EDGE_LOOP('',(#27794,#27795,#27796,#27797,#27798,#27799));
#6651=EDGE_LOOP('',(#27800,#27801,#27802,#27803));
#6652=EDGE_LOOP('',(#27804,#27805,#27806,#27807));
#6653=EDGE_LOOP('',(#27808,#27809,#27810,#27811,#27812,#27813));
#6654=EDGE_LOOP('',(#27814,#27815,#27816,#27817,#27818,#27819));
#6655=EDGE_LOOP('',(#27820,#27821,#27822,#27823));
#6656=EDGE_LOOP('',(#27824,#27825,#27826,#27827));
#6657=EDGE_LOOP('',(#27828,#27829,#27830,#27831,#27832,#27833));
#6658=EDGE_LOOP('',(#27834,#27835,#27836,#27837));
#6659=EDGE_LOOP('',(#27838,#27839,#27840,#27841,#27842,#27843));
#6660=EDGE_LOOP('',(#27844,#27845,#27846,#27847,#27848,#27849));
#6661=EDGE_LOOP('',(#27850,#27851,#27852,#27853));
#6662=EDGE_LOOP('',(#27854,#27855,#27856,#27857));
#6663=EDGE_LOOP('',(#27858,#27859,#27860,#27861,#27862,#27863));
#6664=EDGE_LOOP('',(#27864,#27865,#27866,#27867));
#6665=EDGE_LOOP('',(#27868,#27869,#27870,#27871));
#6666=EDGE_LOOP('',(#27872,#27873,#27874,#27875,#27876,#27877));
#6667=EDGE_LOOP('',(#27878,#27879,#27880,#27881));
#6668=EDGE_LOOP('',(#27882,#27883,#27884,#27885));
#6669=EDGE_LOOP('',(#27886,#27887,#27888,#27889,#27890));
#6670=EDGE_LOOP('',(#27891,#27892,#27893,#27894));
#6671=EDGE_LOOP('',(#27895,#27896,#27897,#27898));
#6672=EDGE_LOOP('',(#27899,#27900,#27901,#27902));
#6673=EDGE_LOOP('',(#27903,#27904,#27905,#27906));
#6674=EDGE_LOOP('',(#27907,#27908,#27909,#27910,#27911));
#6675=EDGE_LOOP('',(#27912,#27913,#27914,#27915,#27916));
#6676=EDGE_LOOP('',(#27917,#27918,#27919,#27920));
#6677=EDGE_LOOP('',(#27921,#27922,#27923,#27924));
#6678=EDGE_LOOP('',(#27925,#27926,#27927,#27928));
#6679=EDGE_LOOP('',(#27929,#27930,#27931,#27932));
#6680=EDGE_LOOP('',(#27933,#27934,#27935,#27936));
#6681=EDGE_LOOP('',(#27937,#27938,#27939,#27940));
#6682=EDGE_LOOP('',(#27941,#27942,#27943,#27944));
#6683=EDGE_LOOP('',(#27945,#27946,#27947,#27948));
#6684=EDGE_LOOP('',(#27949,#27950,#27951,#27952,#27953));
#6685=EDGE_LOOP('',(#27954,#27955,#27956,#27957));
#6686=EDGE_LOOP('',(#27958,#27959,#27960,#27961));
#6687=EDGE_LOOP('',(#27962,#27963,#27964,#27965));
#6688=EDGE_LOOP('',(#27966,#27967,#27968,#27969));
#6689=EDGE_LOOP('',(#27970,#27971,#27972,#27973));
#6690=EDGE_LOOP('',(#27974,#27975,#27976,#27977,#27978));
#6691=EDGE_LOOP('',(#27979,#27980,#27981,#27982));
#6692=EDGE_LOOP('',(#27983,#27984,#27985,#27986));
#6693=EDGE_LOOP('',(#27987,#27988,#27989,#27990,#27991));
#6694=EDGE_LOOP('',(#27992,#27993,#27994,#27995));
#6695=EDGE_LOOP('',(#27996,#27997,#27998,#27999,#28000));
#6696=EDGE_LOOP('',(#28001,#28002,#28003,#28004,#28005,#28006,#28007,#28008,
#28009,#28010,#28011,#28012,#28013,#28014,#28015,#28016,#28017,#28018,#28019,
#28020,#28021,#28022,#28023,#28024,#28025,#28026,#28027,#28028,#28029,#28030,
#28031,#28032,#28033,#28034,#28035,#28036,#28037,#28038,#28039,#28040,#28041,
#28042,#28043,#28044,#28045,#28046,#28047,#28048,#28049,#28050,#28051,#28052,
#28053,#28054,#28055,#28056,#28057,#28058,#28059,#28060,#28061,#28062));
#6697=EDGE_LOOP('',(#28063,#28064,#28065,#28066,#28067));
#6698=EDGE_LOOP('',(#28068,#28069,#28070,#28071,#28072,#28073,#28074,#28075,
#28076,#28077,#28078,#28079,#28080,#28081,#28082,#28083,#28084,#28085,#28086,
#28087,#28088,#28089,#28090,#28091,#28092,#28093,#28094,#28095,#28096,#28097,
#28098,#28099,#28100,#28101,#28102,#28103,#28104,#28105,#28106,#28107,#28108,
#28109,#28110,#28111,#28112,#28113,#28114,#28115,#28116,#28117,#28118,#28119,
#28120,#28121,#28122,#28123,#28124,#28125,#28126,#28127,#28128,#28129));
#6699=EDGE_LOOP('',(#28130,#28131,#28132,#28133,#28134,#28135,#28136));
#6700=EDGE_LOOP('',(#28137));
#6701=EDGE_LOOP('',(#28138));
#6702=EDGE_LOOP('',(#28139,#28140,#28141,#28142,#28143,#28144,#28145));
#6703=EDGE_LOOP('',(#28146));
#6704=EDGE_LOOP('',(#28147,#28148,#28149));
#6705=EDGE_LOOP('',(#28150,#28151,#28152,#28153));
#6706=EDGE_LOOP('',(#28154,#28155,#28156,#28157));
#6707=EDGE_LOOP('',(#28158,#28159,#28160,#28161,#28162,#28163,#28164,#28165,
#28166,#28167,#28168,#28169,#28170,#28171,#28172,#28173,#28174,#28175,#28176,
#28177,#28178,#28179,#28180,#28181,#28182,#28183,#28184,#28185,#28186,#28187,
#28188,#28189,#28190,#28191,#28192,#28193,#28194,#28195,#28196,#28197,#28198,
#28199,#28200,#28201,#28202,#28203,#28204,#28205,#28206,#28207,#28208,#28209,
#28210,#28211,#28212,#28213,#28214,#28215,#28216,#28217,#28218,#28219,#28220,
#28221,#28222,#28223,#28224,#28225,#28226,#28227,#28228,#28229,#28230,#28231,
#28232,#28233,#28234,#28235,#28236,#28237,#28238,#28239,#28240,#28241,#28242,
#28243,#28244,#28245,#28246,#28247,#28248,#28249,#28250,#28251,#28252,#28253,
#28254,#28255,#28256,#28257,#28258,#28259,#28260,#28261,#28262,#28263,#28264,
#28265,#28266,#28267,#28268,#28269,#28270,#28271,#28272,#28273,#28274,#28275,
#28276,#28277,#28278,#28279,#28280,#28281,#28282,#28283,#28284,#28285,#28286,
#28287,#28288,#28289,#28290,#28291,#28292,#28293,#28294,#28295,#28296,#28297,
#28298,#28299,#28300,#28301,#28302,#28303,#28304,#28305,#28306));
#6708=EDGE_LOOP('',(#28307,#28308,#28309,#28310));
#6709=EDGE_LOOP('',(#28311,#28312,#28313,#28314));
#6710=EDGE_LOOP('',(#28315,#28316,#28317));
#6711=EDGE_LOOP('',(#28318,#28319,#28320,#28321,#28322,#28323,#28324,#28325,
#28326,#28327,#28328,#28329,#28330,#28331,#28332,#28333,#28334,#28335,#28336,
#28337,#28338,#28339,#28340,#28341,#28342,#28343,#28344,#28345,#28346,#28347,
#28348,#28349,#28350,#28351,#28352,#28353,#28354,#28355,#28356,#28357,#28358,
#28359,#28360,#28361,#28362,#28363,#28364,#28365,#28366,#28367,#28368,#28369,
#28370,#28371,#28372,#28373,#28374,#28375,#28376,#28377,#28378,#28379,#28380,
#28381,#28382,#28383,#28384,#28385,#28386,#28387,#28388,#28389,#28390,#28391,
#28392,#28393,#28394,#28395,#28396,#28397,#28398,#28399,#28400,#28401,#28402,
#28403,#28404,#28405,#28406,#28407,#28408,#28409,#28410,#28411,#28412,#28413,
#28414,#28415,#28416,#28417,#28418,#28419,#28420,#28421,#28422,#28423,#28424,
#28425,#28426,#28427,#28428));
#6712=EDGE_LOOP('',(#28429,#28430,#28431));
#6713=EDGE_LOOP('',(#28432,#28433,#28434,#28435));
#6714=EDGE_LOOP('',(#28436,#28437,#28438,#28439));
#6715=EDGE_LOOP('',(#28440,#28441,#28442,#28443));
#6716=EDGE_LOOP('',(#28444,#28445,#28446,#28447));
#6717=EDGE_LOOP('',(#28448,#28449,#28450));
#6718=EDGE_LOOP('',(#28451,#28452,#28453));
#6719=EDGE_LOOP('',(#28454,#28455,#28456,#28457));
#6720=EDGE_LOOP('',(#28458,#28459,#28460,#28461));
#6721=EDGE_LOOP('',(#28462,#28463,#28464,#28465));
#6722=EDGE_LOOP('',(#28466,#28467,#28468,#28469));
#6723=EDGE_LOOP('',(#28470,#28471,#28472));
#6724=EDGE_LOOP('',(#28473,#28474,#28475));
#6725=EDGE_LOOP('',(#28476,#28477,#28478,#28479));
#6726=EDGE_LOOP('',(#28480,#28481,#28482,#28483));
#6727=EDGE_LOOP('',(#28484,#28485,#28486,#28487));
#6728=EDGE_LOOP('',(#28488,#28489,#28490,#28491));
#6729=EDGE_LOOP('',(#28492,#28493,#28494));
#6730=EDGE_LOOP('',(#28495,#28496,#28497));
#6731=EDGE_LOOP('',(#28498,#28499,#28500,#28501));
#6732=EDGE_LOOP('',(#28502,#28503,#28504,#28505));
#6733=EDGE_LOOP('',(#28506,#28507,#28508,#28509));
#6734=EDGE_LOOP('',(#28510,#28511,#28512,#28513));
#6735=EDGE_LOOP('',(#28514,#28515,#28516));
#6736=EDGE_LOOP('',(#28517,#28518,#28519));
#6737=EDGE_LOOP('',(#28520,#28521,#28522,#28523));
#6738=EDGE_LOOP('',(#28524,#28525,#28526,#28527));
#6739=EDGE_LOOP('',(#28528,#28529,#28530,#28531));
#6740=EDGE_LOOP('',(#28532,#28533,#28534,#28535));
#6741=EDGE_LOOP('',(#28536,#28537,#28538));
#6742=EDGE_LOOP('',(#28539,#28540,#28541));
#6743=EDGE_LOOP('',(#28542,#28543,#28544,#28545));
#6744=EDGE_LOOP('',(#28546,#28547,#28548,#28549));
#6745=EDGE_LOOP('',(#28550,#28551,#28552,#28553));
#6746=EDGE_LOOP('',(#28554,#28555,#28556,#28557));
#6747=EDGE_LOOP('',(#28558,#28559,#28560));
#6748=EDGE_LOOP('',(#28561,#28562,#28563));
#6749=EDGE_LOOP('',(#28564,#28565,#28566,#28567));
#6750=EDGE_LOOP('',(#28568,#28569,#28570,#28571));
#6751=EDGE_LOOP('',(#28572,#28573,#28574,#28575));
#6752=EDGE_LOOP('',(#28576,#28577,#28578,#28579));
#6753=EDGE_LOOP('',(#28580,#28581,#28582));
#6754=EDGE_LOOP('',(#28583,#28584,#28585));
#6755=EDGE_LOOP('',(#28586,#28587,#28588,#28589));
#6756=EDGE_LOOP('',(#28590,#28591,#28592,#28593));
#6757=EDGE_LOOP('',(#28594,#28595,#28596,#28597));
#6758=EDGE_LOOP('',(#28598,#28599,#28600,#28601));
#6759=EDGE_LOOP('',(#28602,#28603,#28604,#28605));
#6760=EDGE_LOOP('',(#28606,#28607,#28608));
#6761=EDGE_LOOP('',(#28609,#28610,#28611,#28612));
#6762=EDGE_LOOP('',(#28613,#28614,#28615,#28616));
#6763=EDGE_LOOP('',(#28617,#28618,#28619,#28620));
#6764=EDGE_LOOP('',(#28621,#28622,#28623,#28624));
#6765=EDGE_LOOP('',(#28625,#28626,#28627));
#6766=EDGE_LOOP('',(#28628,#28629,#28630));
#6767=EDGE_LOOP('',(#28631,#28632,#28633,#28634));
#6768=EDGE_LOOP('',(#28635,#28636,#28637,#28638));
#6769=EDGE_LOOP('',(#28639,#28640,#28641,#28642));
#6770=EDGE_LOOP('',(#28643,#28644,#28645,#28646));
#6771=EDGE_LOOP('',(#28647,#28648,#28649));
#6772=EDGE_LOOP('',(#28650,#28651,#28652));
#6773=EDGE_LOOP('',(#28653,#28654,#28655,#28656));
#6774=EDGE_LOOP('',(#28657,#28658,#28659,#28660));
#6775=EDGE_LOOP('',(#28661,#28662,#28663,#28664));
#6776=EDGE_LOOP('',(#28665,#28666,#28667,#28668));
#6777=EDGE_LOOP('',(#28669,#28670,#28671));
#6778=EDGE_LOOP('',(#28672,#28673,#28674));
#6779=EDGE_LOOP('',(#28675,#28676,#28677,#28678));
#6780=EDGE_LOOP('',(#28679,#28680,#28681,#28682));
#6781=EDGE_LOOP('',(#28683,#28684,#28685,#28686));
#6782=EDGE_LOOP('',(#28687,#28688,#28689,#28690));
#6783=EDGE_LOOP('',(#28691,#28692,#28693));
#6784=EDGE_LOOP('',(#28694,#28695,#28696));
#6785=EDGE_LOOP('',(#28697,#28698,#28699,#28700));
#6786=EDGE_LOOP('',(#28701,#28702,#28703,#28704));
#6787=EDGE_LOOP('',(#28705,#28706,#28707,#28708));
#6788=EDGE_LOOP('',(#28709,#28710,#28711,#28712));
#6789=EDGE_LOOP('',(#28713,#28714,#28715));
#6790=EDGE_LOOP('',(#28716,#28717,#28718));
#6791=EDGE_LOOP('',(#28719,#28720,#28721,#28722));
#6792=EDGE_LOOP('',(#28723,#28724,#28725,#28726));
#6793=EDGE_LOOP('',(#28727,#28728,#28729,#28730));
#6794=EDGE_LOOP('',(#28731,#28732,#28733,#28734));
#6795=EDGE_LOOP('',(#28735,#28736,#28737));
#6796=EDGE_LOOP('',(#28738,#28739,#28740));
#6797=EDGE_LOOP('',(#28741,#28742,#28743,#28744));
#6798=EDGE_LOOP('',(#28745,#28746,#28747,#28748));
#6799=EDGE_LOOP('',(#28749,#28750,#28751,#28752));
#6800=EDGE_LOOP('',(#28753,#28754,#28755,#28756));
#6801=EDGE_LOOP('',(#28757,#28758,#28759));
#6802=EDGE_LOOP('',(#28760,#28761,#28762));
#6803=EDGE_LOOP('',(#28763,#28764,#28765,#28766));
#6804=EDGE_LOOP('',(#28767,#28768,#28769,#28770));
#6805=EDGE_LOOP('',(#28771,#28772,#28773,#28774));
#6806=EDGE_LOOP('',(#28775,#28776,#28777,#28778));
#6807=EDGE_LOOP('',(#28779,#28780,#28781));
#6808=EDGE_LOOP('',(#28782,#28783,#28784));
#6809=EDGE_LOOP('',(#28785,#28786,#28787,#28788));
#6810=EDGE_LOOP('',(#28789,#28790,#28791,#28792));
#6811=EDGE_LOOP('',(#28793,#28794,#28795,#28796));
#6812=EDGE_LOOP('',(#28797,#28798,#28799,#28800));
#6813=EDGE_LOOP('',(#28801,#28802,#28803));
#6814=EDGE_LOOP('',(#28804,#28805,#28806,#28807,#28808));
#6815=EDGE_LOOP('',(#28809));
#6816=EDGE_LOOP('',(#28810));
#6817=EDGE_LOOP('',(#28811,#28812,#28813,#28814,#28815,#28816,#28817,#28818,
#28819,#28820,#28821,#28822,#28823,#28824,#28825,#28826,#28827,#28828,#28829,
#28830,#28831));
#6818=EDGE_LOOP('',(#28832,#28833,#28834,#28835));
#6819=EDGE_LOOP('',(#28836,#28837,#28838,#28839));
#6820=EDGE_LOOP('',(#28840,#28841,#28842,#28843));
#6821=EDGE_LOOP('',(#28844,#28845,#28846,#28847));
#6822=EDGE_LOOP('',(#28848,#28849,#28850,#28851));
#6823=EDGE_LOOP('',(#28852,#28853,#28854,#28855));
#6824=EDGE_LOOP('',(#28856,#28857,#28858,#28859,#28860,#28861,#28862,#28863));
#6825=EDGE_LOOP('',(#28864,#28865,#28866,#28867,#28868,#28869,#28870,#28871));
#6826=EDGE_LOOP('',(#28872,#28873,#28874,#28875,#28876,#28877,#28878,#28879));
#6827=EDGE_LOOP('',(#28880,#28881));
#6828=EDGE_LOOP('',(#28882,#28883));
#6829=EDGE_LOOP('',(#28884,#28885));
#6830=EDGE_LOOP('',(#28886,#28887));
#6831=EDGE_LOOP('',(#28888,#28889));
#6832=EDGE_LOOP('',(#28890,#28891));
#6833=EDGE_LOOP('',(#28892,#28893));
#6834=EDGE_LOOP('',(#28894,#28895));
#6835=EDGE_LOOP('',(#28896,#28897));
#6836=EDGE_LOOP('',(#28898,#28899));
#6837=EDGE_LOOP('',(#28900,#28901));
#6838=EDGE_LOOP('',(#28902,#28903));
#6839=EDGE_LOOP('',(#28904,#28905,#28906,#28907,#28908,#28909,#28910,#28911));
#6840=EDGE_LOOP('',(#28912,#28913,#28914,#28915,#28916,#28917,#28918,#28919));
#6841=EDGE_LOOP('',(#28920,#28921,#28922,#28923,#28924,#28925,#28926,#28927));
#6842=EDGE_LOOP('',(#28928,#28929,#28930,#28931,#28932,#28933,#28934,#28935));
#6843=EDGE_LOOP('',(#28936,#28937,#28938,#28939));
#6844=EDGE_LOOP('',(#28940,#28941,#28942,#28943));
#6845=EDGE_LOOP('',(#28944,#28945,#28946,#28947));
#6846=EDGE_LOOP('',(#28948,#28949,#28950,#28951,#28952));
#6847=EDGE_LOOP('',(#28953,#28954,#28955,#28956));
#6848=EDGE_LOOP('',(#28957,#28958,#28959,#28960));
#6849=EDGE_LOOP('',(#28961,#28962,#28963,#28964,#28965));
#6850=EDGE_LOOP('',(#28966,#28967,#28968,#28969));
#6851=EDGE_LOOP('',(#28970,#28971,#28972,#28973));
#6852=EDGE_LOOP('',(#28974,#28975,#28976,#28977,#28978));
#6853=EDGE_LOOP('',(#28979,#28980,#28981,#28982));
#6854=EDGE_LOOP('',(#28983,#28984,#28985,#28986));
#6855=EDGE_LOOP('',(#28987,#28988,#28989,#28990));
#6856=EDGE_LOOP('',(#28991,#28992,#28993,#28994));
#6857=EDGE_LOOP('',(#28995,#28996,#28997,#28998));
#6858=EDGE_LOOP('',(#28999,#29000,#29001,#29002,#29003));
#6859=EDGE_LOOP('',(#29004,#29005,#29006,#29007));
#6860=EDGE_LOOP('',(#29008,#29009,#29010,#29011));
#6861=EDGE_LOOP('',(#29012,#29013,#29014,#29015));
#6862=EDGE_LOOP('',(#29016,#29017,#29018,#29019));
#6863=EDGE_LOOP('',(#29020,#29021,#29022,#29023,#29024));
#6864=EDGE_LOOP('',(#29025,#29026,#29027,#29028));
#6865=EDGE_LOOP('',(#29029,#29030,#29031,#29032));
#6866=EDGE_LOOP('',(#29033,#29034,#29035,#29036));
#6867=EDGE_LOOP('',(#29037,#29038,#29039,#29040,#29041));
#6868=EDGE_LOOP('',(#29042,#29043,#29044,#29045));
#6869=EDGE_LOOP('',(#29046,#29047,#29048,#29049));
#6870=EDGE_LOOP('',(#29050,#29051,#29052,#29053));
#6871=EDGE_LOOP('',(#29054,#29055,#29056,#29057));
#6872=EDGE_LOOP('',(#29058,#29059,#29060,#29061));
#6873=EDGE_LOOP('',(#29062,#29063,#29064,#29065));
#6874=EDGE_LOOP('',(#29066,#29067,#29068,#29069));
#6875=EDGE_LOOP('',(#29070,#29071,#29072,#29073));
#6876=EDGE_LOOP('',(#29074,#29075,#29076,#29077,#29078));
#6877=EDGE_LOOP('',(#29079,#29080,#29081,#29082));
#6878=EDGE_LOOP('',(#29083,#29084,#29085,#29086));
#6879=EDGE_LOOP('',(#29087,#29088,#29089,#29090,#29091));
#6880=EDGE_LOOP('',(#29092,#29093,#29094,#29095));
#6881=EDGE_LOOP('',(#29096,#29097,#29098,#29099,#29100));
#6882=EDGE_LOOP('',(#29101,#29102,#29103,#29104));
#6883=EDGE_LOOP('',(#29105,#29106,#29107,#29108,#29109));
#6884=EDGE_LOOP('',(#29110,#29111,#29112,#29113,#29114,#29115,#29116,#29117,
#29118,#29119,#29120,#29121,#29122,#29123,#29124,#29125,#29126,#29127,#29128,
#29129,#29130,#29131,#29132,#29133,#29134,#29135,#29136,#29137,#29138,#29139,
#29140,#29141,#29142,#29143,#29144,#29145,#29146,#29147,#29148,#29149,#29150,
#29151,#29152,#29153,#29154,#29155,#29156,#29157,#29158,#29159));
#6885=EDGE_LOOP('',(#29160,#29161,#29162,#29163,#29164,#29165));
#6886=EDGE_LOOP('',(#29166,#29167,#29168,#29169,#29170,#29171,#29172,#29173,
#29174,#29175,#29176,#29177,#29178,#29179,#29180,#29181,#29182,#29183,#29184,
#29185,#29186,#29187,#29188,#29189,#29190,#29191,#29192,#29193,#29194,#29195,
#29196,#29197,#29198,#29199,#29200,#29201,#29202,#29203,#29204,#29205,#29206,
#29207,#29208,#29209,#29210,#29211));
#6887=EDGE_LOOP('',(#29212,#29213,#29214,#29215,#29216,#29217,#29218));
#6888=EDGE_LOOP('',(#29219));
#6889=EDGE_LOOP('',(#29220));
#6890=EDGE_LOOP('',(#29221,#29222,#29223,#29224,#29225,#29226,#29227));
#6891=EDGE_LOOP('',(#29228));
#6892=EDGE_LOOP('',(#29229,#29230,#29231));
#6893=EDGE_LOOP('',(#29232,#29233,#29234,#29235));
#6894=EDGE_LOOP('',(#29236,#29237,#29238,#29239));
#6895=EDGE_LOOP('',(#29240,#29241,#29242,#29243,#29244,#29245,#29246,#29247,
#29248,#29249,#29250,#29251,#29252,#29253,#29254,#29255,#29256,#29257,#29258,
#29259,#29260,#29261,#29262,#29263,#29264,#29265,#29266,#29267,#29268,#29269,
#29270,#29271,#29272,#29273,#29274,#29275,#29276,#29277,#29278,#29279,#29280,
#29281,#29282,#29283,#29284,#29285,#29286,#29287,#29288,#29289,#29290,#29291,
#29292,#29293,#29294,#29295,#29296,#29297,#29298,#29299,#29300,#29301,#29302,
#29303,#29304,#29305,#29306,#29307,#29308,#29309,#29310,#29311,#29312,#29313,
#29314,#29315,#29316,#29317,#29318,#29319,#29320,#29321,#29322,#29323,#29324,
#29325,#29326,#29327,#29328,#29329,#29330,#29331,#29332,#29333,#29334,#29335,
#29336,#29337,#29338,#29339,#29340,#29341,#29342,#29343,#29344,#29345,#29346,
#29347,#29348,#29349,#29350,#29351,#29352,#29353,#29354,#29355,#29356,#29357,
#29358,#29359,#29360,#29361,#29362,#29363,#29364,#29365,#29366,#29367,#29368,
#29369,#29370,#29371,#29372,#29373,#29374,#29375,#29376,#29377,#29378,#29379,
#29380,#29381,#29382,#29383,#29384,#29385,#29386,#29387,#29388));
#6896=EDGE_LOOP('',(#29389,#29390,#29391,#29392));
#6897=EDGE_LOOP('',(#29393,#29394,#29395,#29396));
#6898=EDGE_LOOP('',(#29397,#29398,#29399));
#6899=EDGE_LOOP('',(#29400,#29401,#29402,#29403,#29404,#29405,#29406,#29407,
#29408,#29409,#29410,#29411,#29412,#29413,#29414,#29415,#29416,#29417,#29418,
#29419,#29420,#29421,#29422,#29423,#29424,#29425,#29426,#29427,#29428,#29429,
#29430,#29431,#29432,#29433,#29434,#29435,#29436,#29437,#29438,#29439,#29440,
#29441,#29442,#29443,#29444,#29445,#29446,#29447,#29448,#29449,#29450,#29451,
#29452,#29453,#29454,#29455,#29456,#29457,#29458,#29459,#29460,#29461,#29462,
#29463,#29464,#29465,#29466,#29467,#29468,#29469,#29470,#29471,#29472,#29473,
#29474,#29475,#29476,#29477,#29478,#29479,#29480,#29481,#29482,#29483,#29484,
#29485,#29486,#29487,#29488,#29489,#29490,#29491,#29492,#29493,#29494,#29495,
#29496,#29497,#29498,#29499,#29500,#29501,#29502,#29503,#29504,#29505,#29506,
#29507,#29508,#29509,#29510));
#6900=EDGE_LOOP('',(#29511,#29512,#29513));
#6901=EDGE_LOOP('',(#29514,#29515,#29516,#29517));
#6902=EDGE_LOOP('',(#29518,#29519,#29520,#29521));
#6903=EDGE_LOOP('',(#29522,#29523,#29524,#29525));
#6904=EDGE_LOOP('',(#29526,#29527,#29528,#29529));
#6905=EDGE_LOOP('',(#29530,#29531,#29532));
#6906=EDGE_LOOP('',(#29533,#29534,#29535));
#6907=EDGE_LOOP('',(#29536,#29537,#29538,#29539));
#6908=EDGE_LOOP('',(#29540,#29541,#29542,#29543));
#6909=EDGE_LOOP('',(#29544,#29545,#29546,#29547));
#6910=EDGE_LOOP('',(#29548,#29549,#29550,#29551));
#6911=EDGE_LOOP('',(#29552,#29553,#29554));
#6912=EDGE_LOOP('',(#29555,#29556,#29557));
#6913=EDGE_LOOP('',(#29558,#29559,#29560,#29561));
#6914=EDGE_LOOP('',(#29562,#29563,#29564,#29565));
#6915=EDGE_LOOP('',(#29566,#29567,#29568,#29569));
#6916=EDGE_LOOP('',(#29570,#29571,#29572,#29573));
#6917=EDGE_LOOP('',(#29574,#29575,#29576));
#6918=EDGE_LOOP('',(#29577,#29578,#29579));
#6919=EDGE_LOOP('',(#29580,#29581,#29582,#29583));
#6920=EDGE_LOOP('',(#29584,#29585,#29586,#29587));
#6921=EDGE_LOOP('',(#29588,#29589,#29590,#29591));
#6922=EDGE_LOOP('',(#29592,#29593,#29594,#29595));
#6923=EDGE_LOOP('',(#29596,#29597,#29598));
#6924=EDGE_LOOP('',(#29599,#29600,#29601));
#6925=EDGE_LOOP('',(#29602,#29603,#29604,#29605));
#6926=EDGE_LOOP('',(#29606,#29607,#29608,#29609));
#6927=EDGE_LOOP('',(#29610,#29611,#29612,#29613));
#6928=EDGE_LOOP('',(#29614,#29615,#29616,#29617));
#6929=EDGE_LOOP('',(#29618,#29619,#29620));
#6930=EDGE_LOOP('',(#29621,#29622,#29623));
#6931=EDGE_LOOP('',(#29624,#29625,#29626,#29627));
#6932=EDGE_LOOP('',(#29628,#29629,#29630,#29631));
#6933=EDGE_LOOP('',(#29632,#29633,#29634,#29635));
#6934=EDGE_LOOP('',(#29636,#29637,#29638,#29639));
#6935=EDGE_LOOP('',(#29640,#29641,#29642));
#6936=EDGE_LOOP('',(#29643,#29644,#29645));
#6937=EDGE_LOOP('',(#29646,#29647,#29648,#29649));
#6938=EDGE_LOOP('',(#29650,#29651,#29652,#29653));
#6939=EDGE_LOOP('',(#29654,#29655,#29656,#29657));
#6940=EDGE_LOOP('',(#29658,#29659,#29660,#29661));
#6941=EDGE_LOOP('',(#29662,#29663,#29664));
#6942=EDGE_LOOP('',(#29665,#29666,#29667));
#6943=EDGE_LOOP('',(#29668,#29669,#29670,#29671));
#6944=EDGE_LOOP('',(#29672,#29673,#29674,#29675));
#6945=EDGE_LOOP('',(#29676,#29677,#29678,#29679));
#6946=EDGE_LOOP('',(#29680,#29681,#29682,#29683));
#6947=EDGE_LOOP('',(#29684,#29685,#29686,#29687));
#6948=EDGE_LOOP('',(#29688,#29689,#29690));
#6949=EDGE_LOOP('',(#29691,#29692,#29693,#29694));
#6950=EDGE_LOOP('',(#29695,#29696,#29697,#29698));
#6951=EDGE_LOOP('',(#29699,#29700,#29701,#29702));
#6952=EDGE_LOOP('',(#29703,#29704,#29705,#29706));
#6953=EDGE_LOOP('',(#29707,#29708,#29709));
#6954=EDGE_LOOP('',(#29710,#29711,#29712));
#6955=EDGE_LOOP('',(#29713,#29714,#29715,#29716));
#6956=EDGE_LOOP('',(#29717,#29718,#29719,#29720));
#6957=EDGE_LOOP('',(#29721,#29722,#29723,#29724));
#6958=EDGE_LOOP('',(#29725,#29726,#29727,#29728));
#6959=EDGE_LOOP('',(#29729,#29730,#29731));
#6960=EDGE_LOOP('',(#29732,#29733,#29734));
#6961=EDGE_LOOP('',(#29735,#29736,#29737,#29738));
#6962=EDGE_LOOP('',(#29739,#29740,#29741,#29742));
#6963=EDGE_LOOP('',(#29743,#29744,#29745,#29746));
#6964=EDGE_LOOP('',(#29747,#29748,#29749,#29750));
#6965=EDGE_LOOP('',(#29751,#29752,#29753));
#6966=EDGE_LOOP('',(#29754,#29755,#29756));
#6967=EDGE_LOOP('',(#29757,#29758,#29759,#29760));
#6968=EDGE_LOOP('',(#29761,#29762,#29763,#29764));
#6969=EDGE_LOOP('',(#29765,#29766,#29767,#29768));
#6970=EDGE_LOOP('',(#29769,#29770,#29771,#29772));
#6971=EDGE_LOOP('',(#29773,#29774,#29775));
#6972=EDGE_LOOP('',(#29776,#29777,#29778));
#6973=EDGE_LOOP('',(#29779,#29780,#29781,#29782));
#6974=EDGE_LOOP('',(#29783,#29784,#29785,#29786));
#6975=EDGE_LOOP('',(#29787,#29788,#29789,#29790));
#6976=EDGE_LOOP('',(#29791,#29792,#29793,#29794));
#6977=EDGE_LOOP('',(#29795,#29796,#29797));
#6978=EDGE_LOOP('',(#29798,#29799,#29800));
#6979=EDGE_LOOP('',(#29801,#29802,#29803,#29804));
#6980=EDGE_LOOP('',(#29805,#29806,#29807,#29808));
#6981=EDGE_LOOP('',(#29809,#29810,#29811,#29812));
#6982=EDGE_LOOP('',(#29813,#29814,#29815,#29816));
#6983=EDGE_LOOP('',(#29817,#29818,#29819));
#6984=EDGE_LOOP('',(#29820,#29821,#29822));
#6985=EDGE_LOOP('',(#29823,#29824,#29825,#29826));
#6986=EDGE_LOOP('',(#29827,#29828,#29829,#29830));
#6987=EDGE_LOOP('',(#29831,#29832,#29833,#29834));
#6988=EDGE_LOOP('',(#29835,#29836,#29837,#29838));
#6989=EDGE_LOOP('',(#29839,#29840,#29841));
#6990=EDGE_LOOP('',(#29842,#29843,#29844));
#6991=EDGE_LOOP('',(#29845,#29846,#29847,#29848));
#6992=EDGE_LOOP('',(#29849,#29850,#29851,#29852));
#6993=EDGE_LOOP('',(#29853,#29854,#29855,#29856));
#6994=EDGE_LOOP('',(#29857,#29858,#29859,#29860));
#6995=EDGE_LOOP('',(#29861,#29862,#29863));
#6996=EDGE_LOOP('',(#29864,#29865,#29866));
#6997=EDGE_LOOP('',(#29867,#29868,#29869,#29870));
#6998=EDGE_LOOP('',(#29871,#29872,#29873,#29874));
#6999=EDGE_LOOP('',(#29875,#29876,#29877,#29878));
#7000=EDGE_LOOP('',(#29879,#29880,#29881,#29882));
#7001=EDGE_LOOP('',(#29883,#29884,#29885));
#7002=EDGE_LOOP('',(#29886,#29887,#29888,#29889,#29890));
#7003=EDGE_LOOP('',(#29891));
#7004=EDGE_LOOP('',(#29892));
#7005=EDGE_LOOP('',(#29893,#29894,#29895,#29896,#29897,#29898,#29899,#29900,
#29901,#29902,#29903,#29904,#29905,#29906,#29907,#29908,#29909,#29910,#29911,
#29912,#29913));
#7006=EDGE_LOOP('',(#29914,#29915,#29916,#29917));
#7007=EDGE_LOOP('',(#29918,#29919,#29920,#29921));
#7008=EDGE_LOOP('',(#29922,#29923,#29924,#29925));
#7009=EDGE_LOOP('',(#29926,#29927,#29928,#29929));
#7010=EDGE_LOOP('',(#29930,#29931,#29932,#29933));
#7011=EDGE_LOOP('',(#29934,#29935,#29936,#29937));
#7012=EDGE_LOOP('',(#29938,#29939,#29940,#29941,#29942,#29943,#29944,#29945));
#7013=EDGE_LOOP('',(#29946,#29947,#29948,#29949,#29950,#29951,#29952,#29953));
#7014=EDGE_LOOP('',(#29954,#29955,#29956,#29957,#29958,#29959,#29960,#29961));
#7015=EDGE_LOOP('',(#29962,#29963));
#7016=EDGE_LOOP('',(#29964,#29965));
#7017=EDGE_LOOP('',(#29966,#29967));
#7018=EDGE_LOOP('',(#29968,#29969));
#7019=EDGE_LOOP('',(#29970,#29971));
#7020=EDGE_LOOP('',(#29972,#29973));
#7021=EDGE_LOOP('',(#29974,#29975));
#7022=EDGE_LOOP('',(#29976,#29977));
#7023=EDGE_LOOP('',(#29978,#29979));
#7024=EDGE_LOOP('',(#29980,#29981));
#7025=EDGE_LOOP('',(#29982,#29983));
#7026=EDGE_LOOP('',(#29984,#29985));
#7027=EDGE_LOOP('',(#29986,#29987,#29988,#29989,#29990,#29991,#29992,#29993));
#7028=EDGE_LOOP('',(#29994,#29995,#29996,#29997,#29998,#29999,#30000,#30001));
#7029=EDGE_LOOP('',(#30002,#30003,#30004,#30005,#30006,#30007,#30008,#30009));
#7030=EDGE_LOOP('',(#30010,#30011,#30012,#30013,#30014,#30015,#30016,#30017));
#7031=EDGE_LOOP('',(#30018,#30019,#30020,#30021));
#7032=EDGE_LOOP('',(#30022,#30023,#30024,#30025));
#7033=EDGE_LOOP('',(#30026,#30027,#30028,#30029));
#7034=EDGE_LOOP('',(#30030,#30031,#30032,#30033));
#7035=EDGE_LOOP('',(#30034,#30035,#30036,#30037));
#7036=EDGE_LOOP('',(#30038,#30039,#30040,#30041));
#7037=EDGE_LOOP('',(#30042,#30043,#30044,#30045));
#7038=EDGE_LOOP('',(#30046,#30047,#30048,#30049));
#7039=EDGE_LOOP('',(#30050,#30051,#30052,#30053));
#7040=EDGE_LOOP('',(#30054,#30055,#30056,#30057));
#7041=EDGE_LOOP('',(#30058,#30059,#30060,#30061));
#7042=EDGE_LOOP('',(#30062,#30063,#30064,#30065));
#7043=EDGE_LOOP('',(#30066,#30067,#30068,#30069,#30070));
#7044=EDGE_LOOP('',(#30071,#30072,#30073,#30074,#30075));
#7045=EDGE_LOOP('',(#30076,#30077,#30078,#30079,#30080));
#7046=EDGE_LOOP('',(#30081,#30082,#30083,#30084,#30085));
#7047=EDGE_LOOP('',(#30086,#30087,#30088,#30089,#30090));
#7048=EDGE_LOOP('',(#30091,#30092,#30093,#30094,#30095));
#7049=EDGE_LOOP('',(#30096,#30097,#30098,#30099,#30100));
#7050=EDGE_LOOP('',(#30101,#30102,#30103,#30104,#30105));
#7051=EDGE_LOOP('',(#30106,#30107,#30108,#30109,#30110));
#7052=EDGE_LOOP('',(#30111,#30112,#30113,#30114,#30115,#30116));
#7053=EDGE_LOOP('',(#30117,#30118,#30119,#30120));
#7054=EDGE_LOOP('',(#30121,#30122,#30123,#30124,#30125,#30126,#30127,#30128,
#30129,#30130,#30131,#30132,#30133,#30134,#30135,#30136,#30137,#30138,#30139,
#30140,#30141,#30142,#30143,#30144,#30145,#30146,#30147,#30148));
#7055=EDGE_LOOP('',(#30149,#30150,#30151,#30152,#30153,#30154));
#7056=EDGE_LOOP('',(#30155,#30156,#30157,#30158,#30159,#30160,#30161,#30162,
#30163,#30164,#30165,#30166,#30167,#30168,#30169,#30170,#30171,#30172,#30173,
#30174,#30175,#30176,#30177,#30178,#30179,#30180,#30181,#30182,#30183,#30184,
#30185,#30186,#30187,#30188,#30189,#30190));
#7057=EDGE_LOOP('',(#30191,#30192,#30193,#30194,#30195,#30196,#30197));
#7058=EDGE_LOOP('',(#30198));
#7059=EDGE_LOOP('',(#30199));
#7060=EDGE_LOOP('',(#30200,#30201,#30202,#30203,#30204));
#7061=EDGE_LOOP('',(#30205,#30206,#30207,#30208,#30209,#30210));
#7062=EDGE_LOOP('',(#30211,#30212,#30213,#30214,#30215,#30216));
#7063=EDGE_LOOP('',(#30217,#30218,#30219,#30220,#30221,#30222,#30223,#30224,
#30225,#30226,#30227,#30228));
#7064=EDGE_LOOP('',(#30229,#30230));
#7065=EDGE_LOOP('',(#30231,#30232));
#7066=EDGE_LOOP('',(#30233,#30234,#30235,#30236));
#7067=EDGE_LOOP('',(#30237));
#7068=EDGE_LOOP('',(#30238,#30239,#30240,#30241,#30242,#30243,#30244,#30245));
#7069=EDGE_LOOP('',(#30246,#30247,#30248,#30249));
#7070=LINE('',#41051,#9907);
#7071=LINE('',#41056,#9908);
#7072=LINE('',#41058,#9909);
#7073=LINE('',#41060,#9910);
#7074=LINE('',#41062,#9911);
#7075=LINE('',#41064,#9912);
#7076=LINE('',#41066,#9913);
#7077=LINE('',#41068,#9914);
#7078=LINE('',#41070,#9915);
#7079=LINE('',#41072,#9916);
#7080=LINE('',#41074,#9917);
#7081=LINE('',#41076,#9918);
#7082=LINE('',#41078,#9919);
#7083=LINE('',#41080,#9920);
#7084=LINE('',#41082,#9921);
#7085=LINE('',#41084,#9922);
#7086=LINE('',#41085,#9923);
#7087=LINE('',#41090,#9924);
#7088=LINE('',#41095,#9925);
#7089=LINE('',#41098,#9926);
#7090=LINE('',#41102,#9927);
#7091=LINE('',#41105,#9928);
#7092=LINE('',#41110,#9929);
#7093=LINE('',#41115,#9930);
#7094=LINE('',#41117,#9931);
#7095=LINE('',#41119,#9932);
#7096=LINE('',#41121,#9933);
#7097=LINE('',#41123,#9934);
#7098=LINE('',#41125,#9935);
#7099=LINE('',#41127,#9936);
#7100=LINE('',#41129,#9937);
#7101=LINE('',#41131,#9938);
#7102=LINE('',#41133,#9939);
#7103=LINE('',#41135,#9940);
#7104=LINE('',#41137,#9941);
#7105=LINE('',#41139,#9942);
#7106=LINE('',#41141,#9943);
#7107=LINE('',#41143,#9944);
#7108=LINE('',#41144,#9945);
#7109=LINE('',#41149,#9946);
#7110=LINE('',#41154,#9947);
#7111=LINE('',#41157,#9948);
#7112=LINE('',#41161,#9949);
#7113=LINE('',#41164,#9950);
#7114=LINE('',#41166,#9951);
#7115=LINE('',#41167,#9952);
#7116=LINE('',#41169,#9953);
#7117=LINE('',#41171,#9954);
#7118=LINE('',#41172,#9955);
#7119=LINE('',#41174,#9956);
#7120=LINE('',#41176,#9957);
#7121=LINE('',#41178,#9958);
#7122=LINE('',#41179,#9959);
#7123=LINE('',#41181,#9960);
#7124=LINE('',#41183,#9961);
#7125=LINE('',#41185,#9962);
#7126=LINE('',#41189,#9963);
#7127=LINE('',#41191,#9964);
#7128=LINE('',#41193,#9965);
#7129=LINE('',#41195,#9966);
#7130=LINE('',#41202,#9967);
#7131=LINE('',#41207,#9968);
#7132=LINE('',#41209,#9969);
#7133=LINE('',#41211,#9970);
#7134=LINE('',#41212,#9971);
#7135=LINE('',#41217,#9972);
#7136=LINE('',#41224,#9973);
#7137=LINE('',#41227,#9974);
#7138=LINE('',#41233,#9975);
#7139=LINE('',#41236,#9976);
#7140=LINE('',#41241,#9977);
#7141=LINE('',#41246,#9978);
#7142=LINE('',#41248,#9979);
#7143=LINE('',#41250,#9980);
#7144=LINE('',#41251,#9981);
#7145=LINE('',#41272,#9982);
#7146=LINE('',#41277,#9983);
#7147=LINE('',#41280,#9984);
#7148=LINE('',#41285,#9985);
#7149=LINE('',#41288,#9986);
#7150=LINE('',#41293,#9987);
#7151=LINE('',#41296,#9988);
#7152=LINE('',#41300,#9989);
#7153=LINE('',#41303,#9990);
#7154=LINE('',#41306,#9991);
#7155=LINE('',#41309,#9992);
#7156=LINE('',#41313,#9993);
#7157=LINE('',#41316,#9994);
#7158=LINE('',#41321,#9995);
#7159=LINE('',#41324,#9996);
#7160=LINE('',#41329,#9997);
#7161=LINE('',#41332,#9998);
#7162=LINE('',#41337,#9999);
#7163=LINE('',#41340,#10000);
#7164=LINE('',#41345,#10001);
#7165=LINE('',#41348,#10002);
#7166=LINE('',#41353,#10003);
#7167=LINE('',#41356,#10004);
#7168=LINE('',#41360,#10005);
#7169=LINE('',#41363,#10006);
#7170=LINE('',#41366,#10007);
#7171=LINE('',#41369,#10008);
#7172=LINE('',#41372,#10009);
#7173=LINE('',#41375,#10010);
#7174=LINE('',#41379,#10011);
#7175=LINE('',#41383,#10012);
#7176=LINE('',#41387,#10013);
#7177=LINE('',#41389,#10014);
#7178=LINE('',#41390,#10015);
#7179=LINE('',#41391,#10016);
#7180=LINE('',#41394,#10017);
#7181=LINE('',#41396,#10018);
#7182=LINE('',#41398,#10019);
#7183=LINE('',#41400,#10020);
#7184=LINE('',#41402,#10021);
#7185=LINE('',#41404,#10022);
#7186=LINE('',#41406,#10023);
#7187=LINE('',#41407,#10024);
#7188=LINE('',#41411,#10025);
#7189=LINE('',#41417,#10026);
#7190=LINE('',#41420,#10027);
#7191=LINE('',#41427,#10028);
#7192=LINE('',#41432,#10029);
#7193=LINE('',#41433,#10030);
#7194=LINE('',#41434,#10031);
#7195=LINE('',#41436,#10032);
#7196=LINE('',#41437,#10033);
#7197=LINE('',#41439,#10034);
#7198=LINE('',#41442,#10035);
#7199=LINE('',#41443,#10036);
#7200=LINE('',#41446,#10037);
#7201=LINE('',#41448,#10038);
#7202=LINE('',#41450,#10039);
#7203=LINE('',#41452,#10040);
#7204=LINE('',#41454,#10041);
#7205=LINE('',#41455,#10042);
#7206=LINE('',#41458,#10043);
#7207=LINE('',#41459,#10044);
#7208=LINE('',#41462,#10045);
#7209=LINE('',#41463,#10046);
#7210=LINE('',#41466,#10047);
#7211=LINE('',#41467,#10048);
#7212=LINE('',#41470,#10049);
#7213=LINE('',#41471,#10050);
#7214=LINE('',#41474,#10051);
#7215=LINE('',#41475,#10052);
#7216=LINE('',#41477,#10053);
#7217=LINE('',#41486,#10054);
#7218=LINE('',#41491,#10055);
#7219=LINE('',#41500,#10056);
#7220=LINE('',#41508,#10057);
#7221=LINE('',#41512,#10058);
#7222=LINE('',#41514,#10059);
#7223=LINE('',#41519,#10060);
#7224=LINE('',#41739,#10061);
#7225=LINE('',#41807,#10062);
#7226=LINE('',#41835,#10063);
#7227=LINE('',#42033,#10064);
#7228=LINE('',#42133,#10065);
#7229=LINE('',#42299,#10066);
#7230=LINE('',#42406,#10067);
#7231=LINE('',#42501,#10068);
#7232=LINE('',#42932,#10069);
#7233=LINE('',#43068,#10070);
#7234=LINE('',#43119,#10071);
#7235=LINE('',#43311,#10072);
#7236=LINE('',#43410,#10073);
#7237=LINE('',#43586,#10074);
#7238=LINE('',#43770,#10075);
#7239=LINE('',#43774,#10076);
#7240=LINE('',#43868,#10077);
#7241=LINE('',#43954,#10078);
#7242=LINE('',#44160,#10079);
#7243=LINE('',#44316,#10080);
#7244=LINE('',#44453,#10081);
#7245=LINE('',#44506,#10082);
#7246=LINE('',#44609,#10083);
#7247=LINE('',#44901,#10084);
#7248=LINE('',#45344,#10085);
#7249=LINE('',#45432,#10086);
#7250=LINE('',#45876,#10087);
#7251=LINE('',#45920,#10088);
#7252=LINE('',#46006,#10089);
#7253=LINE('',#46106,#10090);
#7254=LINE('',#46194,#10091);
#7255=LINE('',#46649,#10092);
#7256=LINE('',#46702,#10093);
#7257=LINE('',#46797,#10094);
#7258=LINE('',#46884,#10095);
#7259=LINE('',#46994,#10096);
#7260=LINE('',#47087,#10097);
#7261=LINE('',#47225,#10098);
#7262=LINE('',#47273,#10099);
#7263=LINE('',#47617,#10100);
#7264=LINE('',#47706,#10101);
#7265=LINE('',#47826,#10102);
#7266=LINE('',#47919,#10103);
#7267=LINE('',#48053,#10104);
#7268=LINE('',#48148,#10105);
#7269=LINE('',#48248,#10106);
#7270=LINE('',#48334,#10107);
#7271=LINE('',#48434,#10108);
#7272=LINE('',#48533,#10109);
#7273=LINE('',#48558,#10110);
#7274=LINE('',#48690,#10111);
#7275=LINE('',#48695,#10112);
#7276=LINE('',#48697,#10113);
#7277=LINE('',#48698,#10114);
#7278=LINE('',#48701,#10115);
#7279=LINE('',#48703,#10116);
#7280=LINE('',#48704,#10117);
#7281=LINE('',#49679,#10118);
#7282=LINE('',#56338,#10119);
#7283=LINE('',#66015,#10120);
#7284=LINE('',#68988,#10121);
#7285=LINE('',#68992,#10122);
#7286=LINE('',#68996,#10123);
#7287=LINE('',#69004,#10124);
#7288=LINE('',#69007,#10125);
#7289=LINE('',#69091,#10126);
#7290=LINE('',#69139,#10127);
#7291=LINE('',#69141,#10128);
#7292=LINE('',#69142,#10129);
#7293=LINE('',#69145,#10130);
#7294=LINE('',#69146,#10131);
#7295=LINE('',#69149,#10132);
#7296=LINE('',#69151,#10133);
#7297=LINE('',#69152,#10134);
#7298=LINE('',#69155,#10135);
#7299=LINE('',#69157,#10136);
#7300=LINE('',#69158,#10137);
#7301=LINE('',#69161,#10138);
#7302=LINE('',#69162,#10139);
#7303=LINE('',#69165,#10140);
#7304=LINE('',#69166,#10141);
#7305=LINE('',#69169,#10142);
#7306=LINE('',#69171,#10143);
#7307=LINE('',#69172,#10144);
#7308=LINE('',#69175,#10145);
#7309=LINE('',#69177,#10146);
#7310=LINE('',#69178,#10147);
#7311=LINE('',#69181,#10148);
#7312=LINE('',#69182,#10149);
#7313=LINE('',#69185,#10150);
#7314=LINE('',#69186,#10151);
#7315=LINE('',#69194,#10152);
#7316=LINE('',#69196,#10153);
#7317=LINE('',#69198,#10154);
#7318=LINE('',#69199,#10155);
#7319=LINE('',#69203,#10156);
#7320=LINE('',#69206,#10157);
#7321=LINE('',#69207,#10158);
#7322=LINE('',#69213,#10159);
#7323=LINE('',#69215,#10160);
#7324=LINE('',#69217,#10161);
#7325=LINE('',#69218,#10162);
#7326=LINE('',#69222,#10163);
#7327=LINE('',#69225,#10164);
#7328=LINE('',#69226,#10165);
#7329=LINE('',#69232,#10166);
#7330=LINE('',#69234,#10167);
#7331=LINE('',#69236,#10168);
#7332=LINE('',#69237,#10169);
#7333=LINE('',#69241,#10170);
#7334=LINE('',#69244,#10171);
#7335=LINE('',#69245,#10172);
#7336=LINE('',#69251,#10173);
#7337=LINE('',#69253,#10174);
#7338=LINE('',#69255,#10175);
#7339=LINE('',#69256,#10176);
#7340=LINE('',#69260,#10177);
#7341=LINE('',#69263,#10178);
#7342=LINE('',#69264,#10179);
#7343=LINE('',#69270,#10180);
#7344=LINE('',#69272,#10181);
#7345=LINE('',#69274,#10182);
#7346=LINE('',#69275,#10183);
#7347=LINE('',#69279,#10184);
#7348=LINE('',#69282,#10185);
#7349=LINE('',#69283,#10186);
#7350=LINE('',#69289,#10187);
#7351=LINE('',#69291,#10188);
#7352=LINE('',#69293,#10189);
#7353=LINE('',#69294,#10190);
#7354=LINE('',#69298,#10191);
#7355=LINE('',#69301,#10192);
#7356=LINE('',#69302,#10193);
#7357=LINE('',#69308,#10194);
#7358=LINE('',#69310,#10195);
#7359=LINE('',#69312,#10196);
#7360=LINE('',#69313,#10197);
#7361=LINE('',#69317,#10198);
#7362=LINE('',#69320,#10199);
#7363=LINE('',#69321,#10200);
#7364=LINE('',#69327,#10201);
#7365=LINE('',#69329,#10202);
#7366=LINE('',#69331,#10203);
#7367=LINE('',#69332,#10204);
#7368=LINE('',#69336,#10205);
#7369=LINE('',#69339,#10206);
#7370=LINE('',#69340,#10207);
#7371=LINE('',#69346,#10208);
#7372=LINE('',#69348,#10209);
#7373=LINE('',#69350,#10210);
#7374=LINE('',#69351,#10211);
#7375=LINE('',#69355,#10212);
#7376=LINE('',#69358,#10213);
#7377=LINE('',#69359,#10214);
#7378=LINE('',#69365,#10215);
#7379=LINE('',#69367,#10216);
#7380=LINE('',#69369,#10217);
#7381=LINE('',#69370,#10218);
#7382=LINE('',#69374,#10219);
#7383=LINE('',#69377,#10220);
#7384=LINE('',#69378,#10221);
#7385=LINE('',#69384,#10222);
#7386=LINE('',#69386,#10223);
#7387=LINE('',#69388,#10224);
#7388=LINE('',#69389,#10225);
#7389=LINE('',#69393,#10226);
#7390=LINE('',#69396,#10227);
#7391=LINE('',#69397,#10228);
#7392=LINE('',#69403,#10229);
#7393=LINE('',#69405,#10230);
#7394=LINE('',#69407,#10231);
#7395=LINE('',#69408,#10232);
#7396=LINE('',#69412,#10233);
#7397=LINE('',#69415,#10234);
#7398=LINE('',#69416,#10235);
#7399=LINE('',#69422,#10236);
#7400=LINE('',#69424,#10237);
#7401=LINE('',#69426,#10238);
#7402=LINE('',#69427,#10239);
#7403=LINE('',#69431,#10240);
#7404=LINE('',#69434,#10241);
#7405=LINE('',#69435,#10242);
#7406=LINE('',#69441,#10243);
#7407=LINE('',#69443,#10244);
#7408=LINE('',#69445,#10245);
#7409=LINE('',#69446,#10246);
#7410=LINE('',#69450,#10247);
#7411=LINE('',#69453,#10248);
#7412=LINE('',#69454,#10249);
#7413=LINE('',#69460,#10250);
#7414=LINE('',#69462,#10251);
#7415=LINE('',#69464,#10252);
#7416=LINE('',#69465,#10253);
#7417=LINE('',#69469,#10254);
#7418=LINE('',#69472,#10255);
#7419=LINE('',#69473,#10256);
#7420=LINE('',#69479,#10257);
#7421=LINE('',#69481,#10258);
#7422=LINE('',#69483,#10259);
#7423=LINE('',#69484,#10260);
#7424=LINE('',#69488,#10261);
#7425=LINE('',#69491,#10262);
#7426=LINE('',#69492,#10263);
#7427=LINE('',#69498,#10264);
#7428=LINE('',#69500,#10265);
#7429=LINE('',#69502,#10266);
#7430=LINE('',#69503,#10267);
#7431=LINE('',#69507,#10268);
#7432=LINE('',#69510,#10269);
#7433=LINE('',#69511,#10270);
#7434=LINE('',#69517,#10271);
#7435=LINE('',#69519,#10272);
#7436=LINE('',#69521,#10273);
#7437=LINE('',#69522,#10274);
#7438=LINE('',#69526,#10275);
#7439=LINE('',#69529,#10276);
#7440=LINE('',#69530,#10277);
#7441=LINE('',#69536,#10278);
#7442=LINE('',#69538,#10279);
#7443=LINE('',#69540,#10280);
#7444=LINE('',#69541,#10281);
#7445=LINE('',#69546,#10282);
#7446=LINE('',#69550,#10283);
#7447=LINE('',#69551,#10284);
#7448=LINE('',#69559,#10285);
#7449=LINE('',#69561,#10286);
#7450=LINE('',#69563,#10287);
#7451=LINE('',#69564,#10288);
#7452=LINE('',#69568,#10289);
#7453=LINE('',#69571,#10290);
#7454=LINE('',#69572,#10291);
#7455=LINE('',#69578,#10292);
#7456=LINE('',#69580,#10293);
#7457=LINE('',#69582,#10294);
#7458=LINE('',#69583,#10295);
#7459=LINE('',#69587,#10296);
#7460=LINE('',#69590,#10297);
#7461=LINE('',#69591,#10298);
#7462=LINE('',#69597,#10299);
#7463=LINE('',#69599,#10300);
#7464=LINE('',#69601,#10301);
#7465=LINE('',#69602,#10302);
#7466=LINE('',#69606,#10303);
#7467=LINE('',#69609,#10304);
#7468=LINE('',#69610,#10305);
#7469=LINE('',#69616,#10306);
#7470=LINE('',#69618,#10307);
#7471=LINE('',#69620,#10308);
#7472=LINE('',#69621,#10309);
#7473=LINE('',#69625,#10310);
#7474=LINE('',#69628,#10311);
#7475=LINE('',#69629,#10312);
#7476=LINE('',#69635,#10313);
#7477=LINE('',#69637,#10314);
#7478=LINE('',#69639,#10315);
#7479=LINE('',#69640,#10316);
#7480=LINE('',#69644,#10317);
#7481=LINE('',#69647,#10318);
#7482=LINE('',#69648,#10319);
#7483=LINE('',#69654,#10320);
#7484=LINE('',#69656,#10321);
#7485=LINE('',#69658,#10322);
#7486=LINE('',#69659,#10323);
#7487=LINE('',#69663,#10324);
#7488=LINE('',#69666,#10325);
#7489=LINE('',#69667,#10326);
#7490=LINE('',#69673,#10327);
#7491=LINE('',#69675,#10328);
#7492=LINE('',#69677,#10329);
#7493=LINE('',#69678,#10330);
#7494=LINE('',#69682,#10331);
#7495=LINE('',#69685,#10332);
#7496=LINE('',#69686,#10333);
#7497=LINE('',#69692,#10334);
#7498=LINE('',#69694,#10335);
#7499=LINE('',#69696,#10336);
#7500=LINE('',#69697,#10337);
#7501=LINE('',#69701,#10338);
#7502=LINE('',#69704,#10339);
#7503=LINE('',#69705,#10340);
#7504=LINE('',#69711,#10341);
#7505=LINE('',#69713,#10342);
#7506=LINE('',#69715,#10343);
#7507=LINE('',#69716,#10344);
#7508=LINE('',#69720,#10345);
#7509=LINE('',#69723,#10346);
#7510=LINE('',#69724,#10347);
#7511=LINE('',#69730,#10348);
#7512=LINE('',#69732,#10349);
#7513=LINE('',#69734,#10350);
#7514=LINE('',#69735,#10351);
#7515=LINE('',#69739,#10352);
#7516=LINE('',#69742,#10353);
#7517=LINE('',#69743,#10354);
#7518=LINE('',#69749,#10355);
#7519=LINE('',#69751,#10356);
#7520=LINE('',#69753,#10357);
#7521=LINE('',#69754,#10358);
#7522=LINE('',#69758,#10359);
#7523=LINE('',#69761,#10360);
#7524=LINE('',#69762,#10361);
#7525=LINE('',#69768,#10362);
#7526=LINE('',#69770,#10363);
#7527=LINE('',#69772,#10364);
#7528=LINE('',#69773,#10365);
#7529=LINE('',#69777,#10366);
#7530=LINE('',#69780,#10367);
#7531=LINE('',#69781,#10368);
#7532=LINE('',#69787,#10369);
#7533=LINE('',#69789,#10370);
#7534=LINE('',#69791,#10371);
#7535=LINE('',#69792,#10372);
#7536=LINE('',#69796,#10373);
#7537=LINE('',#69799,#10374);
#7538=LINE('',#69800,#10375);
#7539=LINE('',#69806,#10376);
#7540=LINE('',#69808,#10377);
#7541=LINE('',#69810,#10378);
#7542=LINE('',#69811,#10379);
#7543=LINE('',#69815,#10380);
#7544=LINE('',#69818,#10381);
#7545=LINE('',#69819,#10382);
#7546=LINE('',#69825,#10383);
#7547=LINE('',#69827,#10384);
#7548=LINE('',#69829,#10385);
#7549=LINE('',#69830,#10386);
#7550=LINE('',#69834,#10387);
#7551=LINE('',#69837,#10388);
#7552=LINE('',#69838,#10389);
#7553=LINE('',#69844,#10390);
#7554=LINE('',#69846,#10391);
#7555=LINE('',#69848,#10392);
#7556=LINE('',#69849,#10393);
#7557=LINE('',#69853,#10394);
#7558=LINE('',#69856,#10395);
#7559=LINE('',#69857,#10396);
#7560=LINE('',#69863,#10397);
#7561=LINE('',#69865,#10398);
#7562=LINE('',#69867,#10399);
#7563=LINE('',#69868,#10400);
#7564=LINE('',#69872,#10401);
#7565=LINE('',#69875,#10402);
#7566=LINE('',#69876,#10403);
#7567=LINE('',#69882,#10404);
#7568=LINE('',#69884,#10405);
#7569=LINE('',#69886,#10406);
#7570=LINE('',#69887,#10407);
#7571=LINE('',#69891,#10408);
#7572=LINE('',#69894,#10409);
#7573=LINE('',#69895,#10410);
#7574=LINE('',#69900,#10411);
#7575=LINE('',#69902,#10412);
#7576=LINE('',#69903,#10413);
#7577=LINE('',#69908,#10414);
#7578=LINE('',#69909,#10415);
#7579=LINE('',#69920,#10416);
#7580=LINE('',#69928,#10417);
#7581=LINE('',#69932,#10418);
#7582=LINE('',#69933,#10419);
#7583=LINE('',#69936,#10420);
#7584=LINE('',#69944,#10421);
#7585=LINE('',#69949,#10422);
#7586=LINE('',#69963,#10423);
#7587=LINE('',#69968,#10424);
#7588=LINE('',#69980,#10425);
#7589=LINE('',#69995,#10426);
#7590=LINE('',#70010,#10427);
#7591=LINE('',#70025,#10428);
#7592=LINE('',#70040,#10429);
#7593=LINE('',#70055,#10430);
#7594=LINE('',#70083,#10431);
#7595=LINE('',#70088,#10432);
#7596=LINE('',#70100,#10433);
#7597=LINE('',#70115,#10434);
#7598=LINE('',#70130,#10435);
#7599=LINE('',#70145,#10436);
#7600=LINE('',#70160,#10437);
#7601=LINE('',#70175,#10438);
#7602=LINE('',#70190,#10439);
#7603=LINE('',#70205,#10440);
#7604=LINE('',#70220,#10441);
#7605=LINE('',#70235,#10442);
#7606=LINE('',#70255,#10443);
#7607=LINE('',#70257,#10444);
#7608=LINE('',#70259,#10445);
#7609=LINE('',#70260,#10446);
#7610=LINE('',#70263,#10447);
#7611=LINE('',#70265,#10448);
#7612=LINE('',#70266,#10449);
#7613=LINE('',#70268,#10450);
#7614=LINE('',#70269,#10451);
#7615=LINE('',#70273,#10452);
#7616=LINE('',#70275,#10453);
#7617=LINE('',#70277,#10454);
#7618=LINE('',#70278,#10455);
#7619=LINE('',#70281,#10456);
#7620=LINE('',#70283,#10457);
#7621=LINE('',#70284,#10458);
#7622=LINE('',#70287,#10459);
#7623=LINE('',#70289,#10460);
#7624=LINE('',#70290,#10461);
#7625=LINE('',#70293,#10462);
#7626=LINE('',#70295,#10463);
#7627=LINE('',#70296,#10464);
#7628=LINE('',#70299,#10465);
#7629=LINE('',#70301,#10466);
#7630=LINE('',#70302,#10467);
#7631=LINE('',#70305,#10468);
#7632=LINE('',#70307,#10469);
#7633=LINE('',#70308,#10470);
#7634=LINE('',#70311,#10471);
#7635=LINE('',#70313,#10472);
#7636=LINE('',#70314,#10473);
#7637=LINE('',#70317,#10474);
#7638=LINE('',#70319,#10475);
#7639=LINE('',#70320,#10476);
#7640=LINE('',#70323,#10477);
#7641=LINE('',#70325,#10478);
#7642=LINE('',#70326,#10479);
#7643=LINE('',#70329,#10480);
#7644=LINE('',#70331,#10481);
#7645=LINE('',#70332,#10482);
#7646=LINE('',#70334,#10483);
#7647=LINE('',#70335,#10484);
#7648=LINE('',#70351,#10485);
#7649=LINE('',#70356,#10486);
#7650=LINE('',#70368,#10487);
#7651=LINE('',#70383,#10488);
#7652=LINE('',#70398,#10489);
#7653=LINE('',#70413,#10490);
#7654=LINE('',#70428,#10491);
#7655=LINE('',#70443,#10492);
#7656=LINE('',#70471,#10493);
#7657=LINE('',#70476,#10494);
#7658=LINE('',#70488,#10495);
#7659=LINE('',#70503,#10496);
#7660=LINE('',#70518,#10497);
#7661=LINE('',#70533,#10498);
#7662=LINE('',#70548,#10499);
#7663=LINE('',#70563,#10500);
#7664=LINE('',#70578,#10501);
#7665=LINE('',#70593,#10502);
#7666=LINE('',#70608,#10503);
#7667=LINE('',#70623,#10504);
#7668=LINE('',#70652,#10505);
#7669=LINE('',#70657,#10506);
#7670=LINE('',#70669,#10507);
#7671=LINE('',#70684,#10508);
#7672=LINE('',#70699,#10509);
#7673=LINE('',#70714,#10510);
#7674=LINE('',#70729,#10511);
#7675=LINE('',#70744,#10512);
#7676=LINE('',#70759,#10513);
#7677=LINE('',#70774,#10514);
#7678=LINE('',#70789,#10515);
#7679=LINE('',#70804,#10516);
#7680=LINE('',#70819,#10517);
#7681=LINE('',#70825,#10518);
#7682=LINE('',#70827,#10519);
#7683=LINE('',#70828,#10520);
#7684=LINE('',#70840,#10521);
#7685=LINE('',#70855,#10522);
#7686=LINE('',#70870,#10523);
#7687=LINE('',#70885,#10524);
#7688=LINE('',#70900,#10525);
#7689=LINE('',#70915,#10526);
#7690=LINE('',#70930,#10527);
#7691=LINE('',#70936,#10528);
#7692=LINE('',#70938,#10529);
#7693=LINE('',#70939,#10530);
#7694=LINE('',#70951,#10531);
#7695=LINE('',#70966,#10532);
#7696=LINE('',#70981,#10533);
#7697=LINE('',#70996,#10534);
#7698=LINE('',#71011,#10535);
#7699=LINE('',#71026,#10536);
#7700=LINE('',#71041,#10537);
#7701=LINE('',#71047,#10538);
#7702=LINE('',#71049,#10539);
#7703=LINE('',#71050,#10540);
#7704=LINE('',#71077,#10541);
#7705=LINE('',#71082,#10542);
#7706=LINE('',#71094,#10543);
#7707=LINE('',#71109,#10544);
#7708=LINE('',#71124,#10545);
#7709=LINE('',#71139,#10546);
#7710=LINE('',#71154,#10547);
#7711=LINE('',#71169,#10548);
#7712=LINE('',#71197,#10549);
#7713=LINE('',#71202,#10550);
#7714=LINE('',#71214,#10551);
#7715=LINE('',#71229,#10552);
#7716=LINE('',#71244,#10553);
#7717=LINE('',#71259,#10554);
#7718=LINE('',#71274,#10555);
#7719=LINE('',#71289,#10556);
#7720=LINE('',#71304,#10557);
#7721=LINE('',#71319,#10558);
#7722=LINE('',#71334,#10559);
#7723=LINE('',#71349,#10560);
#7724=LINE('',#71378,#10561);
#7725=LINE('',#71383,#10562);
#7726=LINE('',#71395,#10563);
#7727=LINE('',#71410,#10564);
#7728=LINE('',#71425,#10565);
#7729=LINE('',#71440,#10566);
#7730=LINE('',#71455,#10567);
#7731=LINE('',#71470,#10568);
#7732=LINE('',#71485,#10569);
#7733=LINE('',#71500,#10570);
#7734=LINE('',#71506,#10571);
#7735=LINE('',#71508,#10572);
#7736=LINE('',#71509,#10573);
#7737=LINE('',#71521,#10574);
#7738=LINE('',#71536,#10575);
#7739=LINE('',#71551,#10576);
#7740=LINE('',#71566,#10577);
#7741=LINE('',#71581,#10578);
#7742=LINE('',#71596,#10579);
#7743=LINE('',#71611,#10580);
#7744=LINE('',#71626,#10581);
#7745=LINE('',#71641,#10582);
#7746=LINE('',#71647,#10583);
#7747=LINE('',#71649,#10584);
#7748=LINE('',#71650,#10585);
#7749=LINE('',#71653,#10586);
#7750=LINE('',#71655,#10587);
#7751=LINE('',#71656,#10588);
#7752=LINE('',#71658,#10589);
#7753=LINE('',#71659,#10590);
#7754=LINE('',#71674,#10591);
#7755=LINE('',#71679,#10592);
#7756=LINE('',#71691,#10593);
#7757=LINE('',#71706,#10594);
#7758=LINE('',#71721,#10595);
#7759=LINE('',#71736,#10596);
#7760=LINE('',#71751,#10597);
#7761=LINE('',#71766,#10598);
#7762=LINE('',#71794,#10599);
#7763=LINE('',#71799,#10600);
#7764=LINE('',#71811,#10601);
#7765=LINE('',#71826,#10602);
#7766=LINE('',#71841,#10603);
#7767=LINE('',#71856,#10604);
#7768=LINE('',#71871,#10605);
#7769=LINE('',#71886,#10606);
#7770=LINE('',#71901,#10607);
#7771=LINE('',#71916,#10608);
#7772=LINE('',#71931,#10609);
#7773=LINE('',#71946,#10610);
#7774=LINE('',#71966,#10611);
#7775=LINE('',#71968,#10612);
#7776=LINE('',#71970,#10613);
#7777=LINE('',#71971,#10614);
#7778=LINE('',#71983,#10615);
#7779=LINE('',#71998,#10616);
#7780=LINE('',#72004,#10617);
#7781=LINE('',#72006,#10618);
#7782=LINE('',#72007,#10619);
#7783=LINE('',#72019,#10620);
#7784=LINE('',#72034,#10621);
#7785=LINE('',#72040,#10622);
#7786=LINE('',#72042,#10623);
#7787=LINE('',#72043,#10624);
#7788=LINE('',#72046,#10625);
#7789=LINE('',#72048,#10626);
#7790=LINE('',#72049,#10627);
#7791=LINE('',#72051,#10628);
#7792=LINE('',#72052,#10629);
#7793=LINE('',#72067,#10630);
#7794=LINE('',#72072,#10631);
#7795=LINE('',#72084,#10632);
#7796=LINE('',#72099,#10633);
#7797=LINE('',#72114,#10634);
#7798=LINE('',#72129,#10635);
#7799=LINE('',#72144,#10636);
#7800=LINE('',#72159,#10637);
#7801=LINE('',#72187,#10638);
#7802=LINE('',#72192,#10639);
#7803=LINE('',#72204,#10640);
#7804=LINE('',#72219,#10641);
#7805=LINE('',#72234,#10642);
#7806=LINE('',#72249,#10643);
#7807=LINE('',#72264,#10644);
#7808=LINE('',#72279,#10645);
#7809=LINE('',#72294,#10646);
#7810=LINE('',#72309,#10647);
#7811=LINE('',#72324,#10648);
#7812=LINE('',#72339,#10649);
#7813=LINE('',#72369,#10650);
#7814=LINE('',#72374,#10651);
#7815=LINE('',#72386,#10652);
#7816=LINE('',#72401,#10653);
#7817=LINE('',#72416,#10654);
#7818=LINE('',#72431,#10655);
#7819=LINE('',#72446,#10656);
#7820=LINE('',#72461,#10657);
#7821=LINE('',#72489,#10658);
#7822=LINE('',#72494,#10659);
#7823=LINE('',#72506,#10660);
#7824=LINE('',#72521,#10661);
#7825=LINE('',#72536,#10662);
#7826=LINE('',#72551,#10663);
#7827=LINE('',#72566,#10664);
#7828=LINE('',#72581,#10665);
#7829=LINE('',#72596,#10666);
#7830=LINE('',#72611,#10667);
#7831=LINE('',#72626,#10668);
#7832=LINE('',#72641,#10669);
#7833=LINE('',#72661,#10670);
#7834=LINE('',#72663,#10671);
#7835=LINE('',#72665,#10672);
#7836=LINE('',#72666,#10673);
#7837=LINE('',#72678,#10674);
#7838=LINE('',#72693,#10675);
#7839=LINE('',#72699,#10676);
#7840=LINE('',#72701,#10677);
#7841=LINE('',#72702,#10678);
#7842=LINE('',#72714,#10679);
#7843=LINE('',#72729,#10680);
#7844=LINE('',#72735,#10681);
#7845=LINE('',#72737,#10682);
#7846=LINE('',#72738,#10683);
#7847=LINE('',#72741,#10684);
#7848=LINE('',#72743,#10685);
#7849=LINE('',#72744,#10686);
#7850=LINE('',#72746,#10687);
#7851=LINE('',#72747,#10688);
#7852=LINE('',#72762,#10689);
#7853=LINE('',#72767,#10690);
#7854=LINE('',#72779,#10691);
#7855=LINE('',#72794,#10692);
#7856=LINE('',#72809,#10693);
#7857=LINE('',#72824,#10694);
#7858=LINE('',#72839,#10695);
#7859=LINE('',#72854,#10696);
#7860=LINE('',#72882,#10697);
#7861=LINE('',#72887,#10698);
#7862=LINE('',#72899,#10699);
#7863=LINE('',#72914,#10700);
#7864=LINE('',#72929,#10701);
#7865=LINE('',#72944,#10702);
#7866=LINE('',#72959,#10703);
#7867=LINE('',#72974,#10704);
#7868=LINE('',#72989,#10705);
#7869=LINE('',#73004,#10706);
#7870=LINE('',#73019,#10707);
#7871=LINE('',#73034,#10708);
#7872=LINE('',#73063,#10709);
#7873=LINE('',#73068,#10710);
#7874=LINE('',#73080,#10711);
#7875=LINE('',#73095,#10712);
#7876=LINE('',#73110,#10713);
#7877=LINE('',#73125,#10714);
#7878=LINE('',#73140,#10715);
#7879=LINE('',#73155,#10716);
#7880=LINE('',#73170,#10717);
#7881=LINE('',#73185,#10718);
#7882=LINE('',#73191,#10719);
#7883=LINE('',#73193,#10720);
#7884=LINE('',#73194,#10721);
#7885=LINE('',#73206,#10722);
#7886=LINE('',#73221,#10723);
#7887=LINE('',#73236,#10724);
#7888=LINE('',#73251,#10725);
#7889=LINE('',#73266,#10726);
#7890=LINE('',#73281,#10727);
#7891=LINE('',#73296,#10728);
#7892=LINE('',#73311,#10729);
#7893=LINE('',#73326,#10730);
#7894=LINE('',#73332,#10731);
#7895=LINE('',#73334,#10732);
#7896=LINE('',#73335,#10733);
#7897=LINE('',#73338,#10734);
#7898=LINE('',#73340,#10735);
#7899=LINE('',#73341,#10736);
#7900=LINE('',#73343,#10737);
#7901=LINE('',#73344,#10738);
#7902=LINE('',#73359,#10739);
#7903=LINE('',#73364,#10740);
#7904=LINE('',#73376,#10741);
#7905=LINE('',#73391,#10742);
#7906=LINE('',#73406,#10743);
#7907=LINE('',#73421,#10744);
#7908=LINE('',#73436,#10745);
#7909=LINE('',#73451,#10746);
#7910=LINE('',#73479,#10747);
#7911=LINE('',#73484,#10748);
#7912=LINE('',#73496,#10749);
#7913=LINE('',#73511,#10750);
#7914=LINE('',#73526,#10751);
#7915=LINE('',#73541,#10752);
#7916=LINE('',#73556,#10753);
#7917=LINE('',#73571,#10754);
#7918=LINE('',#73586,#10755);
#7919=LINE('',#73601,#10756);
#7920=LINE('',#73616,#10757);
#7921=LINE('',#73631,#10758);
#7922=LINE('',#73660,#10759);
#7923=LINE('',#73665,#10760);
#7924=LINE('',#73677,#10761);
#7925=LINE('',#73692,#10762);
#7926=LINE('',#73707,#10763);
#7927=LINE('',#73722,#10764);
#7928=LINE('',#73737,#10765);
#7929=LINE('',#73752,#10766);
#7930=LINE('',#73767,#10767);
#7931=LINE('',#73782,#10768);
#7932=LINE('',#73797,#10769);
#7933=LINE('',#73812,#10770);
#7934=LINE('',#73827,#10771);
#7935=LINE('',#73833,#10772);
#7936=LINE('',#73835,#10773);
#7937=LINE('',#73836,#10774);
#7938=LINE('',#73848,#10775);
#7939=LINE('',#73863,#10776);
#7940=LINE('',#73878,#10777);
#7941=LINE('',#73893,#10778);
#7942=LINE('',#73908,#10779);
#7943=LINE('',#73923,#10780);
#7944=LINE('',#73938,#10781);
#7945=LINE('',#73944,#10782);
#7946=LINE('',#73946,#10783);
#7947=LINE('',#73947,#10784);
#7948=LINE('',#73959,#10785);
#7949=LINE('',#73974,#10786);
#7950=LINE('',#73989,#10787);
#7951=LINE('',#74004,#10788);
#7952=LINE('',#74019,#10789);
#7953=LINE('',#74034,#10790);
#7954=LINE('',#74049,#10791);
#7955=LINE('',#74055,#10792);
#7956=LINE('',#74057,#10793);
#7957=LINE('',#74058,#10794);
#7958=LINE('',#74085,#10795);
#7959=LINE('',#74090,#10796);
#7960=LINE('',#74102,#10797);
#7961=LINE('',#74117,#10798);
#7962=LINE('',#74132,#10799);
#7963=LINE('',#74147,#10800);
#7964=LINE('',#74162,#10801);
#7965=LINE('',#74177,#10802);
#7966=LINE('',#74205,#10803);
#7967=LINE('',#74210,#10804);
#7968=LINE('',#74222,#10805);
#7969=LINE('',#74237,#10806);
#7970=LINE('',#74252,#10807);
#7971=LINE('',#74267,#10808);
#7972=LINE('',#74282,#10809);
#7973=LINE('',#74297,#10810);
#7974=LINE('',#74312,#10811);
#7975=LINE('',#74327,#10812);
#7976=LINE('',#74342,#10813);
#7977=LINE('',#74357,#10814);
#7978=LINE('',#74377,#10815);
#7979=LINE('',#74379,#10816);
#7980=LINE('',#74381,#10817);
#7981=LINE('',#74382,#10818);
#7982=LINE('',#74385,#10819);
#7983=LINE('',#74387,#10820);
#7984=LINE('',#74388,#10821);
#7985=LINE('',#74390,#10822);
#7986=LINE('',#74391,#10823);
#7987=LINE('',#74395,#10824);
#7988=LINE('',#74397,#10825);
#7989=LINE('',#74399,#10826);
#7990=LINE('',#74400,#10827);
#7991=LINE('',#74403,#10828);
#7992=LINE('',#74405,#10829);
#7993=LINE('',#74406,#10830);
#7994=LINE('',#74409,#10831);
#7995=LINE('',#74411,#10832);
#7996=LINE('',#74412,#10833);
#7997=LINE('',#74415,#10834);
#7998=LINE('',#74417,#10835);
#7999=LINE('',#74418,#10836);
#8000=LINE('',#74421,#10837);
#8001=LINE('',#74423,#10838);
#8002=LINE('',#74424,#10839);
#8003=LINE('',#74427,#10840);
#8004=LINE('',#74429,#10841);
#8005=LINE('',#74430,#10842);
#8006=LINE('',#74433,#10843);
#8007=LINE('',#74435,#10844);
#8008=LINE('',#74436,#10845);
#8009=LINE('',#74439,#10846);
#8010=LINE('',#74441,#10847);
#8011=LINE('',#74442,#10848);
#8012=LINE('',#74445,#10849);
#8013=LINE('',#74447,#10850);
#8014=LINE('',#74448,#10851);
#8015=LINE('',#74451,#10852);
#8016=LINE('',#74453,#10853);
#8017=LINE('',#74454,#10854);
#8018=LINE('',#74456,#10855);
#8019=LINE('',#74457,#10856);
#8020=LINE('',#74464,#10857);
#8021=LINE('',#74466,#10858);
#8022=LINE('',#74468,#10859);
#8023=LINE('',#74469,#10860);
#8024=LINE('',#74472,#10861);
#8025=LINE('',#74474,#10862);
#8026=LINE('',#74475,#10863);
#8027=LINE('',#74478,#10864);
#8028=LINE('',#74480,#10865);
#8029=LINE('',#74481,#10866);
#8030=LINE('',#74483,#10867);
#8031=LINE('',#74484,#10868);
#8032=LINE('',#74489,#10869);
#8033=LINE('',#74491,#10870);
#8034=LINE('',#74493,#10871);
#8035=LINE('',#74494,#10872);
#8036=LINE('',#74497,#10873);
#8037=LINE('',#74499,#10874);
#8038=LINE('',#74500,#10875);
#8039=LINE('',#74503,#10876);
#8040=LINE('',#74505,#10877);
#8041=LINE('',#74506,#10878);
#8042=LINE('',#74508,#10879);
#8043=LINE('',#74509,#10880);
#8044=LINE('',#74514,#10881);
#8045=LINE('',#74516,#10882);
#8046=LINE('',#74518,#10883);
#8047=LINE('',#74519,#10884);
#8048=LINE('',#74522,#10885);
#8049=LINE('',#74524,#10886);
#8050=LINE('',#74525,#10887);
#8051=LINE('',#74528,#10888);
#8052=LINE('',#74530,#10889);
#8053=LINE('',#74531,#10890);
#8054=LINE('',#74533,#10891);
#8055=LINE('',#74534,#10892);
#8056=LINE('',#74539,#10893);
#8057=LINE('',#74541,#10894);
#8058=LINE('',#74543,#10895);
#8059=LINE('',#74544,#10896);
#8060=LINE('',#74547,#10897);
#8061=LINE('',#74549,#10898);
#8062=LINE('',#74550,#10899);
#8063=LINE('',#74553,#10900);
#8064=LINE('',#74555,#10901);
#8065=LINE('',#74556,#10902);
#8066=LINE('',#74558,#10903);
#8067=LINE('',#74559,#10904);
#8068=LINE('',#74564,#10905);
#8069=LINE('',#74566,#10906);
#8070=LINE('',#74568,#10907);
#8071=LINE('',#74569,#10908);
#8072=LINE('',#74572,#10909);
#8073=LINE('',#74574,#10910);
#8074=LINE('',#74575,#10911);
#8075=LINE('',#74578,#10912);
#8076=LINE('',#74580,#10913);
#8077=LINE('',#74581,#10914);
#8078=LINE('',#74583,#10915);
#8079=LINE('',#74584,#10916);
#8080=LINE('',#74589,#10917);
#8081=LINE('',#74591,#10918);
#8082=LINE('',#74593,#10919);
#8083=LINE('',#74594,#10920);
#8084=LINE('',#74597,#10921);
#8085=LINE('',#74599,#10922);
#8086=LINE('',#74600,#10923);
#8087=LINE('',#74603,#10924);
#8088=LINE('',#74605,#10925);
#8089=LINE('',#74606,#10926);
#8090=LINE('',#74608,#10927);
#8091=LINE('',#74609,#10928);
#8092=LINE('',#74614,#10929);
#8093=LINE('',#74616,#10930);
#8094=LINE('',#74618,#10931);
#8095=LINE('',#74619,#10932);
#8096=LINE('',#74622,#10933);
#8097=LINE('',#74624,#10934);
#8098=LINE('',#74625,#10935);
#8099=LINE('',#74628,#10936);
#8100=LINE('',#74630,#10937);
#8101=LINE('',#74631,#10938);
#8102=LINE('',#74633,#10939);
#8103=LINE('',#74634,#10940);
#8104=LINE('',#74639,#10941);
#8105=LINE('',#74641,#10942);
#8106=LINE('',#74643,#10943);
#8107=LINE('',#74644,#10944);
#8108=LINE('',#74647,#10945);
#8109=LINE('',#74649,#10946);
#8110=LINE('',#74650,#10947);
#8111=LINE('',#74653,#10948);
#8112=LINE('',#74655,#10949);
#8113=LINE('',#74656,#10950);
#8114=LINE('',#74658,#10951);
#8115=LINE('',#74659,#10952);
#8116=LINE('',#74664,#10953);
#8117=LINE('',#74666,#10954);
#8118=LINE('',#74668,#10955);
#8119=LINE('',#74669,#10956);
#8120=LINE('',#74672,#10957);
#8121=LINE('',#74674,#10958);
#8122=LINE('',#74675,#10959);
#8123=LINE('',#74678,#10960);
#8124=LINE('',#74680,#10961);
#8125=LINE('',#74681,#10962);
#8126=LINE('',#74683,#10963);
#8127=LINE('',#74684,#10964);
#8128=LINE('',#74689,#10965);
#8129=LINE('',#74691,#10966);
#8130=LINE('',#74693,#10967);
#8131=LINE('',#74694,#10968);
#8132=LINE('',#74697,#10969);
#8133=LINE('',#74699,#10970);
#8134=LINE('',#74700,#10971);
#8135=LINE('',#74703,#10972);
#8136=LINE('',#74705,#10973);
#8137=LINE('',#74706,#10974);
#8138=LINE('',#74708,#10975);
#8139=LINE('',#74709,#10976);
#8140=LINE('',#74714,#10977);
#8141=LINE('',#74716,#10978);
#8142=LINE('',#74718,#10979);
#8143=LINE('',#74719,#10980);
#8144=LINE('',#74722,#10981);
#8145=LINE('',#74724,#10982);
#8146=LINE('',#74725,#10983);
#8147=LINE('',#74728,#10984);
#8148=LINE('',#74730,#10985);
#8149=LINE('',#74731,#10986);
#8150=LINE('',#74733,#10987);
#8151=LINE('',#74734,#10988);
#8152=LINE('',#74739,#10989);
#8153=LINE('',#74741,#10990);
#8154=LINE('',#74743,#10991);
#8155=LINE('',#74744,#10992);
#8156=LINE('',#74747,#10993);
#8157=LINE('',#74749,#10994);
#8158=LINE('',#74750,#10995);
#8159=LINE('',#74753,#10996);
#8160=LINE('',#74755,#10997);
#8161=LINE('',#74756,#10998);
#8162=LINE('',#74758,#10999);
#8163=LINE('',#74759,#11000);
#8164=LINE('',#74764,#11001);
#8165=LINE('',#74766,#11002);
#8166=LINE('',#74768,#11003);
#8167=LINE('',#74769,#11004);
#8168=LINE('',#74772,#11005);
#8169=LINE('',#74774,#11006);
#8170=LINE('',#74775,#11007);
#8171=LINE('',#74778,#11008);
#8172=LINE('',#74780,#11009);
#8173=LINE('',#74781,#11010);
#8174=LINE('',#74783,#11011);
#8175=LINE('',#74784,#11012);
#8176=LINE('',#74789,#11013);
#8177=LINE('',#74791,#11014);
#8178=LINE('',#74793,#11015);
#8179=LINE('',#74794,#11016);
#8180=LINE('',#74797,#11017);
#8181=LINE('',#74799,#11018);
#8182=LINE('',#74800,#11019);
#8183=LINE('',#74803,#11020);
#8184=LINE('',#74805,#11021);
#8185=LINE('',#74806,#11022);
#8186=LINE('',#74808,#11023);
#8187=LINE('',#74809,#11024);
#8188=LINE('',#74814,#11025);
#8189=LINE('',#74816,#11026);
#8190=LINE('',#74818,#11027);
#8191=LINE('',#74819,#11028);
#8192=LINE('',#74822,#11029);
#8193=LINE('',#74824,#11030);
#8194=LINE('',#74825,#11031);
#8195=LINE('',#74828,#11032);
#8196=LINE('',#74830,#11033);
#8197=LINE('',#74831,#11034);
#8198=LINE('',#74833,#11035);
#8199=LINE('',#74834,#11036);
#8200=LINE('',#74839,#11037);
#8201=LINE('',#74841,#11038);
#8202=LINE('',#74843,#11039);
#8203=LINE('',#74844,#11040);
#8204=LINE('',#74847,#11041);
#8205=LINE('',#74849,#11042);
#8206=LINE('',#74850,#11043);
#8207=LINE('',#74853,#11044);
#8208=LINE('',#74855,#11045);
#8209=LINE('',#74856,#11046);
#8210=LINE('',#74858,#11047);
#8211=LINE('',#74859,#11048);
#8212=LINE('',#74864,#11049);
#8213=LINE('',#74866,#11050);
#8214=LINE('',#74868,#11051);
#8215=LINE('',#74869,#11052);
#8216=LINE('',#74872,#11053);
#8217=LINE('',#74874,#11054);
#8218=LINE('',#74875,#11055);
#8219=LINE('',#74878,#11056);
#8220=LINE('',#74880,#11057);
#8221=LINE('',#74881,#11058);
#8222=LINE('',#74883,#11059);
#8223=LINE('',#74884,#11060);
#8224=LINE('',#74889,#11061);
#8225=LINE('',#74891,#11062);
#8226=LINE('',#74893,#11063);
#8227=LINE('',#74894,#11064);
#8228=LINE('',#74897,#11065);
#8229=LINE('',#74899,#11066);
#8230=LINE('',#74900,#11067);
#8231=LINE('',#74903,#11068);
#8232=LINE('',#74905,#11069);
#8233=LINE('',#74906,#11070);
#8234=LINE('',#74908,#11071);
#8235=LINE('',#74909,#11072);
#8236=LINE('',#74914,#11073);
#8237=LINE('',#74916,#11074);
#8238=LINE('',#74918,#11075);
#8239=LINE('',#74919,#11076);
#8240=LINE('',#74922,#11077);
#8241=LINE('',#74924,#11078);
#8242=LINE('',#74925,#11079);
#8243=LINE('',#74928,#11080);
#8244=LINE('',#74930,#11081);
#8245=LINE('',#74931,#11082);
#8246=LINE('',#74933,#11083);
#8247=LINE('',#74934,#11084);
#8248=LINE('',#74939,#11085);
#8249=LINE('',#74941,#11086);
#8250=LINE('',#74943,#11087);
#8251=LINE('',#74944,#11088);
#8252=LINE('',#74947,#11089);
#8253=LINE('',#74949,#11090);
#8254=LINE('',#74950,#11091);
#8255=LINE('',#74953,#11092);
#8256=LINE('',#74955,#11093);
#8257=LINE('',#74956,#11094);
#8258=LINE('',#74958,#11095);
#8259=LINE('',#74959,#11096);
#8260=LINE('',#74964,#11097);
#8261=LINE('',#74966,#11098);
#8262=LINE('',#74968,#11099);
#8263=LINE('',#74969,#11100);
#8264=LINE('',#74972,#11101);
#8265=LINE('',#74974,#11102);
#8266=LINE('',#74975,#11103);
#8267=LINE('',#74978,#11104);
#8268=LINE('',#74980,#11105);
#8269=LINE('',#74981,#11106);
#8270=LINE('',#74983,#11107);
#8271=LINE('',#74984,#11108);
#8272=LINE('',#74989,#11109);
#8273=LINE('',#74991,#11110);
#8274=LINE('',#74993,#11111);
#8275=LINE('',#74994,#11112);
#8276=LINE('',#74997,#11113);
#8277=LINE('',#74999,#11114);
#8278=LINE('',#75000,#11115);
#8279=LINE('',#75003,#11116);
#8280=LINE('',#75005,#11117);
#8281=LINE('',#75006,#11118);
#8282=LINE('',#75008,#11119);
#8283=LINE('',#75009,#11120);
#8284=LINE('',#75014,#11121);
#8285=LINE('',#75016,#11122);
#8286=LINE('',#75018,#11123);
#8287=LINE('',#75019,#11124);
#8288=LINE('',#75022,#11125);
#8289=LINE('',#75024,#11126);
#8290=LINE('',#75025,#11127);
#8291=LINE('',#75028,#11128);
#8292=LINE('',#75030,#11129);
#8293=LINE('',#75031,#11130);
#8294=LINE('',#75033,#11131);
#8295=LINE('',#75034,#11132);
#8296=LINE('',#75039,#11133);
#8297=LINE('',#75041,#11134);
#8298=LINE('',#75043,#11135);
#8299=LINE('',#75044,#11136);
#8300=LINE('',#75047,#11137);
#8301=LINE('',#75049,#11138);
#8302=LINE('',#75050,#11139);
#8303=LINE('',#75053,#11140);
#8304=LINE('',#75055,#11141);
#8305=LINE('',#75056,#11142);
#8306=LINE('',#75058,#11143);
#8307=LINE('',#75059,#11144);
#8308=LINE('',#75064,#11145);
#8309=LINE('',#75066,#11146);
#8310=LINE('',#75068,#11147);
#8311=LINE('',#75069,#11148);
#8312=LINE('',#75072,#11149);
#8313=LINE('',#75074,#11150);
#8314=LINE('',#75075,#11151);
#8315=LINE('',#75078,#11152);
#8316=LINE('',#75080,#11153);
#8317=LINE('',#75081,#11154);
#8318=LINE('',#75083,#11155);
#8319=LINE('',#75084,#11156);
#8320=LINE('',#75089,#11157);
#8321=LINE('',#75091,#11158);
#8322=LINE('',#75093,#11159);
#8323=LINE('',#75094,#11160);
#8324=LINE('',#75097,#11161);
#8325=LINE('',#75099,#11162);
#8326=LINE('',#75100,#11163);
#8327=LINE('',#75103,#11164);
#8328=LINE('',#75105,#11165);
#8329=LINE('',#75106,#11166);
#8330=LINE('',#75108,#11167);
#8331=LINE('',#75109,#11168);
#8332=LINE('',#75114,#11169);
#8333=LINE('',#75116,#11170);
#8334=LINE('',#75118,#11171);
#8335=LINE('',#75119,#11172);
#8336=LINE('',#75122,#11173);
#8337=LINE('',#75124,#11174);
#8338=LINE('',#75125,#11175);
#8339=LINE('',#75128,#11176);
#8340=LINE('',#75130,#11177);
#8341=LINE('',#75131,#11178);
#8342=LINE('',#75133,#11179);
#8343=LINE('',#75134,#11180);
#8344=LINE('',#75139,#11181);
#8345=LINE('',#75141,#11182);
#8346=LINE('',#75143,#11183);
#8347=LINE('',#75144,#11184);
#8348=LINE('',#75147,#11185);
#8349=LINE('',#75149,#11186);
#8350=LINE('',#75150,#11187);
#8351=LINE('',#75153,#11188);
#8352=LINE('',#75155,#11189);
#8353=LINE('',#75156,#11190);
#8354=LINE('',#75158,#11191);
#8355=LINE('',#75159,#11192);
#8356=LINE('',#75164,#11193);
#8357=LINE('',#75166,#11194);
#8358=LINE('',#75168,#11195);
#8359=LINE('',#75169,#11196);
#8360=LINE('',#75172,#11197);
#8361=LINE('',#75174,#11198);
#8362=LINE('',#75175,#11199);
#8363=LINE('',#75178,#11200);
#8364=LINE('',#75180,#11201);
#8365=LINE('',#75181,#11202);
#8366=LINE('',#75183,#11203);
#8367=LINE('',#75184,#11204);
#8368=LINE('',#75189,#11205);
#8369=LINE('',#75191,#11206);
#8370=LINE('',#75193,#11207);
#8371=LINE('',#75194,#11208);
#8372=LINE('',#75197,#11209);
#8373=LINE('',#75199,#11210);
#8374=LINE('',#75200,#11211);
#8375=LINE('',#75203,#11212);
#8376=LINE('',#75205,#11213);
#8377=LINE('',#75206,#11214);
#8378=LINE('',#75208,#11215);
#8379=LINE('',#75209,#11216);
#8380=LINE('',#75214,#11217);
#8381=LINE('',#75216,#11218);
#8382=LINE('',#75218,#11219);
#8383=LINE('',#75219,#11220);
#8384=LINE('',#75222,#11221);
#8385=LINE('',#75224,#11222);
#8386=LINE('',#75225,#11223);
#8387=LINE('',#75228,#11224);
#8388=LINE('',#75230,#11225);
#8389=LINE('',#75231,#11226);
#8390=LINE('',#75233,#11227);
#8391=LINE('',#75234,#11228);
#8392=LINE('',#75239,#11229);
#8393=LINE('',#75241,#11230);
#8394=LINE('',#75243,#11231);
#8395=LINE('',#75244,#11232);
#8396=LINE('',#75247,#11233);
#8397=LINE('',#75249,#11234);
#8398=LINE('',#75250,#11235);
#8399=LINE('',#75253,#11236);
#8400=LINE('',#75255,#11237);
#8401=LINE('',#75256,#11238);
#8402=LINE('',#75258,#11239);
#8403=LINE('',#75259,#11240);
#8404=LINE('',#75264,#11241);
#8405=LINE('',#75266,#11242);
#8406=LINE('',#75268,#11243);
#8407=LINE('',#75269,#11244);
#8408=LINE('',#75272,#11245);
#8409=LINE('',#75274,#11246);
#8410=LINE('',#75275,#11247);
#8411=LINE('',#75278,#11248);
#8412=LINE('',#75280,#11249);
#8413=LINE('',#75281,#11250);
#8414=LINE('',#75283,#11251);
#8415=LINE('',#75284,#11252);
#8416=LINE('',#75289,#11253);
#8417=LINE('',#75291,#11254);
#8418=LINE('',#75293,#11255);
#8419=LINE('',#75294,#11256);
#8420=LINE('',#75297,#11257);
#8421=LINE('',#75299,#11258);
#8422=LINE('',#75300,#11259);
#8423=LINE('',#75303,#11260);
#8424=LINE('',#75305,#11261);
#8425=LINE('',#75306,#11262);
#8426=LINE('',#75308,#11263);
#8427=LINE('',#75309,#11264);
#8428=LINE('',#75314,#11265);
#8429=LINE('',#75316,#11266);
#8430=LINE('',#75318,#11267);
#8431=LINE('',#75319,#11268);
#8432=LINE('',#75322,#11269);
#8433=LINE('',#75324,#11270);
#8434=LINE('',#75325,#11271);
#8435=LINE('',#75328,#11272);
#8436=LINE('',#75330,#11273);
#8437=LINE('',#75331,#11274);
#8438=LINE('',#75333,#11275);
#8439=LINE('',#75334,#11276);
#8440=LINE('',#75339,#11277);
#8441=LINE('',#75341,#11278);
#8442=LINE('',#75343,#11279);
#8443=LINE('',#75344,#11280);
#8444=LINE('',#75347,#11281);
#8445=LINE('',#75349,#11282);
#8446=LINE('',#75350,#11283);
#8447=LINE('',#75353,#11284);
#8448=LINE('',#75355,#11285);
#8449=LINE('',#75356,#11286);
#8450=LINE('',#75358,#11287);
#8451=LINE('',#75359,#11288);
#8452=LINE('',#75364,#11289);
#8453=LINE('',#75366,#11290);
#8454=LINE('',#75368,#11291);
#8455=LINE('',#75369,#11292);
#8456=LINE('',#75372,#11293);
#8457=LINE('',#75374,#11294);
#8458=LINE('',#75375,#11295);
#8459=LINE('',#75378,#11296);
#8460=LINE('',#75380,#11297);
#8461=LINE('',#75381,#11298);
#8462=LINE('',#75383,#11299);
#8463=LINE('',#75384,#11300);
#8464=LINE('',#75389,#11301);
#8465=LINE('',#75391,#11302);
#8466=LINE('',#75393,#11303);
#8467=LINE('',#75394,#11304);
#8468=LINE('',#75397,#11305);
#8469=LINE('',#75399,#11306);
#8470=LINE('',#75400,#11307);
#8471=LINE('',#75403,#11308);
#8472=LINE('',#75405,#11309);
#8473=LINE('',#75406,#11310);
#8474=LINE('',#75408,#11311);
#8475=LINE('',#75409,#11312);
#8476=LINE('',#75414,#11313);
#8477=LINE('',#75416,#11314);
#8478=LINE('',#75418,#11315);
#8479=LINE('',#75419,#11316);
#8480=LINE('',#75422,#11317);
#8481=LINE('',#75424,#11318);
#8482=LINE('',#75425,#11319);
#8483=LINE('',#75428,#11320);
#8484=LINE('',#75430,#11321);
#8485=LINE('',#75431,#11322);
#8486=LINE('',#75433,#11323);
#8487=LINE('',#75434,#11324);
#8488=LINE('',#75439,#11325);
#8489=LINE('',#75441,#11326);
#8490=LINE('',#75443,#11327);
#8491=LINE('',#75444,#11328);
#8492=LINE('',#75447,#11329);
#8493=LINE('',#75449,#11330);
#8494=LINE('',#75450,#11331);
#8495=LINE('',#75453,#11332);
#8496=LINE('',#75455,#11333);
#8497=LINE('',#75456,#11334);
#8498=LINE('',#75458,#11335);
#8499=LINE('',#75459,#11336);
#8500=LINE('',#75464,#11337);
#8501=LINE('',#75466,#11338);
#8502=LINE('',#75468,#11339);
#8503=LINE('',#75469,#11340);
#8504=LINE('',#75472,#11341);
#8505=LINE('',#75474,#11342);
#8506=LINE('',#75475,#11343);
#8507=LINE('',#75478,#11344);
#8508=LINE('',#75480,#11345);
#8509=LINE('',#75481,#11346);
#8510=LINE('',#75483,#11347);
#8511=LINE('',#75484,#11348);
#8512=LINE('',#75489,#11349);
#8513=LINE('',#75491,#11350);
#8514=LINE('',#75493,#11351);
#8515=LINE('',#75494,#11352);
#8516=LINE('',#75497,#11353);
#8517=LINE('',#75499,#11354);
#8518=LINE('',#75500,#11355);
#8519=LINE('',#75503,#11356);
#8520=LINE('',#75505,#11357);
#8521=LINE('',#75506,#11358);
#8522=LINE('',#75508,#11359);
#8523=LINE('',#75509,#11360);
#8524=LINE('',#75514,#11361);
#8525=LINE('',#75516,#11362);
#8526=LINE('',#75518,#11363);
#8527=LINE('',#75519,#11364);
#8528=LINE('',#75522,#11365);
#8529=LINE('',#75524,#11366);
#8530=LINE('',#75525,#11367);
#8531=LINE('',#75528,#11368);
#8532=LINE('',#75530,#11369);
#8533=LINE('',#75531,#11370);
#8534=LINE('',#75533,#11371);
#8535=LINE('',#75534,#11372);
#8536=LINE('',#75539,#11373);
#8537=LINE('',#75541,#11374);
#8538=LINE('',#75543,#11375);
#8539=LINE('',#75544,#11376);
#8540=LINE('',#75547,#11377);
#8541=LINE('',#75549,#11378);
#8542=LINE('',#75550,#11379);
#8543=LINE('',#75553,#11380);
#8544=LINE('',#75555,#11381);
#8545=LINE('',#75556,#11382);
#8546=LINE('',#75558,#11383);
#8547=LINE('',#75559,#11384);
#8548=LINE('',#75564,#11385);
#8549=LINE('',#75566,#11386);
#8550=LINE('',#75568,#11387);
#8551=LINE('',#75569,#11388);
#8552=LINE('',#75572,#11389);
#8553=LINE('',#75574,#11390);
#8554=LINE('',#75575,#11391);
#8555=LINE('',#75578,#11392);
#8556=LINE('',#75580,#11393);
#8557=LINE('',#75581,#11394);
#8558=LINE('',#75583,#11395);
#8559=LINE('',#75584,#11396);
#8560=LINE('',#75589,#11397);
#8561=LINE('',#75591,#11398);
#8562=LINE('',#75593,#11399);
#8563=LINE('',#75594,#11400);
#8564=LINE('',#75597,#11401);
#8565=LINE('',#75599,#11402);
#8566=LINE('',#75600,#11403);
#8567=LINE('',#75603,#11404);
#8568=LINE('',#75605,#11405);
#8569=LINE('',#75606,#11406);
#8570=LINE('',#75608,#11407);
#8571=LINE('',#75609,#11408);
#8572=LINE('',#75614,#11409);
#8573=LINE('',#75616,#11410);
#8574=LINE('',#75618,#11411);
#8575=LINE('',#75619,#11412);
#8576=LINE('',#75622,#11413);
#8577=LINE('',#75624,#11414);
#8578=LINE('',#75625,#11415);
#8579=LINE('',#75628,#11416);
#8580=LINE('',#75630,#11417);
#8581=LINE('',#75631,#11418);
#8582=LINE('',#75633,#11419);
#8583=LINE('',#75634,#11420);
#8584=LINE('',#75639,#11421);
#8585=LINE('',#75641,#11422);
#8586=LINE('',#75643,#11423);
#8587=LINE('',#75644,#11424);
#8588=LINE('',#75647,#11425);
#8589=LINE('',#75649,#11426);
#8590=LINE('',#75650,#11427);
#8591=LINE('',#75653,#11428);
#8592=LINE('',#75655,#11429);
#8593=LINE('',#75656,#11430);
#8594=LINE('',#75658,#11431);
#8595=LINE('',#75659,#11432);
#8596=LINE('',#75664,#11433);
#8597=LINE('',#75666,#11434);
#8598=LINE('',#75668,#11435);
#8599=LINE('',#75669,#11436);
#8600=LINE('',#75672,#11437);
#8601=LINE('',#75674,#11438);
#8602=LINE('',#75675,#11439);
#8603=LINE('',#75678,#11440);
#8604=LINE('',#75680,#11441);
#8605=LINE('',#75681,#11442);
#8606=LINE('',#75683,#11443);
#8607=LINE('',#75684,#11444);
#8608=LINE('',#75689,#11445);
#8609=LINE('',#75691,#11446);
#8610=LINE('',#75693,#11447);
#8611=LINE('',#75694,#11448);
#8612=LINE('',#75697,#11449);
#8613=LINE('',#75699,#11450);
#8614=LINE('',#75700,#11451);
#8615=LINE('',#75703,#11452);
#8616=LINE('',#75705,#11453);
#8617=LINE('',#75706,#11454);
#8618=LINE('',#75708,#11455);
#8619=LINE('',#75709,#11456);
#8620=LINE('',#75714,#11457);
#8621=LINE('',#75716,#11458);
#8622=LINE('',#75718,#11459);
#8623=LINE('',#75719,#11460);
#8624=LINE('',#75722,#11461);
#8625=LINE('',#75724,#11462);
#8626=LINE('',#75725,#11463);
#8627=LINE('',#75728,#11464);
#8628=LINE('',#75730,#11465);
#8629=LINE('',#75731,#11466);
#8630=LINE('',#75733,#11467);
#8631=LINE('',#75734,#11468);
#8632=LINE('',#75739,#11469);
#8633=LINE('',#75741,#11470);
#8634=LINE('',#75743,#11471);
#8635=LINE('',#75744,#11472);
#8636=LINE('',#75747,#11473);
#8637=LINE('',#75749,#11474);
#8638=LINE('',#75750,#11475);
#8639=LINE('',#75753,#11476);
#8640=LINE('',#75755,#11477);
#8641=LINE('',#75756,#11478);
#8642=LINE('',#75758,#11479);
#8643=LINE('',#75759,#11480);
#8644=LINE('',#75764,#11481);
#8645=LINE('',#75766,#11482);
#8646=LINE('',#75768,#11483);
#8647=LINE('',#75769,#11484);
#8648=LINE('',#75772,#11485);
#8649=LINE('',#75774,#11486);
#8650=LINE('',#75775,#11487);
#8651=LINE('',#75778,#11488);
#8652=LINE('',#75780,#11489);
#8653=LINE('',#75781,#11490);
#8654=LINE('',#75783,#11491);
#8655=LINE('',#75784,#11492);
#8656=LINE('',#75789,#11493);
#8657=LINE('',#75791,#11494);
#8658=LINE('',#75793,#11495);
#8659=LINE('',#75794,#11496);
#8660=LINE('',#75797,#11497);
#8661=LINE('',#75799,#11498);
#8662=LINE('',#75800,#11499);
#8663=LINE('',#75803,#11500);
#8664=LINE('',#75805,#11501);
#8665=LINE('',#75806,#11502);
#8666=LINE('',#75808,#11503);
#8667=LINE('',#75809,#11504);
#8668=LINE('',#75814,#11505);
#8669=LINE('',#75816,#11506);
#8670=LINE('',#75818,#11507);
#8671=LINE('',#75819,#11508);
#8672=LINE('',#75822,#11509);
#8673=LINE('',#75824,#11510);
#8674=LINE('',#75825,#11511);
#8675=LINE('',#75828,#11512);
#8676=LINE('',#75830,#11513);
#8677=LINE('',#75831,#11514);
#8678=LINE('',#75833,#11515);
#8679=LINE('',#75834,#11516);
#8680=LINE('',#75839,#11517);
#8681=LINE('',#75841,#11518);
#8682=LINE('',#75843,#11519);
#8683=LINE('',#75844,#11520);
#8684=LINE('',#75847,#11521);
#8685=LINE('',#75849,#11522);
#8686=LINE('',#75850,#11523);
#8687=LINE('',#75853,#11524);
#8688=LINE('',#75855,#11525);
#8689=LINE('',#75856,#11526);
#8690=LINE('',#75858,#11527);
#8691=LINE('',#75859,#11528);
#8692=LINE('',#75864,#11529);
#8693=LINE('',#75866,#11530);
#8694=LINE('',#75868,#11531);
#8695=LINE('',#75869,#11532);
#8696=LINE('',#75872,#11533);
#8697=LINE('',#75874,#11534);
#8698=LINE('',#75875,#11535);
#8699=LINE('',#75878,#11536);
#8700=LINE('',#75880,#11537);
#8701=LINE('',#75881,#11538);
#8702=LINE('',#75883,#11539);
#8703=LINE('',#75884,#11540);
#8704=LINE('',#75889,#11541);
#8705=LINE('',#75891,#11542);
#8706=LINE('',#75893,#11543);
#8707=LINE('',#75894,#11544);
#8708=LINE('',#75897,#11545);
#8709=LINE('',#75899,#11546);
#8710=LINE('',#75900,#11547);
#8711=LINE('',#75903,#11548);
#8712=LINE('',#75905,#11549);
#8713=LINE('',#75906,#11550);
#8714=LINE('',#75908,#11551);
#8715=LINE('',#75909,#11552);
#8716=LINE('',#75914,#11553);
#8717=LINE('',#75916,#11554);
#8718=LINE('',#75918,#11555);
#8719=LINE('',#75919,#11556);
#8720=LINE('',#75922,#11557);
#8721=LINE('',#75924,#11558);
#8722=LINE('',#75925,#11559);
#8723=LINE('',#75928,#11560);
#8724=LINE('',#75930,#11561);
#8725=LINE('',#75931,#11562);
#8726=LINE('',#75933,#11563);
#8727=LINE('',#75934,#11564);
#8728=LINE('',#75939,#11565);
#8729=LINE('',#75941,#11566);
#8730=LINE('',#75943,#11567);
#8731=LINE('',#75944,#11568);
#8732=LINE('',#75947,#11569);
#8733=LINE('',#75949,#11570);
#8734=LINE('',#75950,#11571);
#8735=LINE('',#75953,#11572);
#8736=LINE('',#75955,#11573);
#8737=LINE('',#75956,#11574);
#8738=LINE('',#75958,#11575);
#8739=LINE('',#75959,#11576);
#8740=LINE('',#75964,#11577);
#8741=LINE('',#75966,#11578);
#8742=LINE('',#75968,#11579);
#8743=LINE('',#75969,#11580);
#8744=LINE('',#75972,#11581);
#8745=LINE('',#75974,#11582);
#8746=LINE('',#75975,#11583);
#8747=LINE('',#75978,#11584);
#8748=LINE('',#75980,#11585);
#8749=LINE('',#75981,#11586);
#8750=LINE('',#75983,#11587);
#8751=LINE('',#75984,#11588);
#8752=LINE('',#75989,#11589);
#8753=LINE('',#75991,#11590);
#8754=LINE('',#75993,#11591);
#8755=LINE('',#75994,#11592);
#8756=LINE('',#75997,#11593);
#8757=LINE('',#75999,#11594);
#8758=LINE('',#76000,#11595);
#8759=LINE('',#76003,#11596);
#8760=LINE('',#76005,#11597);
#8761=LINE('',#76006,#11598);
#8762=LINE('',#76008,#11599);
#8763=LINE('',#76009,#11600);
#8764=LINE('',#76014,#11601);
#8765=LINE('',#76016,#11602);
#8766=LINE('',#76018,#11603);
#8767=LINE('',#76019,#11604);
#8768=LINE('',#76022,#11605);
#8769=LINE('',#76024,#11606);
#8770=LINE('',#76025,#11607);
#8771=LINE('',#76028,#11608);
#8772=LINE('',#76030,#11609);
#8773=LINE('',#76031,#11610);
#8774=LINE('',#76033,#11611);
#8775=LINE('',#76034,#11612);
#8776=LINE('',#76039,#11613);
#8777=LINE('',#76041,#11614);
#8778=LINE('',#76043,#11615);
#8779=LINE('',#76044,#11616);
#8780=LINE('',#76047,#11617);
#8781=LINE('',#76049,#11618);
#8782=LINE('',#76050,#11619);
#8783=LINE('',#76053,#11620);
#8784=LINE('',#76055,#11621);
#8785=LINE('',#76056,#11622);
#8786=LINE('',#76058,#11623);
#8787=LINE('',#76059,#11624);
#8788=LINE('',#76064,#11625);
#8789=LINE('',#76066,#11626);
#8790=LINE('',#76068,#11627);
#8791=LINE('',#76069,#11628);
#8792=LINE('',#76072,#11629);
#8793=LINE('',#76074,#11630);
#8794=LINE('',#76075,#11631);
#8795=LINE('',#76078,#11632);
#8796=LINE('',#76080,#11633);
#8797=LINE('',#76081,#11634);
#8798=LINE('',#76083,#11635);
#8799=LINE('',#76084,#11636);
#8800=LINE('',#76089,#11637);
#8801=LINE('',#76091,#11638);
#8802=LINE('',#76093,#11639);
#8803=LINE('',#76094,#11640);
#8804=LINE('',#76097,#11641);
#8805=LINE('',#76099,#11642);
#8806=LINE('',#76100,#11643);
#8807=LINE('',#76103,#11644);
#8808=LINE('',#76105,#11645);
#8809=LINE('',#76106,#11646);
#8810=LINE('',#76108,#11647);
#8811=LINE('',#76109,#11648);
#8812=LINE('',#76114,#11649);
#8813=LINE('',#76116,#11650);
#8814=LINE('',#76118,#11651);
#8815=LINE('',#76119,#11652);
#8816=LINE('',#76122,#11653);
#8817=LINE('',#76124,#11654);
#8818=LINE('',#76125,#11655);
#8819=LINE('',#76128,#11656);
#8820=LINE('',#76130,#11657);
#8821=LINE('',#76131,#11658);
#8822=LINE('',#76133,#11659);
#8823=LINE('',#76134,#11660);
#8824=LINE('',#76139,#11661);
#8825=LINE('',#76141,#11662);
#8826=LINE('',#76143,#11663);
#8827=LINE('',#76144,#11664);
#8828=LINE('',#76147,#11665);
#8829=LINE('',#76149,#11666);
#8830=LINE('',#76150,#11667);
#8831=LINE('',#76153,#11668);
#8832=LINE('',#76155,#11669);
#8833=LINE('',#76156,#11670);
#8834=LINE('',#76158,#11671);
#8835=LINE('',#76159,#11672);
#8836=LINE('',#76164,#11673);
#8837=LINE('',#76166,#11674);
#8838=LINE('',#76168,#11675);
#8839=LINE('',#76169,#11676);
#8840=LINE('',#76172,#11677);
#8841=LINE('',#76174,#11678);
#8842=LINE('',#76175,#11679);
#8843=LINE('',#76178,#11680);
#8844=LINE('',#76180,#11681);
#8845=LINE('',#76181,#11682);
#8846=LINE('',#76183,#11683);
#8847=LINE('',#76184,#11684);
#8848=LINE('',#76189,#11685);
#8849=LINE('',#76191,#11686);
#8850=LINE('',#76193,#11687);
#8851=LINE('',#76194,#11688);
#8852=LINE('',#76197,#11689);
#8853=LINE('',#76199,#11690);
#8854=LINE('',#76200,#11691);
#8855=LINE('',#76203,#11692);
#8856=LINE('',#76205,#11693);
#8857=LINE('',#76206,#11694);
#8858=LINE('',#76208,#11695);
#8859=LINE('',#76209,#11696);
#8860=LINE('',#76214,#11697);
#8861=LINE('',#76216,#11698);
#8862=LINE('',#76218,#11699);
#8863=LINE('',#76219,#11700);
#8864=LINE('',#76222,#11701);
#8865=LINE('',#76224,#11702);
#8866=LINE('',#76225,#11703);
#8867=LINE('',#76228,#11704);
#8868=LINE('',#76230,#11705);
#8869=LINE('',#76231,#11706);
#8870=LINE('',#76233,#11707);
#8871=LINE('',#76234,#11708);
#8872=LINE('',#76239,#11709);
#8873=LINE('',#76241,#11710);
#8874=LINE('',#76243,#11711);
#8875=LINE('',#76244,#11712);
#8876=LINE('',#76247,#11713);
#8877=LINE('',#76249,#11714);
#8878=LINE('',#76250,#11715);
#8879=LINE('',#76253,#11716);
#8880=LINE('',#76255,#11717);
#8881=LINE('',#76256,#11718);
#8882=LINE('',#76258,#11719);
#8883=LINE('',#76259,#11720);
#8884=LINE('',#76264,#11721);
#8885=LINE('',#76266,#11722);
#8886=LINE('',#76268,#11723);
#8887=LINE('',#76269,#11724);
#8888=LINE('',#76272,#11725);
#8889=LINE('',#76274,#11726);
#8890=LINE('',#76275,#11727);
#8891=LINE('',#76278,#11728);
#8892=LINE('',#76280,#11729);
#8893=LINE('',#76281,#11730);
#8894=LINE('',#76283,#11731);
#8895=LINE('',#76284,#11732);
#8896=LINE('',#76289,#11733);
#8897=LINE('',#76291,#11734);
#8898=LINE('',#76293,#11735);
#8899=LINE('',#76294,#11736);
#8900=LINE('',#76297,#11737);
#8901=LINE('',#76299,#11738);
#8902=LINE('',#76300,#11739);
#8903=LINE('',#76303,#11740);
#8904=LINE('',#76305,#11741);
#8905=LINE('',#76306,#11742);
#8906=LINE('',#76308,#11743);
#8907=LINE('',#76309,#11744);
#8908=LINE('',#76314,#11745);
#8909=LINE('',#76316,#11746);
#8910=LINE('',#76318,#11747);
#8911=LINE('',#76319,#11748);
#8912=LINE('',#76322,#11749);
#8913=LINE('',#76324,#11750);
#8914=LINE('',#76325,#11751);
#8915=LINE('',#76328,#11752);
#8916=LINE('',#76330,#11753);
#8917=LINE('',#76331,#11754);
#8918=LINE('',#76333,#11755);
#8919=LINE('',#76334,#11756);
#8920=LINE('',#76339,#11757);
#8921=LINE('',#76341,#11758);
#8922=LINE('',#76343,#11759);
#8923=LINE('',#76344,#11760);
#8924=LINE('',#76347,#11761);
#8925=LINE('',#76349,#11762);
#8926=LINE('',#76350,#11763);
#8927=LINE('',#76353,#11764);
#8928=LINE('',#76355,#11765);
#8929=LINE('',#76356,#11766);
#8930=LINE('',#76358,#11767);
#8931=LINE('',#76359,#11768);
#8932=LINE('',#76364,#11769);
#8933=LINE('',#76366,#11770);
#8934=LINE('',#76368,#11771);
#8935=LINE('',#76369,#11772);
#8936=LINE('',#76372,#11773);
#8937=LINE('',#76374,#11774);
#8938=LINE('',#76375,#11775);
#8939=LINE('',#76378,#11776);
#8940=LINE('',#76380,#11777);
#8941=LINE('',#76381,#11778);
#8942=LINE('',#76383,#11779);
#8943=LINE('',#76384,#11780);
#8944=LINE('',#76389,#11781);
#8945=LINE('',#76391,#11782);
#8946=LINE('',#76393,#11783);
#8947=LINE('',#76394,#11784);
#8948=LINE('',#76397,#11785);
#8949=LINE('',#76399,#11786);
#8950=LINE('',#76400,#11787);
#8951=LINE('',#76403,#11788);
#8952=LINE('',#76405,#11789);
#8953=LINE('',#76406,#11790);
#8954=LINE('',#76408,#11791);
#8955=LINE('',#76409,#11792);
#8956=LINE('',#76414,#11793);
#8957=LINE('',#76416,#11794);
#8958=LINE('',#76418,#11795);
#8959=LINE('',#76419,#11796);
#8960=LINE('',#76422,#11797);
#8961=LINE('',#76424,#11798);
#8962=LINE('',#76425,#11799);
#8963=LINE('',#76428,#11800);
#8964=LINE('',#76430,#11801);
#8965=LINE('',#76431,#11802);
#8966=LINE('',#76433,#11803);
#8967=LINE('',#76434,#11804);
#8968=LINE('',#76439,#11805);
#8969=LINE('',#76441,#11806);
#8970=LINE('',#76443,#11807);
#8971=LINE('',#76444,#11808);
#8972=LINE('',#76447,#11809);
#8973=LINE('',#76449,#11810);
#8974=LINE('',#76450,#11811);
#8975=LINE('',#76453,#11812);
#8976=LINE('',#76455,#11813);
#8977=LINE('',#76456,#11814);
#8978=LINE('',#76458,#11815);
#8979=LINE('',#76459,#11816);
#8980=LINE('',#76464,#11817);
#8981=LINE('',#76466,#11818);
#8982=LINE('',#76468,#11819);
#8983=LINE('',#76469,#11820);
#8984=LINE('',#76472,#11821);
#8985=LINE('',#76474,#11822);
#8986=LINE('',#76475,#11823);
#8987=LINE('',#76478,#11824);
#8988=LINE('',#76480,#11825);
#8989=LINE('',#76481,#11826);
#8990=LINE('',#76483,#11827);
#8991=LINE('',#76484,#11828);
#8992=LINE('',#76489,#11829);
#8993=LINE('',#76491,#11830);
#8994=LINE('',#76493,#11831);
#8995=LINE('',#76494,#11832);
#8996=LINE('',#76497,#11833);
#8997=LINE('',#76499,#11834);
#8998=LINE('',#76500,#11835);
#8999=LINE('',#76503,#11836);
#9000=LINE('',#76505,#11837);
#9001=LINE('',#76506,#11838);
#9002=LINE('',#76508,#11839);
#9003=LINE('',#76509,#11840);
#9004=LINE('',#76514,#11841);
#9005=LINE('',#76516,#11842);
#9006=LINE('',#76518,#11843);
#9007=LINE('',#76519,#11844);
#9008=LINE('',#76522,#11845);
#9009=LINE('',#76524,#11846);
#9010=LINE('',#76525,#11847);
#9011=LINE('',#76528,#11848);
#9012=LINE('',#76530,#11849);
#9013=LINE('',#76531,#11850);
#9014=LINE('',#76533,#11851);
#9015=LINE('',#76534,#11852);
#9016=LINE('',#76539,#11853);
#9017=LINE('',#76541,#11854);
#9018=LINE('',#76543,#11855);
#9019=LINE('',#76544,#11856);
#9020=LINE('',#76547,#11857);
#9021=LINE('',#76549,#11858);
#9022=LINE('',#76550,#11859);
#9023=LINE('',#76553,#11860);
#9024=LINE('',#76555,#11861);
#9025=LINE('',#76556,#11862);
#9026=LINE('',#76558,#11863);
#9027=LINE('',#76559,#11864);
#9028=LINE('',#76564,#11865);
#9029=LINE('',#76566,#11866);
#9030=LINE('',#76568,#11867);
#9031=LINE('',#76569,#11868);
#9032=LINE('',#76572,#11869);
#9033=LINE('',#76574,#11870);
#9034=LINE('',#76575,#11871);
#9035=LINE('',#76578,#11872);
#9036=LINE('',#76580,#11873);
#9037=LINE('',#76581,#11874);
#9038=LINE('',#76583,#11875);
#9039=LINE('',#76584,#11876);
#9040=LINE('',#76590,#11877);
#9041=LINE('',#76596,#11878);
#9042=LINE('',#76601,#11879);
#9043=LINE('',#76603,#11880);
#9044=LINE('',#76605,#11881);
#9045=LINE('',#76606,#11882);
#9046=LINE('',#76612,#11883);
#9047=LINE('',#76615,#11884);
#9048=LINE('',#76617,#11885);
#9049=LINE('',#76618,#11886);
#9050=LINE('',#76624,#11887);
#9051=LINE('',#76627,#11888);
#9052=LINE('',#76629,#11889);
#9053=LINE('',#76630,#11890);
#9054=LINE('',#76636,#11891);
#9055=LINE('',#76639,#11892);
#9056=LINE('',#76641,#11893);
#9057=LINE('',#76642,#11894);
#9058=LINE('',#76652,#11895);
#9059=LINE('',#76654,#11896);
#9060=LINE('',#76656,#11897);
#9061=LINE('',#76657,#11898);
#9062=LINE('',#76660,#11899);
#9063=LINE('',#76662,#11900);
#9064=LINE('',#76663,#11901);
#9065=LINE('',#76666,#11902);
#9066=LINE('',#76668,#11903);
#9067=LINE('',#76669,#11904);
#9068=LINE('',#76671,#11905);
#9069=LINE('',#76672,#11906);
#9070=LINE('',#76677,#11907);
#9071=LINE('',#76679,#11908);
#9072=LINE('',#76681,#11909);
#9073=LINE('',#76682,#11910);
#9074=LINE('',#76685,#11911);
#9075=LINE('',#76687,#11912);
#9076=LINE('',#76688,#11913);
#9077=LINE('',#76691,#11914);
#9078=LINE('',#76693,#11915);
#9079=LINE('',#76694,#11916);
#9080=LINE('',#76696,#11917);
#9081=LINE('',#76697,#11918);
#9082=LINE('',#76702,#11919);
#9083=LINE('',#76704,#11920);
#9084=LINE('',#76706,#11921);
#9085=LINE('',#76707,#11922);
#9086=LINE('',#76710,#11923);
#9087=LINE('',#76712,#11924);
#9088=LINE('',#76713,#11925);
#9089=LINE('',#76716,#11926);
#9090=LINE('',#76718,#11927);
#9091=LINE('',#76719,#11928);
#9092=LINE('',#76721,#11929);
#9093=LINE('',#76722,#11930);
#9094=LINE('',#76727,#11931);
#9095=LINE('',#76729,#11932);
#9096=LINE('',#76731,#11933);
#9097=LINE('',#76732,#11934);
#9098=LINE('',#76735,#11935);
#9099=LINE('',#76737,#11936);
#9100=LINE('',#76738,#11937);
#9101=LINE('',#76741,#11938);
#9102=LINE('',#76743,#11939);
#9103=LINE('',#76744,#11940);
#9104=LINE('',#76746,#11941);
#9105=LINE('',#76747,#11942);
#9106=LINE('',#76752,#11943);
#9107=LINE('',#76754,#11944);
#9108=LINE('',#76756,#11945);
#9109=LINE('',#76757,#11946);
#9110=LINE('',#76760,#11947);
#9111=LINE('',#76762,#11948);
#9112=LINE('',#76763,#11949);
#9113=LINE('',#76766,#11950);
#9114=LINE('',#76768,#11951);
#9115=LINE('',#76769,#11952);
#9116=LINE('',#76771,#11953);
#9117=LINE('',#76772,#11954);
#9118=LINE('',#76777,#11955);
#9119=LINE('',#76779,#11956);
#9120=LINE('',#76781,#11957);
#9121=LINE('',#76782,#11958);
#9122=LINE('',#76785,#11959);
#9123=LINE('',#76787,#11960);
#9124=LINE('',#76788,#11961);
#9125=LINE('',#76791,#11962);
#9126=LINE('',#76793,#11963);
#9127=LINE('',#76794,#11964);
#9128=LINE('',#76796,#11965);
#9129=LINE('',#76797,#11966);
#9130=LINE('',#76802,#11967);
#9131=LINE('',#76804,#11968);
#9132=LINE('',#76806,#11969);
#9133=LINE('',#76807,#11970);
#9134=LINE('',#76810,#11971);
#9135=LINE('',#76812,#11972);
#9136=LINE('',#76813,#11973);
#9137=LINE('',#76816,#11974);
#9138=LINE('',#76818,#11975);
#9139=LINE('',#76819,#11976);
#9140=LINE('',#76821,#11977);
#9141=LINE('',#76822,#11978);
#9142=LINE('',#76827,#11979);
#9143=LINE('',#76829,#11980);
#9144=LINE('',#76831,#11981);
#9145=LINE('',#76832,#11982);
#9146=LINE('',#76835,#11983);
#9147=LINE('',#76837,#11984);
#9148=LINE('',#76838,#11985);
#9149=LINE('',#76841,#11986);
#9150=LINE('',#76843,#11987);
#9151=LINE('',#76844,#11988);
#9152=LINE('',#76846,#11989);
#9153=LINE('',#76847,#11990);
#9154=LINE('',#76852,#11991);
#9155=LINE('',#76854,#11992);
#9156=LINE('',#76856,#11993);
#9157=LINE('',#76857,#11994);
#9158=LINE('',#76860,#11995);
#9159=LINE('',#76862,#11996);
#9160=LINE('',#76863,#11997);
#9161=LINE('',#76866,#11998);
#9162=LINE('',#76868,#11999);
#9163=LINE('',#76869,#12000);
#9164=LINE('',#76871,#12001);
#9165=LINE('',#76872,#12002);
#9166=LINE('',#76877,#12003);
#9167=LINE('',#76879,#12004);
#9168=LINE('',#76881,#12005);
#9169=LINE('',#76882,#12006);
#9170=LINE('',#76885,#12007);
#9171=LINE('',#76887,#12008);
#9172=LINE('',#76888,#12009);
#9173=LINE('',#76891,#12010);
#9174=LINE('',#76893,#12011);
#9175=LINE('',#76894,#12012);
#9176=LINE('',#76896,#12013);
#9177=LINE('',#76897,#12014);
#9178=LINE('',#76902,#12015);
#9179=LINE('',#76904,#12016);
#9180=LINE('',#76906,#12017);
#9181=LINE('',#76907,#12018);
#9182=LINE('',#76910,#12019);
#9183=LINE('',#76912,#12020);
#9184=LINE('',#76913,#12021);
#9185=LINE('',#76916,#12022);
#9186=LINE('',#76918,#12023);
#9187=LINE('',#76919,#12024);
#9188=LINE('',#76921,#12025);
#9189=LINE('',#76922,#12026);
#9190=LINE('',#76928,#12027);
#9191=LINE('',#76934,#12028);
#9192=LINE('',#76939,#12029);
#9193=LINE('',#76941,#12030);
#9194=LINE('',#76943,#12031);
#9195=LINE('',#76944,#12032);
#9196=LINE('',#76947,#12033);
#9197=LINE('',#76949,#12034);
#9198=LINE('',#76950,#12035);
#9199=LINE('',#76953,#12036);
#9200=LINE('',#76955,#12037);
#9201=LINE('',#76956,#12038);
#9202=LINE('',#76959,#12039);
#9203=LINE('',#76961,#12040);
#9204=LINE('',#76962,#12041);
#9205=LINE('',#76965,#12042);
#9206=LINE('',#76967,#12043);
#9207=LINE('',#76968,#12044);
#9208=LINE('',#76971,#12045);
#9209=LINE('',#76973,#12046);
#9210=LINE('',#76974,#12047);
#9211=LINE('',#76977,#12048);
#9212=LINE('',#76979,#12049);
#9213=LINE('',#76980,#12050);
#9214=LINE('',#76982,#12051);
#9215=LINE('',#76983,#12052);
#9216=LINE('',#77002,#12053);
#9217=LINE('',#77006,#12054);
#9218=LINE('',#77008,#12055);
#9219=LINE('',#77010,#12056);
#9220=LINE('',#77012,#12057);
#9221=LINE('',#77013,#12058);
#9222=LINE('',#77016,#12059);
#9223=LINE('',#77020,#12060);
#9224=LINE('',#77024,#12061);
#9225=LINE('',#77028,#12062);
#9226=LINE('',#77042,#12063);
#9227=LINE('',#77044,#12064);
#9228=LINE('',#77045,#12065);
#9229=LINE('',#77047,#12066);
#9230=LINE('',#77049,#12067);
#9231=LINE('',#77050,#12068);
#9232=LINE('',#77052,#12069);
#9233=LINE('',#77054,#12070);
#9234=LINE('',#77055,#12071);
#9235=LINE('',#77068,#12072);
#9236=LINE('',#77076,#12073);
#9237=LINE('',#77084,#12074);
#9238=LINE('',#77085,#12075);
#9239=LINE('',#77087,#12076);
#9240=LINE('',#77088,#12077);
#9241=LINE('',#77089,#12078);
#9242=LINE('',#77093,#12079);
#9243=LINE('',#77094,#12080);
#9244=LINE('',#77095,#12081);
#9245=LINE('',#77102,#12082);
#9246=LINE('',#77106,#12083);
#9247=LINE('',#77107,#12084);
#9248=LINE('',#77113,#12085);
#9249=LINE('',#77114,#12086);
#9250=LINE('',#77115,#12087);
#9251=LINE('',#77122,#12088);
#9252=LINE('',#77126,#12089);
#9253=LINE('',#77127,#12090);
#9254=LINE('',#77132,#12091);
#9255=LINE('',#77133,#12092);
#9256=LINE('',#77134,#12093);
#9257=LINE('',#77136,#12094);
#9258=LINE('',#77137,#12095);
#9259=LINE('',#77140,#12096);
#9260=LINE('',#77141,#12097);
#9261=LINE('',#77144,#12098);
#9262=LINE('',#77145,#12099);
#9263=LINE('',#77147,#12100);
#9264=LINE('',#77149,#12101);
#9265=LINE('',#77150,#12102);
#9266=LINE('',#77157,#12103);
#9267=LINE('',#77253,#12104);
#9268=LINE('',#77643,#12105);
#9269=LINE('',#78042,#12106);
#9270=LINE('',#78422,#12107);
#9271=LINE('',#78777,#12108);
#9272=LINE('',#79143,#12109);
#9273=LINE('',#79502,#12110);
#9274=LINE('',#79886,#12111);
#9275=LINE('',#80256,#12112);
#9276=LINE('',#80489,#12113);
#9277=LINE('',#80835,#12114);
#9278=LINE('',#81169,#12115);
#9279=LINE('',#81506,#12116);
#9280=LINE('',#81844,#12117);
#9281=LINE('',#82194,#12118);
#9282=LINE('',#82543,#12119);
#9283=LINE('',#84080,#12120);
#9284=LINE('',#84084,#12121);
#9285=LINE('',#84086,#12122);
#9286=LINE('',#84090,#12123);
#9287=LINE('',#84093,#12124);
#9288=LINE('',#84096,#12125);
#9289=LINE('',#84098,#12126);
#9290=LINE('',#84102,#12127);
#9291=LINE('',#84105,#12128);
#9292=LINE('',#84108,#12129);
#9293=LINE('',#84110,#12130);
#9294=LINE('',#84114,#12131);
#9295=LINE('',#84117,#12132);
#9296=LINE('',#84119,#12133);
#9297=LINE('',#84121,#12134);
#9298=LINE('',#84123,#12135);
#9299=LINE('',#84124,#12136);
#9300=LINE('',#84126,#12137);
#9301=LINE('',#84128,#12138);
#9302=LINE('',#84129,#12139);
#9303=LINE('',#84131,#12140);
#9304=LINE('',#84133,#12141);
#9305=LINE('',#84134,#12142);
#9306=LINE('',#84138,#12143);
#9307=LINE('',#84141,#12144);
#9308=LINE('',#84143,#12145);
#9309=LINE('',#84147,#12146);
#9310=LINE('',#84150,#12147);
#9311=LINE('',#84159,#12148);
#9312=LINE('',#84163,#12149);
#9313=LINE('',#84165,#12150);
#9314=LINE('',#84166,#12151);
#9315=LINE('',#84173,#12152);
#9316=LINE('',#84176,#12153);
#9317=LINE('',#84184,#12154);
#9318=LINE('',#84188,#12155);
#9319=LINE('',#84195,#12156);
#9320=LINE('',#84197,#12157);
#9321=LINE('',#84199,#12158);
#9322=LINE('',#84200,#12159);
#9323=LINE('',#84203,#12160);
#9324=LINE('',#84208,#12161);
#9325=LINE('',#84212,#12162);
#9326=LINE('',#84219,#12163);
#9327=LINE('',#84221,#12164);
#9328=LINE('',#84223,#12165);
#9329=LINE('',#84224,#12166);
#9330=LINE('',#84227,#12167);
#9331=LINE('',#84232,#12168);
#9332=LINE('',#84236,#12169);
#9333=LINE('',#84238,#12170);
#9334=LINE('',#84239,#12171);
#9335=LINE('',#84241,#12172);
#9336=LINE('',#84243,#12173);
#9337=LINE('',#84244,#12174);
#9338=LINE('',#84255,#12175);
#9339=LINE('',#84260,#12176);
#9340=LINE('',#84263,#12177);
#9341=LINE('',#84267,#12178);
#9342=LINE('',#84270,#12179);
#9343=LINE('',#84274,#12180);
#9344=LINE('',#84277,#12181);
#9345=LINE('',#84282,#12182);
#9346=LINE('',#84285,#12183);
#9347=LINE('',#84295,#12184);
#9348=LINE('',#84299,#12185);
#9349=LINE('',#84305,#12186);
#9350=LINE('',#84310,#12187);
#9351=LINE('',#84313,#12188);
#9352=LINE('',#84315,#12189);
#9353=LINE('',#84317,#12190);
#9354=LINE('',#84318,#12191);
#9355=LINE('',#84320,#12192);
#9356=LINE('',#84321,#12193);
#9357=LINE('',#84323,#12194);
#9358=LINE('',#84325,#12195);
#9359=LINE('',#84327,#12196);
#9360=LINE('',#84329,#12197);
#9361=LINE('',#84331,#12198);
#9362=LINE('',#84338,#12199);
#9363=LINE('',#84446,#12200);
#9364=LINE('',#84872,#12201);
#9365=LINE('',#85332,#12202);
#9366=LINE('',#85822,#12203);
#9367=LINE('',#86288,#12204);
#9368=LINE('',#86748,#12205);
#9369=LINE('',#87218,#12206);
#9370=LINE('',#87702,#12207);
#9371=LINE('',#88166,#12208);
#9372=LINE('',#88640,#12209);
#9373=LINE('',#89108,#12210);
#9374=LINE('',#89566,#12211);
#9375=LINE('',#90008,#12212);
#9376=LINE('',#90484,#12213);
#9377=LINE('',#90948,#12214);
#9378=LINE('',#91392,#12215);
#9379=LINE('',#91868,#12216);
#9380=LINE('',#92312,#12217);
#9381=LINE('',#92786,#12218);
#9382=LINE('',#93292,#12219);
#9383=LINE('',#93762,#12220);
#9384=LINE('',#94226,#12221);
#9385=LINE('',#94687,#12222);
#9386=LINE('',#94890,#12223);
#9387=LINE('',#95364,#12224);
#9388=LINE('',#95794,#12225);
#9389=LINE('',#96222,#12226);
#9390=LINE('',#96665,#12227);
#9391=LINE('',#97106,#12228);
#9392=LINE('',#97548,#12229);
#9393=LINE('',#97972,#12230);
#9394=LINE('',#98398,#12231);
#9395=LINE('',#98846,#12232);
#9396=LINE('',#99304,#12233);
#9397=LINE('',#99730,#12234);
#9398=LINE('',#100162,#12235);
#9399=LINE('',#100586,#12236);
#9400=LINE('',#101043,#12237);
#9401=LINE('',#101461,#12238);
#9402=LINE('',#101885,#12239);
#9403=LINE('',#102321,#12240);
#9404=LINE('',#102739,#12241);
#9405=LINE('',#103177,#12242);
#9406=LINE('',#103636,#12243);
#9407=LINE('',#104050,#12244);
#9408=LINE('',#106664,#12245);
#9409=LINE('',#106672,#12246);
#9410=LINE('',#106673,#12247);
#9411=LINE('',#106676,#12248);
#9412=LINE('',#106678,#12249);
#9413=LINE('',#106684,#12250);
#9414=LINE('',#106693,#12251);
#9415=LINE('',#106700,#12252);
#9416=LINE('',#106704,#12253);
#9417=LINE('',#106708,#12254);
#9418=LINE('',#106712,#12255);
#9419=LINE('',#106716,#12256);
#9420=LINE('',#106720,#12257);
#9421=LINE('',#106724,#12258);
#9422=LINE('',#106728,#12259);
#9423=LINE('',#106732,#12260);
#9424=LINE('',#106736,#12261);
#9425=LINE('',#106740,#12262);
#9426=LINE('',#106744,#12263);
#9427=LINE('',#106748,#12264);
#9428=LINE('',#106752,#12265);
#9429=LINE('',#106756,#12266);
#9430=LINE('',#106760,#12267);
#9431=LINE('',#106764,#12268);
#9432=LINE('',#106768,#12269);
#9433=LINE('',#106772,#12270);
#9434=LINE('',#106776,#12271);
#9435=LINE('',#106780,#12272);
#9436=LINE('',#106784,#12273);
#9437=LINE('',#106788,#12274);
#9438=LINE('',#106792,#12275);
#9439=LINE('',#106796,#12276);
#9440=LINE('',#106800,#12277);
#9441=LINE('',#106804,#12278);
#9442=LINE('',#106808,#12279);
#9443=LINE('',#106812,#12280);
#9444=LINE('',#106816,#12281);
#9445=LINE('',#106820,#12282);
#9446=LINE('',#106824,#12283);
#9447=LINE('',#106828,#12284);
#9448=LINE('',#106833,#12285);
#9449=LINE('',#106837,#12286);
#9450=LINE('',#106841,#12287);
#9451=LINE('',#106845,#12288);
#9452=LINE('',#106849,#12289);
#9453=LINE('',#106853,#12290);
#9454=LINE('',#106857,#12291);
#9455=LINE('',#106861,#12292);
#9456=LINE('',#106865,#12293);
#9457=LINE('',#106869,#12294);
#9458=LINE('',#106873,#12295);
#9459=LINE('',#106877,#12296);
#9460=LINE('',#106881,#12297);
#9461=LINE('',#106885,#12298);
#9462=LINE('',#106889,#12299);
#9463=LINE('',#106893,#12300);
#9464=LINE('',#106897,#12301);
#9465=LINE('',#106901,#12302);
#9466=LINE('',#106905,#12303);
#9467=LINE('',#106909,#12304);
#9468=LINE('',#106913,#12305);
#9469=LINE('',#106917,#12306);
#9470=LINE('',#106921,#12307);
#9471=LINE('',#106925,#12308);
#9472=LINE('',#106929,#12309);
#9473=LINE('',#106933,#12310);
#9474=LINE('',#106937,#12311);
#9475=LINE('',#106941,#12312);
#9476=LINE('',#106945,#12313);
#9477=LINE('',#106949,#12314);
#9478=LINE('',#106953,#12315);
#9479=LINE('',#106957,#12316);
#9480=LINE('',#106961,#12317);
#9481=LINE('',#106965,#12318);
#9482=LINE('',#106969,#12319);
#9483=LINE('',#106973,#12320);
#9484=LINE('',#106976,#12321);
#9485=LINE('',#106979,#12322);
#9486=LINE('',#106981,#12323);
#9487=LINE('',#106989,#12324);
#9488=LINE('',#107231,#12325);
#9489=LINE('',#107235,#12326);
#9490=LINE('',#107236,#12327);
#9491=LINE('',#107238,#12328);
#9492=LINE('',#107242,#12329);
#9493=LINE('',#107243,#12330);
#9494=LINE('',#107245,#12331);
#9495=LINE('',#107249,#12332);
#9496=LINE('',#107250,#12333);
#9497=LINE('',#107252,#12334);
#9498=LINE('',#107256,#12335);
#9499=LINE('',#107257,#12336);
#9500=LINE('',#107259,#12337);
#9501=LINE('',#107263,#12338);
#9502=LINE('',#107264,#12339);
#9503=LINE('',#107266,#12340);
#9504=LINE('',#107270,#12341);
#9505=LINE('',#107271,#12342);
#9506=LINE('',#107273,#12343);
#9507=LINE('',#107277,#12344);
#9508=LINE('',#107278,#12345);
#9509=LINE('',#107280,#12346);
#9510=LINE('',#107284,#12347);
#9511=LINE('',#107285,#12348);
#9512=LINE('',#107287,#12349);
#9513=LINE('',#107291,#12350);
#9514=LINE('',#107292,#12351);
#9515=LINE('',#107294,#12352);
#9516=LINE('',#107298,#12353);
#9517=LINE('',#107299,#12354);
#9518=LINE('',#107301,#12355);
#9519=LINE('',#107305,#12356);
#9520=LINE('',#107306,#12357);
#9521=LINE('',#107308,#12358);
#9522=LINE('',#107312,#12359);
#9523=LINE('',#107313,#12360);
#9524=LINE('',#107315,#12361);
#9525=LINE('',#107319,#12362);
#9526=LINE('',#107320,#12363);
#9527=LINE('',#107322,#12364);
#9528=LINE('',#107326,#12365);
#9529=LINE('',#107327,#12366);
#9530=LINE('',#107329,#12367);
#9531=LINE('',#107333,#12368);
#9532=LINE('',#107334,#12369);
#9533=LINE('',#107336,#12370);
#9534=LINE('',#107340,#12371);
#9535=LINE('',#107341,#12372);
#9536=LINE('',#107343,#12373);
#9537=LINE('',#107347,#12374);
#9538=LINE('',#107348,#12375);
#9539=LINE('',#107350,#12376);
#9540=LINE('',#107354,#12377);
#9541=LINE('',#107355,#12378);
#9542=LINE('',#107357,#12379);
#9543=LINE('',#107361,#12380);
#9544=LINE('',#107362,#12381);
#9545=LINE('',#107364,#12382);
#9546=LINE('',#107368,#12383);
#9547=LINE('',#107369,#12384);
#9548=LINE('',#107371,#12385);
#9549=LINE('',#107375,#12386);
#9550=LINE('',#107376,#12387);
#9551=LINE('',#107378,#12388);
#9552=LINE('',#107382,#12389);
#9553=LINE('',#107383,#12390);
#9554=LINE('',#107385,#12391);
#9555=LINE('',#107389,#12392);
#9556=LINE('',#107390,#12393);
#9557=LINE('',#107392,#12394);
#9558=LINE('',#107396,#12395);
#9559=LINE('',#107397,#12396);
#9560=LINE('',#107399,#12397);
#9561=LINE('',#107403,#12398);
#9562=LINE('',#107404,#12399);
#9563=LINE('',#107406,#12400);
#9564=LINE('',#107410,#12401);
#9565=LINE('',#107411,#12402);
#9566=LINE('',#107413,#12403);
#9567=LINE('',#107417,#12404);
#9568=LINE('',#107418,#12405);
#9569=LINE('',#107420,#12406);
#9570=LINE('',#107424,#12407);
#9571=LINE('',#107425,#12408);
#9572=LINE('',#107427,#12409);
#9573=LINE('',#107431,#12410);
#9574=LINE('',#107432,#12411);
#9575=LINE('',#107434,#12412);
#9576=LINE('',#107438,#12413);
#9577=LINE('',#107439,#12414);
#9578=LINE('',#107441,#12415);
#9579=LINE('',#107445,#12416);
#9580=LINE('',#107446,#12417);
#9581=LINE('',#107448,#12418);
#9582=LINE('',#107452,#12419);
#9583=LINE('',#107453,#12420);
#9584=LINE('',#107455,#12421);
#9585=LINE('',#107459,#12422);
#9586=LINE('',#107460,#12423);
#9587=LINE('',#107462,#12424);
#9588=LINE('',#107466,#12425);
#9589=LINE('',#107467,#12426);
#9590=LINE('',#107469,#12427);
#9591=LINE('',#107537,#12428);
#9592=LINE('',#107540,#12429);
#9593=LINE('',#107542,#12430);
#9594=LINE('',#107546,#12431);
#9595=LINE('',#107549,#12432);
#9596=LINE('',#107552,#12433);
#9597=LINE('',#107554,#12434);
#9598=LINE('',#107558,#12435);
#9599=LINE('',#107561,#12436);
#9600=LINE('',#107564,#12437);
#9601=LINE('',#107566,#12438);
#9602=LINE('',#107570,#12439);
#9603=LINE('',#107573,#12440);
#9604=LINE('',#107575,#12441);
#9605=LINE('',#107577,#12442);
#9606=LINE('',#107579,#12443);
#9607=LINE('',#107580,#12444);
#9608=LINE('',#107582,#12445);
#9609=LINE('',#107584,#12446);
#9610=LINE('',#107585,#12447);
#9611=LINE('',#107587,#12448);
#9612=LINE('',#107589,#12449);
#9613=LINE('',#107590,#12450);
#9614=LINE('',#107594,#12451);
#9615=LINE('',#107597,#12452);
#9616=LINE('',#107599,#12453);
#9617=LINE('',#107603,#12454);
#9618=LINE('',#107606,#12455);
#9619=LINE('',#107615,#12456);
#9620=LINE('',#107619,#12457);
#9621=LINE('',#107621,#12458);
#9622=LINE('',#107622,#12459);
#9623=LINE('',#107629,#12460);
#9624=LINE('',#107793,#12461);
#9625=LINE('',#108213,#12462);
#9626=LINE('',#108665,#12463);
#9627=LINE('',#109119,#12464);
#9628=LINE('',#109553,#12465);
#9629=LINE('',#109989,#12466);
#9630=LINE('',#110498,#12467);
#9631=LINE('',#110946,#12468);
#9632=LINE('',#111392,#12469);
#9633=LINE('',#111849,#12470);
#9634=LINE('',#112309,#12471);
#9635=LINE('',#112761,#12472);
#9636=LINE('',#113257,#12473);
#9637=LINE('',#113691,#12474);
#9638=LINE('',#114151,#12475);
#9639=LINE('',#114548,#12476);
#9640=LINE('',#114990,#12477);
#9641=LINE('',#115432,#12478);
#9642=LINE('',#115832,#12479);
#9643=LINE('',#116052,#12480);
#9644=LINE('',#116529,#12481);
#9645=LINE('',#116947,#12482);
#9646=LINE('',#117361,#12483);
#9647=LINE('',#117835,#12484);
#9648=LINE('',#118270,#12485);
#9649=LINE('',#118700,#12486);
#9650=LINE('',#119140,#12487);
#9651=LINE('',#119570,#12488);
#9652=LINE('',#120080,#12489);
#9653=LINE('',#120512,#12490);
#9654=LINE('',#120930,#12491);
#9655=LINE('',#121376,#12492);
#9656=LINE('',#121842,#12493);
#9657=LINE('',#122269,#12494);
#9658=LINE('',#122693,#12495);
#9659=LINE('',#123121,#12496);
#9660=LINE('',#123562,#12497);
#9661=LINE('',#125944,#12498);
#9662=LINE('',#125952,#12499);
#9663=LINE('',#125953,#12500);
#9664=LINE('',#125956,#12501);
#9665=LINE('',#125958,#12502);
#9666=LINE('',#125964,#12503);
#9667=LINE('',#125973,#12504);
#9668=LINE('',#125980,#12505);
#9669=LINE('',#125984,#12506);
#9670=LINE('',#125988,#12507);
#9671=LINE('',#125992,#12508);
#9672=LINE('',#125996,#12509);
#9673=LINE('',#126000,#12510);
#9674=LINE('',#126004,#12511);
#9675=LINE('',#126008,#12512);
#9676=LINE('',#126012,#12513);
#9677=LINE('',#126016,#12514);
#9678=LINE('',#126020,#12515);
#9679=LINE('',#126024,#12516);
#9680=LINE('',#126028,#12517);
#9681=LINE('',#126032,#12518);
#9682=LINE('',#126036,#12519);
#9683=LINE('',#126040,#12520);
#9684=LINE('',#126044,#12521);
#9685=LINE('',#126048,#12522);
#9686=LINE('',#126052,#12523);
#9687=LINE('',#126056,#12524);
#9688=LINE('',#126060,#12525);
#9689=LINE('',#126064,#12526);
#9690=LINE('',#126068,#12527);
#9691=LINE('',#126072,#12528);
#9692=LINE('',#126076,#12529);
#9693=LINE('',#126080,#12530);
#9694=LINE('',#126084,#12531);
#9695=LINE('',#126088,#12532);
#9696=LINE('',#126092,#12533);
#9697=LINE('',#126096,#12534);
#9698=LINE('',#126100,#12535);
#9699=LINE('',#126104,#12536);
#9700=LINE('',#126108,#12537);
#9701=LINE('',#126113,#12538);
#9702=LINE('',#126117,#12539);
#9703=LINE('',#126121,#12540);
#9704=LINE('',#126125,#12541);
#9705=LINE('',#126129,#12542);
#9706=LINE('',#126133,#12543);
#9707=LINE('',#126137,#12544);
#9708=LINE('',#126141,#12545);
#9709=LINE('',#126145,#12546);
#9710=LINE('',#126149,#12547);
#9711=LINE('',#126153,#12548);
#9712=LINE('',#126157,#12549);
#9713=LINE('',#126161,#12550);
#9714=LINE('',#126165,#12551);
#9715=LINE('',#126169,#12552);
#9716=LINE('',#126173,#12553);
#9717=LINE('',#126177,#12554);
#9718=LINE('',#126181,#12555);
#9719=LINE('',#126185,#12556);
#9720=LINE('',#126189,#12557);
#9721=LINE('',#126193,#12558);
#9722=LINE('',#126197,#12559);
#9723=LINE('',#126201,#12560);
#9724=LINE('',#126205,#12561);
#9725=LINE('',#126209,#12562);
#9726=LINE('',#126213,#12563);
#9727=LINE('',#126217,#12564);
#9728=LINE('',#126221,#12565);
#9729=LINE('',#126225,#12566);
#9730=LINE('',#126229,#12567);
#9731=LINE('',#126233,#12568);
#9732=LINE('',#126237,#12569);
#9733=LINE('',#126241,#12570);
#9734=LINE('',#126245,#12571);
#9735=LINE('',#126249,#12572);
#9736=LINE('',#126253,#12573);
#9737=LINE('',#126256,#12574);
#9738=LINE('',#126259,#12575);
#9739=LINE('',#126261,#12576);
#9740=LINE('',#126269,#12577);
#9741=LINE('',#126511,#12578);
#9742=LINE('',#126515,#12579);
#9743=LINE('',#126516,#12580);
#9744=LINE('',#126518,#12581);
#9745=LINE('',#126522,#12582);
#9746=LINE('',#126523,#12583);
#9747=LINE('',#126525,#12584);
#9748=LINE('',#126529,#12585);
#9749=LINE('',#126530,#12586);
#9750=LINE('',#126532,#12587);
#9751=LINE('',#126536,#12588);
#9752=LINE('',#126537,#12589);
#9753=LINE('',#126539,#12590);
#9754=LINE('',#126543,#12591);
#9755=LINE('',#126544,#12592);
#9756=LINE('',#126546,#12593);
#9757=LINE('',#126550,#12594);
#9758=LINE('',#126551,#12595);
#9759=LINE('',#126553,#12596);
#9760=LINE('',#126557,#12597);
#9761=LINE('',#126558,#12598);
#9762=LINE('',#126560,#12599);
#9763=LINE('',#126564,#12600);
#9764=LINE('',#126565,#12601);
#9765=LINE('',#126567,#12602);
#9766=LINE('',#126571,#12603);
#9767=LINE('',#126572,#12604);
#9768=LINE('',#126574,#12605);
#9769=LINE('',#126578,#12606);
#9770=LINE('',#126579,#12607);
#9771=LINE('',#126581,#12608);
#9772=LINE('',#126585,#12609);
#9773=LINE('',#126586,#12610);
#9774=LINE('',#126588,#12611);
#9775=LINE('',#126592,#12612);
#9776=LINE('',#126593,#12613);
#9777=LINE('',#126595,#12614);
#9778=LINE('',#126599,#12615);
#9779=LINE('',#126600,#12616);
#9780=LINE('',#126602,#12617);
#9781=LINE('',#126606,#12618);
#9782=LINE('',#126607,#12619);
#9783=LINE('',#126609,#12620);
#9784=LINE('',#126613,#12621);
#9785=LINE('',#126614,#12622);
#9786=LINE('',#126616,#12623);
#9787=LINE('',#126620,#12624);
#9788=LINE('',#126621,#12625);
#9789=LINE('',#126623,#12626);
#9790=LINE('',#126627,#12627);
#9791=LINE('',#126628,#12628);
#9792=LINE('',#126630,#12629);
#9793=LINE('',#126634,#12630);
#9794=LINE('',#126635,#12631);
#9795=LINE('',#126637,#12632);
#9796=LINE('',#126641,#12633);
#9797=LINE('',#126642,#12634);
#9798=LINE('',#126644,#12635);
#9799=LINE('',#126648,#12636);
#9800=LINE('',#126649,#12637);
#9801=LINE('',#126651,#12638);
#9802=LINE('',#126655,#12639);
#9803=LINE('',#126656,#12640);
#9804=LINE('',#126658,#12641);
#9805=LINE('',#126662,#12642);
#9806=LINE('',#126663,#12643);
#9807=LINE('',#126665,#12644);
#9808=LINE('',#126669,#12645);
#9809=LINE('',#126670,#12646);
#9810=LINE('',#126672,#12647);
#9811=LINE('',#126676,#12648);
#9812=LINE('',#126677,#12649);
#9813=LINE('',#126679,#12650);
#9814=LINE('',#126683,#12651);
#9815=LINE('',#126684,#12652);
#9816=LINE('',#126686,#12653);
#9817=LINE('',#126690,#12654);
#9818=LINE('',#126691,#12655);
#9819=LINE('',#126693,#12656);
#9820=LINE('',#126697,#12657);
#9821=LINE('',#126698,#12658);
#9822=LINE('',#126700,#12659);
#9823=LINE('',#126704,#12660);
#9824=LINE('',#126705,#12661);
#9825=LINE('',#126707,#12662);
#9826=LINE('',#126711,#12663);
#9827=LINE('',#126712,#12664);
#9828=LINE('',#126714,#12665);
#9829=LINE('',#126718,#12666);
#9830=LINE('',#126719,#12667);
#9831=LINE('',#126721,#12668);
#9832=LINE('',#126725,#12669);
#9833=LINE('',#126726,#12670);
#9834=LINE('',#126728,#12671);
#9835=LINE('',#126732,#12672);
#9836=LINE('',#126733,#12673);
#9837=LINE('',#126735,#12674);
#9838=LINE('',#126739,#12675);
#9839=LINE('',#126740,#12676);
#9840=LINE('',#126742,#12677);
#9841=LINE('',#126746,#12678);
#9842=LINE('',#126747,#12679);
#9843=LINE('',#126749,#12680);
#9844=LINE('',#126817,#12681);
#9845=LINE('',#126820,#12682);
#9846=LINE('',#126822,#12683);
#9847=LINE('',#126826,#12684);
#9848=LINE('',#126829,#12685);
#9849=LINE('',#126832,#12686);
#9850=LINE('',#126834,#12687);
#9851=LINE('',#126838,#12688);
#9852=LINE('',#126841,#12689);
#9853=LINE('',#126844,#12690);
#9854=LINE('',#126846,#12691);
#9855=LINE('',#126850,#12692);
#9856=LINE('',#126853,#12693);
#9857=LINE('',#126855,#12694);
#9858=LINE('',#126857,#12695);
#9859=LINE('',#126859,#12696);
#9860=LINE('',#126860,#12697);
#9861=LINE('',#126862,#12698);
#9862=LINE('',#126864,#12699);
#9863=LINE('',#126865,#12700);
#9864=LINE('',#126867,#12701);
#9865=LINE('',#126869,#12702);
#9866=LINE('',#126870,#12703);
#9867=LINE('',#126874,#12704);
#9868=LINE('',#126877,#12705);
#9869=LINE('',#126879,#12706);
#9870=LINE('',#126883,#12707);
#9871=LINE('',#126886,#12708);
#9872=LINE('',#126895,#12709);
#9873=LINE('',#126899,#12710);
#9874=LINE('',#126901,#12711);
#9875=LINE('',#126902,#12712);
#9876=LINE('',#126909,#12713);
#9877=LINE('',#126996,#12714);
#9878=LINE('',#127369,#12715);
#9879=LINE('',#127731,#12716);
#9880=LINE('',#128103,#12717);
#9881=LINE('',#128439,#12718);
#9882=LINE('',#128795,#12719);
#9883=LINE('',#129163,#12720);
#9884=LINE('',#129519,#12721);
#9885=LINE('',#129871,#12722);
#9886=LINE('',#130211,#12723);
#9887=LINE('',#130587,#12724);
#9888=LINE('',#130642,#12725);
#9889=LINE('',#131007,#12726);
#9890=LINE('',#131376,#12727);
#9891=LINE('',#131745,#12728);
#9892=LINE('',#132100,#12729);
#9893=LINE('',#132464,#12730);
#9894=LINE('',#132843,#12731);
#9895=LINE('',#133216,#12732);
#9896=LINE('',#133579,#12733);
#9897=LINE('',#135183,#12734);
#9898=LINE('',#135187,#12735);
#9899=LINE('',#135191,#12736);
#9900=LINE('',#135193,#12737);
#9901=LINE('',#135199,#12738);
#9902=LINE('',#135205,#12739);
#9903=LINE('',#135211,#12740);
#9904=LINE('',#135216,#12741);
#9905=LINE('',#135218,#12742);
#9906=LINE('',#135230,#12743);
#9907=VECTOR('',#34232,1.65);
#9908=VECTOR('',#34237,10.);
#9909=VECTOR('',#34238,10.);
#9910=VECTOR('',#34239,10.);
#9911=VECTOR('',#34240,10.);
#9912=VECTOR('',#34241,10.);
#9913=VECTOR('',#34242,10.);
#9914=VECTOR('',#34243,10.);
#9915=VECTOR('',#34244,10.);
#9916=VECTOR('',#34245,9.99999999999998);
#9917=VECTOR('',#34246,10.);
#9918=VECTOR('',#34247,9.99999999999998);
#9919=VECTOR('',#34248,10.);
#9920=VECTOR('',#34249,10.);
#9921=VECTOR('',#34250,10.);
#9922=VECTOR('',#34251,9.99999999999998);
#9923=VECTOR('',#34252,10.);
#9924=VECTOR('',#34257,1.55);
#9925=VECTOR('',#34264,1.65);
#9926=VECTOR('',#34267,1.55);
#9927=VECTOR('',#34272,1.55);
#9928=VECTOR('',#34275,1.55);
#9929=VECTOR('',#34280,1.65);
#9930=VECTOR('',#34285,10.);
#9931=VECTOR('',#34286,10.);
#9932=VECTOR('',#34287,9.99999999999998);
#9933=VECTOR('',#34288,10.);
#9934=VECTOR('',#34289,10.);
#9935=VECTOR('',#34290,10.);
#9936=VECTOR('',#34291,9.99999999999998);
#9937=VECTOR('',#34292,10.);
#9938=VECTOR('',#34293,9.99999999999998);
#9939=VECTOR('',#34294,10.);
#9940=VECTOR('',#34295,10.);
#9941=VECTOR('',#34296,10.);
#9942=VECTOR('',#34297,10.);
#9943=VECTOR('',#34298,10.);
#9944=VECTOR('',#34299,10.);
#9945=VECTOR('',#34300,10.);
#9946=VECTOR('',#34305,1.55);
#9947=VECTOR('',#34312,1.65);
#9948=VECTOR('',#34315,1.55);
#9949=VECTOR('',#34320,0.775000000000001);
#9950=VECTOR('',#34323,0.775);
#9951=VECTOR('',#34326,10.);
#9952=VECTOR('',#34327,10.);
#9953=VECTOR('',#34330,10.);
#9954=VECTOR('',#34333,10.);
#9955=VECTOR('',#34334,10.);
#9956=VECTOR('',#34337,10.);
#9957=VECTOR('',#34340,10.);
#9958=VECTOR('',#34343,10.);
#9959=VECTOR('',#34344,10.);
#9960=VECTOR('',#34347,10.);
#9961=VECTOR('',#34350,10.);
#9962=VECTOR('',#34353,10.);
#9963=VECTOR('',#34360,10.);
#9964=VECTOR('',#34363,10.);
#9965=VECTOR('',#34366,10.);
#9966=VECTOR('',#34369,10.);
#9967=VECTOR('',#34378,1.125);
#9968=VECTOR('',#34383,10.);
#9969=VECTOR('',#34384,10.);
#9970=VECTOR('',#34385,10.);
#9971=VECTOR('',#34386,10.);
#9972=VECTOR('',#34391,1.05);
#9973=VECTOR('',#34400,1.125);
#9974=VECTOR('',#34403,1.05);
#9975=VECTOR('',#34410,0.524999999999993);
#9976=VECTOR('',#34413,0.524999999999993);
#9977=VECTOR('',#34418,1.125);
#9978=VECTOR('',#34423,10.);
#9979=VECTOR('',#34424,10.);
#9980=VECTOR('',#34425,10.);
#9981=VECTOR('',#34426,10.);
#9982=VECTOR('',#34447,1.05);
#9983=VECTOR('',#34454,1.125);
#9984=VECTOR('',#34457,1.05);
#9985=VECTOR('',#34464,1.125);
#9986=VECTOR('',#34467,1.05);
#9987=VECTOR('',#34474,1.125);
#9988=VECTOR('',#34477,1.05);
#9989=VECTOR('',#34482,0.525);
#9990=VECTOR('',#34485,0.525);
#9991=VECTOR('',#34488,0.525);
#9992=VECTOR('',#34491,0.525);
#9993=VECTOR('',#34496,2.2);
#9994=VECTOR('',#34499,2.05);
#9995=VECTOR('',#34506,2.2);
#9996=VECTOR('',#34509,2.05);
#9997=VECTOR('',#34516,2.2);
#9998=VECTOR('',#34519,2.05);
#9999=VECTOR('',#34526,2.2);
#10000=VECTOR('',#34529,2.05);
#10001=VECTOR('',#34536,2.2);
#10002=VECTOR('',#34539,2.05);
#10003=VECTOR('',#34546,2.2);
#10004=VECTOR('',#34549,2.05);
#10005=VECTOR('',#34554,1.025);
#10006=VECTOR('',#34557,1.025);
#10007=VECTOR('',#34560,1.025);
#10008=VECTOR('',#34563,1.025);
#10009=VECTOR('',#34566,1.025);
#10010=VECTOR('',#34569,1.025);
#10011=VECTOR('',#34572,10.);
#10012=VECTOR('',#34575,10.);
#10013=VECTOR('',#34580,10.);
#10014=VECTOR('',#34581,10.);
#10015=VECTOR('',#34582,10.);
#10016=VECTOR('',#34583,10.);
#10017=VECTOR('',#34586,10.);
#10018=VECTOR('',#34587,10.);
#10019=VECTOR('',#34588,10.);
#10020=VECTOR('',#34589,10.);
#10021=VECTOR('',#34590,10.);
#10022=VECTOR('',#34591,10.);
#10023=VECTOR('',#34592,10.);
#10024=VECTOR('',#34593,10.);
#10025=VECTOR('',#34596,10.);
#10026=VECTOR('',#34605,10.);
#10027=VECTOR('',#34608,10.);
#10028=VECTOR('',#34617,4.5);
#10029=VECTOR('',#34624,10.);
#10030=VECTOR('',#34625,10.);
#10031=VECTOR('',#34626,10.);
#10032=VECTOR('',#34629,10.);
#10033=VECTOR('',#34630,10.);
#10034=VECTOR('',#34633,10.);
#10035=VECTOR('',#34638,10.);
#10036=VECTOR('',#34639,10.);
#10037=VECTOR('',#34642,10.);
#10038=VECTOR('',#34643,10.);
#10039=VECTOR('',#34644,10.);
#10040=VECTOR('',#34645,10.);
#10041=VECTOR('',#34646,10.);
#10042=VECTOR('',#34647,10.);
#10043=VECTOR('',#34650,10.);
#10044=VECTOR('',#34651,10.);
#10045=VECTOR('',#34654,10.);
#10046=VECTOR('',#34655,10.);
#10047=VECTOR('',#34658,10.);
#10048=VECTOR('',#34659,10.);
#10049=VECTOR('',#34662,10.);
#10050=VECTOR('',#34663,10.);
#10051=VECTOR('',#34666,10.);
#10052=VECTOR('',#34667,10.);
#10053=VECTOR('',#34670,10.);
#10054=VECTOR('',#34681,2.675);
#10055=VECTOR('',#34688,2.525);
#10056=VECTOR('',#34699,2.675);
#10057=VECTOR('',#34710,4.35);
#10058=VECTOR('',#34715,4.5);
#10059=VECTOR('',#34718,4.35);
#10060=VECTOR('',#34723,2.5);
#10061=VECTOR('',#34726,2.5);
#10062=VECTOR('',#34727,10.);
#10063=VECTOR('',#34730,2.5);
#10064=VECTOR('',#34733,2.5);
#10065=VECTOR('',#34736,2.5);
#10066=VECTOR('',#34739,2.5);
#10067=VECTOR('',#34742,2.5);
#10068=VECTOR('',#34745,2.5);
#10069=VECTOR('',#34748,2.5);
#10070=VECTOR('',#34751,2.5);
#10071=VECTOR('',#34754,2.5);
#10072=VECTOR('',#34757,2.5);
#10073=VECTOR('',#34760,2.5);
#10074=VECTOR('',#34763,2.5);
#10075=VECTOR('',#34766,2.5);
#10076=VECTOR('',#34769,2.5);
#10077=VECTOR('',#34772,2.5);
#10078=VECTOR('',#34775,2.5);
#10079=VECTOR('',#34778,2.5);
#10080=VECTOR('',#34781,2.5);
#10081=VECTOR('',#34784,2.5);
#10082=VECTOR('',#34787,2.5);
#10083=VECTOR('',#34790,2.5);
#10084=VECTOR('',#34793,2.5);
#10085=VECTOR('',#34796,2.5);
#10086=VECTOR('',#34799,2.5);
#10087=VECTOR('',#34802,2.5);
#10088=VECTOR('',#34805,2.5);
#10089=VECTOR('',#34808,2.5);
#10090=VECTOR('',#34811,2.5);
#10091=VECTOR('',#34814,2.5);
#10092=VECTOR('',#34817,2.5);
#10093=VECTOR('',#34820,2.5);
#10094=VECTOR('',#34823,2.5);
#10095=VECTOR('',#34826,2.5);
#10096=VECTOR('',#34829,2.5);
#10097=VECTOR('',#34832,2.5);
#10098=VECTOR('',#34835,2.5);
#10099=VECTOR('',#34838,2.5);
#10100=VECTOR('',#34841,2.5);
#10101=VECTOR('',#34844,2.5);
#10102=VECTOR('',#34847,2.5);
#10103=VECTOR('',#34850,2.5);
#10104=VECTOR('',#34853,2.5);
#10105=VECTOR('',#34856,2.5);
#10106=VECTOR('',#34859,2.5);
#10107=VECTOR('',#34862,2.5);
#10108=VECTOR('',#34867,2.5);
#10109=VECTOR('',#34868,2.5);
#10110=VECTOR('',#34869,10.);
#10111=VECTOR('',#34876,10.);
#10112=VECTOR('',#34881,10.);
#10113=VECTOR('',#34884,10.);
#10114=VECTOR('',#34885,10.);
#10115=VECTOR('',#34888,10.);
#10116=VECTOR('',#34889,10.);
#10117=VECTOR('',#34890,10.);
#10118=VECTOR('',#34891,10.);
#10119=VECTOR('',#34892,10.);
#10120=VECTOR('',#34893,10.);
#10121=VECTOR('',#34904,1.85);
#10122=VECTOR('',#34909,2.);
#10123=VECTOR('',#34914,2.35);
#10124=VECTOR('',#34925,2.);
#10125=VECTOR('',#34928,1.85);
#10126=VECTOR('',#34961,1.55);
#10127=VECTOR('',#34964,10.);
#10128=VECTOR('',#34965,10.);
#10129=VECTOR('',#34966,10.);
#10130=VECTOR('',#34969,10.);
#10131=VECTOR('',#34970,10.);
#10132=VECTOR('',#34973,10.);
#10133=VECTOR('',#34974,10.);
#10134=VECTOR('',#34975,10.);
#10135=VECTOR('',#34978,10.);
#10136=VECTOR('',#34979,10.);
#10137=VECTOR('',#34980,10.);
#10138=VECTOR('',#34983,10.);
#10139=VECTOR('',#34984,10.);
#10140=VECTOR('',#34987,10.);
#10141=VECTOR('',#34988,10.);
#10142=VECTOR('',#34991,10.);
#10143=VECTOR('',#34992,10.);
#10144=VECTOR('',#34993,10.);
#10145=VECTOR('',#34996,10.);
#10146=VECTOR('',#34997,10.);
#10147=VECTOR('',#34998,10.);
#10148=VECTOR('',#35001,10.);
#10149=VECTOR('',#35002,10.);
#10150=VECTOR('',#35005,10.);
#10151=VECTOR('',#35006,10.);
#10152=VECTOR('',#35017,10.);
#10153=VECTOR('',#35018,10.);
#10154=VECTOR('',#35019,10.);
#10155=VECTOR('',#35020,10.);
#10156=VECTOR('',#35025,10.);
#10157=VECTOR('',#35028,10.);
#10158=VECTOR('',#35029,10.);
#10159=VECTOR('',#35036,10.);
#10160=VECTOR('',#35037,10.);
#10161=VECTOR('',#35038,10.);
#10162=VECTOR('',#35039,10.);
#10163=VECTOR('',#35044,10.);
#10164=VECTOR('',#35047,10.);
#10165=VECTOR('',#35048,10.);
#10166=VECTOR('',#35055,10.);
#10167=VECTOR('',#35056,10.);
#10168=VECTOR('',#35057,10.);
#10169=VECTOR('',#35058,10.);
#10170=VECTOR('',#35063,10.);
#10171=VECTOR('',#35066,10.);
#10172=VECTOR('',#35067,10.);
#10173=VECTOR('',#35074,10.);
#10174=VECTOR('',#35075,10.);
#10175=VECTOR('',#35076,10.);
#10176=VECTOR('',#35077,10.);
#10177=VECTOR('',#35082,10.);
#10178=VECTOR('',#35085,10.);
#10179=VECTOR('',#35086,10.);
#10180=VECTOR('',#35093,10.);
#10181=VECTOR('',#35094,10.);
#10182=VECTOR('',#35095,10.);
#10183=VECTOR('',#35096,10.);
#10184=VECTOR('',#35101,10.);
#10185=VECTOR('',#35104,10.);
#10186=VECTOR('',#35105,10.);
#10187=VECTOR('',#35112,10.);
#10188=VECTOR('',#35113,10.);
#10189=VECTOR('',#35114,10.);
#10190=VECTOR('',#35115,10.);
#10191=VECTOR('',#35120,10.);
#10192=VECTOR('',#35123,10.);
#10193=VECTOR('',#35124,10.);
#10194=VECTOR('',#35131,10.);
#10195=VECTOR('',#35132,10.);
#10196=VECTOR('',#35133,10.);
#10197=VECTOR('',#35134,10.);
#10198=VECTOR('',#35139,10.);
#10199=VECTOR('',#35142,10.);
#10200=VECTOR('',#35143,10.);
#10201=VECTOR('',#35150,10.);
#10202=VECTOR('',#35151,10.);
#10203=VECTOR('',#35152,10.);
#10204=VECTOR('',#35153,10.);
#10205=VECTOR('',#35158,10.);
#10206=VECTOR('',#35161,10.);
#10207=VECTOR('',#35162,10.);
#10208=VECTOR('',#35169,10.);
#10209=VECTOR('',#35170,10.);
#10210=VECTOR('',#35171,10.);
#10211=VECTOR('',#35172,10.);
#10212=VECTOR('',#35177,10.);
#10213=VECTOR('',#35180,10.);
#10214=VECTOR('',#35181,10.);
#10215=VECTOR('',#35188,10.);
#10216=VECTOR('',#35189,10.);
#10217=VECTOR('',#35190,10.);
#10218=VECTOR('',#35191,10.);
#10219=VECTOR('',#35196,10.);
#10220=VECTOR('',#35199,10.);
#10221=VECTOR('',#35200,10.);
#10222=VECTOR('',#35207,10.);
#10223=VECTOR('',#35208,10.);
#10224=VECTOR('',#35209,10.);
#10225=VECTOR('',#35210,10.);
#10226=VECTOR('',#35215,10.);
#10227=VECTOR('',#35218,10.);
#10228=VECTOR('',#35219,10.);
#10229=VECTOR('',#35226,10.);
#10230=VECTOR('',#35227,10.);
#10231=VECTOR('',#35228,10.);
#10232=VECTOR('',#35229,10.);
#10233=VECTOR('',#35234,10.);
#10234=VECTOR('',#35237,10.);
#10235=VECTOR('',#35238,10.);
#10236=VECTOR('',#35245,10.);
#10237=VECTOR('',#35246,10.);
#10238=VECTOR('',#35247,10.);
#10239=VECTOR('',#35248,10.);
#10240=VECTOR('',#35253,10.);
#10241=VECTOR('',#35256,10.);
#10242=VECTOR('',#35257,10.);
#10243=VECTOR('',#35264,10.);
#10244=VECTOR('',#35265,10.);
#10245=VECTOR('',#35266,10.);
#10246=VECTOR('',#35267,10.);
#10247=VECTOR('',#35272,10.);
#10248=VECTOR('',#35275,10.);
#10249=VECTOR('',#35276,10.);
#10250=VECTOR('',#35283,10.);
#10251=VECTOR('',#35284,10.);
#10252=VECTOR('',#35285,10.);
#10253=VECTOR('',#35286,10.);
#10254=VECTOR('',#35291,10.);
#10255=VECTOR('',#35294,10.);
#10256=VECTOR('',#35295,10.);
#10257=VECTOR('',#35302,10.);
#10258=VECTOR('',#35303,10.);
#10259=VECTOR('',#35304,10.);
#10260=VECTOR('',#35305,10.);
#10261=VECTOR('',#35310,10.);
#10262=VECTOR('',#35313,10.);
#10263=VECTOR('',#35314,10.);
#10264=VECTOR('',#35321,10.);
#10265=VECTOR('',#35322,10.);
#10266=VECTOR('',#35323,10.);
#10267=VECTOR('',#35324,10.);
#10268=VECTOR('',#35329,10.);
#10269=VECTOR('',#35332,10.);
#10270=VECTOR('',#35333,10.);
#10271=VECTOR('',#35340,10.);
#10272=VECTOR('',#35341,10.);
#10273=VECTOR('',#35342,10.);
#10274=VECTOR('',#35343,10.);
#10275=VECTOR('',#35348,10.);
#10276=VECTOR('',#35351,10.);
#10277=VECTOR('',#35352,10.);
#10278=VECTOR('',#35359,10.);
#10279=VECTOR('',#35360,10.);
#10280=VECTOR('',#35361,10.);
#10281=VECTOR('',#35362,10.);
#10282=VECTOR('',#35367,10.);
#10283=VECTOR('',#35372,10.);
#10284=VECTOR('',#35373,10.);
#10285=VECTOR('',#35382,10.);
#10286=VECTOR('',#35383,10.);
#10287=VECTOR('',#35384,10.);
#10288=VECTOR('',#35385,10.);
#10289=VECTOR('',#35390,10.);
#10290=VECTOR('',#35393,10.);
#10291=VECTOR('',#35394,10.);
#10292=VECTOR('',#35401,10.);
#10293=VECTOR('',#35402,10.);
#10294=VECTOR('',#35403,10.);
#10295=VECTOR('',#35404,10.);
#10296=VECTOR('',#35409,10.);
#10297=VECTOR('',#35412,10.);
#10298=VECTOR('',#35413,10.);
#10299=VECTOR('',#35420,10.);
#10300=VECTOR('',#35421,10.);
#10301=VECTOR('',#35422,10.);
#10302=VECTOR('',#35423,10.);
#10303=VECTOR('',#35428,10.);
#10304=VECTOR('',#35431,10.);
#10305=VECTOR('',#35432,10.);
#10306=VECTOR('',#35439,10.);
#10307=VECTOR('',#35440,10.);
#10308=VECTOR('',#35441,10.);
#10309=VECTOR('',#35442,10.);
#10310=VECTOR('',#35447,10.);
#10311=VECTOR('',#35450,10.);
#10312=VECTOR('',#35451,10.);
#10313=VECTOR('',#35458,10.);
#10314=VECTOR('',#35459,10.);
#10315=VECTOR('',#35460,10.);
#10316=VECTOR('',#35461,10.);
#10317=VECTOR('',#35466,10.);
#10318=VECTOR('',#35469,10.);
#10319=VECTOR('',#35470,10.);
#10320=VECTOR('',#35477,10.);
#10321=VECTOR('',#35478,10.);
#10322=VECTOR('',#35479,10.);
#10323=VECTOR('',#35480,10.);
#10324=VECTOR('',#35485,10.);
#10325=VECTOR('',#35488,10.);
#10326=VECTOR('',#35489,10.);
#10327=VECTOR('',#35496,10.);
#10328=VECTOR('',#35497,10.);
#10329=VECTOR('',#35498,10.);
#10330=VECTOR('',#35499,10.);
#10331=VECTOR('',#35504,10.);
#10332=VECTOR('',#35507,10.);
#10333=VECTOR('',#35508,10.);
#10334=VECTOR('',#35515,10.);
#10335=VECTOR('',#35516,10.);
#10336=VECTOR('',#35517,10.);
#10337=VECTOR('',#35518,10.);
#10338=VECTOR('',#35523,10.);
#10339=VECTOR('',#35526,10.);
#10340=VECTOR('',#35527,10.);
#10341=VECTOR('',#35534,10.);
#10342=VECTOR('',#35535,10.);
#10343=VECTOR('',#35536,10.);
#10344=VECTOR('',#35537,10.);
#10345=VECTOR('',#35542,10.);
#10346=VECTOR('',#35545,10.);
#10347=VECTOR('',#35546,10.);
#10348=VECTOR('',#35553,10.);
#10349=VECTOR('',#35554,10.);
#10350=VECTOR('',#35555,10.);
#10351=VECTOR('',#35556,10.);
#10352=VECTOR('',#35561,10.);
#10353=VECTOR('',#35564,10.);
#10354=VECTOR('',#35565,10.);
#10355=VECTOR('',#35572,10.);
#10356=VECTOR('',#35573,10.);
#10357=VECTOR('',#35574,10.);
#10358=VECTOR('',#35575,10.);
#10359=VECTOR('',#35580,10.);
#10360=VECTOR('',#35583,10.);
#10361=VECTOR('',#35584,10.);
#10362=VECTOR('',#35591,10.);
#10363=VECTOR('',#35592,10.);
#10364=VECTOR('',#35593,10.);
#10365=VECTOR('',#35594,10.);
#10366=VECTOR('',#35599,10.);
#10367=VECTOR('',#35602,10.);
#10368=VECTOR('',#35603,10.);
#10369=VECTOR('',#35610,10.);
#10370=VECTOR('',#35611,10.);
#10371=VECTOR('',#35612,10.);
#10372=VECTOR('',#35613,10.);
#10373=VECTOR('',#35618,10.);
#10374=VECTOR('',#35621,10.);
#10375=VECTOR('',#35622,10.);
#10376=VECTOR('',#35629,10.);
#10377=VECTOR('',#35630,10.);
#10378=VECTOR('',#35631,10.);
#10379=VECTOR('',#35632,10.);
#10380=VECTOR('',#35637,10.);
#10381=VECTOR('',#35640,10.);
#10382=VECTOR('',#35641,10.);
#10383=VECTOR('',#35648,10.);
#10384=VECTOR('',#35649,10.);
#10385=VECTOR('',#35650,10.);
#10386=VECTOR('',#35651,10.);
#10387=VECTOR('',#35656,10.);
#10388=VECTOR('',#35659,10.);
#10389=VECTOR('',#35660,10.);
#10390=VECTOR('',#35667,10.);
#10391=VECTOR('',#35668,10.);
#10392=VECTOR('',#35669,10.);
#10393=VECTOR('',#35670,10.);
#10394=VECTOR('',#35675,10.);
#10395=VECTOR('',#35678,10.);
#10396=VECTOR('',#35679,10.);
#10397=VECTOR('',#35686,10.);
#10398=VECTOR('',#35687,10.);
#10399=VECTOR('',#35688,10.);
#10400=VECTOR('',#35689,10.);
#10401=VECTOR('',#35694,10.);
#10402=VECTOR('',#35697,10.);
#10403=VECTOR('',#35698,10.);
#10404=VECTOR('',#35705,10.);
#10405=VECTOR('',#35706,10.);
#10406=VECTOR('',#35707,10.);
#10407=VECTOR('',#35708,10.);
#10408=VECTOR('',#35713,10.);
#10409=VECTOR('',#35716,10.);
#10410=VECTOR('',#35717,10.);
#10411=VECTOR('',#35724,10.);
#10412=VECTOR('',#35725,10.);
#10413=VECTOR('',#35726,10.);
#10414=VECTOR('',#35733,10.);
#10415=VECTOR('',#35734,10.);
#10416=VECTOR('',#35751,3.905);
#10417=VECTOR('',#35762,7.2);
#10418=VECTOR('',#35767,7.5);
#10419=VECTOR('',#35768,7.5);
#10420=VECTOR('',#35771,7.3);
#10421=VECTOR('',#35782,2.8);
#10422=VECTOR('',#35789,2.01);
#10423=VECTOR('',#35792,10.);
#10424=VECTOR('',#35793,10.);
#10425=VECTOR('',#35794,10.);
#10426=VECTOR('',#35795,10.);
#10427=VECTOR('',#35796,10.);
#10428=VECTOR('',#35797,10.);
#10429=VECTOR('',#35798,10.);
#10430=VECTOR('',#35799,10.);
#10431=VECTOR('',#35800,10.);
#10432=VECTOR('',#35801,10.);
#10433=VECTOR('',#35802,10.);
#10434=VECTOR('',#35803,10.);
#10435=VECTOR('',#35804,10.);
#10436=VECTOR('',#35805,10.);
#10437=VECTOR('',#35806,10.);
#10438=VECTOR('',#35807,10.);
#10439=VECTOR('',#35808,10.);
#10440=VECTOR('',#35809,10.);
#10441=VECTOR('',#35810,10.);
#10442=VECTOR('',#35811,10.);
#10443=VECTOR('',#35816,10.);
#10444=VECTOR('',#35817,10.);
#10445=VECTOR('',#35818,10.);
#10446=VECTOR('',#35819,10.);
#10447=VECTOR('',#35822,10.);
#10448=VECTOR('',#35823,10.);
#10449=VECTOR('',#35824,10.);
#10450=VECTOR('',#35827,10.);
#10451=VECTOR('',#35828,10.);
#10452=VECTOR('',#35831,10.);
#10453=VECTOR('',#35832,10.);
#10454=VECTOR('',#35833,10.);
#10455=VECTOR('',#35834,10.);
#10456=VECTOR('',#35837,10.);
#10457=VECTOR('',#35838,10.);
#10458=VECTOR('',#35839,10.);
#10459=VECTOR('',#35842,10.);
#10460=VECTOR('',#35843,10.);
#10461=VECTOR('',#35844,10.);
#10462=VECTOR('',#35847,10.);
#10463=VECTOR('',#35848,10.);
#10464=VECTOR('',#35849,10.);
#10465=VECTOR('',#35852,10.);
#10466=VECTOR('',#35853,10.);
#10467=VECTOR('',#35854,10.);
#10468=VECTOR('',#35857,10.);
#10469=VECTOR('',#35858,10.);
#10470=VECTOR('',#35859,10.);
#10471=VECTOR('',#35862,9.99999999999999);
#10472=VECTOR('',#35863,10.);
#10473=VECTOR('',#35864,9.99999999999999);
#10474=VECTOR('',#35867,10.);
#10475=VECTOR('',#35868,10.);
#10476=VECTOR('',#35869,10.);
#10477=VECTOR('',#35872,10.);
#10478=VECTOR('',#35873,10.);
#10479=VECTOR('',#35874,10.);
#10480=VECTOR('',#35877,10.);
#10481=VECTOR('',#35878,10.);
#10482=VECTOR('',#35879,10.);
#10483=VECTOR('',#35882,10.);
#10484=VECTOR('',#35883,10.);
#10485=VECTOR('',#35890,10.);
#10486=VECTOR('',#35891,10.);
#10487=VECTOR('',#35892,10.);
#10488=VECTOR('',#35893,10.);
#10489=VECTOR('',#35894,10.);
#10490=VECTOR('',#35895,10.);
#10491=VECTOR('',#35896,10.);
#10492=VECTOR('',#35897,10.);
#10493=VECTOR('',#35898,10.);
#10494=VECTOR('',#35899,10.);
#10495=VECTOR('',#35900,10.);
#10496=VECTOR('',#35901,10.);
#10497=VECTOR('',#35902,10.);
#10498=VECTOR('',#35903,10.);
#10499=VECTOR('',#35904,10.);
#10500=VECTOR('',#35905,10.);
#10501=VECTOR('',#35906,10.);
#10502=VECTOR('',#35907,10.);
#10503=VECTOR('',#35908,10.);
#10504=VECTOR('',#35909,10.);
#10505=VECTOR('',#35912,10.);
#10506=VECTOR('',#35913,10.);
#10507=VECTOR('',#35914,10.);
#10508=VECTOR('',#35915,10.);
#10509=VECTOR('',#35916,10.);
#10510=VECTOR('',#35917,10.);
#10511=VECTOR('',#35918,10.);
#10512=VECTOR('',#35919,10.);
#10513=VECTOR('',#35920,10.);
#10514=VECTOR('',#35921,10.);
#10515=VECTOR('',#35922,10.);
#10516=VECTOR('',#35923,10.);
#10517=VECTOR('',#35924,10.);
#10518=VECTOR('',#35927,10.);
#10519=VECTOR('',#35928,10.);
#10520=VECTOR('',#35929,10.);
#10521=VECTOR('',#35930,10.);
#10522=VECTOR('',#35931,10.);
#10523=VECTOR('',#35932,10.);
#10524=VECTOR('',#35933,10.);
#10525=VECTOR('',#35934,10.);
#10526=VECTOR('',#35935,10.);
#10527=VECTOR('',#35936,10.);
#10528=VECTOR('',#35939,10.);
#10529=VECTOR('',#35940,10.);
#10530=VECTOR('',#35941,10.);
#10531=VECTOR('',#35942,10.);
#10532=VECTOR('',#35943,10.);
#10533=VECTOR('',#35944,10.);
#10534=VECTOR('',#35945,10.);
#10535=VECTOR('',#35946,10.);
#10536=VECTOR('',#35947,10.);
#10537=VECTOR('',#35948,10.);
#10538=VECTOR('',#35951,10.);
#10539=VECTOR('',#35952,10.);
#10540=VECTOR('',#35953,10.);
#10541=VECTOR('',#35958,10.);
#10542=VECTOR('',#35959,10.);
#10543=VECTOR('',#35960,10.);
#10544=VECTOR('',#35961,10.);
#10545=VECTOR('',#35962,10.);
#10546=VECTOR('',#35963,10.);
#10547=VECTOR('',#35964,10.);
#10548=VECTOR('',#35965,10.);
#10549=VECTOR('',#35966,10.);
#10550=VECTOR('',#35967,10.);
#10551=VECTOR('',#35968,10.);
#10552=VECTOR('',#35969,10.);
#10553=VECTOR('',#35970,10.);
#10554=VECTOR('',#35971,10.);
#10555=VECTOR('',#35972,10.);
#10556=VECTOR('',#35973,10.);
#10557=VECTOR('',#35974,10.);
#10558=VECTOR('',#35975,10.);
#10559=VECTOR('',#35976,10.);
#10560=VECTOR('',#35977,10.);
#10561=VECTOR('',#35980,10.);
#10562=VECTOR('',#35981,10.);
#10563=VECTOR('',#35982,10.);
#10564=VECTOR('',#35983,10.);
#10565=VECTOR('',#35984,10.);
#10566=VECTOR('',#35985,10.);
#10567=VECTOR('',#35986,10.);
#10568=VECTOR('',#35987,10.);
#10569=VECTOR('',#35988,10.);
#10570=VECTOR('',#35989,10.);
#10571=VECTOR('',#35992,10.);
#10572=VECTOR('',#35993,10.);
#10573=VECTOR('',#35994,10.);
#10574=VECTOR('',#35995,10.);
#10575=VECTOR('',#35996,10.);
#10576=VECTOR('',#35997,10.);
#10577=VECTOR('',#35998,10.);
#10578=VECTOR('',#35999,10.);
#10579=VECTOR('',#36000,10.);
#10580=VECTOR('',#36001,10.);
#10581=VECTOR('',#36002,10.);
#10582=VECTOR('',#36003,10.);
#10583=VECTOR('',#36006,10.);
#10584=VECTOR('',#36007,10.);
#10585=VECTOR('',#36008,10.);
#10586=VECTOR('',#36011,10.);
#10587=VECTOR('',#36012,10.);
#10588=VECTOR('',#36013,10.);
#10589=VECTOR('',#36016,10.);
#10590=VECTOR('',#36017,10.);
#10591=VECTOR('',#36022,10.);
#10592=VECTOR('',#36023,10.);
#10593=VECTOR('',#36024,10.);
#10594=VECTOR('',#36025,10.);
#10595=VECTOR('',#36026,10.);
#10596=VECTOR('',#36027,10.);
#10597=VECTOR('',#36028,10.);
#10598=VECTOR('',#36029,10.);
#10599=VECTOR('',#36030,10.);
#10600=VECTOR('',#36031,10.);
#10601=VECTOR('',#36032,10.);
#10602=VECTOR('',#36033,10.);
#10603=VECTOR('',#36034,10.);
#10604=VECTOR('',#36035,10.);
#10605=VECTOR('',#36036,10.);
#10606=VECTOR('',#36037,10.);
#10607=VECTOR('',#36038,10.);
#10608=VECTOR('',#36039,10.);
#10609=VECTOR('',#36040,10.);
#10610=VECTOR('',#36041,10.);
#10611=VECTOR('',#36046,10.);
#10612=VECTOR('',#36047,10.);
#10613=VECTOR('',#36048,10.);
#10614=VECTOR('',#36049,10.);
#10615=VECTOR('',#36050,10.);
#10616=VECTOR('',#36051,10.);
#10617=VECTOR('',#36054,10.);
#10618=VECTOR('',#36055,10.);
#10619=VECTOR('',#36056,10.);
#10620=VECTOR('',#36057,10.);
#10621=VECTOR('',#36058,10.);
#10622=VECTOR('',#36061,10.);
#10623=VECTOR('',#36062,10.);
#10624=VECTOR('',#36063,10.);
#10625=VECTOR('',#36066,10.);
#10626=VECTOR('',#36067,10.);
#10627=VECTOR('',#36068,10.);
#10628=VECTOR('',#36071,10.);
#10629=VECTOR('',#36072,10.);
#10630=VECTOR('',#36077,10.);
#10631=VECTOR('',#36078,10.);
#10632=VECTOR('',#36079,10.);
#10633=VECTOR('',#36080,10.);
#10634=VECTOR('',#36081,10.);
#10635=VECTOR('',#36082,10.);
#10636=VECTOR('',#36083,10.);
#10637=VECTOR('',#36084,10.);
#10638=VECTOR('',#36085,10.);
#10639=VECTOR('',#36086,10.);
#10640=VECTOR('',#36087,10.);
#10641=VECTOR('',#36088,10.);
#10642=VECTOR('',#36089,10.);
#10643=VECTOR('',#36090,10.);
#10644=VECTOR('',#36091,10.);
#10645=VECTOR('',#36092,10.);
#10646=VECTOR('',#36093,10.);
#10647=VECTOR('',#36094,10.);
#10648=VECTOR('',#36095,10.);
#10649=VECTOR('',#36096,10.);
#10650=VECTOR('',#36101,10.);
#10651=VECTOR('',#36102,10.);
#10652=VECTOR('',#36103,10.);
#10653=VECTOR('',#36104,10.);
#10654=VECTOR('',#36105,10.);
#10655=VECTOR('',#36106,10.);
#10656=VECTOR('',#36107,10.);
#10657=VECTOR('',#36108,10.);
#10658=VECTOR('',#36109,10.);
#10659=VECTOR('',#36110,10.);
#10660=VECTOR('',#36111,10.);
#10661=VECTOR('',#36112,10.);
#10662=VECTOR('',#36113,10.);
#10663=VECTOR('',#36114,10.);
#10664=VECTOR('',#36115,10.);
#10665=VECTOR('',#36116,10.);
#10666=VECTOR('',#36117,10.);
#10667=VECTOR('',#36118,10.);
#10668=VECTOR('',#36119,10.);
#10669=VECTOR('',#36120,10.);
#10670=VECTOR('',#36125,10.);
#10671=VECTOR('',#36126,10.);
#10672=VECTOR('',#36127,10.);
#10673=VECTOR('',#36128,10.);
#10674=VECTOR('',#36129,10.);
#10675=VECTOR('',#36130,10.);
#10676=VECTOR('',#36133,10.);
#10677=VECTOR('',#36134,10.);
#10678=VECTOR('',#36135,10.);
#10679=VECTOR('',#36136,10.);
#10680=VECTOR('',#36137,10.);
#10681=VECTOR('',#36140,10.);
#10682=VECTOR('',#36141,10.);
#10683=VECTOR('',#36142,10.);
#10684=VECTOR('',#36145,10.);
#10685=VECTOR('',#36146,10.);
#10686=VECTOR('',#36147,10.);
#10687=VECTOR('',#36150,10.);
#10688=VECTOR('',#36151,10.);
#10689=VECTOR('',#36156,10.);
#10690=VECTOR('',#36157,10.);
#10691=VECTOR('',#36158,10.);
#10692=VECTOR('',#36159,10.);
#10693=VECTOR('',#36160,10.);
#10694=VECTOR('',#36161,10.);
#10695=VECTOR('',#36162,10.);
#10696=VECTOR('',#36163,10.);
#10697=VECTOR('',#36164,10.);
#10698=VECTOR('',#36165,10.);
#10699=VECTOR('',#36166,10.);
#10700=VECTOR('',#36167,10.);
#10701=VECTOR('',#36168,10.);
#10702=VECTOR('',#36169,10.);
#10703=VECTOR('',#36170,10.);
#10704=VECTOR('',#36171,10.);
#10705=VECTOR('',#36172,10.);
#10706=VECTOR('',#36173,10.);
#10707=VECTOR('',#36174,10.);
#10708=VECTOR('',#36175,10.);
#10709=VECTOR('',#36178,10.);
#10710=VECTOR('',#36179,10.);
#10711=VECTOR('',#36180,10.);
#10712=VECTOR('',#36181,10.);
#10713=VECTOR('',#36182,10.);
#10714=VECTOR('',#36183,10.);
#10715=VECTOR('',#36184,10.);
#10716=VECTOR('',#36185,10.);
#10717=VECTOR('',#36186,10.);
#10718=VECTOR('',#36187,10.);
#10719=VECTOR('',#36190,10.);
#10720=VECTOR('',#36191,10.);
#10721=VECTOR('',#36192,10.);
#10722=VECTOR('',#36193,10.);
#10723=VECTOR('',#36194,10.);
#10724=VECTOR('',#36195,10.);
#10725=VECTOR('',#36196,10.);
#10726=VECTOR('',#36197,10.);
#10727=VECTOR('',#36198,10.);
#10728=VECTOR('',#36199,10.);
#10729=VECTOR('',#36200,10.);
#10730=VECTOR('',#36201,10.);
#10731=VECTOR('',#36204,10.);
#10732=VECTOR('',#36205,10.);
#10733=VECTOR('',#36206,10.);
#10734=VECTOR('',#36209,10.);
#10735=VECTOR('',#36210,10.);
#10736=VECTOR('',#36211,10.);
#10737=VECTOR('',#36214,10.);
#10738=VECTOR('',#36215,10.);
#10739=VECTOR('',#36220,10.);
#10740=VECTOR('',#36221,10.);
#10741=VECTOR('',#36222,10.);
#10742=VECTOR('',#36223,10.);
#10743=VECTOR('',#36224,10.);
#10744=VECTOR('',#36225,10.);
#10745=VECTOR('',#36226,10.);
#10746=VECTOR('',#36227,10.);
#10747=VECTOR('',#36228,10.);
#10748=VECTOR('',#36229,10.);
#10749=VECTOR('',#36230,10.);
#10750=VECTOR('',#36231,10.);
#10751=VECTOR('',#36232,10.);
#10752=VECTOR('',#36233,10.);
#10753=VECTOR('',#36234,10.);
#10754=VECTOR('',#36235,10.);
#10755=VECTOR('',#36236,10.);
#10756=VECTOR('',#36237,10.);
#10757=VECTOR('',#36238,10.);
#10758=VECTOR('',#36239,10.);
#10759=VECTOR('',#36242,10.);
#10760=VECTOR('',#36243,10.);
#10761=VECTOR('',#36244,10.);
#10762=VECTOR('',#36245,10.);
#10763=VECTOR('',#36246,10.);
#10764=VECTOR('',#36247,10.);
#10765=VECTOR('',#36248,10.);
#10766=VECTOR('',#36249,10.);
#10767=VECTOR('',#36250,10.);
#10768=VECTOR('',#36251,10.);
#10769=VECTOR('',#36252,10.);
#10770=VECTOR('',#36253,10.);
#10771=VECTOR('',#36254,10.);
#10772=VECTOR('',#36257,10.);
#10773=VECTOR('',#36258,10.);
#10774=VECTOR('',#36259,10.);
#10775=VECTOR('',#36260,10.);
#10776=VECTOR('',#36261,10.);
#10777=VECTOR('',#36262,10.);
#10778=VECTOR('',#36263,10.);
#10779=VECTOR('',#36264,10.);
#10780=VECTOR('',#36265,10.);
#10781=VECTOR('',#36266,10.);
#10782=VECTOR('',#36269,10.);
#10783=VECTOR('',#36270,10.);
#10784=VECTOR('',#36271,10.);
#10785=VECTOR('',#36272,10.);
#10786=VECTOR('',#36273,10.);
#10787=VECTOR('',#36274,10.);
#10788=VECTOR('',#36275,10.);
#10789=VECTOR('',#36276,10.);
#10790=VECTOR('',#36277,10.);
#10791=VECTOR('',#36278,10.);
#10792=VECTOR('',#36281,10.);
#10793=VECTOR('',#36282,10.);
#10794=VECTOR('',#36283,10.);
#10795=VECTOR('',#36288,10.);
#10796=VECTOR('',#36289,10.);
#10797=VECTOR('',#36290,10.);
#10798=VECTOR('',#36291,10.);
#10799=VECTOR('',#36292,10.);
#10800=VECTOR('',#36293,10.);
#10801=VECTOR('',#36294,10.);
#10802=VECTOR('',#36295,10.);
#10803=VECTOR('',#36296,10.);
#10804=VECTOR('',#36297,10.);
#10805=VECTOR('',#36298,10.);
#10806=VECTOR('',#36299,10.);
#10807=VECTOR('',#36300,10.);
#10808=VECTOR('',#36301,10.);
#10809=VECTOR('',#36302,10.);
#10810=VECTOR('',#36303,10.);
#10811=VECTOR('',#36304,10.);
#10812=VECTOR('',#36305,10.);
#10813=VECTOR('',#36306,10.);
#10814=VECTOR('',#36307,10.);
#10815=VECTOR('',#36312,10.);
#10816=VECTOR('',#36313,10.);
#10817=VECTOR('',#36314,10.);
#10818=VECTOR('',#36315,10.);
#10819=VECTOR('',#36318,10.);
#10820=VECTOR('',#36319,10.);
#10821=VECTOR('',#36320,10.);
#10822=VECTOR('',#36323,10.);
#10823=VECTOR('',#36324,10.);
#10824=VECTOR('',#36327,10.);
#10825=VECTOR('',#36328,10.);
#10826=VECTOR('',#36329,10.);
#10827=VECTOR('',#36330,10.);
#10828=VECTOR('',#36333,10.);
#10829=VECTOR('',#36334,10.);
#10830=VECTOR('',#36335,10.);
#10831=VECTOR('',#36338,10.);
#10832=VECTOR('',#36339,10.);
#10833=VECTOR('',#36340,10.);
#10834=VECTOR('',#36343,10.);
#10835=VECTOR('',#36344,10.);
#10836=VECTOR('',#36345,10.);
#10837=VECTOR('',#36348,10.);
#10838=VECTOR('',#36349,10.);
#10839=VECTOR('',#36350,10.);
#10840=VECTOR('',#36353,10.);
#10841=VECTOR('',#36354,10.);
#10842=VECTOR('',#36355,10.);
#10843=VECTOR('',#36358,9.99999999999999);
#10844=VECTOR('',#36359,10.);
#10845=VECTOR('',#36360,9.99999999999999);
#10846=VECTOR('',#36363,10.);
#10847=VECTOR('',#36364,10.);
#10848=VECTOR('',#36365,10.);
#10849=VECTOR('',#36368,10.);
#10850=VECTOR('',#36369,10.);
#10851=VECTOR('',#36370,10.);
#10852=VECTOR('',#36373,10.);
#10853=VECTOR('',#36374,10.);
#10854=VECTOR('',#36375,10.);
#10855=VECTOR('',#36378,10.);
#10856=VECTOR('',#36379,10.);
#10857=VECTOR('',#36388,10.);
#10858=VECTOR('',#36389,10.);
#10859=VECTOR('',#36390,10.);
#10860=VECTOR('',#36391,10.);
#10861=VECTOR('',#36394,10.);
#10862=VECTOR('',#36395,10.);
#10863=VECTOR('',#36396,10.);
#10864=VECTOR('',#36399,10.);
#10865=VECTOR('',#36400,10.);
#10866=VECTOR('',#36401,10.);
#10867=VECTOR('',#36404,10.);
#10868=VECTOR('',#36405,10.);
#10869=VECTOR('',#36410,10.);
#10870=VECTOR('',#36411,10.);
#10871=VECTOR('',#36412,10.);
#10872=VECTOR('',#36413,10.);
#10873=VECTOR('',#36416,10.);
#10874=VECTOR('',#36417,10.);
#10875=VECTOR('',#36418,10.);
#10876=VECTOR('',#36421,10.);
#10877=VECTOR('',#36422,10.);
#10878=VECTOR('',#36423,10.);
#10879=VECTOR('',#36426,10.);
#10880=VECTOR('',#36427,10.);
#10881=VECTOR('',#36432,10.);
#10882=VECTOR('',#36433,10.);
#10883=VECTOR('',#36434,10.);
#10884=VECTOR('',#36435,10.);
#10885=VECTOR('',#36438,10.);
#10886=VECTOR('',#36439,10.);
#10887=VECTOR('',#36440,10.);
#10888=VECTOR('',#36443,10.);
#10889=VECTOR('',#36444,10.);
#10890=VECTOR('',#36445,10.);
#10891=VECTOR('',#36448,10.);
#10892=VECTOR('',#36449,10.);
#10893=VECTOR('',#36454,10.);
#10894=VECTOR('',#36455,10.);
#10895=VECTOR('',#36456,10.);
#10896=VECTOR('',#36457,10.);
#10897=VECTOR('',#36460,10.);
#10898=VECTOR('',#36461,10.);
#10899=VECTOR('',#36462,10.);
#10900=VECTOR('',#36465,10.);
#10901=VECTOR('',#36466,10.);
#10902=VECTOR('',#36467,10.);
#10903=VECTOR('',#36470,10.);
#10904=VECTOR('',#36471,10.);
#10905=VECTOR('',#36476,10.);
#10906=VECTOR('',#36477,10.);
#10907=VECTOR('',#36478,10.);
#10908=VECTOR('',#36479,10.);
#10909=VECTOR('',#36482,10.);
#10910=VECTOR('',#36483,10.);
#10911=VECTOR('',#36484,10.);
#10912=VECTOR('',#36487,10.);
#10913=VECTOR('',#36488,10.);
#10914=VECTOR('',#36489,10.);
#10915=VECTOR('',#36492,10.);
#10916=VECTOR('',#36493,10.);
#10917=VECTOR('',#36498,10.);
#10918=VECTOR('',#36499,10.);
#10919=VECTOR('',#36500,10.);
#10920=VECTOR('',#36501,10.);
#10921=VECTOR('',#36504,10.);
#10922=VECTOR('',#36505,10.);
#10923=VECTOR('',#36506,10.);
#10924=VECTOR('',#36509,10.);
#10925=VECTOR('',#36510,10.);
#10926=VECTOR('',#36511,10.);
#10927=VECTOR('',#36514,10.);
#10928=VECTOR('',#36515,10.);
#10929=VECTOR('',#36520,10.);
#10930=VECTOR('',#36521,10.);
#10931=VECTOR('',#36522,10.);
#10932=VECTOR('',#36523,10.);
#10933=VECTOR('',#36526,10.);
#10934=VECTOR('',#36527,10.);
#10935=VECTOR('',#36528,10.);
#10936=VECTOR('',#36531,10.);
#10937=VECTOR('',#36532,10.);
#10938=VECTOR('',#36533,10.);
#10939=VECTOR('',#36536,10.);
#10940=VECTOR('',#36537,10.);
#10941=VECTOR('',#36542,10.);
#10942=VECTOR('',#36543,10.);
#10943=VECTOR('',#36544,10.);
#10944=VECTOR('',#36545,10.);
#10945=VECTOR('',#36548,10.);
#10946=VECTOR('',#36549,10.);
#10947=VECTOR('',#36550,10.);
#10948=VECTOR('',#36553,10.);
#10949=VECTOR('',#36554,10.);
#10950=VECTOR('',#36555,10.);
#10951=VECTOR('',#36558,10.);
#10952=VECTOR('',#36559,10.);
#10953=VECTOR('',#36564,10.);
#10954=VECTOR('',#36565,10.);
#10955=VECTOR('',#36566,10.);
#10956=VECTOR('',#36567,10.);
#10957=VECTOR('',#36570,10.);
#10958=VECTOR('',#36571,10.);
#10959=VECTOR('',#36572,10.);
#10960=VECTOR('',#36575,10.);
#10961=VECTOR('',#36576,10.);
#10962=VECTOR('',#36577,10.);
#10963=VECTOR('',#36580,10.);
#10964=VECTOR('',#36581,10.);
#10965=VECTOR('',#36586,10.);
#10966=VECTOR('',#36587,10.);
#10967=VECTOR('',#36588,10.);
#10968=VECTOR('',#36589,10.);
#10969=VECTOR('',#36592,10.);
#10970=VECTOR('',#36593,10.);
#10971=VECTOR('',#36594,10.);
#10972=VECTOR('',#36597,10.);
#10973=VECTOR('',#36598,10.);
#10974=VECTOR('',#36599,10.);
#10975=VECTOR('',#36602,10.);
#10976=VECTOR('',#36603,10.);
#10977=VECTOR('',#36608,10.);
#10978=VECTOR('',#36609,10.);
#10979=VECTOR('',#36610,10.);
#10980=VECTOR('',#36611,10.);
#10981=VECTOR('',#36614,10.);
#10982=VECTOR('',#36615,10.);
#10983=VECTOR('',#36616,10.);
#10984=VECTOR('',#36619,10.);
#10985=VECTOR('',#36620,10.);
#10986=VECTOR('',#36621,10.);
#10987=VECTOR('',#36624,10.);
#10988=VECTOR('',#36625,10.);
#10989=VECTOR('',#36630,10.);
#10990=VECTOR('',#36631,10.);
#10991=VECTOR('',#36632,10.);
#10992=VECTOR('',#36633,10.);
#10993=VECTOR('',#36636,10.);
#10994=VECTOR('',#36637,10.);
#10995=VECTOR('',#36638,10.);
#10996=VECTOR('',#36641,10.);
#10997=VECTOR('',#36642,10.);
#10998=VECTOR('',#36643,10.);
#10999=VECTOR('',#36646,10.);
#11000=VECTOR('',#36647,10.);
#11001=VECTOR('',#36652,10.);
#11002=VECTOR('',#36653,10.);
#11003=VECTOR('',#36654,10.);
#11004=VECTOR('',#36655,10.);
#11005=VECTOR('',#36658,10.);
#11006=VECTOR('',#36659,10.);
#11007=VECTOR('',#36660,10.);
#11008=VECTOR('',#36663,10.);
#11009=VECTOR('',#36664,10.);
#11010=VECTOR('',#36665,10.);
#11011=VECTOR('',#36668,10.);
#11012=VECTOR('',#36669,10.);
#11013=VECTOR('',#36674,10.);
#11014=VECTOR('',#36675,10.);
#11015=VECTOR('',#36676,10.);
#11016=VECTOR('',#36677,10.);
#11017=VECTOR('',#36680,10.);
#11018=VECTOR('',#36681,10.);
#11019=VECTOR('',#36682,10.);
#11020=VECTOR('',#36685,10.);
#11021=VECTOR('',#36686,10.);
#11022=VECTOR('',#36687,10.);
#11023=VECTOR('',#36690,10.);
#11024=VECTOR('',#36691,10.);
#11025=VECTOR('',#36696,10.);
#11026=VECTOR('',#36697,10.);
#11027=VECTOR('',#36698,10.);
#11028=VECTOR('',#36699,10.);
#11029=VECTOR('',#36702,10.);
#11030=VECTOR('',#36703,10.);
#11031=VECTOR('',#36704,10.);
#11032=VECTOR('',#36707,10.);
#11033=VECTOR('',#36708,10.);
#11034=VECTOR('',#36709,10.);
#11035=VECTOR('',#36712,10.);
#11036=VECTOR('',#36713,10.);
#11037=VECTOR('',#36718,10.);
#11038=VECTOR('',#36719,10.);
#11039=VECTOR('',#36720,10.);
#11040=VECTOR('',#36721,10.);
#11041=VECTOR('',#36724,10.);
#11042=VECTOR('',#36725,10.);
#11043=VECTOR('',#36726,10.);
#11044=VECTOR('',#36729,10.);
#11045=VECTOR('',#36730,10.);
#11046=VECTOR('',#36731,10.);
#11047=VECTOR('',#36734,10.);
#11048=VECTOR('',#36735,10.);
#11049=VECTOR('',#36740,10.);
#11050=VECTOR('',#36741,10.);
#11051=VECTOR('',#36742,10.);
#11052=VECTOR('',#36743,10.);
#11053=VECTOR('',#36746,10.);
#11054=VECTOR('',#36747,10.);
#11055=VECTOR('',#36748,10.);
#11056=VECTOR('',#36751,10.);
#11057=VECTOR('',#36752,10.);
#11058=VECTOR('',#36753,10.);
#11059=VECTOR('',#36756,10.);
#11060=VECTOR('',#36757,10.);
#11061=VECTOR('',#36762,10.);
#11062=VECTOR('',#36763,10.);
#11063=VECTOR('',#36764,10.);
#11064=VECTOR('',#36765,10.);
#11065=VECTOR('',#36768,10.);
#11066=VECTOR('',#36769,10.);
#11067=VECTOR('',#36770,10.);
#11068=VECTOR('',#36773,10.);
#11069=VECTOR('',#36774,10.);
#11070=VECTOR('',#36775,10.);
#11071=VECTOR('',#36778,10.);
#11072=VECTOR('',#36779,10.);
#11073=VECTOR('',#36784,10.);
#11074=VECTOR('',#36785,10.);
#11075=VECTOR('',#36786,10.);
#11076=VECTOR('',#36787,10.);
#11077=VECTOR('',#36790,10.);
#11078=VECTOR('',#36791,10.);
#11079=VECTOR('',#36792,10.);
#11080=VECTOR('',#36795,10.);
#11081=VECTOR('',#36796,10.);
#11082=VECTOR('',#36797,10.);
#11083=VECTOR('',#36800,10.);
#11084=VECTOR('',#36801,10.);
#11085=VECTOR('',#36806,10.);
#11086=VECTOR('',#36807,10.);
#11087=VECTOR('',#36808,10.);
#11088=VECTOR('',#36809,10.);
#11089=VECTOR('',#36812,10.);
#11090=VECTOR('',#36813,10.);
#11091=VECTOR('',#36814,10.);
#11092=VECTOR('',#36817,10.);
#11093=VECTOR('',#36818,10.);
#11094=VECTOR('',#36819,10.);
#11095=VECTOR('',#36822,10.);
#11096=VECTOR('',#36823,10.);
#11097=VECTOR('',#36828,10.);
#11098=VECTOR('',#36829,10.);
#11099=VECTOR('',#36830,10.);
#11100=VECTOR('',#36831,10.);
#11101=VECTOR('',#36834,10.);
#11102=VECTOR('',#36835,10.);
#11103=VECTOR('',#36836,10.);
#11104=VECTOR('',#36839,10.);
#11105=VECTOR('',#36840,10.);
#11106=VECTOR('',#36841,10.);
#11107=VECTOR('',#36844,10.);
#11108=VECTOR('',#36845,10.);
#11109=VECTOR('',#36850,10.);
#11110=VECTOR('',#36851,10.);
#11111=VECTOR('',#36852,10.);
#11112=VECTOR('',#36853,10.);
#11113=VECTOR('',#36856,10.);
#11114=VECTOR('',#36857,10.);
#11115=VECTOR('',#36858,10.);
#11116=VECTOR('',#36861,10.);
#11117=VECTOR('',#36862,10.);
#11118=VECTOR('',#36863,10.);
#11119=VECTOR('',#36866,10.);
#11120=VECTOR('',#36867,10.);
#11121=VECTOR('',#36872,10.);
#11122=VECTOR('',#36873,10.);
#11123=VECTOR('',#36874,10.);
#11124=VECTOR('',#36875,10.);
#11125=VECTOR('',#36878,10.);
#11126=VECTOR('',#36879,10.);
#11127=VECTOR('',#36880,10.);
#11128=VECTOR('',#36883,10.);
#11129=VECTOR('',#36884,10.);
#11130=VECTOR('',#36885,10.);
#11131=VECTOR('',#36888,10.);
#11132=VECTOR('',#36889,10.);
#11133=VECTOR('',#36894,10.);
#11134=VECTOR('',#36895,10.);
#11135=VECTOR('',#36896,10.);
#11136=VECTOR('',#36897,10.);
#11137=VECTOR('',#36900,10.);
#11138=VECTOR('',#36901,10.);
#11139=VECTOR('',#36902,10.);
#11140=VECTOR('',#36905,10.);
#11141=VECTOR('',#36906,10.);
#11142=VECTOR('',#36907,10.);
#11143=VECTOR('',#36910,10.);
#11144=VECTOR('',#36911,10.);
#11145=VECTOR('',#36916,10.);
#11146=VECTOR('',#36917,10.);
#11147=VECTOR('',#36918,10.);
#11148=VECTOR('',#36919,10.);
#11149=VECTOR('',#36922,10.);
#11150=VECTOR('',#36923,10.);
#11151=VECTOR('',#36924,10.);
#11152=VECTOR('',#36927,10.);
#11153=VECTOR('',#36928,10.);
#11154=VECTOR('',#36929,10.);
#11155=VECTOR('',#36932,10.);
#11156=VECTOR('',#36933,10.);
#11157=VECTOR('',#36938,10.);
#11158=VECTOR('',#36939,10.);
#11159=VECTOR('',#36940,10.);
#11160=VECTOR('',#36941,10.);
#11161=VECTOR('',#36944,10.);
#11162=VECTOR('',#36945,10.);
#11163=VECTOR('',#36946,10.);
#11164=VECTOR('',#36949,10.);
#11165=VECTOR('',#36950,10.);
#11166=VECTOR('',#36951,10.);
#11167=VECTOR('',#36954,10.);
#11168=VECTOR('',#36955,10.);
#11169=VECTOR('',#36960,10.);
#11170=VECTOR('',#36961,10.);
#11171=VECTOR('',#36962,10.);
#11172=VECTOR('',#36963,10.);
#11173=VECTOR('',#36966,10.);
#11174=VECTOR('',#36967,10.);
#11175=VECTOR('',#36968,10.);
#11176=VECTOR('',#36971,10.);
#11177=VECTOR('',#36972,10.);
#11178=VECTOR('',#36973,10.);
#11179=VECTOR('',#36976,10.);
#11180=VECTOR('',#36977,10.);
#11181=VECTOR('',#36982,10.);
#11182=VECTOR('',#36983,10.);
#11183=VECTOR('',#36984,10.);
#11184=VECTOR('',#36985,10.);
#11185=VECTOR('',#36988,10.);
#11186=VECTOR('',#36989,10.);
#11187=VECTOR('',#36990,10.);
#11188=VECTOR('',#36993,10.);
#11189=VECTOR('',#36994,10.);
#11190=VECTOR('',#36995,10.);
#11191=VECTOR('',#36998,10.);
#11192=VECTOR('',#36999,10.);
#11193=VECTOR('',#37004,10.);
#11194=VECTOR('',#37005,10.);
#11195=VECTOR('',#37006,10.);
#11196=VECTOR('',#37007,10.);
#11197=VECTOR('',#37010,10.);
#11198=VECTOR('',#37011,10.);
#11199=VECTOR('',#37012,10.);
#11200=VECTOR('',#37015,10.);
#11201=VECTOR('',#37016,10.);
#11202=VECTOR('',#37017,10.);
#11203=VECTOR('',#37020,10.);
#11204=VECTOR('',#37021,10.);
#11205=VECTOR('',#37026,10.);
#11206=VECTOR('',#37027,10.);
#11207=VECTOR('',#37028,10.);
#11208=VECTOR('',#37029,10.);
#11209=VECTOR('',#37032,10.);
#11210=VECTOR('',#37033,10.);
#11211=VECTOR('',#37034,10.);
#11212=VECTOR('',#37037,10.);
#11213=VECTOR('',#37038,10.);
#11214=VECTOR('',#37039,10.);
#11215=VECTOR('',#37042,10.);
#11216=VECTOR('',#37043,10.);
#11217=VECTOR('',#37048,10.);
#11218=VECTOR('',#37049,10.);
#11219=VECTOR('',#37050,10.);
#11220=VECTOR('',#37051,10.);
#11221=VECTOR('',#37054,10.);
#11222=VECTOR('',#37055,10.);
#11223=VECTOR('',#37056,10.);
#11224=VECTOR('',#37059,10.);
#11225=VECTOR('',#37060,10.);
#11226=VECTOR('',#37061,10.);
#11227=VECTOR('',#37064,10.);
#11228=VECTOR('',#37065,10.);
#11229=VECTOR('',#37070,10.);
#11230=VECTOR('',#37071,10.);
#11231=VECTOR('',#37072,10.);
#11232=VECTOR('',#37073,10.);
#11233=VECTOR('',#37076,10.);
#11234=VECTOR('',#37077,10.);
#11235=VECTOR('',#37078,10.);
#11236=VECTOR('',#37081,10.);
#11237=VECTOR('',#37082,10.);
#11238=VECTOR('',#37083,10.);
#11239=VECTOR('',#37086,10.);
#11240=VECTOR('',#37087,10.);
#11241=VECTOR('',#37092,10.);
#11242=VECTOR('',#37093,10.);
#11243=VECTOR('',#37094,10.);
#11244=VECTOR('',#37095,10.);
#11245=VECTOR('',#37098,10.);
#11246=VECTOR('',#37099,10.);
#11247=VECTOR('',#37100,10.);
#11248=VECTOR('',#37103,10.);
#11249=VECTOR('',#37104,10.);
#11250=VECTOR('',#37105,10.);
#11251=VECTOR('',#37108,10.);
#11252=VECTOR('',#37109,10.);
#11253=VECTOR('',#37114,10.);
#11254=VECTOR('',#37115,10.);
#11255=VECTOR('',#37116,10.);
#11256=VECTOR('',#37117,10.);
#11257=VECTOR('',#37120,10.);
#11258=VECTOR('',#37121,10.);
#11259=VECTOR('',#37122,10.);
#11260=VECTOR('',#37125,10.);
#11261=VECTOR('',#37126,10.);
#11262=VECTOR('',#37127,10.);
#11263=VECTOR('',#37130,10.);
#11264=VECTOR('',#37131,10.);
#11265=VECTOR('',#37136,10.);
#11266=VECTOR('',#37137,10.);
#11267=VECTOR('',#37138,10.);
#11268=VECTOR('',#37139,10.);
#11269=VECTOR('',#37142,10.);
#11270=VECTOR('',#37143,10.);
#11271=VECTOR('',#37144,10.);
#11272=VECTOR('',#37147,10.);
#11273=VECTOR('',#37148,10.);
#11274=VECTOR('',#37149,10.);
#11275=VECTOR('',#37152,10.);
#11276=VECTOR('',#37153,10.);
#11277=VECTOR('',#37158,10.);
#11278=VECTOR('',#37159,10.);
#11279=VECTOR('',#37160,10.);
#11280=VECTOR('',#37161,10.);
#11281=VECTOR('',#37164,10.);
#11282=VECTOR('',#37165,10.);
#11283=VECTOR('',#37166,10.);
#11284=VECTOR('',#37169,10.);
#11285=VECTOR('',#37170,10.);
#11286=VECTOR('',#37171,10.);
#11287=VECTOR('',#37174,10.);
#11288=VECTOR('',#37175,10.);
#11289=VECTOR('',#37180,10.);
#11290=VECTOR('',#37181,10.);
#11291=VECTOR('',#37182,10.);
#11292=VECTOR('',#37183,10.);
#11293=VECTOR('',#37186,10.);
#11294=VECTOR('',#37187,10.);
#11295=VECTOR('',#37188,10.);
#11296=VECTOR('',#37191,10.);
#11297=VECTOR('',#37192,10.);
#11298=VECTOR('',#37193,10.);
#11299=VECTOR('',#37196,10.);
#11300=VECTOR('',#37197,10.);
#11301=VECTOR('',#37202,10.);
#11302=VECTOR('',#37203,10.);
#11303=VECTOR('',#37204,10.);
#11304=VECTOR('',#37205,10.);
#11305=VECTOR('',#37208,10.);
#11306=VECTOR('',#37209,10.);
#11307=VECTOR('',#37210,10.);
#11308=VECTOR('',#37213,10.);
#11309=VECTOR('',#37214,10.);
#11310=VECTOR('',#37215,10.);
#11311=VECTOR('',#37218,10.);
#11312=VECTOR('',#37219,10.);
#11313=VECTOR('',#37224,10.);
#11314=VECTOR('',#37225,10.);
#11315=VECTOR('',#37226,10.);
#11316=VECTOR('',#37227,10.);
#11317=VECTOR('',#37230,10.);
#11318=VECTOR('',#37231,10.);
#11319=VECTOR('',#37232,10.);
#11320=VECTOR('',#37235,10.);
#11321=VECTOR('',#37236,10.);
#11322=VECTOR('',#37237,10.);
#11323=VECTOR('',#37240,10.);
#11324=VECTOR('',#37241,10.);
#11325=VECTOR('',#37246,10.);
#11326=VECTOR('',#37247,10.);
#11327=VECTOR('',#37248,10.);
#11328=VECTOR('',#37249,10.);
#11329=VECTOR('',#37252,10.);
#11330=VECTOR('',#37253,10.);
#11331=VECTOR('',#37254,10.);
#11332=VECTOR('',#37257,10.);
#11333=VECTOR('',#37258,10.);
#11334=VECTOR('',#37259,10.);
#11335=VECTOR('',#37262,10.);
#11336=VECTOR('',#37263,10.);
#11337=VECTOR('',#37268,10.);
#11338=VECTOR('',#37269,10.);
#11339=VECTOR('',#37270,10.);
#11340=VECTOR('',#37271,10.);
#11341=VECTOR('',#37274,10.);
#11342=VECTOR('',#37275,10.);
#11343=VECTOR('',#37276,10.);
#11344=VECTOR('',#37279,10.);
#11345=VECTOR('',#37280,10.);
#11346=VECTOR('',#37281,10.);
#11347=VECTOR('',#37284,10.);
#11348=VECTOR('',#37285,10.);
#11349=VECTOR('',#37290,10.);
#11350=VECTOR('',#37291,10.);
#11351=VECTOR('',#37292,10.);
#11352=VECTOR('',#37293,10.);
#11353=VECTOR('',#37296,10.);
#11354=VECTOR('',#37297,10.);
#11355=VECTOR('',#37298,10.);
#11356=VECTOR('',#37301,10.);
#11357=VECTOR('',#37302,10.);
#11358=VECTOR('',#37303,10.);
#11359=VECTOR('',#37306,10.);
#11360=VECTOR('',#37307,10.);
#11361=VECTOR('',#37312,10.);
#11362=VECTOR('',#37313,10.);
#11363=VECTOR('',#37314,10.);
#11364=VECTOR('',#37315,10.);
#11365=VECTOR('',#37318,10.);
#11366=VECTOR('',#37319,10.);
#11367=VECTOR('',#37320,10.);
#11368=VECTOR('',#37323,10.);
#11369=VECTOR('',#37324,10.);
#11370=VECTOR('',#37325,10.);
#11371=VECTOR('',#37328,10.);
#11372=VECTOR('',#37329,10.);
#11373=VECTOR('',#37334,10.);
#11374=VECTOR('',#37335,10.);
#11375=VECTOR('',#37336,10.);
#11376=VECTOR('',#37337,10.);
#11377=VECTOR('',#37340,10.);
#11378=VECTOR('',#37341,10.);
#11379=VECTOR('',#37342,10.);
#11380=VECTOR('',#37345,10.);
#11381=VECTOR('',#37346,10.);
#11382=VECTOR('',#37347,10.);
#11383=VECTOR('',#37350,10.);
#11384=VECTOR('',#37351,10.);
#11385=VECTOR('',#37356,10.);
#11386=VECTOR('',#37357,10.);
#11387=VECTOR('',#37358,10.);
#11388=VECTOR('',#37359,10.);
#11389=VECTOR('',#37362,10.);
#11390=VECTOR('',#37363,10.);
#11391=VECTOR('',#37364,10.);
#11392=VECTOR('',#37367,10.);
#11393=VECTOR('',#37368,10.);
#11394=VECTOR('',#37369,10.);
#11395=VECTOR('',#37372,10.);
#11396=VECTOR('',#37373,10.);
#11397=VECTOR('',#37378,10.);
#11398=VECTOR('',#37379,10.);
#11399=VECTOR('',#37380,10.);
#11400=VECTOR('',#37381,10.);
#11401=VECTOR('',#37384,10.);
#11402=VECTOR('',#37385,10.);
#11403=VECTOR('',#37386,10.);
#11404=VECTOR('',#37389,10.);
#11405=VECTOR('',#37390,10.);
#11406=VECTOR('',#37391,10.);
#11407=VECTOR('',#37394,10.);
#11408=VECTOR('',#37395,10.);
#11409=VECTOR('',#37400,10.);
#11410=VECTOR('',#37401,10.);
#11411=VECTOR('',#37402,10.);
#11412=VECTOR('',#37403,10.);
#11413=VECTOR('',#37406,10.);
#11414=VECTOR('',#37407,10.);
#11415=VECTOR('',#37408,10.);
#11416=VECTOR('',#37411,10.);
#11417=VECTOR('',#37412,10.);
#11418=VECTOR('',#37413,10.);
#11419=VECTOR('',#37416,10.);
#11420=VECTOR('',#37417,10.);
#11421=VECTOR('',#37422,10.);
#11422=VECTOR('',#37423,10.);
#11423=VECTOR('',#37424,10.);
#11424=VECTOR('',#37425,10.);
#11425=VECTOR('',#37428,10.);
#11426=VECTOR('',#37429,10.);
#11427=VECTOR('',#37430,10.);
#11428=VECTOR('',#37433,10.);
#11429=VECTOR('',#37434,10.);
#11430=VECTOR('',#37435,10.);
#11431=VECTOR('',#37438,10.);
#11432=VECTOR('',#37439,10.);
#11433=VECTOR('',#37444,10.);
#11434=VECTOR('',#37445,10.);
#11435=VECTOR('',#37446,10.);
#11436=VECTOR('',#37447,10.);
#11437=VECTOR('',#37450,10.);
#11438=VECTOR('',#37451,10.);
#11439=VECTOR('',#37452,10.);
#11440=VECTOR('',#37455,10.);
#11441=VECTOR('',#37456,10.);
#11442=VECTOR('',#37457,10.);
#11443=VECTOR('',#37460,10.);
#11444=VECTOR('',#37461,10.);
#11445=VECTOR('',#37466,10.);
#11446=VECTOR('',#37467,10.);
#11447=VECTOR('',#37468,10.);
#11448=VECTOR('',#37469,10.);
#11449=VECTOR('',#37472,10.);
#11450=VECTOR('',#37473,10.);
#11451=VECTOR('',#37474,10.);
#11452=VECTOR('',#37477,10.);
#11453=VECTOR('',#37478,10.);
#11454=VECTOR('',#37479,10.);
#11455=VECTOR('',#37482,10.);
#11456=VECTOR('',#37483,10.);
#11457=VECTOR('',#37488,10.);
#11458=VECTOR('',#37489,10.);
#11459=VECTOR('',#37490,10.);
#11460=VECTOR('',#37491,10.);
#11461=VECTOR('',#37494,10.);
#11462=VECTOR('',#37495,10.);
#11463=VECTOR('',#37496,10.);
#11464=VECTOR('',#37499,10.);
#11465=VECTOR('',#37500,10.);
#11466=VECTOR('',#37501,10.);
#11467=VECTOR('',#37504,10.);
#11468=VECTOR('',#37505,10.);
#11469=VECTOR('',#37510,10.);
#11470=VECTOR('',#37511,10.);
#11471=VECTOR('',#37512,10.);
#11472=VECTOR('',#37513,10.);
#11473=VECTOR('',#37516,10.);
#11474=VECTOR('',#37517,10.);
#11475=VECTOR('',#37518,10.);
#11476=VECTOR('',#37521,10.);
#11477=VECTOR('',#37522,10.);
#11478=VECTOR('',#37523,10.);
#11479=VECTOR('',#37526,10.);
#11480=VECTOR('',#37527,10.);
#11481=VECTOR('',#37532,10.);
#11482=VECTOR('',#37533,10.);
#11483=VECTOR('',#37534,10.);
#11484=VECTOR('',#37535,10.);
#11485=VECTOR('',#37538,10.);
#11486=VECTOR('',#37539,10.);
#11487=VECTOR('',#37540,10.);
#11488=VECTOR('',#37543,10.);
#11489=VECTOR('',#37544,10.);
#11490=VECTOR('',#37545,10.);
#11491=VECTOR('',#37548,10.);
#11492=VECTOR('',#37549,10.);
#11493=VECTOR('',#37554,10.);
#11494=VECTOR('',#37555,10.);
#11495=VECTOR('',#37556,10.);
#11496=VECTOR('',#37557,10.);
#11497=VECTOR('',#37560,10.);
#11498=VECTOR('',#37561,10.);
#11499=VECTOR('',#37562,10.);
#11500=VECTOR('',#37565,10.);
#11501=VECTOR('',#37566,10.);
#11502=VECTOR('',#37567,10.);
#11503=VECTOR('',#37570,10.);
#11504=VECTOR('',#37571,10.);
#11505=VECTOR('',#37576,10.);
#11506=VECTOR('',#37577,10.);
#11507=VECTOR('',#37578,10.);
#11508=VECTOR('',#37579,10.);
#11509=VECTOR('',#37582,10.);
#11510=VECTOR('',#37583,10.);
#11511=VECTOR('',#37584,10.);
#11512=VECTOR('',#37587,10.);
#11513=VECTOR('',#37588,10.);
#11514=VECTOR('',#37589,10.);
#11515=VECTOR('',#37592,10.);
#11516=VECTOR('',#37593,10.);
#11517=VECTOR('',#37598,10.);
#11518=VECTOR('',#37599,10.);
#11519=VECTOR('',#37600,10.);
#11520=VECTOR('',#37601,10.);
#11521=VECTOR('',#37604,10.);
#11522=VECTOR('',#37605,10.);
#11523=VECTOR('',#37606,10.);
#11524=VECTOR('',#37609,10.);
#11525=VECTOR('',#37610,10.);
#11526=VECTOR('',#37611,10.);
#11527=VECTOR('',#37614,10.);
#11528=VECTOR('',#37615,10.);
#11529=VECTOR('',#37620,10.);
#11530=VECTOR('',#37621,10.);
#11531=VECTOR('',#37622,10.);
#11532=VECTOR('',#37623,10.);
#11533=VECTOR('',#37626,10.);
#11534=VECTOR('',#37627,10.);
#11535=VECTOR('',#37628,10.);
#11536=VECTOR('',#37631,10.);
#11537=VECTOR('',#37632,10.);
#11538=VECTOR('',#37633,10.);
#11539=VECTOR('',#37636,10.);
#11540=VECTOR('',#37637,10.);
#11541=VECTOR('',#37642,10.);
#11542=VECTOR('',#37643,10.);
#11543=VECTOR('',#37644,10.);
#11544=VECTOR('',#37645,10.);
#11545=VECTOR('',#37648,10.);
#11546=VECTOR('',#37649,10.);
#11547=VECTOR('',#37650,10.);
#11548=VECTOR('',#37653,10.);
#11549=VECTOR('',#37654,10.);
#11550=VECTOR('',#37655,10.);
#11551=VECTOR('',#37658,10.);
#11552=VECTOR('',#37659,10.);
#11553=VECTOR('',#37664,10.);
#11554=VECTOR('',#37665,10.);
#11555=VECTOR('',#37666,10.);
#11556=VECTOR('',#37667,10.);
#11557=VECTOR('',#37670,10.);
#11558=VECTOR('',#37671,10.);
#11559=VECTOR('',#37672,10.);
#11560=VECTOR('',#37675,10.);
#11561=VECTOR('',#37676,10.);
#11562=VECTOR('',#37677,10.);
#11563=VECTOR('',#37680,10.);
#11564=VECTOR('',#37681,10.);
#11565=VECTOR('',#37686,10.);
#11566=VECTOR('',#37687,10.);
#11567=VECTOR('',#37688,10.);
#11568=VECTOR('',#37689,10.);
#11569=VECTOR('',#37692,10.);
#11570=VECTOR('',#37693,10.);
#11571=VECTOR('',#37694,10.);
#11572=VECTOR('',#37697,10.);
#11573=VECTOR('',#37698,10.);
#11574=VECTOR('',#37699,10.);
#11575=VECTOR('',#37702,10.);
#11576=VECTOR('',#37703,10.);
#11577=VECTOR('',#37708,10.);
#11578=VECTOR('',#37709,10.);
#11579=VECTOR('',#37710,10.);
#11580=VECTOR('',#37711,10.);
#11581=VECTOR('',#37714,10.);
#11582=VECTOR('',#37715,10.);
#11583=VECTOR('',#37716,10.);
#11584=VECTOR('',#37719,10.);
#11585=VECTOR('',#37720,10.);
#11586=VECTOR('',#37721,10.);
#11587=VECTOR('',#37724,10.);
#11588=VECTOR('',#37725,10.);
#11589=VECTOR('',#37730,10.);
#11590=VECTOR('',#37731,10.);
#11591=VECTOR('',#37732,10.);
#11592=VECTOR('',#37733,10.);
#11593=VECTOR('',#37736,10.);
#11594=VECTOR('',#37737,10.);
#11595=VECTOR('',#37738,10.);
#11596=VECTOR('',#37741,10.);
#11597=VECTOR('',#37742,10.);
#11598=VECTOR('',#37743,10.);
#11599=VECTOR('',#37746,10.);
#11600=VECTOR('',#37747,10.);
#11601=VECTOR('',#37752,10.);
#11602=VECTOR('',#37753,10.);
#11603=VECTOR('',#37754,10.);
#11604=VECTOR('',#37755,10.);
#11605=VECTOR('',#37758,10.);
#11606=VECTOR('',#37759,10.);
#11607=VECTOR('',#37760,10.);
#11608=VECTOR('',#37763,10.);
#11609=VECTOR('',#37764,10.);
#11610=VECTOR('',#37765,10.);
#11611=VECTOR('',#37768,10.);
#11612=VECTOR('',#37769,10.);
#11613=VECTOR('',#37774,10.);
#11614=VECTOR('',#37775,10.);
#11615=VECTOR('',#37776,10.);
#11616=VECTOR('',#37777,10.);
#11617=VECTOR('',#37780,10.);
#11618=VECTOR('',#37781,10.);
#11619=VECTOR('',#37782,10.);
#11620=VECTOR('',#37785,10.);
#11621=VECTOR('',#37786,10.);
#11622=VECTOR('',#37787,10.);
#11623=VECTOR('',#37790,10.);
#11624=VECTOR('',#37791,10.);
#11625=VECTOR('',#37796,10.);
#11626=VECTOR('',#37797,10.);
#11627=VECTOR('',#37798,10.);
#11628=VECTOR('',#37799,10.);
#11629=VECTOR('',#37802,10.);
#11630=VECTOR('',#37803,10.);
#11631=VECTOR('',#37804,10.);
#11632=VECTOR('',#37807,10.);
#11633=VECTOR('',#37808,10.);
#11634=VECTOR('',#37809,10.);
#11635=VECTOR('',#37812,10.);
#11636=VECTOR('',#37813,10.);
#11637=VECTOR('',#37818,10.);
#11638=VECTOR('',#37819,10.);
#11639=VECTOR('',#37820,10.);
#11640=VECTOR('',#37821,10.);
#11641=VECTOR('',#37824,10.);
#11642=VECTOR('',#37825,10.);
#11643=VECTOR('',#37826,10.);
#11644=VECTOR('',#37829,10.);
#11645=VECTOR('',#37830,10.);
#11646=VECTOR('',#37831,10.);
#11647=VECTOR('',#37834,10.);
#11648=VECTOR('',#37835,10.);
#11649=VECTOR('',#37840,10.);
#11650=VECTOR('',#37841,10.);
#11651=VECTOR('',#37842,10.);
#11652=VECTOR('',#37843,10.);
#11653=VECTOR('',#37846,10.);
#11654=VECTOR('',#37847,10.);
#11655=VECTOR('',#37848,10.);
#11656=VECTOR('',#37851,10.);
#11657=VECTOR('',#37852,10.);
#11658=VECTOR('',#37853,10.);
#11659=VECTOR('',#37856,10.);
#11660=VECTOR('',#37857,10.);
#11661=VECTOR('',#37862,10.);
#11662=VECTOR('',#37863,10.);
#11663=VECTOR('',#37864,10.);
#11664=VECTOR('',#37865,10.);
#11665=VECTOR('',#37868,10.);
#11666=VECTOR('',#37869,10.);
#11667=VECTOR('',#37870,10.);
#11668=VECTOR('',#37873,10.);
#11669=VECTOR('',#37874,10.);
#11670=VECTOR('',#37875,10.);
#11671=VECTOR('',#37878,10.);
#11672=VECTOR('',#37879,10.);
#11673=VECTOR('',#37884,10.);
#11674=VECTOR('',#37885,10.);
#11675=VECTOR('',#37886,10.);
#11676=VECTOR('',#37887,10.);
#11677=VECTOR('',#37890,10.);
#11678=VECTOR('',#37891,10.);
#11679=VECTOR('',#37892,10.);
#11680=VECTOR('',#37895,10.);
#11681=VECTOR('',#37896,10.);
#11682=VECTOR('',#37897,10.);
#11683=VECTOR('',#37900,10.);
#11684=VECTOR('',#37901,10.);
#11685=VECTOR('',#37906,10.);
#11686=VECTOR('',#37907,10.);
#11687=VECTOR('',#37908,10.);
#11688=VECTOR('',#37909,10.);
#11689=VECTOR('',#37912,10.);
#11690=VECTOR('',#37913,10.);
#11691=VECTOR('',#37914,10.);
#11692=VECTOR('',#37917,10.);
#11693=VECTOR('',#37918,10.);
#11694=VECTOR('',#37919,10.);
#11695=VECTOR('',#37922,10.);
#11696=VECTOR('',#37923,10.);
#11697=VECTOR('',#37928,10.);
#11698=VECTOR('',#37929,10.);
#11699=VECTOR('',#37930,10.);
#11700=VECTOR('',#37931,10.);
#11701=VECTOR('',#37934,10.);
#11702=VECTOR('',#37935,10.);
#11703=VECTOR('',#37936,10.);
#11704=VECTOR('',#37939,10.);
#11705=VECTOR('',#37940,10.);
#11706=VECTOR('',#37941,10.);
#11707=VECTOR('',#37944,10.);
#11708=VECTOR('',#37945,10.);
#11709=VECTOR('',#37950,10.);
#11710=VECTOR('',#37951,10.);
#11711=VECTOR('',#37952,10.);
#11712=VECTOR('',#37953,10.);
#11713=VECTOR('',#37956,10.);
#11714=VECTOR('',#37957,10.);
#11715=VECTOR('',#37958,10.);
#11716=VECTOR('',#37961,10.);
#11717=VECTOR('',#37962,10.);
#11718=VECTOR('',#37963,10.);
#11719=VECTOR('',#37966,10.);
#11720=VECTOR('',#37967,10.);
#11721=VECTOR('',#37972,10.);
#11722=VECTOR('',#37973,10.);
#11723=VECTOR('',#37974,10.);
#11724=VECTOR('',#37975,10.);
#11725=VECTOR('',#37978,10.);
#11726=VECTOR('',#37979,10.);
#11727=VECTOR('',#37980,10.);
#11728=VECTOR('',#37983,10.);
#11729=VECTOR('',#37984,10.);
#11730=VECTOR('',#37985,10.);
#11731=VECTOR('',#37988,10.);
#11732=VECTOR('',#37989,10.);
#11733=VECTOR('',#37994,10.);
#11734=VECTOR('',#37995,10.);
#11735=VECTOR('',#37996,10.);
#11736=VECTOR('',#37997,10.);
#11737=VECTOR('',#38000,10.);
#11738=VECTOR('',#38001,10.);
#11739=VECTOR('',#38002,10.);
#11740=VECTOR('',#38005,10.);
#11741=VECTOR('',#38006,10.);
#11742=VECTOR('',#38007,10.);
#11743=VECTOR('',#38010,10.);
#11744=VECTOR('',#38011,10.);
#11745=VECTOR('',#38016,10.);
#11746=VECTOR('',#38017,10.);
#11747=VECTOR('',#38018,10.);
#11748=VECTOR('',#38019,10.);
#11749=VECTOR('',#38022,10.);
#11750=VECTOR('',#38023,10.);
#11751=VECTOR('',#38024,10.);
#11752=VECTOR('',#38027,10.);
#11753=VECTOR('',#38028,10.);
#11754=VECTOR('',#38029,10.);
#11755=VECTOR('',#38032,10.);
#11756=VECTOR('',#38033,10.);
#11757=VECTOR('',#38038,10.);
#11758=VECTOR('',#38039,10.);
#11759=VECTOR('',#38040,10.);
#11760=VECTOR('',#38041,10.);
#11761=VECTOR('',#38044,10.);
#11762=VECTOR('',#38045,10.);
#11763=VECTOR('',#38046,10.);
#11764=VECTOR('',#38049,10.);
#11765=VECTOR('',#38050,10.);
#11766=VECTOR('',#38051,10.);
#11767=VECTOR('',#38054,10.);
#11768=VECTOR('',#38055,10.);
#11769=VECTOR('',#38060,10.);
#11770=VECTOR('',#38061,10.);
#11771=VECTOR('',#38062,10.);
#11772=VECTOR('',#38063,10.);
#11773=VECTOR('',#38066,10.);
#11774=VECTOR('',#38067,10.);
#11775=VECTOR('',#38068,10.);
#11776=VECTOR('',#38071,10.);
#11777=VECTOR('',#38072,10.);
#11778=VECTOR('',#38073,10.);
#11779=VECTOR('',#38076,10.);
#11780=VECTOR('',#38077,10.);
#11781=VECTOR('',#38082,10.);
#11782=VECTOR('',#38083,10.);
#11783=VECTOR('',#38084,10.);
#11784=VECTOR('',#38085,10.);
#11785=VECTOR('',#38088,10.);
#11786=VECTOR('',#38089,10.);
#11787=VECTOR('',#38090,10.);
#11788=VECTOR('',#38093,10.);
#11789=VECTOR('',#38094,10.);
#11790=VECTOR('',#38095,10.);
#11791=VECTOR('',#38098,10.);
#11792=VECTOR('',#38099,10.);
#11793=VECTOR('',#38104,10.);
#11794=VECTOR('',#38105,10.);
#11795=VECTOR('',#38106,10.);
#11796=VECTOR('',#38107,10.);
#11797=VECTOR('',#38110,10.);
#11798=VECTOR('',#38111,10.);
#11799=VECTOR('',#38112,10.);
#11800=VECTOR('',#38115,10.);
#11801=VECTOR('',#38116,10.);
#11802=VECTOR('',#38117,10.);
#11803=VECTOR('',#38120,10.);
#11804=VECTOR('',#38121,10.);
#11805=VECTOR('',#38126,10.);
#11806=VECTOR('',#38127,10.);
#11807=VECTOR('',#38128,10.);
#11808=VECTOR('',#38129,10.);
#11809=VECTOR('',#38132,10.);
#11810=VECTOR('',#38133,10.);
#11811=VECTOR('',#38134,10.);
#11812=VECTOR('',#38137,10.);
#11813=VECTOR('',#38138,10.);
#11814=VECTOR('',#38139,10.);
#11815=VECTOR('',#38142,10.);
#11816=VECTOR('',#38143,10.);
#11817=VECTOR('',#38148,10.);
#11818=VECTOR('',#38149,10.);
#11819=VECTOR('',#38150,10.);
#11820=VECTOR('',#38151,10.);
#11821=VECTOR('',#38154,10.);
#11822=VECTOR('',#38155,10.);
#11823=VECTOR('',#38156,10.);
#11824=VECTOR('',#38159,10.);
#11825=VECTOR('',#38160,10.);
#11826=VECTOR('',#38161,10.);
#11827=VECTOR('',#38164,10.);
#11828=VECTOR('',#38165,10.);
#11829=VECTOR('',#38170,10.);
#11830=VECTOR('',#38171,10.);
#11831=VECTOR('',#38172,10.);
#11832=VECTOR('',#38173,10.);
#11833=VECTOR('',#38176,10.);
#11834=VECTOR('',#38177,10.);
#11835=VECTOR('',#38178,10.);
#11836=VECTOR('',#38181,10.);
#11837=VECTOR('',#38182,10.);
#11838=VECTOR('',#38183,10.);
#11839=VECTOR('',#38186,10.);
#11840=VECTOR('',#38187,10.);
#11841=VECTOR('',#38192,10.);
#11842=VECTOR('',#38193,10.);
#11843=VECTOR('',#38194,10.);
#11844=VECTOR('',#38195,10.);
#11845=VECTOR('',#38198,10.);
#11846=VECTOR('',#38199,10.);
#11847=VECTOR('',#38200,10.);
#11848=VECTOR('',#38203,10.);
#11849=VECTOR('',#38204,10.);
#11850=VECTOR('',#38205,10.);
#11851=VECTOR('',#38208,10.);
#11852=VECTOR('',#38209,10.);
#11853=VECTOR('',#38214,10.);
#11854=VECTOR('',#38215,10.);
#11855=VECTOR('',#38216,10.);
#11856=VECTOR('',#38217,10.);
#11857=VECTOR('',#38220,10.);
#11858=VECTOR('',#38221,10.);
#11859=VECTOR('',#38222,10.);
#11860=VECTOR('',#38225,10.);
#11861=VECTOR('',#38226,10.);
#11862=VECTOR('',#38227,10.);
#11863=VECTOR('',#38230,10.);
#11864=VECTOR('',#38231,10.);
#11865=VECTOR('',#38236,10.);
#11866=VECTOR('',#38237,10.);
#11867=VECTOR('',#38238,10.);
#11868=VECTOR('',#38239,10.);
#11869=VECTOR('',#38242,10.);
#11870=VECTOR('',#38243,10.);
#11871=VECTOR('',#38244,10.);
#11872=VECTOR('',#38247,10.);
#11873=VECTOR('',#38248,10.);
#11874=VECTOR('',#38249,10.);
#11875=VECTOR('',#38252,10.);
#11876=VECTOR('',#38253,10.);
#11877=VECTOR('',#38260,1.1);
#11878=VECTOR('',#38267,1.1);
#11879=VECTOR('',#38272,10.);
#11880=VECTOR('',#38273,10.);
#11881=VECTOR('',#38274,10.);
#11882=VECTOR('',#38275,10.);
#11883=VECTOR('',#38282,10.);
#11884=VECTOR('',#38285,10.);
#11885=VECTOR('',#38286,10.);
#11886=VECTOR('',#38287,10.);
#11887=VECTOR('',#38294,10.);
#11888=VECTOR('',#38297,10.);
#11889=VECTOR('',#38298,10.);
#11890=VECTOR('',#38299,10.);
#11891=VECTOR('',#38306,10.);
#11892=VECTOR('',#38309,10.);
#11893=VECTOR('',#38310,10.);
#11894=VECTOR('',#38311,10.);
#11895=VECTOR('',#38326,10.);
#11896=VECTOR('',#38327,10.);
#11897=VECTOR('',#38328,10.);
#11898=VECTOR('',#38329,10.);
#11899=VECTOR('',#38332,10.);
#11900=VECTOR('',#38333,10.);
#11901=VECTOR('',#38334,10.);
#11902=VECTOR('',#38337,10.);
#11903=VECTOR('',#38338,10.);
#11904=VECTOR('',#38339,10.);
#11905=VECTOR('',#38342,10.);
#11906=VECTOR('',#38343,10.);
#11907=VECTOR('',#38348,10.);
#11908=VECTOR('',#38349,10.);
#11909=VECTOR('',#38350,10.);
#11910=VECTOR('',#38351,10.);
#11911=VECTOR('',#38354,10.);
#11912=VECTOR('',#38355,10.);
#11913=VECTOR('',#38356,10.);
#11914=VECTOR('',#38359,10.);
#11915=VECTOR('',#38360,10.);
#11916=VECTOR('',#38361,10.);
#11917=VECTOR('',#38364,10.);
#11918=VECTOR('',#38365,10.);
#11919=VECTOR('',#38370,10.);
#11920=VECTOR('',#38371,10.);
#11921=VECTOR('',#38372,10.);
#11922=VECTOR('',#38373,10.);
#11923=VECTOR('',#38376,10.);
#11924=VECTOR('',#38377,10.);
#11925=VECTOR('',#38378,10.);
#11926=VECTOR('',#38381,10.);
#11927=VECTOR('',#38382,10.);
#11928=VECTOR('',#38383,10.);
#11929=VECTOR('',#38386,10.);
#11930=VECTOR('',#38387,10.);
#11931=VECTOR('',#38392,10.);
#11932=VECTOR('',#38393,10.);
#11933=VECTOR('',#38394,10.);
#11934=VECTOR('',#38395,10.);
#11935=VECTOR('',#38398,10.);
#11936=VECTOR('',#38399,10.);
#11937=VECTOR('',#38400,10.);
#11938=VECTOR('',#38403,10.);
#11939=VECTOR('',#38404,10.);
#11940=VECTOR('',#38405,10.);
#11941=VECTOR('',#38408,10.);
#11942=VECTOR('',#38409,10.);
#11943=VECTOR('',#38414,10.);
#11944=VECTOR('',#38415,10.);
#11945=VECTOR('',#38416,10.);
#11946=VECTOR('',#38417,10.);
#11947=VECTOR('',#38420,10.);
#11948=VECTOR('',#38421,10.);
#11949=VECTOR('',#38422,10.);
#11950=VECTOR('',#38425,10.);
#11951=VECTOR('',#38426,10.);
#11952=VECTOR('',#38427,10.);
#11953=VECTOR('',#38430,10.);
#11954=VECTOR('',#38431,10.);
#11955=VECTOR('',#38436,10.);
#11956=VECTOR('',#38437,10.);
#11957=VECTOR('',#38438,10.);
#11958=VECTOR('',#38439,10.);
#11959=VECTOR('',#38442,10.);
#11960=VECTOR('',#38443,10.);
#11961=VECTOR('',#38444,10.);
#11962=VECTOR('',#38447,10.);
#11963=VECTOR('',#38448,10.);
#11964=VECTOR('',#38449,10.);
#11965=VECTOR('',#38452,10.);
#11966=VECTOR('',#38453,10.);
#11967=VECTOR('',#38458,10.);
#11968=VECTOR('',#38459,10.);
#11969=VECTOR('',#38460,10.);
#11970=VECTOR('',#38461,10.);
#11971=VECTOR('',#38464,10.);
#11972=VECTOR('',#38465,10.);
#11973=VECTOR('',#38466,10.);
#11974=VECTOR('',#38469,10.);
#11975=VECTOR('',#38470,10.);
#11976=VECTOR('',#38471,10.);
#11977=VECTOR('',#38474,10.);
#11978=VECTOR('',#38475,10.);
#11979=VECTOR('',#38480,10.);
#11980=VECTOR('',#38481,10.);
#11981=VECTOR('',#38482,10.);
#11982=VECTOR('',#38483,10.);
#11983=VECTOR('',#38486,10.);
#11984=VECTOR('',#38487,10.);
#11985=VECTOR('',#38488,10.);
#11986=VECTOR('',#38491,10.);
#11987=VECTOR('',#38492,10.);
#11988=VECTOR('',#38493,10.);
#11989=VECTOR('',#38496,10.);
#11990=VECTOR('',#38497,10.);
#11991=VECTOR('',#38502,10.);
#11992=VECTOR('',#38503,10.);
#11993=VECTOR('',#38504,10.);
#11994=VECTOR('',#38505,10.);
#11995=VECTOR('',#38508,10.);
#11996=VECTOR('',#38509,10.);
#11997=VECTOR('',#38510,10.);
#11998=VECTOR('',#38513,10.);
#11999=VECTOR('',#38514,10.);
#12000=VECTOR('',#38515,10.);
#12001=VECTOR('',#38518,10.);
#12002=VECTOR('',#38519,10.);
#12003=VECTOR('',#38524,10.);
#12004=VECTOR('',#38525,10.);
#12005=VECTOR('',#38526,10.);
#12006=VECTOR('',#38527,10.);
#12007=VECTOR('',#38530,10.);
#12008=VECTOR('',#38531,10.);
#12009=VECTOR('',#38532,10.);
#12010=VECTOR('',#38535,10.);
#12011=VECTOR('',#38536,10.);
#12012=VECTOR('',#38537,10.);
#12013=VECTOR('',#38540,10.);
#12014=VECTOR('',#38541,10.);
#12015=VECTOR('',#38546,10.);
#12016=VECTOR('',#38547,10.);
#12017=VECTOR('',#38548,10.);
#12018=VECTOR('',#38549,10.);
#12019=VECTOR('',#38552,10.);
#12020=VECTOR('',#38553,10.);
#12021=VECTOR('',#38554,10.);
#12022=VECTOR('',#38557,10.);
#12023=VECTOR('',#38558,10.);
#12024=VECTOR('',#38559,10.);
#12025=VECTOR('',#38562,10.);
#12026=VECTOR('',#38563,10.);
#12027=VECTOR('',#38570,1.1);
#12028=VECTOR('',#38577,1.1);
#12029=VECTOR('',#38582,10.);
#12030=VECTOR('',#38583,10.);
#12031=VECTOR('',#38584,10.);
#12032=VECTOR('',#38585,10.);
#12033=VECTOR('',#38588,10.);
#12034=VECTOR('',#38589,10.);
#12035=VECTOR('',#38590,10.);
#12036=VECTOR('',#38593,10.);
#12037=VECTOR('',#38594,10.);
#12038=VECTOR('',#38595,10.);
#12039=VECTOR('',#38598,10.);
#12040=VECTOR('',#38599,10.);
#12041=VECTOR('',#38600,10.);
#12042=VECTOR('',#38603,10.);
#12043=VECTOR('',#38604,10.);
#12044=VECTOR('',#38605,10.);
#12045=VECTOR('',#38608,10.);
#12046=VECTOR('',#38609,10.);
#12047=VECTOR('',#38610,10.);
#12048=VECTOR('',#38613,10.);
#12049=VECTOR('',#38614,10.);
#12050=VECTOR('',#38615,10.);
#12051=VECTOR('',#38618,10.);
#12052=VECTOR('',#38619,10.);
#12053=VECTOR('',#38634,10.);
#12054=VECTOR('',#38637,10.);
#12055=VECTOR('',#38638,10.);
#12056=VECTOR('',#38639,10.);
#12057=VECTOR('',#38640,10.);
#12058=VECTOR('',#38641,10.);
#12059=VECTOR('',#38642,10.);
#12060=VECTOR('',#38645,10.);
#12061=VECTOR('',#38648,10.);
#12062=VECTOR('',#38651,10.);
#12063=VECTOR('',#38660,10.);
#12064=VECTOR('',#38661,10.);
#12065=VECTOR('',#38662,10.);
#12066=VECTOR('',#38663,10.);
#12067=VECTOR('',#38664,10.);
#12068=VECTOR('',#38665,10.);
#12069=VECTOR('',#38666,10.);
#12070=VECTOR('',#38667,10.);
#12071=VECTOR('',#38668,10.);
#12072=VECTOR('',#38687,1.7);
#12073=VECTOR('',#38696,1.7);
#12074=VECTOR('',#38705,10.);
#12075=VECTOR('',#38706,10.);
#12076=VECTOR('',#38707,10.);
#12077=VECTOR('',#38708,10.);
#12078=VECTOR('',#38709,10.);
#12079=VECTOR('',#38712,10.);
#12080=VECTOR('',#38713,10.);
#12081=VECTOR('',#38714,10.);
#12082=VECTOR('',#38721,10.);
#12083=VECTOR('',#38726,10.);
#12084=VECTOR('',#38727,10.);
#12085=VECTOR('',#38734,10.);
#12086=VECTOR('',#38735,10.);
#12087=VECTOR('',#38736,10.);
#12088=VECTOR('',#38743,10.);
#12089=VECTOR('',#38748,10.);
#12090=VECTOR('',#38749,10.);
#12091=VECTOR('',#38756,10.);
#12092=VECTOR('',#38757,10.);
#12093=VECTOR('',#38758,10.);
#12094=VECTOR('',#38759,10.);
#12095=VECTOR('',#38760,10.);
#12096=VECTOR('',#38763,10.);
#12097=VECTOR('',#38764,10.);
#12098=VECTOR('',#38767,10.);
#12099=VECTOR('',#38768,10.);
#12100=VECTOR('',#38771,10.);
#12101=VECTOR('',#38774,10.);
#12102=VECTOR('',#38775,10.);
#12103=VECTOR('',#38784,1.4635);
#12104=VECTOR('',#38789,1.4635);
#12105=VECTOR('',#38792,1.4635);
#12106=VECTOR('',#38795,1.4635);
#12107=VECTOR('',#38798,1.4635);
#12108=VECTOR('',#38801,1.4635);
#12109=VECTOR('',#38804,1.4635);
#12110=VECTOR('',#38807,1.4635);
#12111=VECTOR('',#38810,1.4635);
#12112=VECTOR('',#38813,1.17775);
#12113=VECTOR('',#38818,1.17775);
#12114=VECTOR('',#38821,1.17775);
#12115=VECTOR('',#38824,1.17775);
#12116=VECTOR('',#38827,1.17775);
#12117=VECTOR('',#38830,1.17775);
#12118=VECTOR('',#38833,1.17775);
#12119=VECTOR('',#38836,1.17775);
#12120=VECTOR('',#38871,0.916025403784424);
#12121=VECTOR('',#38876,10.);
#12122=VECTOR('',#38877,10.);
#12123=VECTOR('',#38882,10.);
#12124=VECTOR('',#38885,10.);
#12125=VECTOR('',#38888,10.);
#12126=VECTOR('',#38889,10.);
#12127=VECTOR('',#38894,10.);
#12128=VECTOR('',#38897,10.);
#12129=VECTOR('',#38900,10.);
#12130=VECTOR('',#38901,10.);
#12131=VECTOR('',#38906,10.);
#12132=VECTOR('',#38909,10.);
#12133=VECTOR('',#38912,10.);
#12134=VECTOR('',#38913,10.);
#12135=VECTOR('',#38914,10.);
#12136=VECTOR('',#38915,10.);
#12137=VECTOR('',#38918,10.);
#12138=VECTOR('',#38919,10.);
#12139=VECTOR('',#38920,10.);
#12140=VECTOR('',#38923,10.);
#12141=VECTOR('',#38924,10.);
#12142=VECTOR('',#38925,10.);
#12143=VECTOR('',#38932,10.);
#12144=VECTOR('',#38937,10.);
#12145=VECTOR('',#38940,10.);
#12146=VECTOR('',#38943,10.);
#12147=VECTOR('',#38948,10.);
#12148=VECTOR('',#38965,10.);
#12149=VECTOR('',#38970,0.433012701892235);
#12150=VECTOR('',#38973,10.);
#12151=VECTOR('',#38974,10.);
#12152=VECTOR('',#38985,1.25);
#12153=VECTOR('',#38988,1.35);
#12154=VECTOR('',#38999,1.125);
#12155=VECTOR('',#39004,1.05);
#12156=VECTOR('',#39011,10.);
#12157=VECTOR('',#39012,10.);
#12158=VECTOR('',#39013,10.);
#12159=VECTOR('',#39014,10.);
#12160=VECTOR('',#39017,1.05);
#12161=VECTOR('',#39022,1.125);
#12162=VECTOR('',#39027,1.05);
#12163=VECTOR('',#39034,10.);
#12164=VECTOR('',#39035,10.);
#12165=VECTOR('',#39036,10.);
#12166=VECTOR('',#39037,10.);
#12167=VECTOR('',#39040,0.525);
#12168=VECTOR('',#39045,1.65);
#12169=VECTOR('',#39050,9.99999999999999);
#12170=VECTOR('',#39051,10.);
#12171=VECTOR('',#39052,10.);
#12172=VECTOR('',#39053,10.);
#12173=VECTOR('',#39054,10.);
#12174=VECTOR('',#39055,10.);
#12175=VECTOR('',#39066,1.55);
#12176=VECTOR('',#39073,1.65);
#12177=VECTOR('',#39076,1.55);
#12178=VECTOR('',#39081,0.775000000000001);
#12179=VECTOR('',#39084,0.775);
#12180=VECTOR('',#39089,3.15);
#12181=VECTOR('',#39092,3.);
#12182=VECTOR('',#39099,3.15);
#12183=VECTOR('',#39102,3.);
#12184=VECTOR('',#39115,1.7);
#12185=VECTOR('',#39120,1.7);
#12186=VECTOR('',#39127,2.165);
#12187=VECTOR('',#39134,2.015);
#12188=VECTOR('',#39137,9.99999999999999);
#12189=VECTOR('',#39138,10.);
#12190=VECTOR('',#39139,10.);
#12191=VECTOR('',#39140,10.);
#12192=VECTOR('',#39141,10.);
#12193=VECTOR('',#39142,10.);
#12194=VECTOR('',#39145,2.165);
#12195=VECTOR('',#39148,10.);
#12196=VECTOR('',#39151,10.);
#12197=VECTOR('',#39154,10.);
#12198=VECTOR('',#39157,10.);
#12199=VECTOR('',#39166,1.4635);
#12200=VECTOR('',#39171,1.4635);
#12201=VECTOR('',#39174,1.4635);
#12202=VECTOR('',#39177,1.4635);
#12203=VECTOR('',#39180,1.4635);
#12204=VECTOR('',#39183,1.4635);
#12205=VECTOR('',#39186,1.4635);
#12206=VECTOR('',#39189,1.4635);
#12207=VECTOR('',#39192,1.4635);
#12208=VECTOR('',#39195,1.4635);
#12209=VECTOR('',#39198,1.4635);
#12210=VECTOR('',#39201,1.4635);
#12211=VECTOR('',#39204,1.4635);
#12212=VECTOR('',#39207,1.4635);
#12213=VECTOR('',#39210,1.4635);
#12214=VECTOR('',#39213,1.4635);
#12215=VECTOR('',#39216,1.4635);
#12216=VECTOR('',#39219,1.4635);
#12217=VECTOR('',#39222,1.4635);
#12218=VECTOR('',#39225,1.4635);
#12219=VECTOR('',#39228,1.4635);
#12220=VECTOR('',#39231,1.4635);
#12221=VECTOR('',#39234,1.4635);
#12222=VECTOR('',#39237,1.17775);
#12223=VECTOR('',#39242,1.17775);
#12224=VECTOR('',#39245,1.17775);
#12225=VECTOR('',#39248,1.17775);
#12226=VECTOR('',#39251,1.17775);
#12227=VECTOR('',#39254,1.17775);
#12228=VECTOR('',#39257,1.17775);
#12229=VECTOR('',#39260,1.17775);
#12230=VECTOR('',#39263,1.17775);
#12231=VECTOR('',#39266,1.17775);
#12232=VECTOR('',#39269,1.17775);
#12233=VECTOR('',#39272,1.17775);
#12234=VECTOR('',#39275,1.17775);
#12235=VECTOR('',#39278,1.17775);
#12236=VECTOR('',#39281,1.17775);
#12237=VECTOR('',#39284,1.17775);
#12238=VECTOR('',#39287,1.17775);
#12239=VECTOR('',#39290,1.17775);
#12240=VECTOR('',#39293,1.17775);
#12241=VECTOR('',#39296,1.17775);
#12242=VECTOR('',#39299,1.17775);
#12243=VECTOR('',#39302,1.17775);
#12244=VECTOR('',#39305,1.17775);
#12245=VECTOR('',#39338,1.2885);
#12246=VECTOR('',#39347,10.);
#12247=VECTOR('',#39348,10.);
#12248=VECTOR('',#39351,10.);
#12249=VECTOR('',#39352,10.);
#12250=VECTOR('',#39355,10.);
#12251=VECTOR('',#39360,2.75);
#12252=VECTOR('',#39367,10.);
#12253=VECTOR('',#39370,10.);
#12254=VECTOR('',#39373,10.);
#12255=VECTOR('',#39376,10.);
#12256=VECTOR('',#39379,10.);
#12257=VECTOR('',#39382,10.);
#12258=VECTOR('',#39385,10.);
#12259=VECTOR('',#39388,10.);
#12260=VECTOR('',#39391,10.);
#12261=VECTOR('',#39394,10.);
#12262=VECTOR('',#39397,10.);
#12263=VECTOR('',#39400,10.);
#12264=VECTOR('',#39403,10.);
#12265=VECTOR('',#39406,10.);
#12266=VECTOR('',#39409,10.);
#12267=VECTOR('',#39412,10.);
#12268=VECTOR('',#39415,10.);
#12269=VECTOR('',#39418,10.);
#12270=VECTOR('',#39421,10.);
#12271=VECTOR('',#39424,10.);
#12272=VECTOR('',#39427,10.);
#12273=VECTOR('',#39430,10.);
#12274=VECTOR('',#39433,10.);
#12275=VECTOR('',#39436,10.);
#12276=VECTOR('',#39439,10.);
#12277=VECTOR('',#39442,10.);
#12278=VECTOR('',#39445,10.);
#12279=VECTOR('',#39448,10.);
#12280=VECTOR('',#39451,10.);
#12281=VECTOR('',#39454,10.);
#12282=VECTOR('',#39457,10.);
#12283=VECTOR('',#39460,10.);
#12284=VECTOR('',#39463,10.);
#12285=VECTOR('',#39468,10.);
#12286=VECTOR('',#39471,10.);
#12287=VECTOR('',#39474,10.);
#12288=VECTOR('',#39477,10.);
#12289=VECTOR('',#39480,10.);
#12290=VECTOR('',#39483,10.);
#12291=VECTOR('',#39486,10.);
#12292=VECTOR('',#39489,10.);
#12293=VECTOR('',#39492,10.);
#12294=VECTOR('',#39495,10.);
#12295=VECTOR('',#39498,10.);
#12296=VECTOR('',#39501,10.);
#12297=VECTOR('',#39504,10.);
#12298=VECTOR('',#39507,10.);
#12299=VECTOR('',#39510,10.);
#12300=VECTOR('',#39513,10.);
#12301=VECTOR('',#39516,10.);
#12302=VECTOR('',#39519,10.);
#12303=VECTOR('',#39522,10.);
#12304=VECTOR('',#39525,10.);
#12305=VECTOR('',#39528,10.);
#12306=VECTOR('',#39531,10.);
#12307=VECTOR('',#39534,10.);
#12308=VECTOR('',#39537,10.);
#12309=VECTOR('',#39540,10.);
#12310=VECTOR('',#39543,10.);
#12311=VECTOR('',#39546,10.);
#12312=VECTOR('',#39549,10.);
#12313=VECTOR('',#39552,10.);
#12314=VECTOR('',#39555,10.);
#12315=VECTOR('',#39558,10.);
#12316=VECTOR('',#39561,10.);
#12317=VECTOR('',#39564,10.);
#12318=VECTOR('',#39567,10.);
#12319=VECTOR('',#39570,10.);
#12320=VECTOR('',#39573,10.);
#12321=VECTOR('',#39576,10.);
#12322=VECTOR('',#39579,10.);
#12323=VECTOR('',#39580,10.);
#12324=VECTOR('',#39583,10.);
#12325=VECTOR('',#39588,2.6);
#12326=VECTOR('',#39593,10.);
#12327=VECTOR('',#39594,10.);
#12328=VECTOR('',#39597,10.);
#12329=VECTOR('',#39602,10.);
#12330=VECTOR('',#39603,10.);
#12331=VECTOR('',#39606,10.);
#12332=VECTOR('',#39611,10.);
#12333=VECTOR('',#39612,10.);
#12334=VECTOR('',#39615,10.);
#12335=VECTOR('',#39620,10.);
#12336=VECTOR('',#39621,10.);
#12337=VECTOR('',#39624,10.);
#12338=VECTOR('',#39629,10.);
#12339=VECTOR('',#39630,10.);
#12340=VECTOR('',#39633,10.);
#12341=VECTOR('',#39638,10.);
#12342=VECTOR('',#39639,10.);
#12343=VECTOR('',#39642,10.);
#12344=VECTOR('',#39647,10.);
#12345=VECTOR('',#39648,10.);
#12346=VECTOR('',#39651,10.);
#12347=VECTOR('',#39656,10.);
#12348=VECTOR('',#39657,10.);
#12349=VECTOR('',#39660,10.);
#12350=VECTOR('',#39665,10.);
#12351=VECTOR('',#39666,10.);
#12352=VECTOR('',#39669,10.);
#12353=VECTOR('',#39674,10.);
#12354=VECTOR('',#39675,10.);
#12355=VECTOR('',#39678,10.);
#12356=VECTOR('',#39683,10.);
#12357=VECTOR('',#39684,10.);
#12358=VECTOR('',#39687,10.);
#12359=VECTOR('',#39692,10.);
#12360=VECTOR('',#39693,10.);
#12361=VECTOR('',#39696,10.);
#12362=VECTOR('',#39701,10.);
#12363=VECTOR('',#39702,10.);
#12364=VECTOR('',#39705,10.);
#12365=VECTOR('',#39710,10.);
#12366=VECTOR('',#39711,10.);
#12367=VECTOR('',#39714,10.);
#12368=VECTOR('',#39719,10.);
#12369=VECTOR('',#39720,10.);
#12370=VECTOR('',#39723,10.);
#12371=VECTOR('',#39728,10.);
#12372=VECTOR('',#39729,10.);
#12373=VECTOR('',#39732,10.);
#12374=VECTOR('',#39737,10.);
#12375=VECTOR('',#39738,10.);
#12376=VECTOR('',#39741,10.);
#12377=VECTOR('',#39746,10.);
#12378=VECTOR('',#39747,10.);
#12379=VECTOR('',#39750,10.);
#12380=VECTOR('',#39755,10.);
#12381=VECTOR('',#39756,10.);
#12382=VECTOR('',#39759,10.);
#12383=VECTOR('',#39764,10.);
#12384=VECTOR('',#39765,10.);
#12385=VECTOR('',#39768,10.);
#12386=VECTOR('',#39773,10.);
#12387=VECTOR('',#39774,9.99999999999999);
#12388=VECTOR('',#39777,10.);
#12389=VECTOR('',#39782,10.);
#12390=VECTOR('',#39783,10.);
#12391=VECTOR('',#39786,10.);
#12392=VECTOR('',#39791,10.);
#12393=VECTOR('',#39792,10.);
#12394=VECTOR('',#39795,10.);
#12395=VECTOR('',#39800,10.);
#12396=VECTOR('',#39801,10.);
#12397=VECTOR('',#39804,10.);
#12398=VECTOR('',#39809,10.);
#12399=VECTOR('',#39810,10.);
#12400=VECTOR('',#39813,10.);
#12401=VECTOR('',#39818,10.);
#12402=VECTOR('',#39819,10.);
#12403=VECTOR('',#39822,10.);
#12404=VECTOR('',#39827,10.);
#12405=VECTOR('',#39828,10.);
#12406=VECTOR('',#39831,10.);
#12407=VECTOR('',#39836,10.);
#12408=VECTOR('',#39837,10.);
#12409=VECTOR('',#39840,10.);
#12410=VECTOR('',#39845,9.99999999999999);
#12411=VECTOR('',#39846,10.);
#12412=VECTOR('',#39849,10.);
#12413=VECTOR('',#39854,10.);
#12414=VECTOR('',#39855,10.);
#12415=VECTOR('',#39858,10.);
#12416=VECTOR('',#39863,10.);
#12417=VECTOR('',#39864,10.);
#12418=VECTOR('',#39867,10.);
#12419=VECTOR('',#39872,10.);
#12420=VECTOR('',#39873,10.);
#12421=VECTOR('',#39876,10.);
#12422=VECTOR('',#39881,10.);
#12423=VECTOR('',#39882,10.);
#12424=VECTOR('',#39885,10.);
#12425=VECTOR('',#39890,10.);
#12426=VECTOR('',#39891,10.);
#12427=VECTOR('',#39894,10.);
#12428=VECTOR('',#39919,1.49337567297406);
#12429=VECTOR('',#39922,10.);
#12430=VECTOR('',#39923,10.);
#12431=VECTOR('',#39928,10.);
#12432=VECTOR('',#39931,10.);
#12433=VECTOR('',#39934,10.);
#12434=VECTOR('',#39935,10.);
#12435=VECTOR('',#39940,10.);
#12436=VECTOR('',#39943,10.);
#12437=VECTOR('',#39946,10.);
#12438=VECTOR('',#39947,10.);
#12439=VECTOR('',#39952,10.);
#12440=VECTOR('',#39955,10.);
#12441=VECTOR('',#39958,10.);
#12442=VECTOR('',#39959,10.);
#12443=VECTOR('',#39960,10.);
#12444=VECTOR('',#39961,10.);
#12445=VECTOR('',#39964,10.);
#12446=VECTOR('',#39965,10.);
#12447=VECTOR('',#39966,10.);
#12448=VECTOR('',#39969,10.);
#12449=VECTOR('',#39970,10.);
#12450=VECTOR('',#39971,10.);
#12451=VECTOR('',#39978,10.);
#12452=VECTOR('',#39983,10.);
#12453=VECTOR('',#39986,10.);
#12454=VECTOR('',#39989,10.);
#12455=VECTOR('',#39994,10.);
#12456=VECTOR('',#40011,10.);
#12457=VECTOR('',#40016,0.721687836487032);
#12458=VECTOR('',#40019,10.);
#12459=VECTOR('',#40020,10.);
#12460=VECTOR('',#40029,1.4635);
#12461=VECTOR('',#40034,1.4635);
#12462=VECTOR('',#40037,1.4635);
#12463=VECTOR('',#40040,1.4635);
#12464=VECTOR('',#40043,1.4635);
#12465=VECTOR('',#40046,1.4635);
#12466=VECTOR('',#40049,1.4635);
#12467=VECTOR('',#40052,1.4635);
#12468=VECTOR('',#40055,1.4635);
#12469=VECTOR('',#40058,1.4635);
#12470=VECTOR('',#40061,1.4635);
#12471=VECTOR('',#40064,1.4635);
#12472=VECTOR('',#40067,1.4635);
#12473=VECTOR('',#40070,1.4635);
#12474=VECTOR('',#40073,1.4635);
#12475=VECTOR('',#40076,1.4635);
#12476=VECTOR('',#40079,1.4635);
#12477=VECTOR('',#40082,1.4635);
#12478=VECTOR('',#40085,1.4635);
#12479=VECTOR('',#40088,1.17775);
#12480=VECTOR('',#40093,1.17775);
#12481=VECTOR('',#40096,1.17775);
#12482=VECTOR('',#40099,1.17775);
#12483=VECTOR('',#40102,1.17775);
#12484=VECTOR('',#40105,1.17775);
#12485=VECTOR('',#40108,1.17775);
#12486=VECTOR('',#40111,1.17775);
#12487=VECTOR('',#40114,1.17775);
#12488=VECTOR('',#40117,1.17775);
#12489=VECTOR('',#40120,1.17775);
#12490=VECTOR('',#40123,1.17775);
#12491=VECTOR('',#40126,1.17775);
#12492=VECTOR('',#40129,1.17775);
#12493=VECTOR('',#40132,1.17775);
#12494=VECTOR('',#40135,1.17775);
#12495=VECTOR('',#40138,1.17775);
#12496=VECTOR('',#40141,1.17775);
#12497=VECTOR('',#40144,1.17775);
#12498=VECTOR('',#40177,1.2885);
#12499=VECTOR('',#40186,10.);
#12500=VECTOR('',#40187,10.);
#12501=VECTOR('',#40190,10.);
#12502=VECTOR('',#40191,10.);
#12503=VECTOR('',#40194,10.);
#12504=VECTOR('',#40199,2.75);
#12505=VECTOR('',#40206,10.);
#12506=VECTOR('',#40209,10.);
#12507=VECTOR('',#40212,10.);
#12508=VECTOR('',#40215,10.);
#12509=VECTOR('',#40218,10.);
#12510=VECTOR('',#40221,10.);
#12511=VECTOR('',#40224,10.);
#12512=VECTOR('',#40227,10.);
#12513=VECTOR('',#40230,10.);
#12514=VECTOR('',#40233,10.);
#12515=VECTOR('',#40236,10.);
#12516=VECTOR('',#40239,10.);
#12517=VECTOR('',#40242,10.);
#12518=VECTOR('',#40245,10.);
#12519=VECTOR('',#40248,10.);
#12520=VECTOR('',#40251,10.);
#12521=VECTOR('',#40254,10.);
#12522=VECTOR('',#40257,10.);
#12523=VECTOR('',#40260,10.);
#12524=VECTOR('',#40263,10.);
#12525=VECTOR('',#40266,10.);
#12526=VECTOR('',#40269,10.);
#12527=VECTOR('',#40272,10.);
#12528=VECTOR('',#40275,10.);
#12529=VECTOR('',#40278,10.);
#12530=VECTOR('',#40281,10.);
#12531=VECTOR('',#40284,10.);
#12532=VECTOR('',#40287,10.);
#12533=VECTOR('',#40290,10.);
#12534=VECTOR('',#40293,10.);
#12535=VECTOR('',#40296,10.);
#12536=VECTOR('',#40299,10.);
#12537=VECTOR('',#40302,10.);
#12538=VECTOR('',#40307,10.);
#12539=VECTOR('',#40310,10.);
#12540=VECTOR('',#40313,10.);
#12541=VECTOR('',#40316,10.);
#12542=VECTOR('',#40319,10.);
#12543=VECTOR('',#40322,10.);
#12544=VECTOR('',#40325,10.);
#12545=VECTOR('',#40328,10.);
#12546=VECTOR('',#40331,10.);
#12547=VECTOR('',#40334,10.);
#12548=VECTOR('',#40337,10.);
#12549=VECTOR('',#40340,10.);
#12550=VECTOR('',#40343,10.);
#12551=VECTOR('',#40346,10.);
#12552=VECTOR('',#40349,10.);
#12553=VECTOR('',#40352,10.);
#12554=VECTOR('',#40355,10.);
#12555=VECTOR('',#40358,10.);
#12556=VECTOR('',#40361,10.);
#12557=VECTOR('',#40364,10.);
#12558=VECTOR('',#40367,10.);
#12559=VECTOR('',#40370,10.);
#12560=VECTOR('',#40373,10.);
#12561=VECTOR('',#40376,10.);
#12562=VECTOR('',#40379,10.);
#12563=VECTOR('',#40382,10.);
#12564=VECTOR('',#40385,10.);
#12565=VECTOR('',#40388,10.);
#12566=VECTOR('',#40391,10.);
#12567=VECTOR('',#40394,10.);
#12568=VECTOR('',#40397,10.);
#12569=VECTOR('',#40400,10.);
#12570=VECTOR('',#40403,10.);
#12571=VECTOR('',#40406,10.);
#12572=VECTOR('',#40409,10.);
#12573=VECTOR('',#40412,10.);
#12574=VECTOR('',#40415,10.);
#12575=VECTOR('',#40418,10.);
#12576=VECTOR('',#40419,10.);
#12577=VECTOR('',#40422,10.);
#12578=VECTOR('',#40427,2.6);
#12579=VECTOR('',#40432,10.);
#12580=VECTOR('',#40433,10.);
#12581=VECTOR('',#40436,10.);
#12582=VECTOR('',#40441,10.);
#12583=VECTOR('',#40442,10.);
#12584=VECTOR('',#40445,10.);
#12585=VECTOR('',#40450,10.);
#12586=VECTOR('',#40451,10.);
#12587=VECTOR('',#40454,10.);
#12588=VECTOR('',#40459,10.);
#12589=VECTOR('',#40460,10.);
#12590=VECTOR('',#40463,10.);
#12591=VECTOR('',#40468,10.);
#12592=VECTOR('',#40469,10.);
#12593=VECTOR('',#40472,10.);
#12594=VECTOR('',#40477,10.);
#12595=VECTOR('',#40478,10.);
#12596=VECTOR('',#40481,10.);
#12597=VECTOR('',#40486,10.);
#12598=VECTOR('',#40487,10.);
#12599=VECTOR('',#40490,10.);
#12600=VECTOR('',#40495,10.);
#12601=VECTOR('',#40496,10.);
#12602=VECTOR('',#40499,10.);
#12603=VECTOR('',#40504,10.);
#12604=VECTOR('',#40505,10.);
#12605=VECTOR('',#40508,10.);
#12606=VECTOR('',#40513,10.);
#12607=VECTOR('',#40514,10.);
#12608=VECTOR('',#40517,10.);
#12609=VECTOR('',#40522,10.);
#12610=VECTOR('',#40523,10.);
#12611=VECTOR('',#40526,10.);
#12612=VECTOR('',#40531,10.);
#12613=VECTOR('',#40532,10.);
#12614=VECTOR('',#40535,10.);
#12615=VECTOR('',#40540,10.);
#12616=VECTOR('',#40541,10.);
#12617=VECTOR('',#40544,10.);
#12618=VECTOR('',#40549,10.);
#12619=VECTOR('',#40550,10.);
#12620=VECTOR('',#40553,10.);
#12621=VECTOR('',#40558,10.);
#12622=VECTOR('',#40559,10.);
#12623=VECTOR('',#40562,10.);
#12624=VECTOR('',#40567,10.);
#12625=VECTOR('',#40568,10.);
#12626=VECTOR('',#40571,10.);
#12627=VECTOR('',#40576,10.);
#12628=VECTOR('',#40577,10.);
#12629=VECTOR('',#40580,10.);
#12630=VECTOR('',#40585,10.);
#12631=VECTOR('',#40586,10.);
#12632=VECTOR('',#40589,10.);
#12633=VECTOR('',#40594,10.);
#12634=VECTOR('',#40595,10.);
#12635=VECTOR('',#40598,10.);
#12636=VECTOR('',#40603,10.);
#12637=VECTOR('',#40604,10.);
#12638=VECTOR('',#40607,10.);
#12639=VECTOR('',#40612,10.);
#12640=VECTOR('',#40613,9.99999999999999);
#12641=VECTOR('',#40616,10.);
#12642=VECTOR('',#40621,10.);
#12643=VECTOR('',#40622,10.);
#12644=VECTOR('',#40625,10.);
#12645=VECTOR('',#40630,10.);
#12646=VECTOR('',#40631,10.);
#12647=VECTOR('',#40634,10.);
#12648=VECTOR('',#40639,10.);
#12649=VECTOR('',#40640,10.);
#12650=VECTOR('',#40643,10.);
#12651=VECTOR('',#40648,10.);
#12652=VECTOR('',#40649,10.);
#12653=VECTOR('',#40652,10.);
#12654=VECTOR('',#40657,10.);
#12655=VECTOR('',#40658,10.);
#12656=VECTOR('',#40661,10.);
#12657=VECTOR('',#40666,10.);
#12658=VECTOR('',#40667,10.);
#12659=VECTOR('',#40670,10.);
#12660=VECTOR('',#40675,10.);
#12661=VECTOR('',#40676,10.);
#12662=VECTOR('',#40679,10.);
#12663=VECTOR('',#40684,9.99999999999999);
#12664=VECTOR('',#40685,10.);
#12665=VECTOR('',#40688,10.);
#12666=VECTOR('',#40693,10.);
#12667=VECTOR('',#40694,10.);
#12668=VECTOR('',#40697,10.);
#12669=VECTOR('',#40702,10.);
#12670=VECTOR('',#40703,10.);
#12671=VECTOR('',#40706,10.);
#12672=VECTOR('',#40711,10.);
#12673=VECTOR('',#40712,10.);
#12674=VECTOR('',#40715,10.);
#12675=VECTOR('',#40720,10.);
#12676=VECTOR('',#40721,10.);
#12677=VECTOR('',#40724,10.);
#12678=VECTOR('',#40729,10.);
#12679=VECTOR('',#40730,10.);
#12680=VECTOR('',#40733,10.);
#12681=VECTOR('',#40758,1.49337567297406);
#12682=VECTOR('',#40761,10.);
#12683=VECTOR('',#40762,10.);
#12684=VECTOR('',#40767,10.);
#12685=VECTOR('',#40770,10.);
#12686=VECTOR('',#40773,10.);
#12687=VECTOR('',#40774,10.);
#12688=VECTOR('',#40779,10.);
#12689=VECTOR('',#40782,10.);
#12690=VECTOR('',#40785,10.);
#12691=VECTOR('',#40786,10.);
#12692=VECTOR('',#40791,10.);
#12693=VECTOR('',#40794,10.);
#12694=VECTOR('',#40797,10.);
#12695=VECTOR('',#40798,10.);
#12696=VECTOR('',#40799,10.);
#12697=VECTOR('',#40800,10.);
#12698=VECTOR('',#40803,10.);
#12699=VECTOR('',#40804,10.);
#12700=VECTOR('',#40805,10.);
#12701=VECTOR('',#40808,10.);
#12702=VECTOR('',#40809,10.);
#12703=VECTOR('',#40810,10.);
#12704=VECTOR('',#40817,10.);
#12705=VECTOR('',#40822,10.);
#12706=VECTOR('',#40825,10.);
#12707=VECTOR('',#40828,10.);
#12708=VECTOR('',#40833,10.);
#12709=VECTOR('',#40850,10.);
#12710=VECTOR('',#40855,0.721687836487032);
#12711=VECTOR('',#40858,10.);
#12712=VECTOR('',#40859,10.);
#12713=VECTOR('',#40868,0.96675);
#12714=VECTOR('',#40873,0.96675);
#12715=VECTOR('',#40876,0.96675);
#12716=VECTOR('',#40879,0.96675);
#12717=VECTOR('',#40882,0.96675);
#12718=VECTOR('',#40885,0.96675);
#12719=VECTOR('',#40888,0.96675);
#12720=VECTOR('',#40891,0.96675);
#12721=VECTOR('',#40894,0.96675);
#12722=VECTOR('',#40897,0.96675);
#12723=VECTOR('',#40900,0.96675);
#12724=VECTOR('',#40903,0.739000000000001);
#12725=VECTOR('',#40908,0.739000000000001);
#12726=VECTOR('',#40911,0.739000000000001);
#12727=VECTOR('',#40914,0.739000000000001);
#12728=VECTOR('',#40917,0.739000000000001);
#12729=VECTOR('',#40920,0.739000000000001);
#12730=VECTOR('',#40923,0.739000000000001);
#12731=VECTOR('',#40926,0.739000000000001);
#12732=VECTOR('',#40929,0.739000000000001);
#12733=VECTOR('',#40932,0.739000000000001);
#12734=VECTOR('',#40961,10.);
#12735=VECTOR('',#40964,10.);
#12736=VECTOR('',#40969,10.);
#12737=VECTOR('',#40970,10.);
#12738=VECTOR('',#40971,10.);
#12739=VECTOR('',#40974,10.);
#12740=VECTOR('',#40975,10.);
#12741=VECTOR('',#40976,10.);
#12742=VECTOR('',#40979,1.9);
#12743=VECTOR('',#41000,0.825);
#12744=CIRCLE('',#32235,1.55);
#12745=CIRCLE('',#32236,1.75);
#12746=CIRCLE('',#32238,1.75);
#12747=CIRCLE('',#32240,1.55);
#12748=CIRCLE('',#32242,1.55);
#12749=CIRCLE('',#32244,1.55);
#12750=CIRCLE('',#32248,1.55);
#12751=CIRCLE('',#32249,1.75);
#12752=CIRCLE('',#32251,1.75);
#12753=CIRCLE('',#32253,1.55);
#12754=CIRCLE('',#32255,1.55);
#12755=CIRCLE('',#32257,1.55);
#12756=CIRCLE('',#32278,1.05);
#12757=CIRCLE('',#32279,1.2);
#12758=CIRCLE('',#32281,1.2);
#12759=CIRCLE('',#32283,1.05);
#12760=CIRCLE('',#32284,1.05);
#12761=CIRCLE('',#32286,1.05);
#12762=CIRCLE('',#32288,1.05);
#12763=CIRCLE('',#32289,1.05);
#12764=CIRCLE('',#32293,1.05);
#12765=CIRCLE('',#32294,1.2);
#12766=CIRCLE('',#32296,1.2);
#12767=CIRCLE('',#32297,1.2);
#12768=CIRCLE('',#32298,2.35);
#12769=CIRCLE('',#32299,2.35);
#12770=CIRCLE('',#32300,2.35);
#12771=CIRCLE('',#32301,2.35);
#12772=CIRCLE('',#32302,2.35);
#12773=CIRCLE('',#32303,2.35);
#12774=CIRCLE('',#32304,1.2);
#12775=CIRCLE('',#32306,1.05);
#12776=CIRCLE('',#32308,1.05);
#12777=CIRCLE('',#32310,1.05);
#12778=CIRCLE('',#32312,1.05);
#12779=CIRCLE('',#32314,1.05);
#12780=CIRCLE('',#32316,1.05);
#12781=CIRCLE('',#32318,1.05);
#12782=CIRCLE('',#32324,2.05);
#12783=CIRCLE('',#32326,2.05);
#12784=CIRCLE('',#32328,2.05);
#12785=CIRCLE('',#32330,2.05);
#12786=CIRCLE('',#32332,2.05);
#12787=CIRCLE('',#32334,2.05);
#12788=CIRCLE('',#32336,2.05);
#12789=CIRCLE('',#32338,2.05);
#12790=CIRCLE('',#32340,2.05);
#12791=CIRCLE('',#32342,2.05);
#12792=CIRCLE('',#32344,2.05);
#12793=CIRCLE('',#32346,2.05);
#12794=CIRCLE('',#32354,3.);
#12795=CIRCLE('',#32355,3.);
#12796=CIRCLE('',#32359,3.);
#12797=CIRCLE('',#32360,3.);
#12798=CIRCLE('',#32362,4.5);
#12799=CIRCLE('',#32364,4.5);
#12800=CIRCLE('',#32366,4.5);
#12801=CIRCLE('',#32367,4.5);
#12802=CIRCLE('',#32368,4.5);
#12803=CIRCLE('',#32369,4.5);
#12804=CIRCLE('',#32386,2.525);
#12805=CIRCLE('',#32387,2.825);
#12806=CIRCLE('',#32388,2.525);
#12807=CIRCLE('',#32390,2.525);
#12808=CIRCLE('',#32391,2.525);
#12809=CIRCLE('',#32393,4.2);
#12810=CIRCLE('',#32395,2.825);
#12811=CIRCLE('',#32397,4.2);
#12812=CIRCLE('',#32399,4.5);
#12813=CIRCLE('',#32401,4.5);
#12814=CIRCLE('',#32405,2.5);
#12815=CIRCLE('',#32452,2.5);
#12816=CIRCLE('',#32455,2.);
#12817=CIRCLE('',#32457,2.);
#12818=CIRCLE('',#32462,1.7);
#12819=CIRCLE('',#32464,2.);
#12820=CIRCLE('',#32466,2.);
#12821=CIRCLE('',#32469,2.2);
#12822=CIRCLE('',#32471,2.);
#12823=CIRCLE('',#32473,2.);
#12824=CIRCLE('',#32475,1.7);
#12825=CIRCLE('',#32502,7.5);
#12826=CIRCLE('',#32504,7.5);
#12827=CIRCLE('',#32507,7.5);
#12828=CIRCLE('',#32510,7.5);
#12829=CIRCLE('',#32513,7.5);
#12830=CIRCLE('',#32516,7.5);
#12831=CIRCLE('',#32519,7.5);
#12832=CIRCLE('',#32522,7.5);
#12833=CIRCLE('',#32525,7.5);
#12834=CIRCLE('',#32528,7.5);
#12835=CIRCLE('',#32531,7.5);
#12836=CIRCLE('',#32534,7.5);
#12837=CIRCLE('',#32537,7.5);
#12838=CIRCLE('',#32540,7.5);
#12839=CIRCLE('',#32543,7.5);
#12840=CIRCLE('',#32546,7.5);
#12841=CIRCLE('',#32549,7.5);
#12842=CIRCLE('',#32552,7.5);
#12843=CIRCLE('',#32555,7.5);
#12844=CIRCLE('',#32558,7.5);
#12845=CIRCLE('',#32561,7.5);
#12846=CIRCLE('',#32564,7.5);
#12847=CIRCLE('',#32567,7.5);
#12848=CIRCLE('',#32570,7.5);
#12849=CIRCLE('',#32573,7.5);
#12850=CIRCLE('',#32576,7.5);
#12851=CIRCLE('',#32579,7.5);
#12852=CIRCLE('',#32582,7.5);
#12853=CIRCLE('',#32585,7.5);
#12854=CIRCLE('',#32588,7.5);
#12855=CIRCLE('',#32591,7.5);
#12856=CIRCLE('',#32594,7.5);
#12857=CIRCLE('',#32597,7.5);
#12858=CIRCLE('',#32600,7.5);
#12859=CIRCLE('',#32603,7.5);
#12860=CIRCLE('',#32606,7.5);
#12861=CIRCLE('',#32609,7.5);
#12862=CIRCLE('',#32612,7.5);
#12863=CIRCLE('',#32615,7.5);
#12864=CIRCLE('',#32616,7.5);
#12865=CIRCLE('',#32619,7.5);
#12866=CIRCLE('',#32620,7.5);
#12867=CIRCLE('',#32623,7.5);
#12868=CIRCLE('',#32626,7.5);
#12869=CIRCLE('',#32629,7.5);
#12870=CIRCLE('',#32632,7.5);
#12871=CIRCLE('',#32635,7.5);
#12872=CIRCLE('',#32638,7.5);
#12873=CIRCLE('',#32641,7.5);
#12874=CIRCLE('',#32644,7.5);
#12875=CIRCLE('',#32647,7.5);
#12876=CIRCLE('',#32650,7.5);
#12877=CIRCLE('',#32653,7.5);
#12878=CIRCLE('',#32656,7.5);
#12879=CIRCLE('',#32659,7.5);
#12880=CIRCLE('',#32662,7.5);
#12881=CIRCLE('',#32665,7.5);
#12882=CIRCLE('',#32668,7.5);
#12883=CIRCLE('',#32671,7.5);
#12884=CIRCLE('',#32674,7.5);
#12885=CIRCLE('',#32677,7.5);
#12886=CIRCLE('',#32680,7.5);
#12887=CIRCLE('',#32683,7.5);
#12888=CIRCLE('',#32686,7.5);
#12889=CIRCLE('',#32689,7.5);
#12890=CIRCLE('',#32692,7.5);
#12891=CIRCLE('',#32695,7.5);
#12892=CIRCLE('',#32698,7.5);
#12893=CIRCLE('',#32701,7.5);
#12894=CIRCLE('',#32704,7.5);
#12895=CIRCLE('',#32707,7.5);
#12896=CIRCLE('',#32710,7.5);
#12897=CIRCLE('',#32713,7.5);
#12898=CIRCLE('',#32716,7.5);
#12899=CIRCLE('',#32719,7.5);
#12900=CIRCLE('',#32722,7.5);
#12901=CIRCLE('',#32725,7.5);
#12902=CIRCLE('',#32728,7.5);
#12903=CIRCLE('',#32731,7.5);
#12904=CIRCLE('',#32734,7.5);
#12905=CIRCLE('',#32736,7.5);
#12906=CIRCLE('',#32738,7.5);
#12907=CIRCLE('',#32740,2.01);
#12908=CIRCLE('',#32741,5.8);
#12909=CIRCLE('',#32743,6.9);
#12910=CIRCLE('',#32745,7.5);
#12911=CIRCLE('',#32747,7.5);
#12912=CIRCLE('',#32749,7.1);
#12913=CIRCLE('',#32751,2.8);
#12914=CIRCLE('',#32753,2.8);
#12915=CIRCLE('',#32755,2.01);
#12916=CIRCLE('',#33264,1.1);
#12917=CIRCLE('',#33265,1.1);
#12918=CIRCLE('',#33267,1.1);
#12919=CIRCLE('',#33268,1.1);
#12920=CIRCLE('',#33271,0.799999999999998);
#12921=CIRCLE('',#33272,0.799999999999998);
#12922=CIRCLE('',#33275,0.800000000000018);
#12923=CIRCLE('',#33276,0.800000000000018);
#12924=CIRCLE('',#33279,0.800000000000025);
#12925=CIRCLE('',#33280,0.800000000000025);
#12926=CIRCLE('',#33283,0.799999999999996);
#12927=CIRCLE('',#33284,0.799999999999996);
#12928=CIRCLE('',#33344,1.1);
#12929=CIRCLE('',#33345,1.1);
#12930=CIRCLE('',#33347,1.1);
#12931=CIRCLE('',#33348,1.1);
#12932=CIRCLE('',#33361,3.3);
#12933=CIRCLE('',#33362,3.);
#12934=CIRCLE('',#33364,3.3);
#12935=CIRCLE('',#33365,2.25);
#12936=CIRCLE('',#33366,2.25);
#12937=CIRCLE('',#33367,2.25);
#12938=CIRCLE('',#33368,2.25);
#12939=CIRCLE('',#33370,3.);
#12940=CIRCLE('',#33373,3.);
#12941=CIRCLE('',#33375,1.7);
#12942=CIRCLE('',#33377,3.);
#12943=CIRCLE('',#33379,1.7);
#12944=CIRCLE('',#33381,1.7);
#12945=CIRCLE('',#33383,1.7);
#12946=CIRCLE('',#33385,1.7);
#12947=CIRCLE('',#33387,1.7);
#12948=CIRCLE('',#33392,2.25);
#12949=CIRCLE('',#33393,2.25);
#12950=CIRCLE('',#33396,2.25);
#12951=CIRCLE('',#33400,2.25);
#12952=CIRCLE('',#33401,2.25);
#12953=CIRCLE('',#33404,2.25);
#12954=CIRCLE('',#33414,1.4635);
#12955=CIRCLE('',#33424,1.17775);
#12956=CIRCLE('',#33433,1.17775);
#12957=CIRCLE('',#33435,1.4635);
#12958=CIRCLE('',#33437,1.4635);
#12959=CIRCLE('',#33438,1.4635);
#12960=CIRCLE('',#33440,1.4635);
#12961=CIRCLE('',#33441,1.4635);
#12962=CIRCLE('',#33443,0.816025403784426);
#12963=CIRCLE('',#33444,0.816025403784426);
#12964=CIRCLE('',#33445,0.816025403784426);
#12965=CIRCLE('',#33446,0.816025403784426);
#12966=CIRCLE('',#33447,0.816025403784426);
#12967=CIRCLE('',#33448,0.816025403784426);
#12968=CIRCLE('',#33449,1.01602540378442);
#12969=CIRCLE('',#33451,0.816025403784426);
#12970=CIRCLE('',#33453,0.816025403784426);
#12971=CIRCLE('',#33455,0.816025403784426);
#12972=CIRCLE('',#33457,0.816025403784426);
#12973=CIRCLE('',#33459,0.816025403784426);
#12974=CIRCLE('',#33461,0.816025403784426);
#12975=CIRCLE('',#33472,0.866025403784452);
#12976=CIRCLE('',#33474,0.866025403784452);
#12977=CIRCLE('',#33476,0.866025403784452);
#12978=CIRCLE('',#33478,0.866025403784452);
#12979=CIRCLE('',#33480,0.866025403784452);
#12980=CIRCLE('',#33482,0.866025403784452);
#12981=CIRCLE('',#33488,0.999999999999996);
#12982=CIRCLE('',#33491,1.19999999999999);
#12983=CIRCLE('',#33495,1.05);
#12984=CIRCLE('',#33496,1.2);
#12985=CIRCLE('',#33498,1.05);
#12986=CIRCLE('',#33499,1.05);
#12987=CIRCLE('',#33503,1.05);
#12988=CIRCLE('',#33504,1.2);
#12989=CIRCLE('',#33506,1.05);
#12990=CIRCLE('',#33507,1.05);
#12991=CIRCLE('',#33511,1.55);
#12992=CIRCLE('',#33512,1.75);
#12993=CIRCLE('',#33514,1.75);
#12994=CIRCLE('',#33515,3.3);
#12995=CIRCLE('',#33516,2.315);
#12996=CIRCLE('',#33517,3.3);
#12997=CIRCLE('',#33519,1.55);
#12998=CIRCLE('',#33521,1.55);
#12999=CIRCLE('',#33523,1.55);
#13000=CIRCLE('',#33527,3.);
#13001=CIRCLE('',#33529,3.);
#13002=CIRCLE('',#33531,3.);
#13003=CIRCLE('',#33533,3.);
#13004=CIRCLE('',#33535,1.7);
#13005=CIRCLE('',#33537,1.7);
#13006=CIRCLE('',#33539,1.7);
#13007=CIRCLE('',#33541,1.7);
#13008=CIRCLE('',#33543,2.015);
#13009=CIRCLE('',#33544,2.315);
#13010=CIRCLE('',#33546,2.015);
#13011=CIRCLE('',#33557,1.4635);
#13012=CIRCLE('',#33581,1.17775);
#13013=CIRCLE('',#33605,1.17775);
#13014=CIRCLE('',#33607,1.4635);
#13015=CIRCLE('',#33609,1.4635);
#13016=CIRCLE('',#33610,1.4635);
#13017=CIRCLE('',#33612,1.4635);
#13018=CIRCLE('',#33613,1.4635);
#13019=CIRCLE('',#33615,1.5635);
#13020=CIRCLE('',#33616,0.1);
#13021=CIRCLE('',#33618,2.55);
#13022=CIRCLE('',#33620,1.1135);
#13023=CIRCLE('',#33623,2.75);
#13024=CIRCLE('',#33627,2.75);
#13025=CIRCLE('',#33628,2.75);
#13026=CIRCLE('',#33629,2.75);
#13027=CIRCLE('',#33630,2.75);
#13028=CIRCLE('',#33631,2.75);
#13029=CIRCLE('',#33632,2.75);
#13030=CIRCLE('',#33633,2.75);
#13031=CIRCLE('',#33634,2.75);
#13032=CIRCLE('',#33635,2.75);
#13033=CIRCLE('',#33636,2.75);
#13034=CIRCLE('',#33637,2.75);
#13035=CIRCLE('',#33638,2.75);
#13036=CIRCLE('',#33639,2.75);
#13037=CIRCLE('',#33640,2.75);
#13038=CIRCLE('',#33641,2.75);
#13039=CIRCLE('',#33642,2.75);
#13040=CIRCLE('',#33643,2.75);
#13041=CIRCLE('',#33644,2.75);
#13042=CIRCLE('',#33645,2.75);
#13043=CIRCLE('',#33646,2.75);
#13044=CIRCLE('',#33647,2.75);
#13045=CIRCLE('',#33648,2.75);
#13046=CIRCLE('',#33649,2.75);
#13047=CIRCLE('',#33650,2.75);
#13048=CIRCLE('',#33651,2.75);
#13049=CIRCLE('',#33652,2.75);
#13050=CIRCLE('',#33653,2.75);
#13051=CIRCLE('',#33654,2.75);
#13052=CIRCLE('',#33655,2.75);
#13053=CIRCLE('',#33656,2.75);
#13054=CIRCLE('',#33657,2.75);
#13055=CIRCLE('',#33658,2.75);
#13056=CIRCLE('',#33659,2.75);
#13057=CIRCLE('',#33660,2.75);
#13058=CIRCLE('',#33661,2.75);
#13059=CIRCLE('',#33662,2.75);
#13060=CIRCLE('',#33663,2.75);
#13061=CIRCLE('',#33664,2.75);
#13062=CIRCLE('',#33665,2.75);
#13063=CIRCLE('',#33666,2.75);
#13064=CIRCLE('',#33667,2.75);
#13065=CIRCLE('',#33668,2.75);
#13066=CIRCLE('',#33669,2.75);
#13067=CIRCLE('',#33670,2.75);
#13068=CIRCLE('',#33671,2.75);
#13069=CIRCLE('',#33672,2.75);
#13070=CIRCLE('',#33673,2.75);
#13071=CIRCLE('',#33674,2.75);
#13072=CIRCLE('',#33675,2.75);
#13073=CIRCLE('',#33676,2.75);
#13074=CIRCLE('',#33677,2.75);
#13075=CIRCLE('',#33678,2.75);
#13076=CIRCLE('',#33679,2.75);
#13077=CIRCLE('',#33680,2.75);
#13078=CIRCLE('',#33681,2.75);
#13079=CIRCLE('',#33682,2.75);
#13080=CIRCLE('',#33683,2.75);
#13081=CIRCLE('',#33684,2.75);
#13082=CIRCLE('',#33685,2.75);
#13083=CIRCLE('',#33686,2.75);
#13084=CIRCLE('',#33687,2.75);
#13085=CIRCLE('',#33688,2.75);
#13086=CIRCLE('',#33689,2.75);
#13087=CIRCLE('',#33690,2.75);
#13088=CIRCLE('',#33691,2.75);
#13089=CIRCLE('',#33692,2.75);
#13090=CIRCLE('',#33693,2.75);
#13091=CIRCLE('',#33694,2.75);
#13092=CIRCLE('',#33695,2.75);
#13093=CIRCLE('',#33696,2.75);
#13094=CIRCLE('',#33697,2.75);
#13095=CIRCLE('',#33698,2.75);
#13096=CIRCLE('',#33699,2.75);
#13097=CIRCLE('',#33700,2.75);
#13098=CIRCLE('',#33705,2.45);
#13099=CIRCLE('',#33809,0.2);
#13100=CIRCLE('',#33811,1.59337567297406);
#13101=CIRCLE('',#33813,1.39337567297406);
#13102=CIRCLE('',#33814,1.39337567297406);
#13103=CIRCLE('',#33815,1.39337567297406);
#13104=CIRCLE('',#33816,1.39337567297406);
#13105=CIRCLE('',#33817,1.39337567297406);
#13106=CIRCLE('',#33818,1.39337567297406);
#13107=CIRCLE('',#33820,1.39337567297406);
#13108=CIRCLE('',#33822,1.39337567297406);
#13109=CIRCLE('',#33824,1.39337567297406);
#13110=CIRCLE('',#33826,1.39337567297406);
#13111=CIRCLE('',#33828,1.39337567297406);
#13112=CIRCLE('',#33830,1.39337567297406);
#13113=CIRCLE('',#33841,1.44337567297406);
#13114=CIRCLE('',#33843,1.44337567297406);
#13115=CIRCLE('',#33845,1.44337567297406);
#13116=CIRCLE('',#33847,1.44337567297406);
#13117=CIRCLE('',#33849,1.44337567297406);
#13118=CIRCLE('',#33851,1.44337567297406);
#13119=CIRCLE('',#33858,1.4635);
#13120=CIRCLE('',#33878,1.17775);
#13121=CIRCLE('',#33898,1.17775);
#13122=CIRCLE('',#33900,1.4635);
#13123=CIRCLE('',#33902,1.4635);
#13124=CIRCLE('',#33903,1.4635);
#13125=CIRCLE('',#33905,1.4635);
#13126=CIRCLE('',#33906,1.4635);
#13127=CIRCLE('',#33908,1.5635);
#13128=CIRCLE('',#33909,0.1);
#13129=CIRCLE('',#33911,2.55);
#13130=CIRCLE('',#33913,1.1135);
#13131=CIRCLE('',#33916,2.75);
#13132=CIRCLE('',#33920,2.75);
#13133=CIRCLE('',#33921,2.75);
#13134=CIRCLE('',#33922,2.75);
#13135=CIRCLE('',#33923,2.75);
#13136=CIRCLE('',#33924,2.75);
#13137=CIRCLE('',#33925,2.75);
#13138=CIRCLE('',#33926,2.75);
#13139=CIRCLE('',#33927,2.75);
#13140=CIRCLE('',#33928,2.75);
#13141=CIRCLE('',#33929,2.75);
#13142=CIRCLE('',#33930,2.75);
#13143=CIRCLE('',#33931,2.75);
#13144=CIRCLE('',#33932,2.75);
#13145=CIRCLE('',#33933,2.75);
#13146=CIRCLE('',#33934,2.75);
#13147=CIRCLE('',#33935,2.75);
#13148=CIRCLE('',#33936,2.75);
#13149=CIRCLE('',#33937,2.75);
#13150=CIRCLE('',#33938,2.75);
#13151=CIRCLE('',#33939,2.75);
#13152=CIRCLE('',#33940,2.75);
#13153=CIRCLE('',#33941,2.75);
#13154=CIRCLE('',#33942,2.75);
#13155=CIRCLE('',#33943,2.75);
#13156=CIRCLE('',#33944,2.75);
#13157=CIRCLE('',#33945,2.75);
#13158=CIRCLE('',#33946,2.75);
#13159=CIRCLE('',#33947,2.75);
#13160=CIRCLE('',#33948,2.75);
#13161=CIRCLE('',#33949,2.75);
#13162=CIRCLE('',#33950,2.75);
#13163=CIRCLE('',#33951,2.75);
#13164=CIRCLE('',#33952,2.75);
#13165=CIRCLE('',#33953,2.75);
#13166=CIRCLE('',#33954,2.75);
#13167=CIRCLE('',#33955,2.75);
#13168=CIRCLE('',#33956,2.75);
#13169=CIRCLE('',#33957,2.75);
#13170=CIRCLE('',#33958,2.75);
#13171=CIRCLE('',#33959,2.75);
#13172=CIRCLE('',#33960,2.75);
#13173=CIRCLE('',#33961,2.75);
#13174=CIRCLE('',#33962,2.75);
#13175=CIRCLE('',#33963,2.75);
#13176=CIRCLE('',#33964,2.75);
#13177=CIRCLE('',#33965,2.75);
#13178=CIRCLE('',#33966,2.75);
#13179=CIRCLE('',#33967,2.75);
#13180=CIRCLE('',#33968,2.75);
#13181=CIRCLE('',#33969,2.75);
#13182=CIRCLE('',#33970,2.75);
#13183=CIRCLE('',#33971,2.75);
#13184=CIRCLE('',#33972,2.75);
#13185=CIRCLE('',#33973,2.75);
#13186=CIRCLE('',#33974,2.75);
#13187=CIRCLE('',#33975,2.75);
#13188=CIRCLE('',#33976,2.75);
#13189=CIRCLE('',#33977,2.75);
#13190=CIRCLE('',#33978,2.75);
#13191=CIRCLE('',#33979,2.75);
#13192=CIRCLE('',#33980,2.75);
#13193=CIRCLE('',#33981,2.75);
#13194=CIRCLE('',#33982,2.75);
#13195=CIRCLE('',#33983,2.75);
#13196=CIRCLE('',#33984,2.75);
#13197=CIRCLE('',#33985,2.75);
#13198=CIRCLE('',#33986,2.75);
#13199=CIRCLE('',#33987,2.75);
#13200=CIRCLE('',#33988,2.75);
#13201=CIRCLE('',#33989,2.75);
#13202=CIRCLE('',#33990,2.75);
#13203=CIRCLE('',#33991,2.75);
#13204=CIRCLE('',#33992,2.75);
#13205=CIRCLE('',#33993,2.75);
#13206=CIRCLE('',#33998,2.45);
#13207=CIRCLE('',#34102,0.2);
#13208=CIRCLE('',#34104,1.59337567297406);
#13209=CIRCLE('',#34106,1.39337567297406);
#13210=CIRCLE('',#34107,1.39337567297406);
#13211=CIRCLE('',#34108,1.39337567297406);
#13212=CIRCLE('',#34109,1.39337567297406);
#13213=CIRCLE('',#34110,1.39337567297406);
#13214=CIRCLE('',#34111,1.39337567297406);
#13215=CIRCLE('',#34113,1.39337567297406);
#13216=CIRCLE('',#34115,1.39337567297406);
#13217=CIRCLE('',#34117,1.39337567297406);
#13218=CIRCLE('',#34119,1.39337567297406);
#13219=CIRCLE('',#34121,1.39337567297406);
#13220=CIRCLE('',#34123,1.39337567297406);
#13221=CIRCLE('',#34134,1.44337567297406);
#13222=CIRCLE('',#34136,1.44337567297406);
#13223=CIRCLE('',#34138,1.44337567297406);
#13224=CIRCLE('',#34140,1.44337567297406);
#13225=CIRCLE('',#34142,1.44337567297406);
#13226=CIRCLE('',#34144,1.44337567297406);
#13227=CIRCLE('',#34151,0.96675);
#13228=CIRCLE('',#34163,0.739000000000001);
#13229=CIRCLE('',#34174,0.739000000000001);
#13230=CIRCLE('',#34176,0.96675);
#13231=CIRCLE('',#34178,0.96675);
#13232=CIRCLE('',#34179,0.96675);
#13233=CIRCLE('',#34181,1.06675);
#13234=CIRCLE('',#34182,0.1);
#13235=CIRCLE('',#34184,1.9);
#13236=CIRCLE('',#34186,1.9);
#13237=CIRCLE('',#34187,1.9);
#13238=CIRCLE('',#34188,1.9);
#13239=CIRCLE('',#34192,1.9);
#13240=CIRCLE('',#34193,1.9);
#13241=CIRCLE('',#34195,1.5);
#13242=CIRCLE('',#34197,1.5);
#13243=CIRCLE('',#34200,0.649999999999999);
#13244=VERTEX_POINT('',#41048);
#13245=VERTEX_POINT('',#41050);
#13246=VERTEX_POINT('',#41054);
#13247=VERTEX_POINT('',#41055);
#13248=VERTEX_POINT('',#41057);
#13249=VERTEX_POINT('',#41059);
#13250=VERTEX_POINT('',#41061);
#13251=VERTEX_POINT('',#41063);
#13252=VERTEX_POINT('',#41065);
#13253=VERTEX_POINT('',#41067);
#13254=VERTEX_POINT('',#41069);
#13255=VERTEX_POINT('',#41071);
#13256=VERTEX_POINT('',#41073);
#13257=VERTEX_POINT('',#41075);
#13258=VERTEX_POINT('',#41077);
#13259=VERTEX_POINT('',#41079);
#13260=VERTEX_POINT('',#41081);
#13261=VERTEX_POINT('',#41083);
#13262=VERTEX_POINT('',#41086);
#13263=VERTEX_POINT('',#41089);
#13264=VERTEX_POINT('',#41093);
#13265=VERTEX_POINT('',#41097);
#13266=VERTEX_POINT('',#41101);
#13267=VERTEX_POINT('',#41104);
#13268=VERTEX_POINT('',#41107);
#13269=VERTEX_POINT('',#41109);
#13270=VERTEX_POINT('',#41113);
#13271=VERTEX_POINT('',#41114);
#13272=VERTEX_POINT('',#41116);
#13273=VERTEX_POINT('',#41118);
#13274=VERTEX_POINT('',#41120);
#13275=VERTEX_POINT('',#41122);
#13276=VERTEX_POINT('',#41124);
#13277=VERTEX_POINT('',#41126);
#13278=VERTEX_POINT('',#41128);
#13279=VERTEX_POINT('',#41130);
#13280=VERTEX_POINT('',#41132);
#13281=VERTEX_POINT('',#41134);
#13282=VERTEX_POINT('',#41136);
#13283=VERTEX_POINT('',#41138);
#13284=VERTEX_POINT('',#41140);
#13285=VERTEX_POINT('',#41142);
#13286=VERTEX_POINT('',#41145);
#13287=VERTEX_POINT('',#41148);
#13288=VERTEX_POINT('',#41152);
#13289=VERTEX_POINT('',#41156);
#13290=VERTEX_POINT('',#41160);
#13291=VERTEX_POINT('',#41163);
#13292=VERTEX_POINT('',#41199);
#13293=VERTEX_POINT('',#41201);
#13294=VERTEX_POINT('',#41205);
#13295=VERTEX_POINT('',#41206);
#13296=VERTEX_POINT('',#41208);
#13297=VERTEX_POINT('',#41210);
#13298=VERTEX_POINT('',#41213);
#13299=VERTEX_POINT('',#41216);
#13300=VERTEX_POINT('',#41218);
#13301=VERTEX_POINT('',#41222);
#13302=VERTEX_POINT('',#41226);
#13303=VERTEX_POINT('',#41228);
#13304=VERTEX_POINT('',#41232);
#13305=VERTEX_POINT('',#41235);
#13306=VERTEX_POINT('',#41238);
#13307=VERTEX_POINT('',#41240);
#13308=VERTEX_POINT('',#41244);
#13309=VERTEX_POINT('',#41245);
#13310=VERTEX_POINT('',#41247);
#13311=VERTEX_POINT('',#41249);
#13312=VERTEX_POINT('',#41252);
#13313=VERTEX_POINT('',#41254);
#13314=VERTEX_POINT('',#41256);
#13315=VERTEX_POINT('',#41258);
#13316=VERTEX_POINT('',#41260);
#13317=VERTEX_POINT('',#41262);
#13318=VERTEX_POINT('',#41264);
#13319=VERTEX_POINT('',#41266);
#13320=VERTEX_POINT('',#41268);
#13321=VERTEX_POINT('',#41271);
#13322=VERTEX_POINT('',#41275);
#13323=VERTEX_POINT('',#41279);
#13324=VERTEX_POINT('',#41283);
#13325=VERTEX_POINT('',#41287);
#13326=VERTEX_POINT('',#41291);
#13327=VERTEX_POINT('',#41295);
#13328=VERTEX_POINT('',#41299);
#13329=VERTEX_POINT('',#41302);
#13330=VERTEX_POINT('',#41305);
#13331=VERTEX_POINT('',#41308);
#13332=VERTEX_POINT('',#41311);
#13333=VERTEX_POINT('',#41315);
#13334=VERTEX_POINT('',#41319);
#13335=VERTEX_POINT('',#41323);
#13336=VERTEX_POINT('',#41327);
#13337=VERTEX_POINT('',#41331);
#13338=VERTEX_POINT('',#41335);
#13339=VERTEX_POINT('',#41339);
#13340=VERTEX_POINT('',#41343);
#13341=VERTEX_POINT('',#41347);
#13342=VERTEX_POINT('',#41351);
#13343=VERTEX_POINT('',#41355);
#13344=VERTEX_POINT('',#41359);
#13345=VERTEX_POINT('',#41362);
#13346=VERTEX_POINT('',#41365);
#13347=VERTEX_POINT('',#41368);
#13348=VERTEX_POINT('',#41371);
#13349=VERTEX_POINT('',#41374);
#13350=VERTEX_POINT('',#41377);
#13351=VERTEX_POINT('',#41378);
#13352=VERTEX_POINT('',#41380);
#13353=VERTEX_POINT('',#41382);
#13354=VERTEX_POINT('',#41386);
#13355=VERTEX_POINT('',#41388);
#13356=VERTEX_POINT('',#41393);
#13357=VERTEX_POINT('',#41395);
#13358=VERTEX_POINT('',#41397);
#13359=VERTEX_POINT('',#41399);
#13360=VERTEX_POINT('',#41401);
#13361=VERTEX_POINT('',#41403);
#13362=VERTEX_POINT('',#41405);
#13363=VERTEX_POINT('',#41409);
#13364=VERTEX_POINT('',#41410);
#13365=VERTEX_POINT('',#41415);
#13366=VERTEX_POINT('',#41419);
#13367=VERTEX_POINT('',#41423);
#13368=VERTEX_POINT('',#41426);
#13369=VERTEX_POINT('',#41431);
#13370=VERTEX_POINT('',#41445);
#13371=VERTEX_POINT('',#41447);
#13372=VERTEX_POINT('',#41449);
#13373=VERTEX_POINT('',#41451);
#13374=VERTEX_POINT('',#41453);
#13375=VERTEX_POINT('',#41457);
#13376=VERTEX_POINT('',#41461);
#13377=VERTEX_POINT('',#41465);
#13378=VERTEX_POINT('',#41469);
#13379=VERTEX_POINT('',#41473);
#13380=VERTEX_POINT('',#41482);
#13381=VERTEX_POINT('',#41483);
#13382=VERTEX_POINT('',#41485);
#13383=VERTEX_POINT('',#41490);
#13384=VERTEX_POINT('',#41492);
#13385=VERTEX_POINT('',#41496);
#13386=VERTEX_POINT('',#41499);
#13387=VERTEX_POINT('',#41503);
#13388=VERTEX_POINT('',#41506);
#13389=VERTEX_POINT('',#41510);
#13390=VERTEX_POINT('',#41517);
#13391=VERTEX_POINT('',#41518);
#13392=VERTEX_POINT('',#41521);
#13393=VERTEX_POINT('',#41544);
#13394=VERTEX_POINT('',#41738);
#13395=VERTEX_POINT('',#41740);
#13396=VERTEX_POINT('',#41753);
#13397=VERTEX_POINT('',#41806);
#13398=VERTEX_POINT('',#41833);
#13399=VERTEX_POINT('',#41834);
#13400=VERTEX_POINT('',#41880);
#13401=VERTEX_POINT('',#42031);
#13402=VERTEX_POINT('',#42032);
#13403=VERTEX_POINT('',#42131);
#13404=VERTEX_POINT('',#42132);
#13405=VERTEX_POINT('',#42134);
#13406=VERTEX_POINT('',#42179);
#13407=VERTEX_POINT('',#42297);
#13408=VERTEX_POINT('',#42298);
#13409=VERTEX_POINT('',#42300);
#13410=VERTEX_POINT('',#42404);
#13411=VERTEX_POINT('',#42405);
#13412=VERTEX_POINT('',#42407);
#13413=VERTEX_POINT('',#42499);
#13414=VERTEX_POINT('',#42500);
#13415=VERTEX_POINT('',#42502);
#13416=VERTEX_POINT('',#42744);
#13417=VERTEX_POINT('',#42930);
#13418=VERTEX_POINT('',#42931);
#13419=VERTEX_POINT('',#42975);
#13420=VERTEX_POINT('',#43021);
#13421=VERTEX_POINT('',#43046);
#13422=VERTEX_POINT('',#43067);
#13423=VERTEX_POINT('',#43069);
#13424=VERTEX_POINT('',#43117);
#13425=VERTEX_POINT('',#43118);
#13426=VERTEX_POINT('',#43164);
#13427=VERTEX_POINT('',#43197);
#13428=VERTEX_POINT('',#43309);
#13429=VERTEX_POINT('',#43310);
#13430=VERTEX_POINT('',#43312);
#13431=VERTEX_POINT('',#43408);
#13432=VERTEX_POINT('',#43409);
#13433=VERTEX_POINT('',#43411);
#13434=VERTEX_POINT('',#43456);
#13435=VERTEX_POINT('',#43461);
#13436=VERTEX_POINT('',#43584);
#13437=VERTEX_POINT('',#43585);
#13438=VERTEX_POINT('',#43587);
#13439=VERTEX_POINT('',#43679);
#13440=VERTEX_POINT('',#43680);
#13441=VERTEX_POINT('',#43725);
#13442=VERTEX_POINT('',#43772);
#13443=VERTEX_POINT('',#43773);
#13444=VERTEX_POINT('',#43775);
#13445=VERTEX_POINT('',#43822);
#13446=VERTEX_POINT('',#43866);
#13447=VERTEX_POINT('',#43867);
#13448=VERTEX_POINT('',#43952);
#13449=VERTEX_POINT('',#43953);
#13450=VERTEX_POINT('',#43955);
#13451=VERTEX_POINT('',#44000);
#13452=VERTEX_POINT('',#44158);
#13453=VERTEX_POINT('',#44159);
#13454=VERTEX_POINT('',#44203);
#13455=VERTEX_POINT('',#44314);
#13456=VERTEX_POINT('',#44315);
#13457=VERTEX_POINT('',#44404);
#13458=VERTEX_POINT('',#44437);
#13459=VERTEX_POINT('',#44452);
#13460=VERTEX_POINT('',#44454);
#13461=VERTEX_POINT('',#44504);
#13462=VERTEX_POINT('',#44505);
#13463=VERTEX_POINT('',#44547);
#13464=VERTEX_POINT('',#44607);
#13465=VERTEX_POINT('',#44608);
#13466=VERTEX_POINT('',#44610);
#13467=VERTEX_POINT('',#44623);
#13468=VERTEX_POINT('',#44845);
#13469=VERTEX_POINT('',#44899);
#13470=VERTEX_POINT('',#44900);
#13471=VERTEX_POINT('',#44902);
#13472=VERTEX_POINT('',#45185);
#13473=VERTEX_POINT('',#45342);
#13474=VERTEX_POINT('',#45343);
#13475=VERTEX_POINT('',#45430);
#13476=VERTEX_POINT('',#45431);
#13477=VERTEX_POINT('',#45433);
#13478=VERTEX_POINT('',#45440);
#13479=VERTEX_POINT('',#45779);
#13480=VERTEX_POINT('',#45825);
#13481=VERTEX_POINT('',#45862);
#13482=VERTEX_POINT('',#45875);
#13483=VERTEX_POINT('',#45918);
#13484=VERTEX_POINT('',#45919);
#13485=VERTEX_POINT('',#46004);
#13486=VERTEX_POINT('',#46005);
#13487=VERTEX_POINT('',#46007);
#13488=VERTEX_POINT('',#46058);
#13489=VERTEX_POINT('',#46104);
#13490=VERTEX_POINT('',#46105);
#13491=VERTEX_POINT('',#46192);
#13492=VERTEX_POINT('',#46193);
#13493=VERTEX_POINT('',#46195);
#13494=VERTEX_POINT('',#46512);
#13495=VERTEX_POINT('',#46541);
#13496=VERTEX_POINT('',#46648);
#13497=VERTEX_POINT('',#46650);
#13498=VERTEX_POINT('',#46700);
#13499=VERTEX_POINT('',#46701);
#13500=VERTEX_POINT('',#46747);
#13501=VERTEX_POINT('',#46795);
#13502=VERTEX_POINT('',#46796);
#13503=VERTEX_POINT('',#46838);
#13504=VERTEX_POINT('',#46882);
#13505=VERTEX_POINT('',#46883);
#13506=VERTEX_POINT('',#46885);
#13507=VERTEX_POINT('',#46922);
#13508=VERTEX_POINT('',#46940);
#13509=VERTEX_POINT('',#46992);
#13510=VERTEX_POINT('',#46993);
#13511=VERTEX_POINT('',#46995);
#13512=VERTEX_POINT('',#47085);
#13513=VERTEX_POINT('',#47086);
#13514=VERTEX_POINT('',#47088);
#13515=VERTEX_POINT('',#47139);
#13516=VERTEX_POINT('',#47185);
#13517=VERTEX_POINT('',#47224);
#13518=VERTEX_POINT('',#47271);
#13519=VERTEX_POINT('',#47272);
#13520=VERTEX_POINT('',#47274);
#13521=VERTEX_POINT('',#47279);
#13522=VERTEX_POINT('',#47615);
#13523=VERTEX_POINT('',#47616);
#13524=VERTEX_POINT('',#47660);
#13525=VERTEX_POINT('',#47704);
#13526=VERTEX_POINT('',#47705);
#13527=VERTEX_POINT('',#47707);
#13528=VERTEX_POINT('',#47748);
#13529=VERTEX_POINT('',#47824);
#13530=VERTEX_POINT('',#47825);
#13531=VERTEX_POINT('',#47871);
#13532=VERTEX_POINT('',#47917);
#13533=VERTEX_POINT('',#47918);
#13534=VERTEX_POINT('',#47920);
#13535=VERTEX_POINT('',#47925);
#13536=VERTEX_POINT('',#47960);
#13537=VERTEX_POINT('',#47996);
#13538=VERTEX_POINT('',#48039);
#13539=VERTEX_POINT('',#48051);
#13540=VERTEX_POINT('',#48052);
#13541=VERTEX_POINT('',#48054);
#13542=VERTEX_POINT('',#48146);
#13543=VERTEX_POINT('',#48147);
#13544=VERTEX_POINT('',#48149);
#13545=VERTEX_POINT('',#48200);
#13546=VERTEX_POINT('',#48246);
#13547=VERTEX_POINT('',#48247);
#13548=VERTEX_POINT('',#48332);
#13549=VERTEX_POINT('',#48333);
#13550=VERTEX_POINT('',#48335);
#13551=VERTEX_POINT('',#48431);
#13552=VERTEX_POINT('',#48433);
#13553=VERTEX_POINT('',#48435);
#13554=VERTEX_POINT('',#48482);
#13555=VERTEX_POINT('',#48532);
#13556=VERTEX_POINT('',#48534);
#13557=VERTEX_POINT('',#48557);
#13558=VERTEX_POINT('',#48582);
#13559=VERTEX_POINT('',#48631);
#13560=VERTEX_POINT('',#48666);
#13561=VERTEX_POINT('',#48671);
#13562=VERTEX_POINT('',#48687);
#13563=VERTEX_POINT('',#48688);
#13564=VERTEX_POINT('',#48692);
#13565=VERTEX_POINT('',#48693);
#13566=VERTEX_POINT('',#48700);
#13567=VERTEX_POINT('',#48702);
#13568=VERTEX_POINT('',#49448);
#13569=VERTEX_POINT('',#49678);
#13570=VERTEX_POINT('',#68983);
#13571=VERTEX_POINT('',#68986);
#13572=VERTEX_POINT('',#68990);
#13573=VERTEX_POINT('',#68995);
#13574=VERTEX_POINT('',#68999);
#13575=VERTEX_POINT('',#69002);
#13576=VERTEX_POINT('',#69006);
#13577=VERTEX_POINT('',#69012);
#13578=VERTEX_POINT('',#69013);
#13579=VERTEX_POINT('',#69020);
#13580=VERTEX_POINT('',#69022);
#13581=VERTEX_POINT('',#69024);
#13582=VERTEX_POINT('',#69031);
#13583=VERTEX_POINT('',#69033);
#13584=VERTEX_POINT('',#69035);
#13585=VERTEX_POINT('',#69042);
#13586=VERTEX_POINT('',#69044);
#13587=VERTEX_POINT('',#69046);
#13588=VERTEX_POINT('',#69058);
#13589=VERTEX_POINT('',#69060);
#13590=VERTEX_POINT('',#69062);
#13591=VERTEX_POINT('',#69069);
#13592=VERTEX_POINT('',#69071);
#13593=VERTEX_POINT('',#69073);
#13594=VERTEX_POINT('',#69080);
#13595=VERTEX_POINT('',#69082);
#13596=VERTEX_POINT('',#69090);
#13597=VERTEX_POINT('',#69092);
#13598=VERTEX_POINT('',#69138);
#13599=VERTEX_POINT('',#69140);
#13600=VERTEX_POINT('',#69144);
#13601=VERTEX_POINT('',#69148);
#13602=VERTEX_POINT('',#69150);
#13603=VERTEX_POINT('',#69154);
#13604=VERTEX_POINT('',#69156);
#13605=VERTEX_POINT('',#69160);
#13606=VERTEX_POINT('',#69164);
#13607=VERTEX_POINT('',#69168);
#13608=VERTEX_POINT('',#69170);
#13609=VERTEX_POINT('',#69174);
#13610=VERTEX_POINT('',#69176);
#13611=VERTEX_POINT('',#69180);
#13612=VERTEX_POINT('',#69184);
#13613=VERTEX_POINT('',#69192);
#13614=VERTEX_POINT('',#69193);
#13615=VERTEX_POINT('',#69195);
#13616=VERTEX_POINT('',#69197);
#13617=VERTEX_POINT('',#69201);
#13618=VERTEX_POINT('',#69205);
#13619=VERTEX_POINT('',#69211);
#13620=VERTEX_POINT('',#69212);
#13621=VERTEX_POINT('',#69214);
#13622=VERTEX_POINT('',#69216);
#13623=VERTEX_POINT('',#69220);
#13624=VERTEX_POINT('',#69224);
#13625=VERTEX_POINT('',#69230);
#13626=VERTEX_POINT('',#69231);
#13627=VERTEX_POINT('',#69233);
#13628=VERTEX_POINT('',#69235);
#13629=VERTEX_POINT('',#69239);
#13630=VERTEX_POINT('',#69243);
#13631=VERTEX_POINT('',#69249);
#13632=VERTEX_POINT('',#69250);
#13633=VERTEX_POINT('',#69252);
#13634=VERTEX_POINT('',#69254);
#13635=VERTEX_POINT('',#69258);
#13636=VERTEX_POINT('',#69262);
#13637=VERTEX_POINT('',#69268);
#13638=VERTEX_POINT('',#69269);
#13639=VERTEX_POINT('',#69271);
#13640=VERTEX_POINT('',#69273);
#13641=VERTEX_POINT('',#69277);
#13642=VERTEX_POINT('',#69281);
#13643=VERTEX_POINT('',#69287);
#13644=VERTEX_POINT('',#69288);
#13645=VERTEX_POINT('',#69290);
#13646=VERTEX_POINT('',#69292);
#13647=VERTEX_POINT('',#69296);
#13648=VERTEX_POINT('',#69300);
#13649=VERTEX_POINT('',#69306);
#13650=VERTEX_POINT('',#69307);
#13651=VERTEX_POINT('',#69309);
#13652=VERTEX_POINT('',#69311);
#13653=VERTEX_POINT('',#69315);
#13654=VERTEX_POINT('',#69319);
#13655=VERTEX_POINT('',#69325);
#13656=VERTEX_POINT('',#69326);
#13657=VERTEX_POINT('',#69328);
#13658=VERTEX_POINT('',#69330);
#13659=VERTEX_POINT('',#69334);
#13660=VERTEX_POINT('',#69338);
#13661=VERTEX_POINT('',#69344);
#13662=VERTEX_POINT('',#69345);
#13663=VERTEX_POINT('',#69347);
#13664=VERTEX_POINT('',#69349);
#13665=VERTEX_POINT('',#69353);
#13666=VERTEX_POINT('',#69357);
#13667=VERTEX_POINT('',#69363);
#13668=VERTEX_POINT('',#69364);
#13669=VERTEX_POINT('',#69366);
#13670=VERTEX_POINT('',#69368);
#13671=VERTEX_POINT('',#69372);
#13672=VERTEX_POINT('',#69376);
#13673=VERTEX_POINT('',#69382);
#13674=VERTEX_POINT('',#69383);
#13675=VERTEX_POINT('',#69385);
#13676=VERTEX_POINT('',#69387);
#13677=VERTEX_POINT('',#69391);
#13678=VERTEX_POINT('',#69395);
#13679=VERTEX_POINT('',#69401);
#13680=VERTEX_POINT('',#69402);
#13681=VERTEX_POINT('',#69404);
#13682=VERTEX_POINT('',#69406);
#13683=VERTEX_POINT('',#69410);
#13684=VERTEX_POINT('',#69414);
#13685=VERTEX_POINT('',#69420);
#13686=VERTEX_POINT('',#69421);
#13687=VERTEX_POINT('',#69423);
#13688=VERTEX_POINT('',#69425);
#13689=VERTEX_POINT('',#69429);
#13690=VERTEX_POINT('',#69433);
#13691=VERTEX_POINT('',#69439);
#13692=VERTEX_POINT('',#69440);
#13693=VERTEX_POINT('',#69442);
#13694=VERTEX_POINT('',#69444);
#13695=VERTEX_POINT('',#69448);
#13696=VERTEX_POINT('',#69452);
#13697=VERTEX_POINT('',#69458);
#13698=VERTEX_POINT('',#69459);
#13699=VERTEX_POINT('',#69461);
#13700=VERTEX_POINT('',#69463);
#13701=VERTEX_POINT('',#69467);
#13702=VERTEX_POINT('',#69471);
#13703=VERTEX_POINT('',#69477);
#13704=VERTEX_POINT('',#69478);
#13705=VERTEX_POINT('',#69480);
#13706=VERTEX_POINT('',#69482);
#13707=VERTEX_POINT('',#69486);
#13708=VERTEX_POINT('',#69490);
#13709=VERTEX_POINT('',#69496);
#13710=VERTEX_POINT('',#69497);
#13711=VERTEX_POINT('',#69499);
#13712=VERTEX_POINT('',#69501);
#13713=VERTEX_POINT('',#69505);
#13714=VERTEX_POINT('',#69509);
#13715=VERTEX_POINT('',#69515);
#13716=VERTEX_POINT('',#69516);
#13717=VERTEX_POINT('',#69518);
#13718=VERTEX_POINT('',#69520);
#13719=VERTEX_POINT('',#69524);
#13720=VERTEX_POINT('',#69528);
#13721=VERTEX_POINT('',#69534);
#13722=VERTEX_POINT('',#69535);
#13723=VERTEX_POINT('',#69537);
#13724=VERTEX_POINT('',#69539);
#13725=VERTEX_POINT('',#69543);
#13726=VERTEX_POINT('',#69545);
#13727=VERTEX_POINT('',#69549);
#13728=VERTEX_POINT('',#69553);
#13729=VERTEX_POINT('',#69557);
#13730=VERTEX_POINT('',#69558);
#13731=VERTEX_POINT('',#69560);
#13732=VERTEX_POINT('',#69562);
#13733=VERTEX_POINT('',#69566);
#13734=VERTEX_POINT('',#69570);
#13735=VERTEX_POINT('',#69576);
#13736=VERTEX_POINT('',#69577);
#13737=VERTEX_POINT('',#69579);
#13738=VERTEX_POINT('',#69581);
#13739=VERTEX_POINT('',#69585);
#13740=VERTEX_POINT('',#69589);
#13741=VERTEX_POINT('',#69595);
#13742=VERTEX_POINT('',#69596);
#13743=VERTEX_POINT('',#69598);
#13744=VERTEX_POINT('',#69600);
#13745=VERTEX_POINT('',#69604);
#13746=VERTEX_POINT('',#69608);
#13747=VERTEX_POINT('',#69614);
#13748=VERTEX_POINT('',#69615);
#13749=VERTEX_POINT('',#69617);
#13750=VERTEX_POINT('',#69619);
#13751=VERTEX_POINT('',#69623);
#13752=VERTEX_POINT('',#69627);
#13753=VERTEX_POINT('',#69633);
#13754=VERTEX_POINT('',#69634);
#13755=VERTEX_POINT('',#69636);
#13756=VERTEX_POINT('',#69638);
#13757=VERTEX_POINT('',#69642);
#13758=VERTEX_POINT('',#69646);
#13759=VERTEX_POINT('',#69652);
#13760=VERTEX_POINT('',#69653);
#13761=VERTEX_POINT('',#69655);
#13762=VERTEX_POINT('',#69657);
#13763=VERTEX_POINT('',#69661);
#13764=VERTEX_POINT('',#69665);
#13765=VERTEX_POINT('',#69671);
#13766=VERTEX_POINT('',#69672);
#13767=VERTEX_POINT('',#69674);
#13768=VERTEX_POINT('',#69676);
#13769=VERTEX_POINT('',#69680);
#13770=VERTEX_POINT('',#69684);
#13771=VERTEX_POINT('',#69690);
#13772=VERTEX_POINT('',#69691);
#13773=VERTEX_POINT('',#69693);
#13774=VERTEX_POINT('',#69695);
#13775=VERTEX_POINT('',#69699);
#13776=VERTEX_POINT('',#69703);
#13777=VERTEX_POINT('',#69709);
#13778=VERTEX_POINT('',#69710);
#13779=VERTEX_POINT('',#69712);
#13780=VERTEX_POINT('',#69714);
#13781=VERTEX_POINT('',#69718);
#13782=VERTEX_POINT('',#69722);
#13783=VERTEX_POINT('',#69728);
#13784=VERTEX_POINT('',#69729);
#13785=VERTEX_POINT('',#69731);
#13786=VERTEX_POINT('',#69733);
#13787=VERTEX_POINT('',#69737);
#13788=VERTEX_POINT('',#69741);
#13789=VERTEX_POINT('',#69747);
#13790=VERTEX_POINT('',#69748);
#13791=VERTEX_POINT('',#69750);
#13792=VERTEX_POINT('',#69752);
#13793=VERTEX_POINT('',#69756);
#13794=VERTEX_POINT('',#69760);
#13795=VERTEX_POINT('',#69766);
#13796=VERTEX_POINT('',#69767);
#13797=VERTEX_POINT('',#69769);
#13798=VERTEX_POINT('',#69771);
#13799=VERTEX_POINT('',#69775);
#13800=VERTEX_POINT('',#69779);
#13801=VERTEX_POINT('',#69785);
#13802=VERTEX_POINT('',#69786);
#13803=VERTEX_POINT('',#69788);
#13804=VERTEX_POINT('',#69790);
#13805=VERTEX_POINT('',#69794);
#13806=VERTEX_POINT('',#69798);
#13807=VERTEX_POINT('',#69804);
#13808=VERTEX_POINT('',#69805);
#13809=VERTEX_POINT('',#69807);
#13810=VERTEX_POINT('',#69809);
#13811=VERTEX_POINT('',#69813);
#13812=VERTEX_POINT('',#69817);
#13813=VERTEX_POINT('',#69823);
#13814=VERTEX_POINT('',#69824);
#13815=VERTEX_POINT('',#69826);
#13816=VERTEX_POINT('',#69828);
#13817=VERTEX_POINT('',#69832);
#13818=VERTEX_POINT('',#69836);
#13819=VERTEX_POINT('',#69842);
#13820=VERTEX_POINT('',#69843);
#13821=VERTEX_POINT('',#69845);
#13822=VERTEX_POINT('',#69847);
#13823=VERTEX_POINT('',#69851);
#13824=VERTEX_POINT('',#69855);
#13825=VERTEX_POINT('',#69861);
#13826=VERTEX_POINT('',#69862);
#13827=VERTEX_POINT('',#69864);
#13828=VERTEX_POINT('',#69866);
#13829=VERTEX_POINT('',#69870);
#13830=VERTEX_POINT('',#69874);
#13831=VERTEX_POINT('',#69880);
#13832=VERTEX_POINT('',#69881);
#13833=VERTEX_POINT('',#69883);
#13834=VERTEX_POINT('',#69885);
#13835=VERTEX_POINT('',#69889);
#13836=VERTEX_POINT('',#69893);
#13837=VERTEX_POINT('',#69899);
#13838=VERTEX_POINT('',#69901);
#13839=VERTEX_POINT('',#69907);
#13840=VERTEX_POINT('',#69917);
#13841=VERTEX_POINT('',#69919);
#13842=VERTEX_POINT('',#69923);
#13843=VERTEX_POINT('',#69926);
#13844=VERTEX_POINT('',#69930);
#13845=VERTEX_POINT('',#69935);
#13846=VERTEX_POINT('',#69939);
#13847=VERTEX_POINT('',#69942);
#13848=VERTEX_POINT('',#69946);
#13849=VERTEX_POINT('',#69957);
#13850=VERTEX_POINT('',#69958);
#13851=VERTEX_POINT('',#69962);
#13852=VERTEX_POINT('',#69964);
#13853=VERTEX_POINT('',#69975);
#13854=VERTEX_POINT('',#69979);
#13855=VERTEX_POINT('',#69990);
#13856=VERTEX_POINT('',#69994);
#13857=VERTEX_POINT('',#70005);
#13858=VERTEX_POINT('',#70009);
#13859=VERTEX_POINT('',#70020);
#13860=VERTEX_POINT('',#70024);
#13861=VERTEX_POINT('',#70035);
#13862=VERTEX_POINT('',#70039);
#13863=VERTEX_POINT('',#70050);
#13864=VERTEX_POINT('',#70054);
#13865=VERTEX_POINT('',#70077);
#13866=VERTEX_POINT('',#70078);
#13867=VERTEX_POINT('',#70082);
#13868=VERTEX_POINT('',#70084);
#13869=VERTEX_POINT('',#70095);
#13870=VERTEX_POINT('',#70099);
#13871=VERTEX_POINT('',#70110);
#13872=VERTEX_POINT('',#70114);
#13873=VERTEX_POINT('',#70125);
#13874=VERTEX_POINT('',#70129);
#13875=VERTEX_POINT('',#70140);
#13876=VERTEX_POINT('',#70144);
#13877=VERTEX_POINT('',#70155);
#13878=VERTEX_POINT('',#70159);
#13879=VERTEX_POINT('',#70170);
#13880=VERTEX_POINT('',#70174);
#13881=VERTEX_POINT('',#70185);
#13882=VERTEX_POINT('',#70189);
#13883=VERTEX_POINT('',#70200);
#13884=VERTEX_POINT('',#70204);
#13885=VERTEX_POINT('',#70215);
#13886=VERTEX_POINT('',#70219);
#13887=VERTEX_POINT('',#70230);
#13888=VERTEX_POINT('',#70234);
#13889=VERTEX_POINT('',#70253);
#13890=VERTEX_POINT('',#70254);
#13891=VERTEX_POINT('',#70256);
#13892=VERTEX_POINT('',#70258);
#13893=VERTEX_POINT('',#70262);
#13894=VERTEX_POINT('',#70264);
#13895=VERTEX_POINT('',#70271);
#13896=VERTEX_POINT('',#70272);
#13897=VERTEX_POINT('',#70274);
#13898=VERTEX_POINT('',#70276);
#13899=VERTEX_POINT('',#70280);
#13900=VERTEX_POINT('',#70282);
#13901=VERTEX_POINT('',#70286);
#13902=VERTEX_POINT('',#70288);
#13903=VERTEX_POINT('',#70292);
#13904=VERTEX_POINT('',#70294);
#13905=VERTEX_POINT('',#70298);
#13906=VERTEX_POINT('',#70300);
#13907=VERTEX_POINT('',#70304);
#13908=VERTEX_POINT('',#70306);
#13909=VERTEX_POINT('',#70310);
#13910=VERTEX_POINT('',#70312);
#13911=VERTEX_POINT('',#70316);
#13912=VERTEX_POINT('',#70318);
#13913=VERTEX_POINT('',#70322);
#13914=VERTEX_POINT('',#70324);
#13915=VERTEX_POINT('',#70328);
#13916=VERTEX_POINT('',#70330);
#13917=VERTEX_POINT('',#70345);
#13918=VERTEX_POINT('',#70346);
#13919=VERTEX_POINT('',#70350);
#13920=VERTEX_POINT('',#70352);
#13921=VERTEX_POINT('',#70363);
#13922=VERTEX_POINT('',#70367);
#13923=VERTEX_POINT('',#70378);
#13924=VERTEX_POINT('',#70382);
#13925=VERTEX_POINT('',#70393);
#13926=VERTEX_POINT('',#70397);
#13927=VERTEX_POINT('',#70408);
#13928=VERTEX_POINT('',#70412);
#13929=VERTEX_POINT('',#70423);
#13930=VERTEX_POINT('',#70427);
#13931=VERTEX_POINT('',#70438);
#13932=VERTEX_POINT('',#70442);
#13933=VERTEX_POINT('',#70465);
#13934=VERTEX_POINT('',#70466);
#13935=VERTEX_POINT('',#70470);
#13936=VERTEX_POINT('',#70472);
#13937=VERTEX_POINT('',#70483);
#13938=VERTEX_POINT('',#70487);
#13939=VERTEX_POINT('',#70498);
#13940=VERTEX_POINT('',#70502);
#13941=VERTEX_POINT('',#70513);
#13942=VERTEX_POINT('',#70517);
#13943=VERTEX_POINT('',#70528);
#13944=VERTEX_POINT('',#70532);
#13945=VERTEX_POINT('',#70543);
#13946=VERTEX_POINT('',#70547);
#13947=VERTEX_POINT('',#70558);
#13948=VERTEX_POINT('',#70562);
#13949=VERTEX_POINT('',#70573);
#13950=VERTEX_POINT('',#70577);
#13951=VERTEX_POINT('',#70588);
#13952=VERTEX_POINT('',#70592);
#13953=VERTEX_POINT('',#70603);
#13954=VERTEX_POINT('',#70607);
#13955=VERTEX_POINT('',#70618);
#13956=VERTEX_POINT('',#70622);
#13957=VERTEX_POINT('',#70646);
#13958=VERTEX_POINT('',#70647);
#13959=VERTEX_POINT('',#70651);
#13960=VERTEX_POINT('',#70653);
#13961=VERTEX_POINT('',#70664);
#13962=VERTEX_POINT('',#70668);
#13963=VERTEX_POINT('',#70679);
#13964=VERTEX_POINT('',#70683);
#13965=VERTEX_POINT('',#70694);
#13966=VERTEX_POINT('',#70698);
#13967=VERTEX_POINT('',#70709);
#13968=VERTEX_POINT('',#70713);
#13969=VERTEX_POINT('',#70724);
#13970=VERTEX_POINT('',#70728);
#13971=VERTEX_POINT('',#70739);
#13972=VERTEX_POINT('',#70743);
#13973=VERTEX_POINT('',#70754);
#13974=VERTEX_POINT('',#70758);
#13975=VERTEX_POINT('',#70769);
#13976=VERTEX_POINT('',#70773);
#13977=VERTEX_POINT('',#70784);
#13978=VERTEX_POINT('',#70788);
#13979=VERTEX_POINT('',#70799);
#13980=VERTEX_POINT('',#70803);
#13981=VERTEX_POINT('',#70814);
#13982=VERTEX_POINT('',#70818);
#13983=VERTEX_POINT('',#70824);
#13984=VERTEX_POINT('',#70826);
#13985=VERTEX_POINT('',#70835);
#13986=VERTEX_POINT('',#70839);
#13987=VERTEX_POINT('',#70850);
#13988=VERTEX_POINT('',#70854);
#13989=VERTEX_POINT('',#70865);
#13990=VERTEX_POINT('',#70869);
#13991=VERTEX_POINT('',#70880);
#13992=VERTEX_POINT('',#70884);
#13993=VERTEX_POINT('',#70895);
#13994=VERTEX_POINT('',#70899);
#13995=VERTEX_POINT('',#70910);
#13996=VERTEX_POINT('',#70914);
#13997=VERTEX_POINT('',#70925);
#13998=VERTEX_POINT('',#70929);
#13999=VERTEX_POINT('',#70935);
#14000=VERTEX_POINT('',#70937);
#14001=VERTEX_POINT('',#70946);
#14002=VERTEX_POINT('',#70950);
#14003=VERTEX_POINT('',#70961);
#14004=VERTEX_POINT('',#70965);
#14005=VERTEX_POINT('',#70976);
#14006=VERTEX_POINT('',#70980);
#14007=VERTEX_POINT('',#70991);
#14008=VERTEX_POINT('',#70995);
#14009=VERTEX_POINT('',#71006);
#14010=VERTEX_POINT('',#71010);
#14011=VERTEX_POINT('',#71021);
#14012=VERTEX_POINT('',#71025);
#14013=VERTEX_POINT('',#71036);
#14014=VERTEX_POINT('',#71040);
#14015=VERTEX_POINT('',#71046);
#14016=VERTEX_POINT('',#71048);
#14017=VERTEX_POINT('',#71071);
#14018=VERTEX_POINT('',#71072);
#14019=VERTEX_POINT('',#71076);
#14020=VERTEX_POINT('',#71078);
#14021=VERTEX_POINT('',#71089);
#14022=VERTEX_POINT('',#71093);
#14023=VERTEX_POINT('',#71104);
#14024=VERTEX_POINT('',#71108);
#14025=VERTEX_POINT('',#71119);
#14026=VERTEX_POINT('',#71123);
#14027=VERTEX_POINT('',#71134);
#14028=VERTEX_POINT('',#71138);
#14029=VERTEX_POINT('',#71149);
#14030=VERTEX_POINT('',#71153);
#14031=VERTEX_POINT('',#71164);
#14032=VERTEX_POINT('',#71168);
#14033=VERTEX_POINT('',#71191);
#14034=VERTEX_POINT('',#71192);
#14035=VERTEX_POINT('',#71196);
#14036=VERTEX_POINT('',#71198);
#14037=VERTEX_POINT('',#71209);
#14038=VERTEX_POINT('',#71213);
#14039=VERTEX_POINT('',#71224);
#14040=VERTEX_POINT('',#71228);
#14041=VERTEX_POINT('',#71239);
#14042=VERTEX_POINT('',#71243);
#14043=VERTEX_POINT('',#71254);
#14044=VERTEX_POINT('',#71258);
#14045=VERTEX_POINT('',#71269);
#14046=VERTEX_POINT('',#71273);
#14047=VERTEX_POINT('',#71284);
#14048=VERTEX_POINT('',#71288);
#14049=VERTEX_POINT('',#71299);
#14050=VERTEX_POINT('',#71303);
#14051=VERTEX_POINT('',#71314);
#14052=VERTEX_POINT('',#71318);
#14053=VERTEX_POINT('',#71329);
#14054=VERTEX_POINT('',#71333);
#14055=VERTEX_POINT('',#71344);
#14056=VERTEX_POINT('',#71348);
#14057=VERTEX_POINT('',#71372);
#14058=VERTEX_POINT('',#71373);
#14059=VERTEX_POINT('',#71377);
#14060=VERTEX_POINT('',#71379);
#14061=VERTEX_POINT('',#71390);
#14062=VERTEX_POINT('',#71394);
#14063=VERTEX_POINT('',#71405);
#14064=VERTEX_POINT('',#71409);
#14065=VERTEX_POINT('',#71420);
#14066=VERTEX_POINT('',#71424);
#14067=VERTEX_POINT('',#71435);
#14068=VERTEX_POINT('',#71439);
#14069=VERTEX_POINT('',#71450);
#14070=VERTEX_POINT('',#71454);
#14071=VERTEX_POINT('',#71465);
#14072=VERTEX_POINT('',#71469);
#14073=VERTEX_POINT('',#71480);
#14074=VERTEX_POINT('',#71484);
#14075=VERTEX_POINT('',#71495);
#14076=VERTEX_POINT('',#71499);
#14077=VERTEX_POINT('',#71505);
#14078=VERTEX_POINT('',#71507);
#14079=VERTEX_POINT('',#71516);
#14080=VERTEX_POINT('',#71520);
#14081=VERTEX_POINT('',#71531);
#14082=VERTEX_POINT('',#71535);
#14083=VERTEX_POINT('',#71546);
#14084=VERTEX_POINT('',#71550);
#14085=VERTEX_POINT('',#71561);
#14086=VERTEX_POINT('',#71565);
#14087=VERTEX_POINT('',#71576);
#14088=VERTEX_POINT('',#71580);
#14089=VERTEX_POINT('',#71591);
#14090=VERTEX_POINT('',#71595);
#14091=VERTEX_POINT('',#71606);
#14092=VERTEX_POINT('',#71610);
#14093=VERTEX_POINT('',#71621);
#14094=VERTEX_POINT('',#71625);
#14095=VERTEX_POINT('',#71636);
#14096=VERTEX_POINT('',#71640);
#14097=VERTEX_POINT('',#71646);
#14098=VERTEX_POINT('',#71648);
#14099=VERTEX_POINT('',#71652);
#14100=VERTEX_POINT('',#71654);
#14101=VERTEX_POINT('',#71668);
#14102=VERTEX_POINT('',#71669);
#14103=VERTEX_POINT('',#71673);
#14104=VERTEX_POINT('',#71675);
#14105=VERTEX_POINT('',#71686);
#14106=VERTEX_POINT('',#71690);
#14107=VERTEX_POINT('',#71701);
#14108=VERTEX_POINT('',#71705);
#14109=VERTEX_POINT('',#71716);
#14110=VERTEX_POINT('',#71720);
#14111=VERTEX_POINT('',#71731);
#14112=VERTEX_POINT('',#71735);
#14113=VERTEX_POINT('',#71746);
#14114=VERTEX_POINT('',#71750);
#14115=VERTEX_POINT('',#71761);
#14116=VERTEX_POINT('',#71765);
#14117=VERTEX_POINT('',#71788);
#14118=VERTEX_POINT('',#71789);
#14119=VERTEX_POINT('',#71793);
#14120=VERTEX_POINT('',#71795);
#14121=VERTEX_POINT('',#71806);
#14122=VERTEX_POINT('',#71810);
#14123=VERTEX_POINT('',#71821);
#14124=VERTEX_POINT('',#71825);
#14125=VERTEX_POINT('',#71836);
#14126=VERTEX_POINT('',#71840);
#14127=VERTEX_POINT('',#71851);
#14128=VERTEX_POINT('',#71855);
#14129=VERTEX_POINT('',#71866);
#14130=VERTEX_POINT('',#71870);
#14131=VERTEX_POINT('',#71881);
#14132=VERTEX_POINT('',#71885);
#14133=VERTEX_POINT('',#71896);
#14134=VERTEX_POINT('',#71900);
#14135=VERTEX_POINT('',#71911);
#14136=VERTEX_POINT('',#71915);
#14137=VERTEX_POINT('',#71926);
#14138=VERTEX_POINT('',#71930);
#14139=VERTEX_POINT('',#71941);
#14140=VERTEX_POINT('',#71945);
#14141=VERTEX_POINT('',#71964);
#14142=VERTEX_POINT('',#71965);
#14143=VERTEX_POINT('',#71967);
#14144=VERTEX_POINT('',#71969);
#14145=VERTEX_POINT('',#71978);
#14146=VERTEX_POINT('',#71982);
#14147=VERTEX_POINT('',#71993);
#14148=VERTEX_POINT('',#71997);
#14149=VERTEX_POINT('',#72003);
#14150=VERTEX_POINT('',#72005);
#14151=VERTEX_POINT('',#72014);
#14152=VERTEX_POINT('',#72018);
#14153=VERTEX_POINT('',#72029);
#14154=VERTEX_POINT('',#72033);
#14155=VERTEX_POINT('',#72039);
#14156=VERTEX_POINT('',#72041);
#14157=VERTEX_POINT('',#72045);
#14158=VERTEX_POINT('',#72047);
#14159=VERTEX_POINT('',#72061);
#14160=VERTEX_POINT('',#72062);
#14161=VERTEX_POINT('',#72066);
#14162=VERTEX_POINT('',#72068);
#14163=VERTEX_POINT('',#72079);
#14164=VERTEX_POINT('',#72083);
#14165=VERTEX_POINT('',#72094);
#14166=VERTEX_POINT('',#72098);
#14167=VERTEX_POINT('',#72109);
#14168=VERTEX_POINT('',#72113);
#14169=VERTEX_POINT('',#72124);
#14170=VERTEX_POINT('',#72128);
#14171=VERTEX_POINT('',#72139);
#14172=VERTEX_POINT('',#72143);
#14173=VERTEX_POINT('',#72154);
#14174=VERTEX_POINT('',#72158);
#14175=VERTEX_POINT('',#72181);
#14176=VERTEX_POINT('',#72182);
#14177=VERTEX_POINT('',#72186);
#14178=VERTEX_POINT('',#72188);
#14179=VERTEX_POINT('',#72199);
#14180=VERTEX_POINT('',#72203);
#14181=VERTEX_POINT('',#72214);
#14182=VERTEX_POINT('',#72218);
#14183=VERTEX_POINT('',#72229);
#14184=VERTEX_POINT('',#72233);
#14185=VERTEX_POINT('',#72244);
#14186=VERTEX_POINT('',#72248);
#14187=VERTEX_POINT('',#72259);
#14188=VERTEX_POINT('',#72263);
#14189=VERTEX_POINT('',#72274);
#14190=VERTEX_POINT('',#72278);
#14191=VERTEX_POINT('',#72289);
#14192=VERTEX_POINT('',#72293);
#14193=VERTEX_POINT('',#72304);
#14194=VERTEX_POINT('',#72308);
#14195=VERTEX_POINT('',#72319);
#14196=VERTEX_POINT('',#72323);
#14197=VERTEX_POINT('',#72334);
#14198=VERTEX_POINT('',#72338);
#14199=VERTEX_POINT('',#72363);
#14200=VERTEX_POINT('',#72364);
#14201=VERTEX_POINT('',#72368);
#14202=VERTEX_POINT('',#72370);
#14203=VERTEX_POINT('',#72381);
#14204=VERTEX_POINT('',#72385);
#14205=VERTEX_POINT('',#72396);
#14206=VERTEX_POINT('',#72400);
#14207=VERTEX_POINT('',#72411);
#14208=VERTEX_POINT('',#72415);
#14209=VERTEX_POINT('',#72426);
#14210=VERTEX_POINT('',#72430);
#14211=VERTEX_POINT('',#72441);
#14212=VERTEX_POINT('',#72445);
#14213=VERTEX_POINT('',#72456);
#14214=VERTEX_POINT('',#72460);
#14215=VERTEX_POINT('',#72483);
#14216=VERTEX_POINT('',#72484);
#14217=VERTEX_POINT('',#72488);
#14218=VERTEX_POINT('',#72490);
#14219=VERTEX_POINT('',#72501);
#14220=VERTEX_POINT('',#72505);
#14221=VERTEX_POINT('',#72516);
#14222=VERTEX_POINT('',#72520);
#14223=VERTEX_POINT('',#72531);
#14224=VERTEX_POINT('',#72535);
#14225=VERTEX_POINT('',#72546);
#14226=VERTEX_POINT('',#72550);
#14227=VERTEX_POINT('',#72561);
#14228=VERTEX_POINT('',#72565);
#14229=VERTEX_POINT('',#72576);
#14230=VERTEX_POINT('',#72580);
#14231=VERTEX_POINT('',#72591);
#14232=VERTEX_POINT('',#72595);
#14233=VERTEX_POINT('',#72606);
#14234=VERTEX_POINT('',#72610);
#14235=VERTEX_POINT('',#72621);
#14236=VERTEX_POINT('',#72625);
#14237=VERTEX_POINT('',#72636);
#14238=VERTEX_POINT('',#72640);
#14239=VERTEX_POINT('',#72659);
#14240=VERTEX_POINT('',#72660);
#14241=VERTEX_POINT('',#72662);
#14242=VERTEX_POINT('',#72664);
#14243=VERTEX_POINT('',#72673);
#14244=VERTEX_POINT('',#72677);
#14245=VERTEX_POINT('',#72688);
#14246=VERTEX_POINT('',#72692);
#14247=VERTEX_POINT('',#72698);
#14248=VERTEX_POINT('',#72700);
#14249=VERTEX_POINT('',#72709);
#14250=VERTEX_POINT('',#72713);
#14251=VERTEX_POINT('',#72724);
#14252=VERTEX_POINT('',#72728);
#14253=VERTEX_POINT('',#72734);
#14254=VERTEX_POINT('',#72736);
#14255=VERTEX_POINT('',#72740);
#14256=VERTEX_POINT('',#72742);
#14257=VERTEX_POINT('',#72756);
#14258=VERTEX_POINT('',#72757);
#14259=VERTEX_POINT('',#72761);
#14260=VERTEX_POINT('',#72763);
#14261=VERTEX_POINT('',#72774);
#14262=VERTEX_POINT('',#72778);
#14263=VERTEX_POINT('',#72789);
#14264=VERTEX_POINT('',#72793);
#14265=VERTEX_POINT('',#72804);
#14266=VERTEX_POINT('',#72808);
#14267=VERTEX_POINT('',#72819);
#14268=VERTEX_POINT('',#72823);
#14269=VERTEX_POINT('',#72834);
#14270=VERTEX_POINT('',#72838);
#14271=VERTEX_POINT('',#72849);
#14272=VERTEX_POINT('',#72853);
#14273=VERTEX_POINT('',#72876);
#14274=VERTEX_POINT('',#72877);
#14275=VERTEX_POINT('',#72881);
#14276=VERTEX_POINT('',#72883);
#14277=VERTEX_POINT('',#72894);
#14278=VERTEX_POINT('',#72898);
#14279=VERTEX_POINT('',#72909);
#14280=VERTEX_POINT('',#72913);
#14281=VERTEX_POINT('',#72924);
#14282=VERTEX_POINT('',#72928);
#14283=VERTEX_POINT('',#72939);
#14284=VERTEX_POINT('',#72943);
#14285=VERTEX_POINT('',#72954);
#14286=VERTEX_POINT('',#72958);
#14287=VERTEX_POINT('',#72969);
#14288=VERTEX_POINT('',#72973);
#14289=VERTEX_POINT('',#72984);
#14290=VERTEX_POINT('',#72988);
#14291=VERTEX_POINT('',#72999);
#14292=VERTEX_POINT('',#73003);
#14293=VERTEX_POINT('',#73014);
#14294=VERTEX_POINT('',#73018);
#14295=VERTEX_POINT('',#73029);
#14296=VERTEX_POINT('',#73033);
#14297=VERTEX_POINT('',#73057);
#14298=VERTEX_POINT('',#73058);
#14299=VERTEX_POINT('',#73062);
#14300=VERTEX_POINT('',#73064);
#14301=VERTEX_POINT('',#73075);
#14302=VERTEX_POINT('',#73079);
#14303=VERTEX_POINT('',#73090);
#14304=VERTEX_POINT('',#73094);
#14305=VERTEX_POINT('',#73105);
#14306=VERTEX_POINT('',#73109);
#14307=VERTEX_POINT('',#73120);
#14308=VERTEX_POINT('',#73124);
#14309=VERTEX_POINT('',#73135);
#14310=VERTEX_POINT('',#73139);
#14311=VERTEX_POINT('',#73150);
#14312=VERTEX_POINT('',#73154);
#14313=VERTEX_POINT('',#73165);
#14314=VERTEX_POINT('',#73169);
#14315=VERTEX_POINT('',#73180);
#14316=VERTEX_POINT('',#73184);
#14317=VERTEX_POINT('',#73190);
#14318=VERTEX_POINT('',#73192);
#14319=VERTEX_POINT('',#73201);
#14320=VERTEX_POINT('',#73205);
#14321=VERTEX_POINT('',#73216);
#14322=VERTEX_POINT('',#73220);
#14323=VERTEX_POINT('',#73231);
#14324=VERTEX_POINT('',#73235);
#14325=VERTEX_POINT('',#73246);
#14326=VERTEX_POINT('',#73250);
#14327=VERTEX_POINT('',#73261);
#14328=VERTEX_POINT('',#73265);
#14329=VERTEX_POINT('',#73276);
#14330=VERTEX_POINT('',#73280);
#14331=VERTEX_POINT('',#73291);
#14332=VERTEX_POINT('',#73295);
#14333=VERTEX_POINT('',#73306);
#14334=VERTEX_POINT('',#73310);
#14335=VERTEX_POINT('',#73321);
#14336=VERTEX_POINT('',#73325);
#14337=VERTEX_POINT('',#73331);
#14338=VERTEX_POINT('',#73333);
#14339=VERTEX_POINT('',#73337);
#14340=VERTEX_POINT('',#73339);
#14341=VERTEX_POINT('',#73353);
#14342=VERTEX_POINT('',#73354);
#14343=VERTEX_POINT('',#73358);
#14344=VERTEX_POINT('',#73360);
#14345=VERTEX_POINT('',#73371);
#14346=VERTEX_POINT('',#73375);
#14347=VERTEX_POINT('',#73386);
#14348=VERTEX_POINT('',#73390);
#14349=VERTEX_POINT('',#73401);
#14350=VERTEX_POINT('',#73405);
#14351=VERTEX_POINT('',#73416);
#14352=VERTEX_POINT('',#73420);
#14353=VERTEX_POINT('',#73431);
#14354=VERTEX_POINT('',#73435);
#14355=VERTEX_POINT('',#73446);
#14356=VERTEX_POINT('',#73450);
#14357=VERTEX_POINT('',#73473);
#14358=VERTEX_POINT('',#73474);
#14359=VERTEX_POINT('',#73478);
#14360=VERTEX_POINT('',#73480);
#14361=VERTEX_POINT('',#73491);
#14362=VERTEX_POINT('',#73495);
#14363=VERTEX_POINT('',#73506);
#14364=VERTEX_POINT('',#73510);
#14365=VERTEX_POINT('',#73521);
#14366=VERTEX_POINT('',#73525);
#14367=VERTEX_POINT('',#73536);
#14368=VERTEX_POINT('',#73540);
#14369=VERTEX_POINT('',#73551);
#14370=VERTEX_POINT('',#73555);
#14371=VERTEX_POINT('',#73566);
#14372=VERTEX_POINT('',#73570);
#14373=VERTEX_POINT('',#73581);
#14374=VERTEX_POINT('',#73585);
#14375=VERTEX_POINT('',#73596);
#14376=VERTEX_POINT('',#73600);
#14377=VERTEX_POINT('',#73611);
#14378=VERTEX_POINT('',#73615);
#14379=VERTEX_POINT('',#73626);
#14380=VERTEX_POINT('',#73630);
#14381=VERTEX_POINT('',#73654);
#14382=VERTEX_POINT('',#73655);
#14383=VERTEX_POINT('',#73659);
#14384=VERTEX_POINT('',#73661);
#14385=VERTEX_POINT('',#73672);
#14386=VERTEX_POINT('',#73676);
#14387=VERTEX_POINT('',#73687);
#14388=VERTEX_POINT('',#73691);
#14389=VERTEX_POINT('',#73702);
#14390=VERTEX_POINT('',#73706);
#14391=VERTEX_POINT('',#73717);
#14392=VERTEX_POINT('',#73721);
#14393=VERTEX_POINT('',#73732);
#14394=VERTEX_POINT('',#73736);
#14395=VERTEX_POINT('',#73747);
#14396=VERTEX_POINT('',#73751);
#14397=VERTEX_POINT('',#73762);
#14398=VERTEX_POINT('',#73766);
#14399=VERTEX_POINT('',#73777);
#14400=VERTEX_POINT('',#73781);
#14401=VERTEX_POINT('',#73792);
#14402=VERTEX_POINT('',#73796);
#14403=VERTEX_POINT('',#73807);
#14404=VERTEX_POINT('',#73811);
#14405=VERTEX_POINT('',#73822);
#14406=VERTEX_POINT('',#73826);
#14407=VERTEX_POINT('',#73832);
#14408=VERTEX_POINT('',#73834);
#14409=VERTEX_POINT('',#73843);
#14410=VERTEX_POINT('',#73847);
#14411=VERTEX_POINT('',#73858);
#14412=VERTEX_POINT('',#73862);
#14413=VERTEX_POINT('',#73873);
#14414=VERTEX_POINT('',#73877);
#14415=VERTEX_POINT('',#73888);
#14416=VERTEX_POINT('',#73892);
#14417=VERTEX_POINT('',#73903);
#14418=VERTEX_POINT('',#73907);
#14419=VERTEX_POINT('',#73918);
#14420=VERTEX_POINT('',#73922);
#14421=VERTEX_POINT('',#73933);
#14422=VERTEX_POINT('',#73937);
#14423=VERTEX_POINT('',#73943);
#14424=VERTEX_POINT('',#73945);
#14425=VERTEX_POINT('',#73954);
#14426=VERTEX_POINT('',#73958);
#14427=VERTEX_POINT('',#73969);
#14428=VERTEX_POINT('',#73973);
#14429=VERTEX_POINT('',#73984);
#14430=VERTEX_POINT('',#73988);
#14431=VERTEX_POINT('',#73999);
#14432=VERTEX_POINT('',#74003);
#14433=VERTEX_POINT('',#74014);
#14434=VERTEX_POINT('',#74018);
#14435=VERTEX_POINT('',#74029);
#14436=VERTEX_POINT('',#74033);
#14437=VERTEX_POINT('',#74044);
#14438=VERTEX_POINT('',#74048);
#14439=VERTEX_POINT('',#74054);
#14440=VERTEX_POINT('',#74056);
#14441=VERTEX_POINT('',#74079);
#14442=VERTEX_POINT('',#74080);
#14443=VERTEX_POINT('',#74084);
#14444=VERTEX_POINT('',#74086);
#14445=VERTEX_POINT('',#74097);
#14446=VERTEX_POINT('',#74101);
#14447=VERTEX_POINT('',#74112);
#14448=VERTEX_POINT('',#74116);
#14449=VERTEX_POINT('',#74127);
#14450=VERTEX_POINT('',#74131);
#14451=VERTEX_POINT('',#74142);
#14452=VERTEX_POINT('',#74146);
#14453=VERTEX_POINT('',#74157);
#14454=VERTEX_POINT('',#74161);
#14455=VERTEX_POINT('',#74172);
#14456=VERTEX_POINT('',#74176);
#14457=VERTEX_POINT('',#74199);
#14458=VERTEX_POINT('',#74200);
#14459=VERTEX_POINT('',#74204);
#14460=VERTEX_POINT('',#74206);
#14461=VERTEX_POINT('',#74217);
#14462=VERTEX_POINT('',#74221);
#14463=VERTEX_POINT('',#74232);
#14464=VERTEX_POINT('',#74236);
#14465=VERTEX_POINT('',#74247);
#14466=VERTEX_POINT('',#74251);
#14467=VERTEX_POINT('',#74262);
#14468=VERTEX_POINT('',#74266);
#14469=VERTEX_POINT('',#74277);
#14470=VERTEX_POINT('',#74281);
#14471=VERTEX_POINT('',#74292);
#14472=VERTEX_POINT('',#74296);
#14473=VERTEX_POINT('',#74307);
#14474=VERTEX_POINT('',#74311);
#14475=VERTEX_POINT('',#74322);
#14476=VERTEX_POINT('',#74326);
#14477=VERTEX_POINT('',#74337);
#14478=VERTEX_POINT('',#74341);
#14479=VERTEX_POINT('',#74352);
#14480=VERTEX_POINT('',#74356);
#14481=VERTEX_POINT('',#74375);
#14482=VERTEX_POINT('',#74376);
#14483=VERTEX_POINT('',#74378);
#14484=VERTEX_POINT('',#74380);
#14485=VERTEX_POINT('',#74384);
#14486=VERTEX_POINT('',#74386);
#14487=VERTEX_POINT('',#74393);
#14488=VERTEX_POINT('',#74394);
#14489=VERTEX_POINT('',#74396);
#14490=VERTEX_POINT('',#74398);
#14491=VERTEX_POINT('',#74402);
#14492=VERTEX_POINT('',#74404);
#14493=VERTEX_POINT('',#74408);
#14494=VERTEX_POINT('',#74410);
#14495=VERTEX_POINT('',#74414);
#14496=VERTEX_POINT('',#74416);
#14497=VERTEX_POINT('',#74420);
#14498=VERTEX_POINT('',#74422);
#14499=VERTEX_POINT('',#74426);
#14500=VERTEX_POINT('',#74428);
#14501=VERTEX_POINT('',#74432);
#14502=VERTEX_POINT('',#74434);
#14503=VERTEX_POINT('',#74438);
#14504=VERTEX_POINT('',#74440);
#14505=VERTEX_POINT('',#74444);
#14506=VERTEX_POINT('',#74446);
#14507=VERTEX_POINT('',#74450);
#14508=VERTEX_POINT('',#74452);
#14509=VERTEX_POINT('',#74462);
#14510=VERTEX_POINT('',#74463);
#14511=VERTEX_POINT('',#74465);
#14512=VERTEX_POINT('',#74467);
#14513=VERTEX_POINT('',#74471);
#14514=VERTEX_POINT('',#74473);
#14515=VERTEX_POINT('',#74477);
#14516=VERTEX_POINT('',#74479);
#14517=VERTEX_POINT('',#74487);
#14518=VERTEX_POINT('',#74488);
#14519=VERTEX_POINT('',#74490);
#14520=VERTEX_POINT('',#74492);
#14521=VERTEX_POINT('',#74496);
#14522=VERTEX_POINT('',#74498);
#14523=VERTEX_POINT('',#74502);
#14524=VERTEX_POINT('',#74504);
#14525=VERTEX_POINT('',#74512);
#14526=VERTEX_POINT('',#74513);
#14527=VERTEX_POINT('',#74515);
#14528=VERTEX_POINT('',#74517);
#14529=VERTEX_POINT('',#74521);
#14530=VERTEX_POINT('',#74523);
#14531=VERTEX_POINT('',#74527);
#14532=VERTEX_POINT('',#74529);
#14533=VERTEX_POINT('',#74537);
#14534=VERTEX_POINT('',#74538);
#14535=VERTEX_POINT('',#74540);
#14536=VERTEX_POINT('',#74542);
#14537=VERTEX_POINT('',#74546);
#14538=VERTEX_POINT('',#74548);
#14539=VERTEX_POINT('',#74552);
#14540=VERTEX_POINT('',#74554);
#14541=VERTEX_POINT('',#74562);
#14542=VERTEX_POINT('',#74563);
#14543=VERTEX_POINT('',#74565);
#14544=VERTEX_POINT('',#74567);
#14545=VERTEX_POINT('',#74571);
#14546=VERTEX_POINT('',#74573);
#14547=VERTEX_POINT('',#74577);
#14548=VERTEX_POINT('',#74579);
#14549=VERTEX_POINT('',#74587);
#14550=VERTEX_POINT('',#74588);
#14551=VERTEX_POINT('',#74590);
#14552=VERTEX_POINT('',#74592);
#14553=VERTEX_POINT('',#74596);
#14554=VERTEX_POINT('',#74598);
#14555=VERTEX_POINT('',#74602);
#14556=VERTEX_POINT('',#74604);
#14557=VERTEX_POINT('',#74612);
#14558=VERTEX_POINT('',#74613);
#14559=VERTEX_POINT('',#74615);
#14560=VERTEX_POINT('',#74617);
#14561=VERTEX_POINT('',#74621);
#14562=VERTEX_POINT('',#74623);
#14563=VERTEX_POINT('',#74627);
#14564=VERTEX_POINT('',#74629);
#14565=VERTEX_POINT('',#74637);
#14566=VERTEX_POINT('',#74638);
#14567=VERTEX_POINT('',#74640);
#14568=VERTEX_POINT('',#74642);
#14569=VERTEX_POINT('',#74646);
#14570=VERTEX_POINT('',#74648);
#14571=VERTEX_POINT('',#74652);
#14572=VERTEX_POINT('',#74654);
#14573=VERTEX_POINT('',#74662);
#14574=VERTEX_POINT('',#74663);
#14575=VERTEX_POINT('',#74665);
#14576=VERTEX_POINT('',#74667);
#14577=VERTEX_POINT('',#74671);
#14578=VERTEX_POINT('',#74673);
#14579=VERTEX_POINT('',#74677);
#14580=VERTEX_POINT('',#74679);
#14581=VERTEX_POINT('',#74687);
#14582=VERTEX_POINT('',#74688);
#14583=VERTEX_POINT('',#74690);
#14584=VERTEX_POINT('',#74692);
#14585=VERTEX_POINT('',#74696);
#14586=VERTEX_POINT('',#74698);
#14587=VERTEX_POINT('',#74702);
#14588=VERTEX_POINT('',#74704);
#14589=VERTEX_POINT('',#74712);
#14590=VERTEX_POINT('',#74713);
#14591=VERTEX_POINT('',#74715);
#14592=VERTEX_POINT('',#74717);
#14593=VERTEX_POINT('',#74721);
#14594=VERTEX_POINT('',#74723);
#14595=VERTEX_POINT('',#74727);
#14596=VERTEX_POINT('',#74729);
#14597=VERTEX_POINT('',#74737);
#14598=VERTEX_POINT('',#74738);
#14599=VERTEX_POINT('',#74740);
#14600=VERTEX_POINT('',#74742);
#14601=VERTEX_POINT('',#74746);
#14602=VERTEX_POINT('',#74748);
#14603=VERTEX_POINT('',#74752);
#14604=VERTEX_POINT('',#74754);
#14605=VERTEX_POINT('',#74762);
#14606=VERTEX_POINT('',#74763);
#14607=VERTEX_POINT('',#74765);
#14608=VERTEX_POINT('',#74767);
#14609=VERTEX_POINT('',#74771);
#14610=VERTEX_POINT('',#74773);
#14611=VERTEX_POINT('',#74777);
#14612=VERTEX_POINT('',#74779);
#14613=VERTEX_POINT('',#74787);
#14614=VERTEX_POINT('',#74788);
#14615=VERTEX_POINT('',#74790);
#14616=VERTEX_POINT('',#74792);
#14617=VERTEX_POINT('',#74796);
#14618=VERTEX_POINT('',#74798);
#14619=VERTEX_POINT('',#74802);
#14620=VERTEX_POINT('',#74804);
#14621=VERTEX_POINT('',#74812);
#14622=VERTEX_POINT('',#74813);
#14623=VERTEX_POINT('',#74815);
#14624=VERTEX_POINT('',#74817);
#14625=VERTEX_POINT('',#74821);
#14626=VERTEX_POINT('',#74823);
#14627=VERTEX_POINT('',#74827);
#14628=VERTEX_POINT('',#74829);
#14629=VERTEX_POINT('',#74837);
#14630=VERTEX_POINT('',#74838);
#14631=VERTEX_POINT('',#74840);
#14632=VERTEX_POINT('',#74842);
#14633=VERTEX_POINT('',#74846);
#14634=VERTEX_POINT('',#74848);
#14635=VERTEX_POINT('',#74852);
#14636=VERTEX_POINT('',#74854);
#14637=VERTEX_POINT('',#74862);
#14638=VERTEX_POINT('',#74863);
#14639=VERTEX_POINT('',#74865);
#14640=VERTEX_POINT('',#74867);
#14641=VERTEX_POINT('',#74871);
#14642=VERTEX_POINT('',#74873);
#14643=VERTEX_POINT('',#74877);
#14644=VERTEX_POINT('',#74879);
#14645=VERTEX_POINT('',#74887);
#14646=VERTEX_POINT('',#74888);
#14647=VERTEX_POINT('',#74890);
#14648=VERTEX_POINT('',#74892);
#14649=VERTEX_POINT('',#74896);
#14650=VERTEX_POINT('',#74898);
#14651=VERTEX_POINT('',#74902);
#14652=VERTEX_POINT('',#74904);
#14653=VERTEX_POINT('',#74912);
#14654=VERTEX_POINT('',#74913);
#14655=VERTEX_POINT('',#74915);
#14656=VERTEX_POINT('',#74917);
#14657=VERTEX_POINT('',#74921);
#14658=VERTEX_POINT('',#74923);
#14659=VERTEX_POINT('',#74927);
#14660=VERTEX_POINT('',#74929);
#14661=VERTEX_POINT('',#74937);
#14662=VERTEX_POINT('',#74938);
#14663=VERTEX_POINT('',#74940);
#14664=VERTEX_POINT('',#74942);
#14665=VERTEX_POINT('',#74946);
#14666=VERTEX_POINT('',#74948);
#14667=VERTEX_POINT('',#74952);
#14668=VERTEX_POINT('',#74954);
#14669=VERTEX_POINT('',#74962);
#14670=VERTEX_POINT('',#74963);
#14671=VERTEX_POINT('',#74965);
#14672=VERTEX_POINT('',#74967);
#14673=VERTEX_POINT('',#74971);
#14674=VERTEX_POINT('',#74973);
#14675=VERTEX_POINT('',#74977);
#14676=VERTEX_POINT('',#74979);
#14677=VERTEX_POINT('',#74987);
#14678=VERTEX_POINT('',#74988);
#14679=VERTEX_POINT('',#74990);
#14680=VERTEX_POINT('',#74992);
#14681=VERTEX_POINT('',#74996);
#14682=VERTEX_POINT('',#74998);
#14683=VERTEX_POINT('',#75002);
#14684=VERTEX_POINT('',#75004);
#14685=VERTEX_POINT('',#75012);
#14686=VERTEX_POINT('',#75013);
#14687=VERTEX_POINT('',#75015);
#14688=VERTEX_POINT('',#75017);
#14689=VERTEX_POINT('',#75021);
#14690=VERTEX_POINT('',#75023);
#14691=VERTEX_POINT('',#75027);
#14692=VERTEX_POINT('',#75029);
#14693=VERTEX_POINT('',#75037);
#14694=VERTEX_POINT('',#75038);
#14695=VERTEX_POINT('',#75040);
#14696=VERTEX_POINT('',#75042);
#14697=VERTEX_POINT('',#75046);
#14698=VERTEX_POINT('',#75048);
#14699=VERTEX_POINT('',#75052);
#14700=VERTEX_POINT('',#75054);
#14701=VERTEX_POINT('',#75062);
#14702=VERTEX_POINT('',#75063);
#14703=VERTEX_POINT('',#75065);
#14704=VERTEX_POINT('',#75067);
#14705=VERTEX_POINT('',#75071);
#14706=VERTEX_POINT('',#75073);
#14707=VERTEX_POINT('',#75077);
#14708=VERTEX_POINT('',#75079);
#14709=VERTEX_POINT('',#75087);
#14710=VERTEX_POINT('',#75088);
#14711=VERTEX_POINT('',#75090);
#14712=VERTEX_POINT('',#75092);
#14713=VERTEX_POINT('',#75096);
#14714=VERTEX_POINT('',#75098);
#14715=VERTEX_POINT('',#75102);
#14716=VERTEX_POINT('',#75104);
#14717=VERTEX_POINT('',#75112);
#14718=VERTEX_POINT('',#75113);
#14719=VERTEX_POINT('',#75115);
#14720=VERTEX_POINT('',#75117);
#14721=VERTEX_POINT('',#75121);
#14722=VERTEX_POINT('',#75123);
#14723=VERTEX_POINT('',#75127);
#14724=VERTEX_POINT('',#75129);
#14725=VERTEX_POINT('',#75137);
#14726=VERTEX_POINT('',#75138);
#14727=VERTEX_POINT('',#75140);
#14728=VERTEX_POINT('',#75142);
#14729=VERTEX_POINT('',#75146);
#14730=VERTEX_POINT('',#75148);
#14731=VERTEX_POINT('',#75152);
#14732=VERTEX_POINT('',#75154);
#14733=VERTEX_POINT('',#75162);
#14734=VERTEX_POINT('',#75163);
#14735=VERTEX_POINT('',#75165);
#14736=VERTEX_POINT('',#75167);
#14737=VERTEX_POINT('',#75171);
#14738=VERTEX_POINT('',#75173);
#14739=VERTEX_POINT('',#75177);
#14740=VERTEX_POINT('',#75179);
#14741=VERTEX_POINT('',#75187);
#14742=VERTEX_POINT('',#75188);
#14743=VERTEX_POINT('',#75190);
#14744=VERTEX_POINT('',#75192);
#14745=VERTEX_POINT('',#75196);
#14746=VERTEX_POINT('',#75198);
#14747=VERTEX_POINT('',#75202);
#14748=VERTEX_POINT('',#75204);
#14749=VERTEX_POINT('',#75212);
#14750=VERTEX_POINT('',#75213);
#14751=VERTEX_POINT('',#75215);
#14752=VERTEX_POINT('',#75217);
#14753=VERTEX_POINT('',#75221);
#14754=VERTEX_POINT('',#75223);
#14755=VERTEX_POINT('',#75227);
#14756=VERTEX_POINT('',#75229);
#14757=VERTEX_POINT('',#75237);
#14758=VERTEX_POINT('',#75238);
#14759=VERTEX_POINT('',#75240);
#14760=VERTEX_POINT('',#75242);
#14761=VERTEX_POINT('',#75246);
#14762=VERTEX_POINT('',#75248);
#14763=VERTEX_POINT('',#75252);
#14764=VERTEX_POINT('',#75254);
#14765=VERTEX_POINT('',#75262);
#14766=VERTEX_POINT('',#75263);
#14767=VERTEX_POINT('',#75265);
#14768=VERTEX_POINT('',#75267);
#14769=VERTEX_POINT('',#75271);
#14770=VERTEX_POINT('',#75273);
#14771=VERTEX_POINT('',#75277);
#14772=VERTEX_POINT('',#75279);
#14773=VERTEX_POINT('',#75287);
#14774=VERTEX_POINT('',#75288);
#14775=VERTEX_POINT('',#75290);
#14776=VERTEX_POINT('',#75292);
#14777=VERTEX_POINT('',#75296);
#14778=VERTEX_POINT('',#75298);
#14779=VERTEX_POINT('',#75302);
#14780=VERTEX_POINT('',#75304);
#14781=VERTEX_POINT('',#75312);
#14782=VERTEX_POINT('',#75313);
#14783=VERTEX_POINT('',#75315);
#14784=VERTEX_POINT('',#75317);
#14785=VERTEX_POINT('',#75321);
#14786=VERTEX_POINT('',#75323);
#14787=VERTEX_POINT('',#75327);
#14788=VERTEX_POINT('',#75329);
#14789=VERTEX_POINT('',#75337);
#14790=VERTEX_POINT('',#75338);
#14791=VERTEX_POINT('',#75340);
#14792=VERTEX_POINT('',#75342);
#14793=VERTEX_POINT('',#75346);
#14794=VERTEX_POINT('',#75348);
#14795=VERTEX_POINT('',#75352);
#14796=VERTEX_POINT('',#75354);
#14797=VERTEX_POINT('',#75362);
#14798=VERTEX_POINT('',#75363);
#14799=VERTEX_POINT('',#75365);
#14800=VERTEX_POINT('',#75367);
#14801=VERTEX_POINT('',#75371);
#14802=VERTEX_POINT('',#75373);
#14803=VERTEX_POINT('',#75377);
#14804=VERTEX_POINT('',#75379);
#14805=VERTEX_POINT('',#75387);
#14806=VERTEX_POINT('',#75388);
#14807=VERTEX_POINT('',#75390);
#14808=VERTEX_POINT('',#75392);
#14809=VERTEX_POINT('',#75396);
#14810=VERTEX_POINT('',#75398);
#14811=VERTEX_POINT('',#75402);
#14812=VERTEX_POINT('',#75404);
#14813=VERTEX_POINT('',#75412);
#14814=VERTEX_POINT('',#75413);
#14815=VERTEX_POINT('',#75415);
#14816=VERTEX_POINT('',#75417);
#14817=VERTEX_POINT('',#75421);
#14818=VERTEX_POINT('',#75423);
#14819=VERTEX_POINT('',#75427);
#14820=VERTEX_POINT('',#75429);
#14821=VERTEX_POINT('',#75437);
#14822=VERTEX_POINT('',#75438);
#14823=VERTEX_POINT('',#75440);
#14824=VERTEX_POINT('',#75442);
#14825=VERTEX_POINT('',#75446);
#14826=VERTEX_POINT('',#75448);
#14827=VERTEX_POINT('',#75452);
#14828=VERTEX_POINT('',#75454);
#14829=VERTEX_POINT('',#75462);
#14830=VERTEX_POINT('',#75463);
#14831=VERTEX_POINT('',#75465);
#14832=VERTEX_POINT('',#75467);
#14833=VERTEX_POINT('',#75471);
#14834=VERTEX_POINT('',#75473);
#14835=VERTEX_POINT('',#75477);
#14836=VERTEX_POINT('',#75479);
#14837=VERTEX_POINT('',#75487);
#14838=VERTEX_POINT('',#75488);
#14839=VERTEX_POINT('',#75490);
#14840=VERTEX_POINT('',#75492);
#14841=VERTEX_POINT('',#75496);
#14842=VERTEX_POINT('',#75498);
#14843=VERTEX_POINT('',#75502);
#14844=VERTEX_POINT('',#75504);
#14845=VERTEX_POINT('',#75512);
#14846=VERTEX_POINT('',#75513);
#14847=VERTEX_POINT('',#75515);
#14848=VERTEX_POINT('',#75517);
#14849=VERTEX_POINT('',#75521);
#14850=VERTEX_POINT('',#75523);
#14851=VERTEX_POINT('',#75527);
#14852=VERTEX_POINT('',#75529);
#14853=VERTEX_POINT('',#75537);
#14854=VERTEX_POINT('',#75538);
#14855=VERTEX_POINT('',#75540);
#14856=VERTEX_POINT('',#75542);
#14857=VERTEX_POINT('',#75546);
#14858=VERTEX_POINT('',#75548);
#14859=VERTEX_POINT('',#75552);
#14860=VERTEX_POINT('',#75554);
#14861=VERTEX_POINT('',#75562);
#14862=VERTEX_POINT('',#75563);
#14863=VERTEX_POINT('',#75565);
#14864=VERTEX_POINT('',#75567);
#14865=VERTEX_POINT('',#75571);
#14866=VERTEX_POINT('',#75573);
#14867=VERTEX_POINT('',#75577);
#14868=VERTEX_POINT('',#75579);
#14869=VERTEX_POINT('',#75587);
#14870=VERTEX_POINT('',#75588);
#14871=VERTEX_POINT('',#75590);
#14872=VERTEX_POINT('',#75592);
#14873=VERTEX_POINT('',#75596);
#14874=VERTEX_POINT('',#75598);
#14875=VERTEX_POINT('',#75602);
#14876=VERTEX_POINT('',#75604);
#14877=VERTEX_POINT('',#75612);
#14878=VERTEX_POINT('',#75613);
#14879=VERTEX_POINT('',#75615);
#14880=VERTEX_POINT('',#75617);
#14881=VERTEX_POINT('',#75621);
#14882=VERTEX_POINT('',#75623);
#14883=VERTEX_POINT('',#75627);
#14884=VERTEX_POINT('',#75629);
#14885=VERTEX_POINT('',#75637);
#14886=VERTEX_POINT('',#75638);
#14887=VERTEX_POINT('',#75640);
#14888=VERTEX_POINT('',#75642);
#14889=VERTEX_POINT('',#75646);
#14890=VERTEX_POINT('',#75648);
#14891=VERTEX_POINT('',#75652);
#14892=VERTEX_POINT('',#75654);
#14893=VERTEX_POINT('',#75662);
#14894=VERTEX_POINT('',#75663);
#14895=VERTEX_POINT('',#75665);
#14896=VERTEX_POINT('',#75667);
#14897=VERTEX_POINT('',#75671);
#14898=VERTEX_POINT('',#75673);
#14899=VERTEX_POINT('',#75677);
#14900=VERTEX_POINT('',#75679);
#14901=VERTEX_POINT('',#75687);
#14902=VERTEX_POINT('',#75688);
#14903=VERTEX_POINT('',#75690);
#14904=VERTEX_POINT('',#75692);
#14905=VERTEX_POINT('',#75696);
#14906=VERTEX_POINT('',#75698);
#14907=VERTEX_POINT('',#75702);
#14908=VERTEX_POINT('',#75704);
#14909=VERTEX_POINT('',#75712);
#14910=VERTEX_POINT('',#75713);
#14911=VERTEX_POINT('',#75715);
#14912=VERTEX_POINT('',#75717);
#14913=VERTEX_POINT('',#75721);
#14914=VERTEX_POINT('',#75723);
#14915=VERTEX_POINT('',#75727);
#14916=VERTEX_POINT('',#75729);
#14917=VERTEX_POINT('',#75737);
#14918=VERTEX_POINT('',#75738);
#14919=VERTEX_POINT('',#75740);
#14920=VERTEX_POINT('',#75742);
#14921=VERTEX_POINT('',#75746);
#14922=VERTEX_POINT('',#75748);
#14923=VERTEX_POINT('',#75752);
#14924=VERTEX_POINT('',#75754);
#14925=VERTEX_POINT('',#75762);
#14926=VERTEX_POINT('',#75763);
#14927=VERTEX_POINT('',#75765);
#14928=VERTEX_POINT('',#75767);
#14929=VERTEX_POINT('',#75771);
#14930=VERTEX_POINT('',#75773);
#14931=VERTEX_POINT('',#75777);
#14932=VERTEX_POINT('',#75779);
#14933=VERTEX_POINT('',#75787);
#14934=VERTEX_POINT('',#75788);
#14935=VERTEX_POINT('',#75790);
#14936=VERTEX_POINT('',#75792);
#14937=VERTEX_POINT('',#75796);
#14938=VERTEX_POINT('',#75798);
#14939=VERTEX_POINT('',#75802);
#14940=VERTEX_POINT('',#75804);
#14941=VERTEX_POINT('',#75812);
#14942=VERTEX_POINT('',#75813);
#14943=VERTEX_POINT('',#75815);
#14944=VERTEX_POINT('',#75817);
#14945=VERTEX_POINT('',#75821);
#14946=VERTEX_POINT('',#75823);
#14947=VERTEX_POINT('',#75827);
#14948=VERTEX_POINT('',#75829);
#14949=VERTEX_POINT('',#75837);
#14950=VERTEX_POINT('',#75838);
#14951=VERTEX_POINT('',#75840);
#14952=VERTEX_POINT('',#75842);
#14953=VERTEX_POINT('',#75846);
#14954=VERTEX_POINT('',#75848);
#14955=VERTEX_POINT('',#75852);
#14956=VERTEX_POINT('',#75854);
#14957=VERTEX_POINT('',#75862);
#14958=VERTEX_POINT('',#75863);
#14959=VERTEX_POINT('',#75865);
#14960=VERTEX_POINT('',#75867);
#14961=VERTEX_POINT('',#75871);
#14962=VERTEX_POINT('',#75873);
#14963=VERTEX_POINT('',#75877);
#14964=VERTEX_POINT('',#75879);
#14965=VERTEX_POINT('',#75887);
#14966=VERTEX_POINT('',#75888);
#14967=VERTEX_POINT('',#75890);
#14968=VERTEX_POINT('',#75892);
#14969=VERTEX_POINT('',#75896);
#14970=VERTEX_POINT('',#75898);
#14971=VERTEX_POINT('',#75902);
#14972=VERTEX_POINT('',#75904);
#14973=VERTEX_POINT('',#75912);
#14974=VERTEX_POINT('',#75913);
#14975=VERTEX_POINT('',#75915);
#14976=VERTEX_POINT('',#75917);
#14977=VERTEX_POINT('',#75921);
#14978=VERTEX_POINT('',#75923);
#14979=VERTEX_POINT('',#75927);
#14980=VERTEX_POINT('',#75929);
#14981=VERTEX_POINT('',#75937);
#14982=VERTEX_POINT('',#75938);
#14983=VERTEX_POINT('',#75940);
#14984=VERTEX_POINT('',#75942);
#14985=VERTEX_POINT('',#75946);
#14986=VERTEX_POINT('',#75948);
#14987=VERTEX_POINT('',#75952);
#14988=VERTEX_POINT('',#75954);
#14989=VERTEX_POINT('',#75962);
#14990=VERTEX_POINT('',#75963);
#14991=VERTEX_POINT('',#75965);
#14992=VERTEX_POINT('',#75967);
#14993=VERTEX_POINT('',#75971);
#14994=VERTEX_POINT('',#75973);
#14995=VERTEX_POINT('',#75977);
#14996=VERTEX_POINT('',#75979);
#14997=VERTEX_POINT('',#75987);
#14998=VERTEX_POINT('',#75988);
#14999=VERTEX_POINT('',#75990);
#15000=VERTEX_POINT('',#75992);
#15001=VERTEX_POINT('',#75996);
#15002=VERTEX_POINT('',#75998);
#15003=VERTEX_POINT('',#76002);
#15004=VERTEX_POINT('',#76004);
#15005=VERTEX_POINT('',#76012);
#15006=VERTEX_POINT('',#76013);
#15007=VERTEX_POINT('',#76015);
#15008=VERTEX_POINT('',#76017);
#15009=VERTEX_POINT('',#76021);
#15010=VERTEX_POINT('',#76023);
#15011=VERTEX_POINT('',#76027);
#15012=VERTEX_POINT('',#76029);
#15013=VERTEX_POINT('',#76037);
#15014=VERTEX_POINT('',#76038);
#15015=VERTEX_POINT('',#76040);
#15016=VERTEX_POINT('',#76042);
#15017=VERTEX_POINT('',#76046);
#15018=VERTEX_POINT('',#76048);
#15019=VERTEX_POINT('',#76052);
#15020=VERTEX_POINT('',#76054);
#15021=VERTEX_POINT('',#76062);
#15022=VERTEX_POINT('',#76063);
#15023=VERTEX_POINT('',#76065);
#15024=VERTEX_POINT('',#76067);
#15025=VERTEX_POINT('',#76071);
#15026=VERTEX_POINT('',#76073);
#15027=VERTEX_POINT('',#76077);
#15028=VERTEX_POINT('',#76079);
#15029=VERTEX_POINT('',#76087);
#15030=VERTEX_POINT('',#76088);
#15031=VERTEX_POINT('',#76090);
#15032=VERTEX_POINT('',#76092);
#15033=VERTEX_POINT('',#76096);
#15034=VERTEX_POINT('',#76098);
#15035=VERTEX_POINT('',#76102);
#15036=VERTEX_POINT('',#76104);
#15037=VERTEX_POINT('',#76112);
#15038=VERTEX_POINT('',#76113);
#15039=VERTEX_POINT('',#76115);
#15040=VERTEX_POINT('',#76117);
#15041=VERTEX_POINT('',#76121);
#15042=VERTEX_POINT('',#76123);
#15043=VERTEX_POINT('',#76127);
#15044=VERTEX_POINT('',#76129);
#15045=VERTEX_POINT('',#76137);
#15046=VERTEX_POINT('',#76138);
#15047=VERTEX_POINT('',#76140);
#15048=VERTEX_POINT('',#76142);
#15049=VERTEX_POINT('',#76146);
#15050=VERTEX_POINT('',#76148);
#15051=VERTEX_POINT('',#76152);
#15052=VERTEX_POINT('',#76154);
#15053=VERTEX_POINT('',#76162);
#15054=VERTEX_POINT('',#76163);
#15055=VERTEX_POINT('',#76165);
#15056=VERTEX_POINT('',#76167);
#15057=VERTEX_POINT('',#76171);
#15058=VERTEX_POINT('',#76173);
#15059=VERTEX_POINT('',#76177);
#15060=VERTEX_POINT('',#76179);
#15061=VERTEX_POINT('',#76187);
#15062=VERTEX_POINT('',#76188);
#15063=VERTEX_POINT('',#76190);
#15064=VERTEX_POINT('',#76192);
#15065=VERTEX_POINT('',#76196);
#15066=VERTEX_POINT('',#76198);
#15067=VERTEX_POINT('',#76202);
#15068=VERTEX_POINT('',#76204);
#15069=VERTEX_POINT('',#76212);
#15070=VERTEX_POINT('',#76213);
#15071=VERTEX_POINT('',#76215);
#15072=VERTEX_POINT('',#76217);
#15073=VERTEX_POINT('',#76221);
#15074=VERTEX_POINT('',#76223);
#15075=VERTEX_POINT('',#76227);
#15076=VERTEX_POINT('',#76229);
#15077=VERTEX_POINT('',#76237);
#15078=VERTEX_POINT('',#76238);
#15079=VERTEX_POINT('',#76240);
#15080=VERTEX_POINT('',#76242);
#15081=VERTEX_POINT('',#76246);
#15082=VERTEX_POINT('',#76248);
#15083=VERTEX_POINT('',#76252);
#15084=VERTEX_POINT('',#76254);
#15085=VERTEX_POINT('',#76262);
#15086=VERTEX_POINT('',#76263);
#15087=VERTEX_POINT('',#76265);
#15088=VERTEX_POINT('',#76267);
#15089=VERTEX_POINT('',#76271);
#15090=VERTEX_POINT('',#76273);
#15091=VERTEX_POINT('',#76277);
#15092=VERTEX_POINT('',#76279);
#15093=VERTEX_POINT('',#76287);
#15094=VERTEX_POINT('',#76288);
#15095=VERTEX_POINT('',#76290);
#15096=VERTEX_POINT('',#76292);
#15097=VERTEX_POINT('',#76296);
#15098=VERTEX_POINT('',#76298);
#15099=VERTEX_POINT('',#76302);
#15100=VERTEX_POINT('',#76304);
#15101=VERTEX_POINT('',#76312);
#15102=VERTEX_POINT('',#76313);
#15103=VERTEX_POINT('',#76315);
#15104=VERTEX_POINT('',#76317);
#15105=VERTEX_POINT('',#76321);
#15106=VERTEX_POINT('',#76323);
#15107=VERTEX_POINT('',#76327);
#15108=VERTEX_POINT('',#76329);
#15109=VERTEX_POINT('',#76337);
#15110=VERTEX_POINT('',#76338);
#15111=VERTEX_POINT('',#76340);
#15112=VERTEX_POINT('',#76342);
#15113=VERTEX_POINT('',#76346);
#15114=VERTEX_POINT('',#76348);
#15115=VERTEX_POINT('',#76352);
#15116=VERTEX_POINT('',#76354);
#15117=VERTEX_POINT('',#76362);
#15118=VERTEX_POINT('',#76363);
#15119=VERTEX_POINT('',#76365);
#15120=VERTEX_POINT('',#76367);
#15121=VERTEX_POINT('',#76371);
#15122=VERTEX_POINT('',#76373);
#15123=VERTEX_POINT('',#76377);
#15124=VERTEX_POINT('',#76379);
#15125=VERTEX_POINT('',#76387);
#15126=VERTEX_POINT('',#76388);
#15127=VERTEX_POINT('',#76390);
#15128=VERTEX_POINT('',#76392);
#15129=VERTEX_POINT('',#76396);
#15130=VERTEX_POINT('',#76398);
#15131=VERTEX_POINT('',#76402);
#15132=VERTEX_POINT('',#76404);
#15133=VERTEX_POINT('',#76412);
#15134=VERTEX_POINT('',#76413);
#15135=VERTEX_POINT('',#76415);
#15136=VERTEX_POINT('',#76417);
#15137=VERTEX_POINT('',#76421);
#15138=VERTEX_POINT('',#76423);
#15139=VERTEX_POINT('',#76427);
#15140=VERTEX_POINT('',#76429);
#15141=VERTEX_POINT('',#76437);
#15142=VERTEX_POINT('',#76438);
#15143=VERTEX_POINT('',#76440);
#15144=VERTEX_POINT('',#76442);
#15145=VERTEX_POINT('',#76446);
#15146=VERTEX_POINT('',#76448);
#15147=VERTEX_POINT('',#76452);
#15148=VERTEX_POINT('',#76454);
#15149=VERTEX_POINT('',#76462);
#15150=VERTEX_POINT('',#76463);
#15151=VERTEX_POINT('',#76465);
#15152=VERTEX_POINT('',#76467);
#15153=VERTEX_POINT('',#76471);
#15154=VERTEX_POINT('',#76473);
#15155=VERTEX_POINT('',#76477);
#15156=VERTEX_POINT('',#76479);
#15157=VERTEX_POINT('',#76487);
#15158=VERTEX_POINT('',#76488);
#15159=VERTEX_POINT('',#76490);
#15160=VERTEX_POINT('',#76492);
#15161=VERTEX_POINT('',#76496);
#15162=VERTEX_POINT('',#76498);
#15163=VERTEX_POINT('',#76502);
#15164=VERTEX_POINT('',#76504);
#15165=VERTEX_POINT('',#76512);
#15166=VERTEX_POINT('',#76513);
#15167=VERTEX_POINT('',#76515);
#15168=VERTEX_POINT('',#76517);
#15169=VERTEX_POINT('',#76521);
#15170=VERTEX_POINT('',#76523);
#15171=VERTEX_POINT('',#76527);
#15172=VERTEX_POINT('',#76529);
#15173=VERTEX_POINT('',#76537);
#15174=VERTEX_POINT('',#76538);
#15175=VERTEX_POINT('',#76540);
#15176=VERTEX_POINT('',#76542);
#15177=VERTEX_POINT('',#76546);
#15178=VERTEX_POINT('',#76548);
#15179=VERTEX_POINT('',#76552);
#15180=VERTEX_POINT('',#76554);
#15181=VERTEX_POINT('',#76562);
#15182=VERTEX_POINT('',#76563);
#15183=VERTEX_POINT('',#76565);
#15184=VERTEX_POINT('',#76567);
#15185=VERTEX_POINT('',#76571);
#15186=VERTEX_POINT('',#76573);
#15187=VERTEX_POINT('',#76577);
#15188=VERTEX_POINT('',#76579);
#15189=VERTEX_POINT('',#76587);
#15190=VERTEX_POINT('',#76589);
#15191=VERTEX_POINT('',#76593);
#15192=VERTEX_POINT('',#76595);
#15193=VERTEX_POINT('',#76599);
#15194=VERTEX_POINT('',#76600);
#15195=VERTEX_POINT('',#76602);
#15196=VERTEX_POINT('',#76604);
#15197=VERTEX_POINT('',#76608);
#15198=VERTEX_POINT('',#76610);
#15199=VERTEX_POINT('',#76614);
#15200=VERTEX_POINT('',#76616);
#15201=VERTEX_POINT('',#76620);
#15202=VERTEX_POINT('',#76622);
#15203=VERTEX_POINT('',#76626);
#15204=VERTEX_POINT('',#76628);
#15205=VERTEX_POINT('',#76632);
#15206=VERTEX_POINT('',#76634);
#15207=VERTEX_POINT('',#76638);
#15208=VERTEX_POINT('',#76640);
#15209=VERTEX_POINT('',#76650);
#15210=VERTEX_POINT('',#76651);
#15211=VERTEX_POINT('',#76653);
#15212=VERTEX_POINT('',#76655);
#15213=VERTEX_POINT('',#76659);
#15214=VERTEX_POINT('',#76661);
#15215=VERTEX_POINT('',#76665);
#15216=VERTEX_POINT('',#76667);
#15217=VERTEX_POINT('',#76675);
#15218=VERTEX_POINT('',#76676);
#15219=VERTEX_POINT('',#76678);
#15220=VERTEX_POINT('',#76680);
#15221=VERTEX_POINT('',#76684);
#15222=VERTEX_POINT('',#76686);
#15223=VERTEX_POINT('',#76690);
#15224=VERTEX_POINT('',#76692);
#15225=VERTEX_POINT('',#76700);
#15226=VERTEX_POINT('',#76701);
#15227=VERTEX_POINT('',#76703);
#15228=VERTEX_POINT('',#76705);
#15229=VERTEX_POINT('',#76709);
#15230=VERTEX_POINT('',#76711);
#15231=VERTEX_POINT('',#76715);
#15232=VERTEX_POINT('',#76717);
#15233=VERTEX_POINT('',#76725);
#15234=VERTEX_POINT('',#76726);
#15235=VERTEX_POINT('',#76728);
#15236=VERTEX_POINT('',#76730);
#15237=VERTEX_POINT('',#76734);
#15238=VERTEX_POINT('',#76736);
#15239=VERTEX_POINT('',#76740);
#15240=VERTEX_POINT('',#76742);
#15241=VERTEX_POINT('',#76750);
#15242=VERTEX_POINT('',#76751);
#15243=VERTEX_POINT('',#76753);
#15244=VERTEX_POINT('',#76755);
#15245=VERTEX_POINT('',#76759);
#15246=VERTEX_POINT('',#76761);
#15247=VERTEX_POINT('',#76765);
#15248=VERTEX_POINT('',#76767);
#15249=VERTEX_POINT('',#76775);
#15250=VERTEX_POINT('',#76776);
#15251=VERTEX_POINT('',#76778);
#15252=VERTEX_POINT('',#76780);
#15253=VERTEX_POINT('',#76784);
#15254=VERTEX_POINT('',#76786);
#15255=VERTEX_POINT('',#76790);
#15256=VERTEX_POINT('',#76792);
#15257=VERTEX_POINT('',#76800);
#15258=VERTEX_POINT('',#76801);
#15259=VERTEX_POINT('',#76803);
#15260=VERTEX_POINT('',#76805);
#15261=VERTEX_POINT('',#76809);
#15262=VERTEX_POINT('',#76811);
#15263=VERTEX_POINT('',#76815);
#15264=VERTEX_POINT('',#76817);
#15265=VERTEX_POINT('',#76825);
#15266=VERTEX_POINT('',#76826);
#15267=VERTEX_POINT('',#76828);
#15268=VERTEX_POINT('',#76830);
#15269=VERTEX_POINT('',#76834);
#15270=VERTEX_POINT('',#76836);
#15271=VERTEX_POINT('',#76840);
#15272=VERTEX_POINT('',#76842);
#15273=VERTEX_POINT('',#76850);
#15274=VERTEX_POINT('',#76851);
#15275=VERTEX_POINT('',#76853);
#15276=VERTEX_POINT('',#76855);
#15277=VERTEX_POINT('',#76859);
#15278=VERTEX_POINT('',#76861);
#15279=VERTEX_POINT('',#76865);
#15280=VERTEX_POINT('',#76867);
#15281=VERTEX_POINT('',#76875);
#15282=VERTEX_POINT('',#76876);
#15283=VERTEX_POINT('',#76878);
#15284=VERTEX_POINT('',#76880);
#15285=VERTEX_POINT('',#76884);
#15286=VERTEX_POINT('',#76886);
#15287=VERTEX_POINT('',#76890);
#15288=VERTEX_POINT('',#76892);
#15289=VERTEX_POINT('',#76900);
#15290=VERTEX_POINT('',#76901);
#15291=VERTEX_POINT('',#76903);
#15292=VERTEX_POINT('',#76905);
#15293=VERTEX_POINT('',#76909);
#15294=VERTEX_POINT('',#76911);
#15295=VERTEX_POINT('',#76915);
#15296=VERTEX_POINT('',#76917);
#15297=VERTEX_POINT('',#76925);
#15298=VERTEX_POINT('',#76927);
#15299=VERTEX_POINT('',#76931);
#15300=VERTEX_POINT('',#76933);
#15301=VERTEX_POINT('',#76937);
#15302=VERTEX_POINT('',#76938);
#15303=VERTEX_POINT('',#76940);
#15304=VERTEX_POINT('',#76942);
#15305=VERTEX_POINT('',#76946);
#15306=VERTEX_POINT('',#76948);
#15307=VERTEX_POINT('',#76952);
#15308=VERTEX_POINT('',#76954);
#15309=VERTEX_POINT('',#76958);
#15310=VERTEX_POINT('',#76960);
#15311=VERTEX_POINT('',#76964);
#15312=VERTEX_POINT('',#76966);
#15313=VERTEX_POINT('',#76970);
#15314=VERTEX_POINT('',#76972);
#15315=VERTEX_POINT('',#76976);
#15316=VERTEX_POINT('',#76978);
#15317=VERTEX_POINT('',#76988);
#15318=VERTEX_POINT('',#76989);
#15319=VERTEX_POINT('',#76993);
#15320=VERTEX_POINT('',#76995);
#15321=VERTEX_POINT('',#77001);
#15322=VERTEX_POINT('',#77003);
#15323=VERTEX_POINT('',#77005);
#15324=VERTEX_POINT('',#77007);
#15325=VERTEX_POINT('',#77009);
#15326=VERTEX_POINT('',#77011);
#15327=VERTEX_POINT('',#77014);
#15328=VERTEX_POINT('',#77015);
#15329=VERTEX_POINT('',#77017);
#15330=VERTEX_POINT('',#77019);
#15331=VERTEX_POINT('',#77022);
#15332=VERTEX_POINT('',#77023);
#15333=VERTEX_POINT('',#77025);
#15334=VERTEX_POINT('',#77027);
#15335=VERTEX_POINT('',#77031);
#15336=VERTEX_POINT('',#77035);
#15337=VERTEX_POINT('',#77041);
#15338=VERTEX_POINT('',#77043);
#15339=VERTEX_POINT('',#77046);
#15340=VERTEX_POINT('',#77048);
#15341=VERTEX_POINT('',#77051);
#15342=VERTEX_POINT('',#77053);
#15343=VERTEX_POINT('',#77059);
#15344=VERTEX_POINT('',#77064);
#15345=VERTEX_POINT('',#77067);
#15346=VERTEX_POINT('',#77069);
#15347=VERTEX_POINT('',#77071);
#15348=VERTEX_POINT('',#77075);
#15349=VERTEX_POINT('',#77077);
#15350=VERTEX_POINT('',#77079);
#15351=VERTEX_POINT('',#77083);
#15352=VERTEX_POINT('',#77086);
#15353=VERTEX_POINT('',#77091);
#15354=VERTEX_POINT('',#77092);
#15355=VERTEX_POINT('',#77097);
#15356=VERTEX_POINT('',#77098);
#15357=VERTEX_POINT('',#77100);
#15358=VERTEX_POINT('',#77105);
#15359=VERTEX_POINT('',#77111);
#15360=VERTEX_POINT('',#77112);
#15361=VERTEX_POINT('',#77117);
#15362=VERTEX_POINT('',#77118);
#15363=VERTEX_POINT('',#77120);
#15364=VERTEX_POINT('',#77125);
#15365=VERTEX_POINT('',#77131);
#15366=VERTEX_POINT('',#77135);
#15367=VERTEX_POINT('',#77139);
#15368=VERTEX_POINT('',#77143);
#15369=VERTEX_POINT('',#77155);
#15370=VERTEX_POINT('',#77156);
#15371=VERTEX_POINT('',#77158);
#15372=VERTEX_POINT('',#77217);
#15373=VERTEX_POINT('',#77251);
#15374=VERTEX_POINT('',#77252);
#15375=VERTEX_POINT('',#77641);
#15376=VERTEX_POINT('',#77642);
#15377=VERTEX_POINT('',#78040);
#15378=VERTEX_POINT('',#78041);
#15379=VERTEX_POINT('',#78043);
#15380=VERTEX_POINT('',#78228);
#15381=VERTEX_POINT('',#78420);
#15382=VERTEX_POINT('',#78421);
#15383=VERTEX_POINT('',#78423);
#15384=VERTEX_POINT('',#78775);
#15385=VERTEX_POINT('',#78776);
#15386=VERTEX_POINT('',#79141);
#15387=VERTEX_POINT('',#79142);
#15388=VERTEX_POINT('',#79320);
#15389=VERTEX_POINT('',#79500);
#15390=VERTEX_POINT('',#79501);
#15391=VERTEX_POINT('',#79503);
#15392=VERTEX_POINT('',#79692);
#15393=VERTEX_POINT('',#79884);
#15394=VERTEX_POINT('',#79885);
#15395=VERTEX_POINT('',#80254);
#15396=VERTEX_POINT('',#80255);
#15397=VERTEX_POINT('',#80257);
#15398=VERTEX_POINT('',#80388);
#15399=VERTEX_POINT('',#80487);
#15400=VERTEX_POINT('',#80488);
#15401=VERTEX_POINT('',#80833);
#15402=VERTEX_POINT('',#80834);
#15403=VERTEX_POINT('',#81167);
#15404=VERTEX_POINT('',#81168);
#15405=VERTEX_POINT('',#81170);
#15406=VERTEX_POINT('',#81504);
#15407=VERTEX_POINT('',#81505);
#15408=VERTEX_POINT('',#81842);
#15409=VERTEX_POINT('',#81843);
#15410=VERTEX_POINT('',#82192);
#15411=VERTEX_POINT('',#82193);
#15412=VERTEX_POINT('',#82363);
#15413=VERTEX_POINT('',#82541);
#15414=VERTEX_POINT('',#82542);
#15415=VERTEX_POINT('',#82869);
#15416=VERTEX_POINT('',#83026);
#15417=VERTEX_POINT('',#83151);
#15418=VERTEX_POINT('',#83214);
#15419=VERTEX_POINT('',#83257);
#15420=VERTEX_POINT('',#83258);
#15421=VERTEX_POINT('',#83599);
#15422=VERTEX_POINT('',#83690);
#15423=VERTEX_POINT('',#83692);
#15424=VERTEX_POINT('',#84019);
#15425=VERTEX_POINT('',#84020);
#15426=VERTEX_POINT('',#84024);
#15427=VERTEX_POINT('',#84026);
#15428=VERTEX_POINT('',#84030);
#15429=VERTEX_POINT('',#84034);
#15430=VERTEX_POINT('',#84036);
#15431=VERTEX_POINT('',#84040);
#15432=VERTEX_POINT('',#84044);
#15433=VERTEX_POINT('',#84046);
#15434=VERTEX_POINT('',#84050);
#15435=VERTEX_POINT('',#84054);
#15436=VERTEX_POINT('',#84056);
#15437=VERTEX_POINT('',#84060);
#15438=VERTEX_POINT('',#84064);
#15439=VERTEX_POINT('',#84066);
#15440=VERTEX_POINT('',#84070);
#15441=VERTEX_POINT('',#84074);
#15442=VERTEX_POINT('',#84079);
#15443=VERTEX_POINT('',#84083);
#15444=VERTEX_POINT('',#84085);
#15445=VERTEX_POINT('',#84089);
#15446=VERTEX_POINT('',#84091);
#15447=VERTEX_POINT('',#84095);
#15448=VERTEX_POINT('',#84097);
#15449=VERTEX_POINT('',#84101);
#15450=VERTEX_POINT('',#84103);
#15451=VERTEX_POINT('',#84107);
#15452=VERTEX_POINT('',#84109);
#15453=VERTEX_POINT('',#84113);
#15454=VERTEX_POINT('',#84115);
#15455=VERTEX_POINT('',#84120);
#15456=VERTEX_POINT('',#84122);
#15457=VERTEX_POINT('',#84127);
#15458=VERTEX_POINT('',#84132);
#15459=VERTEX_POINT('',#84145);
#15460=VERTEX_POINT('',#84146);
#15461=VERTEX_POINT('',#84162);
#15462=VERTEX_POINT('',#84170);
#15463=VERTEX_POINT('',#84175);
#15464=VERTEX_POINT('',#84181);
#15465=VERTEX_POINT('',#84183);
#15466=VERTEX_POINT('',#84187);
#15467=VERTEX_POINT('',#84189);
#15468=VERTEX_POINT('',#84193);
#15469=VERTEX_POINT('',#84194);
#15470=VERTEX_POINT('',#84196);
#15471=VERTEX_POINT('',#84198);
#15472=VERTEX_POINT('',#84202);
#15473=VERTEX_POINT('',#84205);
#15474=VERTEX_POINT('',#84207);
#15475=VERTEX_POINT('',#84211);
#15476=VERTEX_POINT('',#84213);
#15477=VERTEX_POINT('',#84217);
#15478=VERTEX_POINT('',#84218);
#15479=VERTEX_POINT('',#84220);
#15480=VERTEX_POINT('',#84222);
#15481=VERTEX_POINT('',#84226);
#15482=VERTEX_POINT('',#84229);
#15483=VERTEX_POINT('',#84231);
#15484=VERTEX_POINT('',#84235);
#15485=VERTEX_POINT('',#84237);
#15486=VERTEX_POINT('',#84240);
#15487=VERTEX_POINT('',#84242);
#15488=VERTEX_POINT('',#84245);
#15489=VERTEX_POINT('',#84247);
#15490=VERTEX_POINT('',#84249);
#15491=VERTEX_POINT('',#84251);
#15492=VERTEX_POINT('',#84254);
#15493=VERTEX_POINT('',#84258);
#15494=VERTEX_POINT('',#84262);
#15495=VERTEX_POINT('',#84266);
#15496=VERTEX_POINT('',#84269);
#15497=VERTEX_POINT('',#84272);
#15498=VERTEX_POINT('',#84276);
#15499=VERTEX_POINT('',#84280);
#15500=VERTEX_POINT('',#84284);
#15501=VERTEX_POINT('',#84288);
#15502=VERTEX_POINT('',#84291);
#15503=VERTEX_POINT('',#84294);
#15504=VERTEX_POINT('',#84298);
#15505=VERTEX_POINT('',#84302);
#15506=VERTEX_POINT('',#84304);
#15507=VERTEX_POINT('',#84308);
#15508=VERTEX_POINT('',#84312);
#15509=VERTEX_POINT('',#84314);
#15510=VERTEX_POINT('',#84316);
#15511=VERTEX_POINT('',#84319);
#15512=VERTEX_POINT('',#84336);
#15513=VERTEX_POINT('',#84337);
#15514=VERTEX_POINT('',#84339);
#15515=VERTEX_POINT('',#84410);
#15516=VERTEX_POINT('',#84444);
#15517=VERTEX_POINT('',#84445);
#15518=VERTEX_POINT('',#84870);
#15519=VERTEX_POINT('',#84871);
#15520=VERTEX_POINT('',#85330);
#15521=VERTEX_POINT('',#85331);
#15522=VERTEX_POINT('',#85333);
#15523=VERTEX_POINT('',#85564);
#15524=VERTEX_POINT('',#85820);
#15525=VERTEX_POINT('',#85821);
#15526=VERTEX_POINT('',#86286);
#15527=VERTEX_POINT('',#86287);
#15528=VERTEX_POINT('',#86746);
#15529=VERTEX_POINT('',#86747);
#15530=VERTEX_POINT('',#86749);
#15531=VERTEX_POINT('',#86984);
#15532=VERTEX_POINT('',#87216);
#15533=VERTEX_POINT('',#87217);
#15534=VERTEX_POINT('',#87219);
#15535=VERTEX_POINT('',#87442);
#15536=VERTEX_POINT('',#87700);
#15537=VERTEX_POINT('',#87701);
#15538=VERTEX_POINT('',#88164);
#15539=VERTEX_POINT('',#88165);
#15540=VERTEX_POINT('',#88638);
#15541=VERTEX_POINT('',#88639);
#15542=VERTEX_POINT('',#88641);
#15543=VERTEX_POINT('',#88874);
#15544=VERTEX_POINT('',#89106);
#15545=VERTEX_POINT('',#89107);
#15546=VERTEX_POINT('',#89564);
#15547=VERTEX_POINT('',#89565);
#15548=VERTEX_POINT('',#89567);
#15549=VERTEX_POINT('',#89788);
#15550=VERTEX_POINT('',#90006);
#15551=VERTEX_POINT('',#90007);
#15552=VERTEX_POINT('',#90009);
#15553=VERTEX_POINT('',#90250);
#15554=VERTEX_POINT('',#90482);
#15555=VERTEX_POINT('',#90483);
#15556=VERTEX_POINT('',#90946);
#15557=VERTEX_POINT('',#90947);
#15558=VERTEX_POINT('',#91390);
#15559=VERTEX_POINT('',#91391);
#15560=VERTEX_POINT('',#91393);
#15561=VERTEX_POINT('',#91630);
#15562=VERTEX_POINT('',#91866);
#15563=VERTEX_POINT('',#91867);
#15564=VERTEX_POINT('',#92310);
#15565=VERTEX_POINT('',#92311);
#15566=VERTEX_POINT('',#92784);
#15567=VERTEX_POINT('',#92785);
#15568=VERTEX_POINT('',#92787);
#15569=VERTEX_POINT('',#93044);
#15570=VERTEX_POINT('',#93290);
#15571=VERTEX_POINT('',#93291);
#15572=VERTEX_POINT('',#93760);
#15573=VERTEX_POINT('',#93761);
#15574=VERTEX_POINT('',#94224);
#15575=VERTEX_POINT('',#94225);
#15576=VERTEX_POINT('',#94227);
#15577=VERTEX_POINT('',#94685);
#15578=VERTEX_POINT('',#94686);
#15579=VERTEX_POINT('',#94688);
#15580=VERTEX_POINT('',#94803);
#15581=VERTEX_POINT('',#94888);
#15582=VERTEX_POINT('',#94889);
#15583=VERTEX_POINT('',#95362);
#15584=VERTEX_POINT('',#95363);
#15585=VERTEX_POINT('',#95792);
#15586=VERTEX_POINT('',#95793);
#15587=VERTEX_POINT('',#96220);
#15588=VERTEX_POINT('',#96221);
#15589=VERTEX_POINT('',#96223);
#15590=VERTEX_POINT('',#96663);
#15591=VERTEX_POINT('',#96664);
#15592=VERTEX_POINT('',#96886);
#15593=VERTEX_POINT('',#97104);
#15594=VERTEX_POINT('',#97105);
#15595=VERTEX_POINT('',#97546);
#15596=VERTEX_POINT('',#97547);
#15597=VERTEX_POINT('',#97970);
#15598=VERTEX_POINT('',#97971);
#15599=VERTEX_POINT('',#98396);
#15600=VERTEX_POINT('',#98397);
#15601=VERTEX_POINT('',#98844);
#15602=VERTEX_POINT('',#98845);
#15603=VERTEX_POINT('',#99302);
#15604=VERTEX_POINT('',#99303);
#15605=VERTEX_POINT('',#99728);
#15606=VERTEX_POINT('',#99729);
#15607=VERTEX_POINT('',#100160);
#15608=VERTEX_POINT('',#100161);
#15609=VERTEX_POINT('',#100584);
#15610=VERTEX_POINT('',#100585);
#15611=VERTEX_POINT('',#100587);
#15612=VERTEX_POINT('',#101041);
#15613=VERTEX_POINT('',#101042);
#15614=VERTEX_POINT('',#101459);
#15615=VERTEX_POINT('',#101460);
#15616=VERTEX_POINT('',#101883);
#15617=VERTEX_POINT('',#101884);
#15618=VERTEX_POINT('',#102319);
#15619=VERTEX_POINT('',#102320);
#15620=VERTEX_POINT('',#102737);
#15621=VERTEX_POINT('',#102738);
#15622=VERTEX_POINT('',#103175);
#15623=VERTEX_POINT('',#103176);
#15624=VERTEX_POINT('',#103398);
#15625=VERTEX_POINT('',#103634);
#15626=VERTEX_POINT('',#103635);
#15627=VERTEX_POINT('',#104048);
#15628=VERTEX_POINT('',#104049);
#15629=VERTEX_POINT('',#104514);
#15630=VERTEX_POINT('',#104701);
#15631=VERTEX_POINT('',#104703);
#15632=VERTEX_POINT('',#104834);
#15633=VERTEX_POINT('',#105071);
#15634=VERTEX_POINT('',#105240);
#15635=VERTEX_POINT('',#105241);
#15636=VERTEX_POINT('',#105962);
#15637=VERTEX_POINT('',#105963);
#15638=VERTEX_POINT('',#106656);
#15639=VERTEX_POINT('',#106660);
#15640=VERTEX_POINT('',#106663);
#15641=VERTEX_POINT('',#106668);
#15642=VERTEX_POINT('',#106669);
#15643=VERTEX_POINT('',#106671);
#15644=VERTEX_POINT('',#106675);
#15645=VERTEX_POINT('',#106677);
#15646=VERTEX_POINT('',#106683);
#15647=VERTEX_POINT('',#106689);
#15648=VERTEX_POINT('',#106690);
#15649=VERTEX_POINT('',#106692);
#15650=VERTEX_POINT('',#106694);
#15651=VERTEX_POINT('',#106697);
#15652=VERTEX_POINT('',#106699);
#15653=VERTEX_POINT('',#106701);
#15654=VERTEX_POINT('',#106703);
#15655=VERTEX_POINT('',#106705);
#15656=VERTEX_POINT('',#106707);
#15657=VERTEX_POINT('',#106709);
#15658=VERTEX_POINT('',#106711);
#15659=VERTEX_POINT('',#106713);
#15660=VERTEX_POINT('',#106715);
#15661=VERTEX_POINT('',#106717);
#15662=VERTEX_POINT('',#106719);
#15663=VERTEX_POINT('',#106721);
#15664=VERTEX_POINT('',#106723);
#15665=VERTEX_POINT('',#106725);
#15666=VERTEX_POINT('',#106727);
#15667=VERTEX_POINT('',#106729);
#15668=VERTEX_POINT('',#106731);
#15669=VERTEX_POINT('',#106733);
#15670=VERTEX_POINT('',#106735);
#15671=VERTEX_POINT('',#106737);
#15672=VERTEX_POINT('',#106739);
#15673=VERTEX_POINT('',#106741);
#15674=VERTEX_POINT('',#106743);
#15675=VERTEX_POINT('',#106745);
#15676=VERTEX_POINT('',#106747);
#15677=VERTEX_POINT('',#106749);
#15678=VERTEX_POINT('',#106751);
#15679=VERTEX_POINT('',#106753);
#15680=VERTEX_POINT('',#106755);
#15681=VERTEX_POINT('',#106757);
#15682=VERTEX_POINT('',#106759);
#15683=VERTEX_POINT('',#106761);
#15684=VERTEX_POINT('',#106763);
#15685=VERTEX_POINT('',#106765);
#15686=VERTEX_POINT('',#106767);
#15687=VERTEX_POINT('',#106769);
#15688=VERTEX_POINT('',#106771);
#15689=VERTEX_POINT('',#106773);
#15690=VERTEX_POINT('',#106775);
#15691=VERTEX_POINT('',#106777);
#15692=VERTEX_POINT('',#106779);
#15693=VERTEX_POINT('',#106781);
#15694=VERTEX_POINT('',#106783);
#15695=VERTEX_POINT('',#106785);
#15696=VERTEX_POINT('',#106787);
#15697=VERTEX_POINT('',#106789);
#15698=VERTEX_POINT('',#106791);
#15699=VERTEX_POINT('',#106793);
#15700=VERTEX_POINT('',#106795);
#15701=VERTEX_POINT('',#106797);
#15702=VERTEX_POINT('',#106799);
#15703=VERTEX_POINT('',#106801);
#15704=VERTEX_POINT('',#106803);
#15705=VERTEX_POINT('',#106805);
#15706=VERTEX_POINT('',#106807);
#15707=VERTEX_POINT('',#106809);
#15708=VERTEX_POINT('',#106811);
#15709=VERTEX_POINT('',#106813);
#15710=VERTEX_POINT('',#106815);
#15711=VERTEX_POINT('',#106817);
#15712=VERTEX_POINT('',#106819);
#15713=VERTEX_POINT('',#106821);
#15714=VERTEX_POINT('',#106823);
#15715=VERTEX_POINT('',#106825);
#15716=VERTEX_POINT('',#106827);
#15717=VERTEX_POINT('',#106830);
#15718=VERTEX_POINT('',#106832);
#15719=VERTEX_POINT('',#106834);
#15720=VERTEX_POINT('',#106836);
#15721=VERTEX_POINT('',#106838);
#15722=VERTEX_POINT('',#106840);
#15723=VERTEX_POINT('',#106842);
#15724=VERTEX_POINT('',#106844);
#15725=VERTEX_POINT('',#106846);
#15726=VERTEX_POINT('',#106848);
#15727=VERTEX_POINT('',#106850);
#15728=VERTEX_POINT('',#106852);
#15729=VERTEX_POINT('',#106854);
#15730=VERTEX_POINT('',#106856);
#15731=VERTEX_POINT('',#106858);
#15732=VERTEX_POINT('',#106860);
#15733=VERTEX_POINT('',#106862);
#15734=VERTEX_POINT('',#106864);
#15735=VERTEX_POINT('',#106866);
#15736=VERTEX_POINT('',#106868);
#15737=VERTEX_POINT('',#106870);
#15738=VERTEX_POINT('',#106872);
#15739=VERTEX_POINT('',#106874);
#15740=VERTEX_POINT('',#106876);
#15741=VERTEX_POINT('',#106878);
#15742=VERTEX_POINT('',#106880);
#15743=VERTEX_POINT('',#106882);
#15744=VERTEX_POINT('',#106884);
#15745=VERTEX_POINT('',#106886);
#15746=VERTEX_POINT('',#106888);
#15747=VERTEX_POINT('',#106890);
#15748=VERTEX_POINT('',#106892);
#15749=VERTEX_POINT('',#106894);
#15750=VERTEX_POINT('',#106896);
#15751=VERTEX_POINT('',#106898);
#15752=VERTEX_POINT('',#106900);
#15753=VERTEX_POINT('',#106902);
#15754=VERTEX_POINT('',#106904);
#15755=VERTEX_POINT('',#106906);
#15756=VERTEX_POINT('',#106908);
#15757=VERTEX_POINT('',#106910);
#15758=VERTEX_POINT('',#106912);
#15759=VERTEX_POINT('',#106914);
#15760=VERTEX_POINT('',#106916);
#15761=VERTEX_POINT('',#106918);
#15762=VERTEX_POINT('',#106920);
#15763=VERTEX_POINT('',#106922);
#15764=VERTEX_POINT('',#106924);
#15765=VERTEX_POINT('',#106926);
#15766=VERTEX_POINT('',#106928);
#15767=VERTEX_POINT('',#106930);
#15768=VERTEX_POINT('',#106932);
#15769=VERTEX_POINT('',#106934);
#15770=VERTEX_POINT('',#106936);
#15771=VERTEX_POINT('',#106938);
#15772=VERTEX_POINT('',#106940);
#15773=VERTEX_POINT('',#106942);
#15774=VERTEX_POINT('',#106944);
#15775=VERTEX_POINT('',#106946);
#15776=VERTEX_POINT('',#106948);
#15777=VERTEX_POINT('',#106950);
#15778=VERTEX_POINT('',#106952);
#15779=VERTEX_POINT('',#106954);
#15780=VERTEX_POINT('',#106956);
#15781=VERTEX_POINT('',#106958);
#15782=VERTEX_POINT('',#106960);
#15783=VERTEX_POINT('',#106962);
#15784=VERTEX_POINT('',#106964);
#15785=VERTEX_POINT('',#106966);
#15786=VERTEX_POINT('',#106968);
#15787=VERTEX_POINT('',#106970);
#15788=VERTEX_POINT('',#106972);
#15789=VERTEX_POINT('',#106974);
#15790=VERTEX_POINT('',#106978);
#15791=VERTEX_POINT('',#106980);
#15792=VERTEX_POINT('',#106992);
#15793=VERTEX_POINT('',#106996);
#15794=VERTEX_POINT('',#107003);
#15795=VERTEX_POINT('',#107010);
#15796=VERTEX_POINT('',#107017);
#15797=VERTEX_POINT('',#107024);
#15798=VERTEX_POINT('',#107031);
#15799=VERTEX_POINT('',#107038);
#15800=VERTEX_POINT('',#107045);
#15801=VERTEX_POINT('',#107052);
#15802=VERTEX_POINT('',#107059);
#15803=VERTEX_POINT('',#107066);
#15804=VERTEX_POINT('',#107073);
#15805=VERTEX_POINT('',#107080);
#15806=VERTEX_POINT('',#107087);
#15807=VERTEX_POINT('',#107094);
#15808=VERTEX_POINT('',#107101);
#15809=VERTEX_POINT('',#107108);
#15810=VERTEX_POINT('',#107115);
#15811=VERTEX_POINT('',#107122);
#15812=VERTEX_POINT('',#107129);
#15813=VERTEX_POINT('',#107136);
#15814=VERTEX_POINT('',#107143);
#15815=VERTEX_POINT('',#107150);
#15816=VERTEX_POINT('',#107157);
#15817=VERTEX_POINT('',#107164);
#15818=VERTEX_POINT('',#107171);
#15819=VERTEX_POINT('',#107178);
#15820=VERTEX_POINT('',#107185);
#15821=VERTEX_POINT('',#107192);
#15822=VERTEX_POINT('',#107199);
#15823=VERTEX_POINT('',#107206);
#15824=VERTEX_POINT('',#107213);
#15825=VERTEX_POINT('',#107220);
#15826=VERTEX_POINT('',#107230);
#15827=VERTEX_POINT('',#107234);
#15828=VERTEX_POINT('',#107241);
#15829=VERTEX_POINT('',#107248);
#15830=VERTEX_POINT('',#107255);
#15831=VERTEX_POINT('',#107262);
#15832=VERTEX_POINT('',#107269);
#15833=VERTEX_POINT('',#107276);
#15834=VERTEX_POINT('',#107283);
#15835=VERTEX_POINT('',#107290);
#15836=VERTEX_POINT('',#107297);
#15837=VERTEX_POINT('',#107304);
#15838=VERTEX_POINT('',#107311);
#15839=VERTEX_POINT('',#107318);
#15840=VERTEX_POINT('',#107325);
#15841=VERTEX_POINT('',#107332);
#15842=VERTEX_POINT('',#107339);
#15843=VERTEX_POINT('',#107346);
#15844=VERTEX_POINT('',#107353);
#15845=VERTEX_POINT('',#107360);
#15846=VERTEX_POINT('',#107367);
#15847=VERTEX_POINT('',#107374);
#15848=VERTEX_POINT('',#107381);
#15849=VERTEX_POINT('',#107388);
#15850=VERTEX_POINT('',#107395);
#15851=VERTEX_POINT('',#107402);
#15852=VERTEX_POINT('',#107409);
#15853=VERTEX_POINT('',#107416);
#15854=VERTEX_POINT('',#107423);
#15855=VERTEX_POINT('',#107430);
#15856=VERTEX_POINT('',#107437);
#15857=VERTEX_POINT('',#107444);
#15858=VERTEX_POINT('',#107451);
#15859=VERTEX_POINT('',#107458);
#15860=VERTEX_POINT('',#107465);
#15861=VERTEX_POINT('',#107474);
#15862=VERTEX_POINT('',#107477);
#15863=VERTEX_POINT('',#107478);
#15864=VERTEX_POINT('',#107482);
#15865=VERTEX_POINT('',#107484);
#15866=VERTEX_POINT('',#107488);
#15867=VERTEX_POINT('',#107492);
#15868=VERTEX_POINT('',#107494);
#15869=VERTEX_POINT('',#107498);
#15870=VERTEX_POINT('',#107502);
#15871=VERTEX_POINT('',#107504);
#15872=VERTEX_POINT('',#107508);
#15873=VERTEX_POINT('',#107512);
#15874=VERTEX_POINT('',#107514);
#15875=VERTEX_POINT('',#107518);
#15876=VERTEX_POINT('',#107522);
#15877=VERTEX_POINT('',#107524);
#15878=VERTEX_POINT('',#107528);
#15879=VERTEX_POINT('',#107532);
#15880=VERTEX_POINT('',#107539);
#15881=VERTEX_POINT('',#107541);
#15882=VERTEX_POINT('',#107545);
#15883=VERTEX_POINT('',#107547);
#15884=VERTEX_POINT('',#107551);
#15885=VERTEX_POINT('',#107553);
#15886=VERTEX_POINT('',#107557);
#15887=VERTEX_POINT('',#107559);
#15888=VERTEX_POINT('',#107563);
#15889=VERTEX_POINT('',#107565);
#15890=VERTEX_POINT('',#107569);
#15891=VERTEX_POINT('',#107571);
#15892=VERTEX_POINT('',#107576);
#15893=VERTEX_POINT('',#107578);
#15894=VERTEX_POINT('',#107583);
#15895=VERTEX_POINT('',#107588);
#15896=VERTEX_POINT('',#107601);
#15897=VERTEX_POINT('',#107602);
#15898=VERTEX_POINT('',#107618);
#15899=VERTEX_POINT('',#107627);
#15900=VERTEX_POINT('',#107628);
#15901=VERTEX_POINT('',#107630);
#15902=VERTEX_POINT('',#107757);
#15903=VERTEX_POINT('',#107791);
#15904=VERTEX_POINT('',#107792);
#15905=VERTEX_POINT('',#108211);
#15906=VERTEX_POINT('',#108212);
#15907=VERTEX_POINT('',#108663);
#15908=VERTEX_POINT('',#108664);
#15909=VERTEX_POINT('',#108894);
#15910=VERTEX_POINT('',#109117);
#15911=VERTEX_POINT('',#109118);
#15912=VERTEX_POINT('',#109551);
#15913=VERTEX_POINT('',#109552);
#15914=VERTEX_POINT('',#109987);
#15915=VERTEX_POINT('',#109988);
#15916=VERTEX_POINT('',#109990);
#15917=VERTEX_POINT('',#110496);
#15918=VERTEX_POINT('',#110497);
#15919=VERTEX_POINT('',#110944);
#15920=VERTEX_POINT('',#110945);
#15921=VERTEX_POINT('',#111390);
#15922=VERTEX_POINT('',#111391);
#15923=VERTEX_POINT('',#111623);
#15924=VERTEX_POINT('',#111847);
#15925=VERTEX_POINT('',#111848);
#15926=VERTEX_POINT('',#112307);
#15927=VERTEX_POINT('',#112308);
#15928=VERTEX_POINT('',#112759);
#15929=VERTEX_POINT('',#112760);
#15930=VERTEX_POINT('',#113255);
#15931=VERTEX_POINT('',#113256);
#15932=VERTEX_POINT('',#113689);
#15933=VERTEX_POINT('',#113690);
#15934=VERTEX_POINT('',#114149);
#15935=VERTEX_POINT('',#114150);
#15936=VERTEX_POINT('',#114152);
#15937=VERTEX_POINT('',#114546);
#15938=VERTEX_POINT('',#114547);
#15939=VERTEX_POINT('',#114988);
#15940=VERTEX_POINT('',#114989);
#15941=VERTEX_POINT('',#115430);
#15942=VERTEX_POINT('',#115431);
#15943=VERTEX_POINT('',#115830);
#15944=VERTEX_POINT('',#115831);
#15945=VERTEX_POINT('',#115833);
#15946=VERTEX_POINT('',#115962);
#15947=VERTEX_POINT('',#116050);
#15948=VERTEX_POINT('',#116051);
#15949=VERTEX_POINT('',#116053);
#15950=VERTEX_POINT('',#116527);
#15951=VERTEX_POINT('',#116528);
#15952=VERTEX_POINT('',#116945);
#15953=VERTEX_POINT('',#116946);
#15954=VERTEX_POINT('',#117359);
#15955=VERTEX_POINT('',#117360);
#15956=VERTEX_POINT('',#117833);
#15957=VERTEX_POINT('',#117834);
#15958=VERTEX_POINT('',#117836);
#15959=VERTEX_POINT('',#118268);
#15960=VERTEX_POINT('',#118269);
#15961=VERTEX_POINT('',#118698);
#15962=VERTEX_POINT('',#118699);
#15963=VERTEX_POINT('',#119138);
#15964=VERTEX_POINT('',#119139);
#15965=VERTEX_POINT('',#119568);
#15966=VERTEX_POINT('',#119569);
#15967=VERTEX_POINT('',#120078);
#15968=VERTEX_POINT('',#120079);
#15969=VERTEX_POINT('',#120510);
#15970=VERTEX_POINT('',#120511);
#15971=VERTEX_POINT('',#120928);
#15972=VERTEX_POINT('',#120929);
#15973=VERTEX_POINT('',#121374);
#15974=VERTEX_POINT('',#121375);
#15975=VERTEX_POINT('',#121840);
#15976=VERTEX_POINT('',#121841);
#15977=VERTEX_POINT('',#121843);
#15978=VERTEX_POINT('',#122267);
#15979=VERTEX_POINT('',#122268);
#15980=VERTEX_POINT('',#122691);
#15981=VERTEX_POINT('',#122692);
#15982=VERTEX_POINT('',#123119);
#15983=VERTEX_POINT('',#123120);
#15984=VERTEX_POINT('',#123324);
#15985=VERTEX_POINT('',#123560);
#15986=VERTEX_POINT('',#123561);
#15987=VERTEX_POINT('',#123982);
#15988=VERTEX_POINT('',#124173);
#15989=VERTEX_POINT('',#124175);
#15990=VERTEX_POINT('',#124302);
#15991=VERTEX_POINT('',#124499);
#15992=VERTEX_POINT('',#124638);
#15993=VERTEX_POINT('',#124639);
#15994=VERTEX_POINT('',#125248);
#15995=VERTEX_POINT('',#125339);
#15996=VERTEX_POINT('',#125340);
#15997=VERTEX_POINT('',#125936);
#15998=VERTEX_POINT('',#125940);
#15999=VERTEX_POINT('',#125943);
#16000=VERTEX_POINT('',#125948);
#16001=VERTEX_POINT('',#125949);
#16002=VERTEX_POINT('',#125951);
#16003=VERTEX_POINT('',#125955);
#16004=VERTEX_POINT('',#125957);
#16005=VERTEX_POINT('',#125963);
#16006=VERTEX_POINT('',#125969);
#16007=VERTEX_POINT('',#125970);
#16008=VERTEX_POINT('',#125972);
#16009=VERTEX_POINT('',#125974);
#16010=VERTEX_POINT('',#125977);
#16011=VERTEX_POINT('',#125979);
#16012=VERTEX_POINT('',#125981);
#16013=VERTEX_POINT('',#125983);
#16014=VERTEX_POINT('',#125985);
#16015=VERTEX_POINT('',#125987);
#16016=VERTEX_POINT('',#125989);
#16017=VERTEX_POINT('',#125991);
#16018=VERTEX_POINT('',#125993);
#16019=VERTEX_POINT('',#125995);
#16020=VERTEX_POINT('',#125997);
#16021=VERTEX_POINT('',#125999);
#16022=VERTEX_POINT('',#126001);
#16023=VERTEX_POINT('',#126003);
#16024=VERTEX_POINT('',#126005);
#16025=VERTEX_POINT('',#126007);
#16026=VERTEX_POINT('',#126009);
#16027=VERTEX_POINT('',#126011);
#16028=VERTEX_POINT('',#126013);
#16029=VERTEX_POINT('',#126015);
#16030=VERTEX_POINT('',#126017);
#16031=VERTEX_POINT('',#126019);
#16032=VERTEX_POINT('',#126021);
#16033=VERTEX_POINT('',#126023);
#16034=VERTEX_POINT('',#126025);
#16035=VERTEX_POINT('',#126027);
#16036=VERTEX_POINT('',#126029);
#16037=VERTEX_POINT('',#126031);
#16038=VERTEX_POINT('',#126033);
#16039=VERTEX_POINT('',#126035);
#16040=VERTEX_POINT('',#126037);
#16041=VERTEX_POINT('',#126039);
#16042=VERTEX_POINT('',#126041);
#16043=VERTEX_POINT('',#126043);
#16044=VERTEX_POINT('',#126045);
#16045=VERTEX_POINT('',#126047);
#16046=VERTEX_POINT('',#126049);
#16047=VERTEX_POINT('',#126051);
#16048=VERTEX_POINT('',#126053);
#16049=VERTEX_POINT('',#126055);
#16050=VERTEX_POINT('',#126057);
#16051=VERTEX_POINT('',#126059);
#16052=VERTEX_POINT('',#126061);
#16053=VERTEX_POINT('',#126063);
#16054=VERTEX_POINT('',#126065);
#16055=VERTEX_POINT('',#126067);
#16056=VERTEX_POINT('',#126069);
#16057=VERTEX_POINT('',#126071);
#16058=VERTEX_POINT('',#126073);
#16059=VERTEX_POINT('',#126075);
#16060=VERTEX_POINT('',#126077);
#16061=VERTEX_POINT('',#126079);
#16062=VERTEX_POINT('',#126081);
#16063=VERTEX_POINT('',#126083);
#16064=VERTEX_POINT('',#126085);
#16065=VERTEX_POINT('',#126087);
#16066=VERTEX_POINT('',#126089);
#16067=VERTEX_POINT('',#126091);
#16068=VERTEX_POINT('',#126093);
#16069=VERTEX_POINT('',#126095);
#16070=VERTEX_POINT('',#126097);
#16071=VERTEX_POINT('',#126099);
#16072=VERTEX_POINT('',#126101);
#16073=VERTEX_POINT('',#126103);
#16074=VERTEX_POINT('',#126105);
#16075=VERTEX_POINT('',#126107);
#16076=VERTEX_POINT('',#126110);
#16077=VERTEX_POINT('',#126112);
#16078=VERTEX_POINT('',#126114);
#16079=VERTEX_POINT('',#126116);
#16080=VERTEX_POINT('',#126118);
#16081=VERTEX_POINT('',#126120);
#16082=VERTEX_POINT('',#126122);
#16083=VERTEX_POINT('',#126124);
#16084=VERTEX_POINT('',#126126);
#16085=VERTEX_POINT('',#126128);
#16086=VERTEX_POINT('',#126130);
#16087=VERTEX_POINT('',#126132);
#16088=VERTEX_POINT('',#126134);
#16089=VERTEX_POINT('',#126136);
#16090=VERTEX_POINT('',#126138);
#16091=VERTEX_POINT('',#126140);
#16092=VERTEX_POINT('',#126142);
#16093=VERTEX_POINT('',#126144);
#16094=VERTEX_POINT('',#126146);
#16095=VERTEX_POINT('',#126148);
#16096=VERTEX_POINT('',#126150);
#16097=VERTEX_POINT('',#126152);
#16098=VERTEX_POINT('',#126154);
#16099=VERTEX_POINT('',#126156);
#16100=VERTEX_POINT('',#126158);
#16101=VERTEX_POINT('',#126160);
#16102=VERTEX_POINT('',#126162);
#16103=VERTEX_POINT('',#126164);
#16104=VERTEX_POINT('',#126166);
#16105=VERTEX_POINT('',#126168);
#16106=VERTEX_POINT('',#126170);
#16107=VERTEX_POINT('',#126172);
#16108=VERTEX_POINT('',#126174);
#16109=VERTEX_POINT('',#126176);
#16110=VERTEX_POINT('',#126178);
#16111=VERTEX_POINT('',#126180);
#16112=VERTEX_POINT('',#126182);
#16113=VERTEX_POINT('',#126184);
#16114=VERTEX_POINT('',#126186);
#16115=VERTEX_POINT('',#126188);
#16116=VERTEX_POINT('',#126190);
#16117=VERTEX_POINT('',#126192);
#16118=VERTEX_POINT('',#126194);
#16119=VERTEX_POINT('',#126196);
#16120=VERTEX_POINT('',#126198);
#16121=VERTEX_POINT('',#126200);
#16122=VERTEX_POINT('',#126202);
#16123=VERTEX_POINT('',#126204);
#16124=VERTEX_POINT('',#126206);
#16125=VERTEX_POINT('',#126208);
#16126=VERTEX_POINT('',#126210);
#16127=VERTEX_POINT('',#126212);
#16128=VERTEX_POINT('',#126214);
#16129=VERTEX_POINT('',#126216);
#16130=VERTEX_POINT('',#126218);
#16131=VERTEX_POINT('',#126220);
#16132=VERTEX_POINT('',#126222);
#16133=VERTEX_POINT('',#126224);
#16134=VERTEX_POINT('',#126226);
#16135=VERTEX_POINT('',#126228);
#16136=VERTEX_POINT('',#126230);
#16137=VERTEX_POINT('',#126232);
#16138=VERTEX_POINT('',#126234);
#16139=VERTEX_POINT('',#126236);
#16140=VERTEX_POINT('',#126238);
#16141=VERTEX_POINT('',#126240);
#16142=VERTEX_POINT('',#126242);
#16143=VERTEX_POINT('',#126244);
#16144=VERTEX_POINT('',#126246);
#16145=VERTEX_POINT('',#126248);
#16146=VERTEX_POINT('',#126250);
#16147=VERTEX_POINT('',#126252);
#16148=VERTEX_POINT('',#126254);
#16149=VERTEX_POINT('',#126258);
#16150=VERTEX_POINT('',#126260);
#16151=VERTEX_POINT('',#126272);
#16152=VERTEX_POINT('',#126276);
#16153=VERTEX_POINT('',#126283);
#16154=VERTEX_POINT('',#126290);
#16155=VERTEX_POINT('',#126297);
#16156=VERTEX_POINT('',#126304);
#16157=VERTEX_POINT('',#126311);
#16158=VERTEX_POINT('',#126318);
#16159=VERTEX_POINT('',#126325);
#16160=VERTEX_POINT('',#126332);
#16161=VERTEX_POINT('',#126339);
#16162=VERTEX_POINT('',#126346);
#16163=VERTEX_POINT('',#126353);
#16164=VERTEX_POINT('',#126360);
#16165=VERTEX_POINT('',#126367);
#16166=VERTEX_POINT('',#126374);
#16167=VERTEX_POINT('',#126381);
#16168=VERTEX_POINT('',#126388);
#16169=VERTEX_POINT('',#126395);
#16170=VERTEX_POINT('',#126402);
#16171=VERTEX_POINT('',#126409);
#16172=VERTEX_POINT('',#126416);
#16173=VERTEX_POINT('',#126423);
#16174=VERTEX_POINT('',#126430);
#16175=VERTEX_POINT('',#126437);
#16176=VERTEX_POINT('',#126444);
#16177=VERTEX_POINT('',#126451);
#16178=VERTEX_POINT('',#126458);
#16179=VERTEX_POINT('',#126465);
#16180=VERTEX_POINT('',#126472);
#16181=VERTEX_POINT('',#126479);
#16182=VERTEX_POINT('',#126486);
#16183=VERTEX_POINT('',#126493);
#16184=VERTEX_POINT('',#126500);
#16185=VERTEX_POINT('',#126510);
#16186=VERTEX_POINT('',#126514);
#16187=VERTEX_POINT('',#126521);
#16188=VERTEX_POINT('',#126528);
#16189=VERTEX_POINT('',#126535);
#16190=VERTEX_POINT('',#126542);
#16191=VERTEX_POINT('',#126549);
#16192=VERTEX_POINT('',#126556);
#16193=VERTEX_POINT('',#126563);
#16194=VERTEX_POINT('',#126570);
#16195=VERTEX_POINT('',#126577);
#16196=VERTEX_POINT('',#126584);
#16197=VERTEX_POINT('',#126591);
#16198=VERTEX_POINT('',#126598);
#16199=VERTEX_POINT('',#126605);
#16200=VERTEX_POINT('',#126612);
#16201=VERTEX_POINT('',#126619);
#16202=VERTEX_POINT('',#126626);
#16203=VERTEX_POINT('',#126633);
#16204=VERTEX_POINT('',#126640);
#16205=VERTEX_POINT('',#126647);
#16206=VERTEX_POINT('',#126654);
#16207=VERTEX_POINT('',#126661);
#16208=VERTEX_POINT('',#126668);
#16209=VERTEX_POINT('',#126675);
#16210=VERTEX_POINT('',#126682);
#16211=VERTEX_POINT('',#126689);
#16212=VERTEX_POINT('',#126696);
#16213=VERTEX_POINT('',#126703);
#16214=VERTEX_POINT('',#126710);
#16215=VERTEX_POINT('',#126717);
#16216=VERTEX_POINT('',#126724);
#16217=VERTEX_POINT('',#126731);
#16218=VERTEX_POINT('',#126738);
#16219=VERTEX_POINT('',#126745);
#16220=VERTEX_POINT('',#126754);
#16221=VERTEX_POINT('',#126757);
#16222=VERTEX_POINT('',#126758);
#16223=VERTEX_POINT('',#126762);
#16224=VERTEX_POINT('',#126764);
#16225=VERTEX_POINT('',#126768);
#16226=VERTEX_POINT('',#126772);
#16227=VERTEX_POINT('',#126774);
#16228=VERTEX_POINT('',#126778);
#16229=VERTEX_POINT('',#126782);
#16230=VERTEX_POINT('',#126784);
#16231=VERTEX_POINT('',#126788);
#16232=VERTEX_POINT('',#126792);
#16233=VERTEX_POINT('',#126794);
#16234=VERTEX_POINT('',#126798);
#16235=VERTEX_POINT('',#126802);
#16236=VERTEX_POINT('',#126804);
#16237=VERTEX_POINT('',#126808);
#16238=VERTEX_POINT('',#126812);
#16239=VERTEX_POINT('',#126819);
#16240=VERTEX_POINT('',#126821);
#16241=VERTEX_POINT('',#126825);
#16242=VERTEX_POINT('',#126827);
#16243=VERTEX_POINT('',#126831);
#16244=VERTEX_POINT('',#126833);
#16245=VERTEX_POINT('',#126837);
#16246=VERTEX_POINT('',#126839);
#16247=VERTEX_POINT('',#126843);
#16248=VERTEX_POINT('',#126845);
#16249=VERTEX_POINT('',#126849);
#16250=VERTEX_POINT('',#126851);
#16251=VERTEX_POINT('',#126856);
#16252=VERTEX_POINT('',#126858);
#16253=VERTEX_POINT('',#126863);
#16254=VERTEX_POINT('',#126868);
#16255=VERTEX_POINT('',#126881);
#16256=VERTEX_POINT('',#126882);
#16257=VERTEX_POINT('',#126898);
#16258=VERTEX_POINT('',#126907);
#16259=VERTEX_POINT('',#126908);
#16260=VERTEX_POINT('',#126910);
#16261=VERTEX_POINT('',#126963);
#16262=VERTEX_POINT('',#126994);
#16263=VERTEX_POINT('',#126995);
#16264=VERTEX_POINT('',#127367);
#16265=VERTEX_POINT('',#127368);
#16266=VERTEX_POINT('',#127729);
#16267=VERTEX_POINT('',#127730);
#16268=VERTEX_POINT('',#128101);
#16269=VERTEX_POINT('',#128102);
#16270=VERTEX_POINT('',#128437);
#16271=VERTEX_POINT('',#128438);
#16272=VERTEX_POINT('',#128793);
#16273=VERTEX_POINT('',#128794);
#16274=VERTEX_POINT('',#129161);
#16275=VERTEX_POINT('',#129162);
#16276=VERTEX_POINT('',#129517);
#16277=VERTEX_POINT('',#129518);
#16278=VERTEX_POINT('',#129869);
#16279=VERTEX_POINT('',#129870);
#16280=VERTEX_POINT('',#130209);
#16281=VERTEX_POINT('',#130210);
#16282=VERTEX_POINT('',#130585);
#16283=VERTEX_POINT('',#130586);
#16284=VERTEX_POINT('',#130588);
#16285=VERTEX_POINT('',#130629);
#16286=VERTEX_POINT('',#130640);
#16287=VERTEX_POINT('',#130641);
#16288=VERTEX_POINT('',#130809);
#16289=VERTEX_POINT('',#131005);
#16290=VERTEX_POINT('',#131006);
#16291=VERTEX_POINT('',#131178);
#16292=VERTEX_POINT('',#131374);
#16293=VERTEX_POINT('',#131375);
#16294=VERTEX_POINT('',#131545);
#16295=VERTEX_POINT('',#131743);
#16296=VERTEX_POINT('',#131744);
#16297=VERTEX_POINT('',#131908);
#16298=VERTEX_POINT('',#132098);
#16299=VERTEX_POINT('',#132099);
#16300=VERTEX_POINT('',#132269);
#16301=VERTEX_POINT('',#132462);
#16302=VERTEX_POINT('',#132463);
#16303=VERTEX_POINT('',#132643);
#16304=VERTEX_POINT('',#132841);
#16305=VERTEX_POINT('',#132842);
#16306=VERTEX_POINT('',#133012);
#16307=VERTEX_POINT('',#133214);
#16308=VERTEX_POINT('',#133215);
#16309=VERTEX_POINT('',#133379);
#16310=VERTEX_POINT('',#133577);
#16311=VERTEX_POINT('',#133578);
#16312=VERTEX_POINT('',#133754);
#16313=VERTEX_POINT('',#133945);
#16314=VERTEX_POINT('',#133962);
#16315=VERTEX_POINT('',#134129);
#16316=VERTEX_POINT('',#134131);
#16317=VERTEX_POINT('',#134289);
#16318=VERTEX_POINT('',#134348);
#16319=VERTEX_POINT('',#134672);
#16320=VERTEX_POINT('',#134699);
#16321=VERTEX_POINT('',#134795);
#16322=VERTEX_POINT('',#134797);
#16323=VERTEX_POINT('',#135172);
#16324=VERTEX_POINT('',#135176);
#16325=VERTEX_POINT('',#135179);
#16326=VERTEX_POINT('',#135180);
#16327=VERTEX_POINT('',#135182);
#16328=VERTEX_POINT('',#135184);
#16329=VERTEX_POINT('',#135186);
#16330=VERTEX_POINT('',#135190);
#16331=VERTEX_POINT('',#135192);
#16332=VERTEX_POINT('',#135194);
#16333=VERTEX_POINT('',#135198);
#16334=VERTEX_POINT('',#135204);
#16335=VERTEX_POINT('',#135206);
#16336=VERTEX_POINT('',#135210);
#16337=VERTEX_POINT('',#135212);
#16338=VERTEX_POINT('',#135227);
#16339=EDGE_CURVE('',#13244,#13244,#12744,.T.);
#16340=EDGE_CURVE('',#13244,#13245,#7070,.T.);
#16341=EDGE_CURVE('',#13245,#13245,#12745,.T.);
#16342=EDGE_CURVE('',#13246,#13247,#7071,.T.);
#16343=EDGE_CURVE('',#13246,#13248,#7072,.T.);
#16344=EDGE_CURVE('',#13248,#13249,#7073,.T.);
#16345=EDGE_CURVE('',#13249,#13250,#7074,.T.);
#16346=EDGE_CURVE('',#13250,#13251,#7075,.T.);
#16347=EDGE_CURVE('',#13251,#13252,#7076,.T.);
#16348=EDGE_CURVE('',#13253,#13252,#7077,.T.);
#16349=EDGE_CURVE('',#13253,#13254,#7078,.T.);
#16350=EDGE_CURVE('',#13255,#13254,#7079,.T.);
#16351=EDGE_CURVE('',#13255,#13256,#7080,.T.);
#16352=EDGE_CURVE('',#13257,#13256,#7081,.T.);
#16353=EDGE_CURVE('',#13257,#13258,#7082,.T.);
#16354=EDGE_CURVE('',#13259,#13258,#7083,.T.);
#16355=EDGE_CURVE('',#13259,#13260,#7084,.T.);
#16356=EDGE_CURVE('',#13261,#13260,#7085,.T.);
#16357=EDGE_CURVE('',#13261,#13247,#7086,.T.);
#16358=EDGE_CURVE('',#13262,#13262,#12746,.T.);
#16359=EDGE_CURVE('',#13244,#13263,#7087,.T.);
#16360=EDGE_CURVE('',#13263,#13263,#12747,.T.);
#16361=EDGE_CURVE('',#13264,#13264,#12748,.T.);
#16362=EDGE_CURVE('',#13264,#13262,#7088,.T.);
#16363=EDGE_CURVE('',#13264,#13265,#7089,.T.);
#16364=EDGE_CURVE('',#13265,#13265,#12749,.T.);
#16365=EDGE_CURVE('',#13266,#13263,#7090,.T.);
#16366=EDGE_CURVE('',#13267,#13265,#7091,.T.);
#16367=EDGE_CURVE('',#13268,#13268,#12750,.T.);
#16368=EDGE_CURVE('',#13268,#13269,#7092,.T.);
#16369=EDGE_CURVE('',#13269,#13269,#12751,.T.);
#16370=EDGE_CURVE('',#13270,#13271,#7093,.T.);
#16371=EDGE_CURVE('',#13270,#13272,#7094,.T.);
#16372=EDGE_CURVE('',#13273,#13272,#7095,.T.);
#16373=EDGE_CURVE('',#13273,#13274,#7096,.T.);
#16374=EDGE_CURVE('',#13275,#13274,#7097,.T.);
#16375=EDGE_CURVE('',#13275,#13276,#7098,.T.);
#16376=EDGE_CURVE('',#13277,#13276,#7099,.T.);
#16377=EDGE_CURVE('',#13277,#13278,#7100,.T.);
#16378=EDGE_CURVE('',#13279,#13278,#7101,.T.);
#16379=EDGE_CURVE('',#13279,#13280,#7102,.T.);
#16380=EDGE_CURVE('',#13281,#13280,#7103,.T.);
#16381=EDGE_CURVE('',#13281,#13282,#7104,.T.);
#16382=EDGE_CURVE('',#13282,#13283,#7105,.T.);
#16383=EDGE_CURVE('',#13283,#13284,#7106,.T.);
#16384=EDGE_CURVE('',#13284,#13285,#7107,.T.);
#16385=EDGE_CURVE('',#13285,#13271,#7108,.T.);
#16386=EDGE_CURVE('',#13286,#13286,#12752,.T.);
#16387=EDGE_CURVE('',#13268,#13287,#7109,.T.);
#16388=EDGE_CURVE('',#13287,#13287,#12753,.T.);
#16389=EDGE_CURVE('',#13288,#13288,#12754,.T.);
#16390=EDGE_CURVE('',#13288,#13286,#7110,.T.);
#16391=EDGE_CURVE('',#13288,#13289,#7111,.T.);
#16392=EDGE_CURVE('',#13289,#13289,#12755,.T.);
#16393=EDGE_CURVE('',#13290,#13287,#7112,.T.);
#16394=EDGE_CURVE('',#13291,#13289,#7113,.T.);
#16395=EDGE_CURVE('',#13247,#13270,#7114,.T.);
#16396=EDGE_CURVE('',#13271,#13246,#7115,.T.);
#16397=EDGE_CURVE('',#13272,#13261,#7116,.T.);
#16398=EDGE_CURVE('',#13252,#13281,#7117,.T.);
#16399=EDGE_CURVE('',#13280,#13253,#7118,.T.);
#16400=EDGE_CURVE('',#13254,#13279,#7119,.T.);
#16401=EDGE_CURVE('',#13278,#13255,#7120,.T.);
#16402=EDGE_CURVE('',#13256,#13277,#7121,.T.);
#16403=EDGE_CURVE('',#13276,#13257,#7122,.T.);
#16404=EDGE_CURVE('',#13258,#13275,#7123,.T.);
#16405=EDGE_CURVE('',#13274,#13259,#7124,.T.);
#16406=EDGE_CURVE('',#13260,#13273,#7125,.T.);
#16407=EDGE_CURVE('',#13282,#13251,#7126,.T.);
#16408=EDGE_CURVE('',#13283,#13250,#7127,.T.);
#16409=EDGE_CURVE('',#13284,#13249,#7128,.T.);
#16410=EDGE_CURVE('',#13285,#13248,#7129,.T.);
#16411=EDGE_CURVE('',#13292,#13292,#12756,.T.);
#16412=EDGE_CURVE('',#13292,#13293,#7130,.T.);
#16413=EDGE_CURVE('',#13293,#13293,#12757,.T.);
#16414=EDGE_CURVE('',#13294,#13295,#7131,.T.);
#16415=EDGE_CURVE('',#13296,#13294,#7132,.T.);
#16416=EDGE_CURVE('',#13296,#13297,#7133,.T.);
#16417=EDGE_CURVE('',#13295,#13297,#7134,.T.);
#16418=EDGE_CURVE('',#13298,#13298,#12758,.T.);
#16419=EDGE_CURVE('',#13292,#13299,#7135,.T.);
#16420=EDGE_CURVE('',#13299,#13300,#12759,.T.);
#16421=EDGE_CURVE('',#13300,#13299,#12760,.T.);
#16422=EDGE_CURVE('',#13301,#13301,#12761,.T.);
#16423=EDGE_CURVE('',#13301,#13298,#7136,.T.);
#16424=EDGE_CURVE('',#13301,#13302,#7137,.T.);
#16425=EDGE_CURVE('',#13302,#13303,#12762,.T.);
#16426=EDGE_CURVE('',#13303,#13302,#12763,.T.);
#16427=EDGE_CURVE('',#13304,#13300,#7138,.T.);
#16428=EDGE_CURVE('',#13305,#13303,#7139,.T.);
#16429=EDGE_CURVE('',#13306,#13306,#12764,.T.);
#16430=EDGE_CURVE('',#13306,#13307,#7140,.T.);
#16431=EDGE_CURVE('',#13307,#13307,#12765,.T.);
#16432=EDGE_CURVE('',#13308,#13309,#7141,.T.);
#16433=EDGE_CURVE('',#13310,#13308,#7142,.T.);
#16434=EDGE_CURVE('',#13311,#13310,#7143,.T.);
#16435=EDGE_CURVE('',#13309,#13311,#7144,.T.);
#16436=EDGE_CURVE('',#13312,#13312,#12766,.T.);
#16437=EDGE_CURVE('',#13313,#13313,#12767,.T.);
#16438=EDGE_CURVE('',#13314,#13314,#12768,.T.);
#16439=EDGE_CURVE('',#13315,#13315,#12769,.T.);
#16440=EDGE_CURVE('',#13316,#13316,#12770,.T.);
#16441=EDGE_CURVE('',#13317,#13317,#12771,.T.);
#16442=EDGE_CURVE('',#13318,#13318,#12772,.T.);
#16443=EDGE_CURVE('',#13319,#13319,#12773,.T.);
#16444=EDGE_CURVE('',#13320,#13320,#12774,.T.);
#16445=EDGE_CURVE('',#13306,#13321,#7145,.T.);
#16446=EDGE_CURVE('',#13321,#13321,#12775,.T.);
#16447=EDGE_CURVE('',#13322,#13322,#12776,.T.);
#16448=EDGE_CURVE('',#13322,#13312,#7146,.T.);
#16449=EDGE_CURVE('',#13322,#13323,#7147,.T.);
#16450=EDGE_CURVE('',#13323,#13323,#12777,.T.);
#16451=EDGE_CURVE('',#13324,#13324,#12778,.T.);
#16452=EDGE_CURVE('',#13324,#13320,#7148,.T.);
#16453=EDGE_CURVE('',#13324,#13325,#7149,.T.);
#16454=EDGE_CURVE('',#13325,#13325,#12779,.T.);
#16455=EDGE_CURVE('',#13326,#13326,#12780,.T.);
#16456=EDGE_CURVE('',#13326,#13313,#7150,.T.);
#16457=EDGE_CURVE('',#13326,#13327,#7151,.T.);
#16458=EDGE_CURVE('',#13327,#13327,#12781,.T.);
#16459=EDGE_CURVE('',#13328,#13321,#7152,.T.);
#16460=EDGE_CURVE('',#13329,#13327,#7153,.T.);
#16461=EDGE_CURVE('',#13330,#13325,#7154,.T.);
#16462=EDGE_CURVE('',#13331,#13323,#7155,.T.);
#16463=EDGE_CURVE('',#13332,#13332,#12782,.T.);
#16464=EDGE_CURVE('',#13332,#13314,#7156,.T.);
#16465=EDGE_CURVE('',#13332,#13333,#7157,.T.);
#16466=EDGE_CURVE('',#13333,#13333,#12783,.T.);
#16467=EDGE_CURVE('',#13334,#13334,#12784,.T.);
#16468=EDGE_CURVE('',#13334,#13319,#7158,.T.);
#16469=EDGE_CURVE('',#13334,#13335,#7159,.T.);
#16470=EDGE_CURVE('',#13335,#13335,#12785,.T.);
#16471=EDGE_CURVE('',#13336,#13336,#12786,.T.);
#16472=EDGE_CURVE('',#13336,#13315,#7160,.T.);
#16473=EDGE_CURVE('',#13336,#13337,#7161,.T.);
#16474=EDGE_CURVE('',#13337,#13337,#12787,.T.);
#16475=EDGE_CURVE('',#13338,#13338,#12788,.T.);
#16476=EDGE_CURVE('',#13338,#13318,#7162,.T.);
#16477=EDGE_CURVE('',#13338,#13339,#7163,.T.);
#16478=EDGE_CURVE('',#13339,#13339,#12789,.T.);
#16479=EDGE_CURVE('',#13340,#13340,#12790,.T.);
#16480=EDGE_CURVE('',#13340,#13316,#7164,.T.);
#16481=EDGE_CURVE('',#13340,#13341,#7165,.T.);
#16482=EDGE_CURVE('',#13341,#13341,#12791,.T.);
#16483=EDGE_CURVE('',#13342,#13342,#12792,.T.);
#16484=EDGE_CURVE('',#13342,#13317,#7166,.T.);
#16485=EDGE_CURVE('',#13342,#13343,#7167,.T.);
#16486=EDGE_CURVE('',#13343,#13343,#12793,.T.);
#16487=EDGE_CURVE('',#13344,#13333,#7168,.T.);
#16488=EDGE_CURVE('',#13345,#13343,#7169,.T.);
#16489=EDGE_CURVE('',#13346,#13335,#7170,.T.);
#16490=EDGE_CURVE('',#13347,#13337,#7171,.T.);
#16491=EDGE_CURVE('',#13348,#13339,#7172,.T.);
#16492=EDGE_CURVE('',#13349,#13341,#7173,.T.);
#16493=EDGE_CURVE('',#13350,#13351,#7174,.T.);
#16494=EDGE_CURVE('',#13352,#13350,#12794,.T.);
#16495=EDGE_CURVE('',#13353,#13352,#7175,.T.);
#16496=EDGE_CURVE('',#13351,#13353,#12795,.T.);
#16497=EDGE_CURVE('',#13353,#13354,#7176,.T.);
#16498=EDGE_CURVE('',#13354,#13355,#7177,.T.);
#16499=EDGE_CURVE('',#13295,#13355,#7178,.T.);
#16500=EDGE_CURVE('',#13297,#13351,#7179,.T.);
#16501=EDGE_CURVE('',#13352,#13356,#7180,.T.);
#16502=EDGE_CURVE('',#13356,#13357,#7181,.T.);
#16503=EDGE_CURVE('',#13357,#13358,#7182,.T.);
#16504=EDGE_CURVE('',#13358,#13359,#7183,.T.);
#16505=EDGE_CURVE('',#13359,#13360,#7184,.T.);
#16506=EDGE_CURVE('',#13360,#13361,#7185,.T.);
#16507=EDGE_CURVE('',#13362,#13361,#7186,.T.);
#16508=EDGE_CURVE('',#13362,#13354,#7187,.T.);
#16509=EDGE_CURVE('',#13363,#13364,#7188,.T.);
#16510=EDGE_CURVE('',#13361,#13363,#12796,.T.);
#16511=EDGE_CURVE('',#13364,#13360,#12797,.T.);
#16512=EDGE_CURVE('',#13359,#13365,#12798,.T.);
#16513=EDGE_CURVE('',#13364,#13365,#7189,.T.);
#16514=EDGE_CURVE('',#13366,#13350,#7190,.T.);
#16515=EDGE_CURVE('',#13356,#13366,#12799,.T.);
#16516=EDGE_CURVE('',#13365,#13367,#12800,.T.);
#16517=EDGE_CURVE('',#13367,#13359,#12801,.T.);
#16518=EDGE_CURVE('',#13367,#13368,#7191,.T.);
#16519=EDGE_CURVE('',#13356,#13368,#12802,.T.);
#16520=EDGE_CURVE('',#13368,#13366,#12803,.T.);
#16521=EDGE_CURVE('',#13309,#13369,#7192,.T.);
#16522=EDGE_CURVE('',#13369,#13294,#7193,.T.);
#16523=EDGE_CURVE('',#13294,#13308,#7194,.T.);
#16524=EDGE_CURVE('',#13355,#13369,#7195,.T.);
#16525=EDGE_CURVE('',#13311,#13355,#7196,.T.);
#16526=EDGE_CURVE('',#13295,#13310,#7197,.T.);
#16527=EDGE_CURVE('',#13363,#13296,#7198,.T.);
#16528=EDGE_CURVE('',#13369,#13362,#7199,.T.);
#16529=EDGE_CURVE('',#13370,#13366,#7200,.T.);
#16530=EDGE_CURVE('',#13370,#13371,#7201,.T.);
#16531=EDGE_CURVE('',#13371,#13372,#7202,.T.);
#16532=EDGE_CURVE('',#13372,#13373,#7203,.T.);
#16533=EDGE_CURVE('',#13373,#13374,#7204,.T.);
#16534=EDGE_CURVE('',#13374,#13357,#7205,.T.);
#16535=EDGE_CURVE('',#13358,#13375,#7206,.T.);
#16536=EDGE_CURVE('',#13375,#13374,#7207,.T.);
#16537=EDGE_CURVE('',#13375,#13376,#7208,.T.);
#16538=EDGE_CURVE('',#13376,#13373,#7209,.T.);
#16539=EDGE_CURVE('',#13376,#13377,#7210,.T.);
#16540=EDGE_CURVE('',#13377,#13372,#7211,.T.);
#16541=EDGE_CURVE('',#13377,#13378,#7212,.T.);
#16542=EDGE_CURVE('',#13378,#13371,#7213,.T.);
#16543=EDGE_CURVE('',#13378,#13379,#7214,.T.);
#16544=EDGE_CURVE('',#13379,#13370,#7215,.T.);
#16545=EDGE_CURVE('',#13365,#13379,#7216,.T.);
#16546=EDGE_CURVE('',#13380,#13381,#12804,.T.);
#16547=EDGE_CURVE('',#13381,#13382,#7217,.T.);
#16548=EDGE_CURVE('',#13382,#13382,#12805,.T.);
#16549=EDGE_CURVE('',#13381,#13380,#12806,.T.);
#16550=EDGE_CURVE('',#13380,#13383,#7218,.T.);
#16551=EDGE_CURVE('',#13384,#13383,#12807,.T.);
#16552=EDGE_CURVE('',#13383,#13384,#12808,.T.);
#16553=EDGE_CURVE('',#13385,#13385,#12809,.T.);
#16554=EDGE_CURVE('',#13384,#13386,#7219,.T.);
#16555=EDGE_CURVE('',#13386,#13386,#12810,.T.);
#16556=EDGE_CURVE('',#13387,#13387,#12811,.T.);
#16557=EDGE_CURVE('',#13388,#13388,#12812,.T.);
#16558=EDGE_CURVE('',#13388,#13385,#7220,.T.);
#16559=EDGE_CURVE('',#13389,#13389,#12813,.T.);
#16560=EDGE_CURVE('',#13389,#13388,#7221,.T.);
#16561=EDGE_CURVE('',#13389,#13387,#7222,.T.);
#16562=EDGE_CURVE('',#13390,#13391,#7223,.T.);
#16563=EDGE_CURVE('',#13391,#13391,#12814,.T.);
#16564=EDGE_CURVE('',#13390,#13392,#617,.T.);
#16565=EDGE_CURVE('',#13392,#13393,#618,.T.);
#16566=EDGE_CURVE('',#13393,#13394,#7224,.T.);
#16567=EDGE_CURVE('',#13394,#13395,#619,.T.);
#16568=EDGE_CURVE('',#13395,#13396,#620,.T.);
#16569=EDGE_CURVE('',#13396,#13397,#7225,.T.);
#16570=EDGE_CURVE('',#13397,#13390,#621,.T.);
#16571=EDGE_CURVE('',#13398,#13399,#7226,.T.);
#16572=EDGE_CURVE('',#13399,#13394,#622,.T.);
#16573=EDGE_CURVE('',#13393,#13400,#623,.T.);
#16574=EDGE_CURVE('',#13400,#13398,#624,.T.);
#16575=EDGE_CURVE('',#13401,#13402,#7227,.T.);
#16576=EDGE_CURVE('',#13402,#13399,#625,.T.);
#16577=EDGE_CURVE('',#13398,#13401,#626,.T.);
#16578=EDGE_CURVE('',#13403,#13404,#7228,.T.);
#16579=EDGE_CURVE('',#13404,#13405,#627,.T.);
#16580=EDGE_CURVE('',#13405,#13402,#628,.T.);
#16581=EDGE_CURVE('',#13401,#13406,#629,.T.);
#16582=EDGE_CURVE('',#13406,#13403,#630,.T.);
#16583=EDGE_CURVE('',#13407,#13408,#7229,.T.);
#16584=EDGE_CURVE('',#13408,#13409,#631,.T.);
#16585=EDGE_CURVE('',#13409,#13404,#632,.T.);
#16586=EDGE_CURVE('',#13403,#13407,#633,.T.);
#16587=EDGE_CURVE('',#13410,#13411,#7230,.T.);
#16588=EDGE_CURVE('',#13411,#13412,#634,.T.);
#16589=EDGE_CURVE('',#13412,#13408,#635,.T.);
#16590=EDGE_CURVE('',#13407,#13410,#636,.T.);
#16591=EDGE_CURVE('',#13413,#13414,#7231,.T.);
#16592=EDGE_CURVE('',#13414,#13415,#637,.T.);
#16593=EDGE_CURVE('',#13415,#13411,#638,.T.);
#16594=EDGE_CURVE('',#13410,#13416,#639,.T.);
#16595=EDGE_CURVE('',#13416,#13413,#640,.T.);
#16596=EDGE_CURVE('',#13417,#13418,#7232,.T.);
#16597=EDGE_CURVE('',#13418,#13414,#641,.T.);
#16598=EDGE_CURVE('',#13413,#13419,#642,.T.);
#16599=EDGE_CURVE('',#13419,#13417,#643,.T.);
#16600=EDGE_CURVE('',#13417,#13420,#644,.T.);
#16601=EDGE_CURVE('',#13420,#13421,#645,.T.);
#16602=EDGE_CURVE('',#13421,#13422,#7233,.T.);
#16603=EDGE_CURVE('',#13422,#13423,#646,.T.);
#16604=EDGE_CURVE('',#13423,#13418,#647,.T.);
#16605=EDGE_CURVE('',#13424,#13425,#7234,.T.);
#16606=EDGE_CURVE('',#13425,#13422,#648,.T.);
#16607=EDGE_CURVE('',#13421,#13426,#649,.T.);
#16608=EDGE_CURVE('',#13426,#13427,#650,.T.);
#16609=EDGE_CURVE('',#13427,#13424,#651,.T.);
#16610=EDGE_CURVE('',#13428,#13429,#7235,.T.);
#16611=EDGE_CURVE('',#13429,#13430,#652,.T.);
#16612=EDGE_CURVE('',#13430,#13425,#653,.T.);
#16613=EDGE_CURVE('',#13424,#13428,#654,.T.);
#16614=EDGE_CURVE('',#13431,#13432,#7236,.T.);
#16615=EDGE_CURVE('',#13432,#13433,#655,.T.);
#16616=EDGE_CURVE('',#13433,#13429,#656,.T.);
#16617=EDGE_CURVE('',#13428,#13434,#657,.T.);
#16618=EDGE_CURVE('',#13434,#13435,#658,.T.);
#16619=EDGE_CURVE('',#13435,#13431,#659,.T.);
#16620=EDGE_CURVE('',#13436,#13437,#7237,.T.);
#16621=EDGE_CURVE('',#13437,#13438,#660,.T.);
#16622=EDGE_CURVE('',#13438,#13432,#661,.T.);
#16623=EDGE_CURVE('',#13431,#13436,#662,.T.);
#16624=EDGE_CURVE('',#13439,#13440,#663,.T.);
#16625=EDGE_CURVE('',#13440,#13437,#664,.T.);
#16626=EDGE_CURVE('',#13436,#13441,#665,.T.);
#16627=EDGE_CURVE('',#13441,#13439,#7238,.T.);
#16628=EDGE_CURVE('',#13442,#13443,#7239,.T.);
#16629=EDGE_CURVE('',#13443,#13444,#666,.T.);
#16630=EDGE_CURVE('',#13444,#13439,#667,.T.);
#16631=EDGE_CURVE('',#13441,#13445,#668,.T.);
#16632=EDGE_CURVE('',#13445,#13442,#669,.T.);
#16633=EDGE_CURVE('',#13446,#13447,#7240,.T.);
#16634=EDGE_CURVE('',#13447,#13443,#670,.T.);
#16635=EDGE_CURVE('',#13442,#13446,#671,.T.);
#16636=EDGE_CURVE('',#13448,#13449,#7241,.T.);
#16637=EDGE_CURVE('',#13449,#13450,#672,.T.);
#16638=EDGE_CURVE('',#13450,#13447,#673,.T.);
#16639=EDGE_CURVE('',#13446,#13451,#674,.T.);
#16640=EDGE_CURVE('',#13451,#13448,#675,.T.);
#16641=EDGE_CURVE('',#13452,#13453,#7242,.T.);
#16642=EDGE_CURVE('',#13453,#13449,#676,.T.);
#16643=EDGE_CURVE('',#13448,#13454,#677,.T.);
#16644=EDGE_CURVE('',#13454,#13452,#678,.T.);
#16645=EDGE_CURVE('',#13455,#13456,#7243,.T.);
#16646=EDGE_CURVE('',#13456,#13453,#679,.T.);
#16647=EDGE_CURVE('',#13452,#13455,#680,.T.);
#16648=EDGE_CURVE('',#13455,#13457,#681,.T.);
#16649=EDGE_CURVE('',#13457,#13458,#682,.T.);
#16650=EDGE_CURVE('',#13458,#13459,#7244,.T.);
#16651=EDGE_CURVE('',#13459,#13460,#683,.T.);
#16652=EDGE_CURVE('',#13460,#13456,#684,.T.);
#16653=EDGE_CURVE('',#13461,#13462,#7245,.T.);
#16654=EDGE_CURVE('',#13462,#13459,#685,.T.);
#16655=EDGE_CURVE('',#13458,#13463,#686,.T.);
#16656=EDGE_CURVE('',#13463,#13461,#687,.T.);
#16657=EDGE_CURVE('',#13464,#13465,#7246,.T.);
#16658=EDGE_CURVE('',#13465,#13466,#688,.T.);
#16659=EDGE_CURVE('',#13466,#13467,#689,.T.);
#16660=EDGE_CURVE('',#13467,#13462,#690,.T.);
#16661=EDGE_CURVE('',#13461,#13468,#691,.T.);
#16662=EDGE_CURVE('',#13468,#13464,#692,.T.);
#16663=EDGE_CURVE('',#13469,#13470,#7247,.T.);
#16664=EDGE_CURVE('',#13470,#13471,#693,.T.);
#16665=EDGE_CURVE('',#13471,#13465,#694,.T.);
#16666=EDGE_CURVE('',#13464,#13472,#695,.T.);
#16667=EDGE_CURVE('',#13472,#13469,#696,.T.);
#16668=EDGE_CURVE('',#13473,#13474,#7248,.T.);
#16669=EDGE_CURVE('',#13474,#13470,#697,.T.);
#16670=EDGE_CURVE('',#13469,#13473,#698,.T.);
#16671=EDGE_CURVE('',#13475,#13476,#7249,.T.);
#16672=EDGE_CURVE('',#13476,#13477,#699,.T.);
#16673=EDGE_CURVE('',#13477,#13478,#700,.T.);
#16674=EDGE_CURVE('',#13478,#13474,#701,.T.);
#16675=EDGE_CURVE('',#13473,#13479,#702,.T.);
#16676=EDGE_CURVE('',#13479,#13475,#703,.T.);
#16677=EDGE_CURVE('',#13475,#13480,#704,.T.);
#16678=EDGE_CURVE('',#13480,#13481,#705,.T.);
#16679=EDGE_CURVE('',#13481,#13482,#7250,.T.);
#16680=EDGE_CURVE('',#13482,#13476,#706,.T.);
#16681=EDGE_CURVE('',#13483,#13484,#7251,.T.);
#16682=EDGE_CURVE('',#13484,#13482,#707,.T.);
#16683=EDGE_CURVE('',#13481,#13483,#708,.T.);
#16684=EDGE_CURVE('',#13485,#13486,#7252,.T.);
#16685=EDGE_CURVE('',#13486,#13487,#709,.T.);
#16686=EDGE_CURVE('',#13487,#13484,#710,.T.);
#16687=EDGE_CURVE('',#13483,#13488,#711,.T.);
#16688=EDGE_CURVE('',#13488,#13485,#712,.T.);
#16689=EDGE_CURVE('',#13489,#13490,#7253,.T.);
#16690=EDGE_CURVE('',#13490,#13486,#713,.T.);
#16691=EDGE_CURVE('',#13485,#13489,#714,.T.);
#16692=EDGE_CURVE('',#13491,#13492,#7254,.T.);
#16693=EDGE_CURVE('',#13492,#13493,#715,.T.);
#16694=EDGE_CURVE('',#13493,#13490,#716,.T.);
#16695=EDGE_CURVE('',#13489,#13491,#717,.T.);
#16696=EDGE_CURVE('',#13491,#13494,#718,.T.);
#16697=EDGE_CURVE('',#13494,#13495,#719,.T.);
#16698=EDGE_CURVE('',#13495,#13496,#7255,.T.);
#16699=EDGE_CURVE('',#13496,#13497,#720,.T.);
#16700=EDGE_CURVE('',#13497,#13492,#721,.T.);
#16701=EDGE_CURVE('',#13498,#13499,#7256,.T.);
#16702=EDGE_CURVE('',#13499,#13496,#722,.T.);
#16703=EDGE_CURVE('',#13495,#13500,#723,.T.);
#16704=EDGE_CURVE('',#13500,#13498,#724,.T.);
#16705=EDGE_CURVE('',#13501,#13502,#7257,.T.);
#16706=EDGE_CURVE('',#13502,#13499,#725,.T.);
#16707=EDGE_CURVE('',#13498,#13503,#726,.T.);
#16708=EDGE_CURVE('',#13503,#13501,#727,.T.);
#16709=EDGE_CURVE('',#13504,#13505,#7258,.T.);
#16710=EDGE_CURVE('',#13505,#13506,#728,.T.);
#16711=EDGE_CURVE('',#13506,#13507,#729,.T.);
#16712=EDGE_CURVE('',#13507,#13502,#730,.T.);
#16713=EDGE_CURVE('',#13501,#13508,#731,.T.);
#16714=EDGE_CURVE('',#13508,#13504,#732,.T.);
#16715=EDGE_CURVE('',#13509,#13510,#7259,.T.);
#16716=EDGE_CURVE('',#13510,#13511,#733,.T.);
#16717=EDGE_CURVE('',#13511,#13505,#734,.T.);
#16718=EDGE_CURVE('',#13504,#13509,#735,.T.);
#16719=EDGE_CURVE('',#13512,#13513,#7260,.T.);
#16720=EDGE_CURVE('',#13513,#13514,#736,.T.);
#16721=EDGE_CURVE('',#13514,#13510,#737,.T.);
#16722=EDGE_CURVE('',#13509,#13515,#738,.T.);
#16723=EDGE_CURVE('',#13515,#13512,#739,.T.);
#16724=EDGE_CURVE('',#13512,#13516,#740,.T.);
#16725=EDGE_CURVE('',#13516,#13517,#7261,.T.);
#16726=EDGE_CURVE('',#13517,#13513,#741,.T.);
#16727=EDGE_CURVE('',#13518,#13519,#7262,.T.);
#16728=EDGE_CURVE('',#13519,#13520,#742,.T.);
#16729=EDGE_CURVE('',#13520,#13521,#743,.T.);
#16730=EDGE_CURVE('',#13521,#13517,#744,.T.);
#16731=EDGE_CURVE('',#13516,#13518,#745,.T.);
#16732=EDGE_CURVE('',#13522,#13523,#7263,.T.);
#16733=EDGE_CURVE('',#13523,#13519,#746,.T.);
#16734=EDGE_CURVE('',#13518,#13524,#747,.T.);
#16735=EDGE_CURVE('',#13524,#13522,#748,.T.);
#16736=EDGE_CURVE('',#13525,#13526,#7264,.T.);
#16737=EDGE_CURVE('',#13526,#13527,#749,.T.);
#16738=EDGE_CURVE('',#13527,#13528,#750,.T.);
#16739=EDGE_CURVE('',#13528,#13523,#751,.T.);
#16740=EDGE_CURVE('',#13522,#13525,#752,.T.);
#16741=EDGE_CURVE('',#13529,#13530,#7265,.T.);
#16742=EDGE_CURVE('',#13530,#13526,#753,.T.);
#16743=EDGE_CURVE('',#13525,#13531,#754,.T.);
#16744=EDGE_CURVE('',#13531,#13529,#755,.T.);
#16745=EDGE_CURVE('',#13532,#13533,#7266,.T.);
#16746=EDGE_CURVE('',#13533,#13534,#756,.T.);
#16747=EDGE_CURVE('',#13534,#13535,#757,.T.);
#16748=EDGE_CURVE('',#13535,#13536,#758,.T.);
#16749=EDGE_CURVE('',#13536,#13530,#759,.T.);
#16750=EDGE_CURVE('',#13529,#13537,#760,.T.);
#16751=EDGE_CURVE('',#13537,#13538,#761,.T.);
#16752=EDGE_CURVE('',#13538,#13532,#762,.T.);
#16753=EDGE_CURVE('',#13539,#13540,#7267,.T.);
#16754=EDGE_CURVE('',#13540,#13541,#763,.T.);
#16755=EDGE_CURVE('',#13541,#13533,#764,.T.);
#16756=EDGE_CURVE('',#13532,#13539,#765,.T.);
#16757=EDGE_CURVE('',#13542,#13543,#7268,.T.);
#16758=EDGE_CURVE('',#13543,#13544,#766,.T.);
#16759=EDGE_CURVE('',#13544,#13540,#767,.T.);
#16760=EDGE_CURVE('',#13539,#13545,#768,.T.);
#16761=EDGE_CURVE('',#13545,#13542,#769,.T.);
#16762=EDGE_CURVE('',#13546,#13547,#7269,.T.);
#16763=EDGE_CURVE('',#13547,#13543,#770,.T.);
#16764=EDGE_CURVE('',#13542,#13546,#771,.T.);
#16765=EDGE_CURVE('',#13548,#13549,#7270,.T.);
#16766=EDGE_CURVE('',#13549,#13550,#772,.T.);
#16767=EDGE_CURVE('',#13550,#13547,#773,.T.);
#16768=EDGE_CURVE('',#13546,#13548,#774,.T.);
#16769=EDGE_CURVE('',#13551,#13551,#12815,.T.);
#16770=EDGE_CURVE('',#13551,#13552,#7271,.T.);
#16771=EDGE_CURVE('',#13552,#13553,#775,.F.);
#16772=EDGE_CURVE('',#13553,#13554,#776,.T.);
#16773=EDGE_CURVE('',#13555,#13554,#7272,.T.);
#16774=EDGE_CURVE('',#13555,#13556,#777,.T.);
#16775=EDGE_CURVE('',#13556,#13557,#7273,.T.);
#16776=EDGE_CURVE('',#13557,#13552,#778,.F.);
#16777=EDGE_CURVE('',#13554,#13558,#779,.T.);
#16778=EDGE_CURVE('',#13558,#13549,#780,.T.);
#16779=EDGE_CURVE('',#13548,#13559,#781,.T.);
#16780=EDGE_CURVE('',#13560,#13559,#782,.T.);
#16781=EDGE_CURVE('',#13560,#13561,#783,.T.);
#16782=EDGE_CURVE('',#13561,#13555,#784,.T.);
#16783=EDGE_CURVE('',#13562,#13563,#12816,.T.);
#16784=EDGE_CURVE('',#13563,#13562,#7274,.T.);
#16785=EDGE_CURVE('',#13564,#13565,#12817,.T.);
#16786=EDGE_CURVE('',#13565,#13564,#7275,.T.);
#16787=EDGE_CURVE('',#13565,#13562,#7276,.T.);
#16788=EDGE_CURVE('',#13563,#13564,#7277,.T.);
#16789=EDGE_CURVE('',#13566,#13396,#7278,.T.);
#16790=EDGE_CURVE('',#13567,#13566,#7279,.T.);
#16791=EDGE_CURVE('',#13397,#13567,#7280,.T.);
#16792=EDGE_CURVE('',#13392,#13567,#785,.T.);
#16793=EDGE_CURVE('',#13400,#13566,#786,.T.);
#16794=EDGE_CURVE('',#13568,#13553,#787,.T.);
#16795=EDGE_CURVE('',#13569,#13568,#7281,.T.);
#16796=EDGE_CURVE('',#13569,#13558,#788,.T.);
#16797=EDGE_CURVE('',#13537,#13527,#789,.T.);
#16798=EDGE_CURVE('',#13531,#13521,#790,.T.);
#16799=EDGE_CURVE('',#13508,#13497,#791,.T.);
#16800=EDGE_CURVE('',#13503,#13493,#792,.T.);
#16801=EDGE_CURVE('',#13480,#13471,#793,.T.);
#16802=EDGE_CURVE('',#13479,#13466,#794,.T.);
#16803=EDGE_CURVE('',#13454,#13444,#795,.T.);
#16804=EDGE_CURVE('',#13451,#13440,#796,.T.);
#16805=EDGE_CURVE('',#13406,#13395,#797,.T.);
#16806=EDGE_CURVE('',#13568,#13557,#7282,.T.);
#16807=EDGE_CURVE('',#13545,#13535,#798,.T.);
#16808=EDGE_CURVE('',#13515,#13506,#799,.T.);
#16809=EDGE_CURVE('',#13488,#13477,#800,.T.);
#16810=EDGE_CURVE('',#13457,#13450,#801,.T.);
#16811=EDGE_CURVE('',#13435,#13423,#802,.T.);
#16812=EDGE_CURVE('',#13426,#13415,#803,.T.);
#16813=EDGE_CURVE('',#13559,#13544,#804,.T.);
#16814=EDGE_CURVE('',#13524,#13514,#805,.T.);
#16815=EDGE_CURVE('',#13494,#13487,#806,.T.);
#16816=EDGE_CURVE('',#13472,#13460,#807,.T.);
#16817=EDGE_CURVE('',#13445,#13433,#808,.T.);
#16818=EDGE_CURVE('',#13556,#13569,#7283,.T.);
#16819=EDGE_CURVE('',#13420,#13412,#809,.T.);
#16820=EDGE_CURVE('',#13416,#13405,#810,.T.);
#16821=EDGE_CURVE('',#13570,#13570,#12818,.T.);
#16822=EDGE_CURVE('',#13571,#13571,#12819,.T.);
#16823=EDGE_CURVE('',#13571,#13570,#7284,.T.);
#16824=EDGE_CURVE('',#13572,#13572,#12820,.T.);
#16825=EDGE_CURVE('',#13572,#13571,#7285,.T.);
#16826=EDGE_CURVE('',#13551,#13573,#7286,.T.);
#16827=EDGE_CURVE('',#13573,#13573,#12821,.T.);
#16828=EDGE_CURVE('',#13574,#13574,#12822,.T.);
#16829=EDGE_CURVE('',#13575,#13575,#12823,.T.);
#16830=EDGE_CURVE('',#13575,#13574,#7287,.T.);
#16831=EDGE_CURVE('',#13575,#13576,#7288,.T.);
#16832=EDGE_CURVE('',#13576,#13576,#12824,.T.);
#16833=EDGE_CURVE('',#13577,#13578,#811,.T.);
#16834=EDGE_CURVE('',#13579,#13577,#288,.T.);
#16835=EDGE_CURVE('',#13580,#13579,#289,.T.);
#16836=EDGE_CURVE('',#13581,#13580,#812,.T.);
#16837=EDGE_CURVE('',#13582,#13581,#290,.T.);
#16838=EDGE_CURVE('',#13583,#13582,#291,.T.);
#16839=EDGE_CURVE('',#13584,#13583,#813,.T.);
#16840=EDGE_CURVE('',#13585,#13584,#292,.T.);
#16841=EDGE_CURVE('',#13586,#13585,#293,.T.);
#16842=EDGE_CURVE('',#13587,#13586,#814,.T.);
#16843=EDGE_CURVE('',#13588,#13587,#294,.T.);
#16844=EDGE_CURVE('',#13589,#13588,#295,.T.);
#16845=EDGE_CURVE('',#13590,#13589,#815,.T.);
#16846=EDGE_CURVE('',#13591,#13590,#296,.T.);
#16847=EDGE_CURVE('',#13592,#13591,#297,.T.);
#16848=EDGE_CURVE('',#13593,#13592,#816,.T.);
#16849=EDGE_CURVE('',#13594,#13593,#298,.T.);
#16850=EDGE_CURVE('',#13595,#13594,#299,.T.);
#16851=EDGE_CURVE('',#13578,#13595,#817,.T.);
#16852=EDGE_CURVE('',#13578,#13596,#7289,.T.);
#16853=EDGE_CURVE('',#13597,#13596,#818,.T.);
#16854=EDGE_CURVE('',#13596,#13597,#819,.T.);
#16855=EDGE_CURVE('',#13598,#13577,#7290,.T.);
#16856=EDGE_CURVE('',#13598,#13599,#7291,.T.);
#16857=EDGE_CURVE('',#13599,#13579,#7292,.T.);
#16858=EDGE_CURVE('',#13599,#13600,#7293,.T.);
#16859=EDGE_CURVE('',#13580,#13600,#7294,.T.);
#16860=EDGE_CURVE('',#13601,#13585,#7295,.T.);
#16861=EDGE_CURVE('',#13601,#13602,#7296,.T.);
#16862=EDGE_CURVE('',#13586,#13602,#7297,.T.);
#16863=EDGE_CURVE('',#13603,#13587,#7298,.T.);
#16864=EDGE_CURVE('',#13603,#13604,#7299,.T.);
#16865=EDGE_CURVE('',#13588,#13604,#7300,.T.);
#16866=EDGE_CURVE('',#13605,#13584,#7301,.T.);
#16867=EDGE_CURVE('',#13605,#13601,#7302,.T.);
#16868=EDGE_CURVE('',#13604,#13606,#7303,.T.);
#16869=EDGE_CURVE('',#13589,#13606,#7304,.T.);
#16870=EDGE_CURVE('',#13607,#13581,#7305,.T.);
#16871=EDGE_CURVE('',#13607,#13608,#7306,.T.);
#16872=EDGE_CURVE('',#13608,#13582,#7307,.T.);
#16873=EDGE_CURVE('',#13591,#13609,#7308,.T.);
#16874=EDGE_CURVE('',#13609,#13610,#7309,.T.);
#16875=EDGE_CURVE('',#13592,#13610,#7310,.T.);
#16876=EDGE_CURVE('',#13608,#13611,#7311,.T.);
#16877=EDGE_CURVE('',#13583,#13611,#7312,.T.);
#16878=EDGE_CURVE('',#13612,#13590,#7313,.T.);
#16879=EDGE_CURVE('',#13612,#13609,#7314,.T.);
#16880=EDGE_CURVE('',#13602,#13605,#12825,.T.);
#16881=EDGE_CURVE('',#13606,#13603,#12826,.T.);
#16882=EDGE_CURVE('',#13613,#13614,#7315,.T.);
#16883=EDGE_CURVE('',#13613,#13615,#7316,.T.);
#16884=EDGE_CURVE('',#13616,#13615,#7317,.T.);
#16885=EDGE_CURVE('',#13616,#13614,#7318,.T.);
#16886=EDGE_CURVE('',#13614,#13617,#12827,.T.);
#16887=EDGE_CURVE('',#13617,#13616,#7319,.T.);
#16888=EDGE_CURVE('',#13617,#13618,#7320,.T.);
#16889=EDGE_CURVE('',#13615,#13618,#7321,.T.);
#16890=EDGE_CURVE('',#13618,#13613,#12828,.T.);
#16891=EDGE_CURVE('',#13619,#13620,#7322,.T.);
#16892=EDGE_CURVE('',#13619,#13621,#7323,.T.);
#16893=EDGE_CURVE('',#13622,#13621,#7324,.T.);
#16894=EDGE_CURVE('',#13622,#13620,#7325,.T.);
#16895=EDGE_CURVE('',#13620,#13623,#12829,.T.);
#16896=EDGE_CURVE('',#13623,#13622,#7326,.T.);
#16897=EDGE_CURVE('',#13623,#13624,#7327,.T.);
#16898=EDGE_CURVE('',#13621,#13624,#7328,.T.);
#16899=EDGE_CURVE('',#13624,#13619,#12830,.T.);
#16900=EDGE_CURVE('',#13625,#13626,#7329,.T.);
#16901=EDGE_CURVE('',#13625,#13627,#7330,.T.);
#16902=EDGE_CURVE('',#13628,#13627,#7331,.T.);
#16903=EDGE_CURVE('',#13628,#13626,#7332,.T.);
#16904=EDGE_CURVE('',#13626,#13629,#12831,.T.);
#16905=EDGE_CURVE('',#13629,#13628,#7333,.T.);
#16906=EDGE_CURVE('',#13629,#13630,#7334,.T.);
#16907=EDGE_CURVE('',#13627,#13630,#7335,.T.);
#16908=EDGE_CURVE('',#13630,#13625,#12832,.T.);
#16909=EDGE_CURVE('',#13631,#13632,#7336,.T.);
#16910=EDGE_CURVE('',#13631,#13633,#7337,.T.);
#16911=EDGE_CURVE('',#13634,#13633,#7338,.T.);
#16912=EDGE_CURVE('',#13634,#13632,#7339,.T.);
#16913=EDGE_CURVE('',#13632,#13635,#12833,.T.);
#16914=EDGE_CURVE('',#13635,#13634,#7340,.T.);
#16915=EDGE_CURVE('',#13635,#13636,#7341,.T.);
#16916=EDGE_CURVE('',#13633,#13636,#7342,.T.);
#16917=EDGE_CURVE('',#13636,#13631,#12834,.T.);
#16918=EDGE_CURVE('',#13637,#13638,#7343,.T.);
#16919=EDGE_CURVE('',#13637,#13639,#7344,.T.);
#16920=EDGE_CURVE('',#13640,#13639,#7345,.T.);
#16921=EDGE_CURVE('',#13640,#13638,#7346,.T.);
#16922=EDGE_CURVE('',#13638,#13641,#12835,.T.);
#16923=EDGE_CURVE('',#13641,#13640,#7347,.T.);
#16924=EDGE_CURVE('',#13641,#13642,#7348,.T.);
#16925=EDGE_CURVE('',#13639,#13642,#7349,.T.);
#16926=EDGE_CURVE('',#13642,#13637,#12836,.T.);
#16927=EDGE_CURVE('',#13643,#13644,#7350,.T.);
#16928=EDGE_CURVE('',#13643,#13645,#7351,.T.);
#16929=EDGE_CURVE('',#13646,#13645,#7352,.T.);
#16930=EDGE_CURVE('',#13646,#13644,#7353,.T.);
#16931=EDGE_CURVE('',#13644,#13647,#12837,.T.);
#16932=EDGE_CURVE('',#13647,#13646,#7354,.T.);
#16933=EDGE_CURVE('',#13647,#13648,#7355,.T.);
#16934=EDGE_CURVE('',#13645,#13648,#7356,.T.);
#16935=EDGE_CURVE('',#13648,#13643,#12838,.T.);
#16936=EDGE_CURVE('',#13649,#13650,#7357,.T.);
#16937=EDGE_CURVE('',#13649,#13651,#7358,.T.);
#16938=EDGE_CURVE('',#13652,#13651,#7359,.T.);
#16939=EDGE_CURVE('',#13652,#13650,#7360,.T.);
#16940=EDGE_CURVE('',#13650,#13653,#12839,.T.);
#16941=EDGE_CURVE('',#13653,#13652,#7361,.T.);
#16942=EDGE_CURVE('',#13653,#13654,#7362,.T.);
#16943=EDGE_CURVE('',#13651,#13654,#7363,.T.);
#16944=EDGE_CURVE('',#13654,#13649,#12840,.T.);
#16945=EDGE_CURVE('',#13655,#13656,#7364,.T.);
#16946=EDGE_CURVE('',#13655,#13657,#7365,.T.);
#16947=EDGE_CURVE('',#13658,#13657,#7366,.T.);
#16948=EDGE_CURVE('',#13658,#13656,#7367,.T.);
#16949=EDGE_CURVE('',#13656,#13659,#12841,.T.);
#16950=EDGE_CURVE('',#13659,#13658,#7368,.T.);
#16951=EDGE_CURVE('',#13659,#13660,#7369,.T.);
#16952=EDGE_CURVE('',#13657,#13660,#7370,.T.);
#16953=EDGE_CURVE('',#13660,#13655,#12842,.T.);
#16954=EDGE_CURVE('',#13661,#13662,#7371,.T.);
#16955=EDGE_CURVE('',#13661,#13663,#7372,.T.);
#16956=EDGE_CURVE('',#13664,#13663,#7373,.T.);
#16957=EDGE_CURVE('',#13664,#13662,#7374,.T.);
#16958=EDGE_CURVE('',#13662,#13665,#12843,.T.);
#16959=EDGE_CURVE('',#13665,#13664,#7375,.T.);
#16960=EDGE_CURVE('',#13665,#13666,#7376,.T.);
#16961=EDGE_CURVE('',#13663,#13666,#7377,.T.);
#16962=EDGE_CURVE('',#13666,#13661,#12844,.T.);
#16963=EDGE_CURVE('',#13667,#13668,#7378,.T.);
#16964=EDGE_CURVE('',#13667,#13669,#7379,.T.);
#16965=EDGE_CURVE('',#13670,#13669,#7380,.T.);
#16966=EDGE_CURVE('',#13670,#13668,#7381,.T.);
#16967=EDGE_CURVE('',#13668,#13671,#12845,.T.);
#16968=EDGE_CURVE('',#13671,#13670,#7382,.T.);
#16969=EDGE_CURVE('',#13671,#13672,#7383,.T.);
#16970=EDGE_CURVE('',#13669,#13672,#7384,.T.);
#16971=EDGE_CURVE('',#13672,#13667,#12846,.T.);
#16972=EDGE_CURVE('',#13673,#13674,#7385,.T.);
#16973=EDGE_CURVE('',#13673,#13675,#7386,.T.);
#16974=EDGE_CURVE('',#13676,#13675,#7387,.T.);
#16975=EDGE_CURVE('',#13676,#13674,#7388,.T.);
#16976=EDGE_CURVE('',#13674,#13677,#12847,.T.);
#16977=EDGE_CURVE('',#13677,#13676,#7389,.T.);
#16978=EDGE_CURVE('',#13677,#13678,#7390,.T.);
#16979=EDGE_CURVE('',#13675,#13678,#7391,.T.);
#16980=EDGE_CURVE('',#13678,#13673,#12848,.T.);
#16981=EDGE_CURVE('',#13679,#13680,#7392,.T.);
#16982=EDGE_CURVE('',#13679,#13681,#7393,.T.);
#16983=EDGE_CURVE('',#13682,#13681,#7394,.T.);
#16984=EDGE_CURVE('',#13682,#13680,#7395,.T.);
#16985=EDGE_CURVE('',#13680,#13683,#12849,.T.);
#16986=EDGE_CURVE('',#13683,#13682,#7396,.T.);
#16987=EDGE_CURVE('',#13683,#13684,#7397,.T.);
#16988=EDGE_CURVE('',#13681,#13684,#7398,.T.);
#16989=EDGE_CURVE('',#13684,#13679,#12850,.T.);
#16990=EDGE_CURVE('',#13685,#13686,#7399,.T.);
#16991=EDGE_CURVE('',#13685,#13687,#7400,.T.);
#16992=EDGE_CURVE('',#13688,#13687,#7401,.T.);
#16993=EDGE_CURVE('',#13688,#13686,#7402,.T.);
#16994=EDGE_CURVE('',#13686,#13689,#12851,.T.);
#16995=EDGE_CURVE('',#13689,#13688,#7403,.T.);
#16996=EDGE_CURVE('',#13689,#13690,#7404,.T.);
#16997=EDGE_CURVE('',#13687,#13690,#7405,.T.);
#16998=EDGE_CURVE('',#13690,#13685,#12852,.T.);
#16999=EDGE_CURVE('',#13691,#13692,#7406,.T.);
#17000=EDGE_CURVE('',#13691,#13693,#7407,.T.);
#17001=EDGE_CURVE('',#13694,#13693,#7408,.T.);
#17002=EDGE_CURVE('',#13694,#13692,#7409,.T.);
#17003=EDGE_CURVE('',#13692,#13695,#12853,.T.);
#17004=EDGE_CURVE('',#13695,#13694,#7410,.T.);
#17005=EDGE_CURVE('',#13695,#13696,#7411,.T.);
#17006=EDGE_CURVE('',#13693,#13696,#7412,.T.);
#17007=EDGE_CURVE('',#13696,#13691,#12854,.T.);
#17008=EDGE_CURVE('',#13697,#13698,#7413,.T.);
#17009=EDGE_CURVE('',#13697,#13699,#7414,.T.);
#17010=EDGE_CURVE('',#13700,#13699,#7415,.T.);
#17011=EDGE_CURVE('',#13700,#13698,#7416,.T.);
#17012=EDGE_CURVE('',#13698,#13701,#12855,.T.);
#17013=EDGE_CURVE('',#13701,#13700,#7417,.T.);
#17014=EDGE_CURVE('',#13701,#13702,#7418,.T.);
#17015=EDGE_CURVE('',#13699,#13702,#7419,.T.);
#17016=EDGE_CURVE('',#13702,#13697,#12856,.T.);
#17017=EDGE_CURVE('',#13703,#13704,#7420,.T.);
#17018=EDGE_CURVE('',#13703,#13705,#7421,.T.);
#17019=EDGE_CURVE('',#13706,#13705,#7422,.T.);
#17020=EDGE_CURVE('',#13706,#13704,#7423,.T.);
#17021=EDGE_CURVE('',#13704,#13707,#12857,.T.);
#17022=EDGE_CURVE('',#13707,#13706,#7424,.T.);
#17023=EDGE_CURVE('',#13707,#13708,#7425,.T.);
#17024=EDGE_CURVE('',#13705,#13708,#7426,.T.);
#17025=EDGE_CURVE('',#13708,#13703,#12858,.T.);
#17026=EDGE_CURVE('',#13709,#13710,#7427,.T.);
#17027=EDGE_CURVE('',#13709,#13711,#7428,.T.);
#17028=EDGE_CURVE('',#13712,#13711,#7429,.T.);
#17029=EDGE_CURVE('',#13712,#13710,#7430,.T.);
#17030=EDGE_CURVE('',#13710,#13713,#12859,.T.);
#17031=EDGE_CURVE('',#13713,#13712,#7431,.T.);
#17032=EDGE_CURVE('',#13713,#13714,#7432,.T.);
#17033=EDGE_CURVE('',#13711,#13714,#7433,.T.);
#17034=EDGE_CURVE('',#13714,#13709,#12860,.T.);
#17035=EDGE_CURVE('',#13715,#13716,#7434,.T.);
#17036=EDGE_CURVE('',#13715,#13717,#7435,.T.);
#17037=EDGE_CURVE('',#13718,#13717,#7436,.T.);
#17038=EDGE_CURVE('',#13718,#13716,#7437,.T.);
#17039=EDGE_CURVE('',#13716,#13719,#12861,.T.);
#17040=EDGE_CURVE('',#13719,#13718,#7438,.T.);
#17041=EDGE_CURVE('',#13719,#13720,#7439,.T.);
#17042=EDGE_CURVE('',#13717,#13720,#7440,.T.);
#17043=EDGE_CURVE('',#13720,#13715,#12862,.T.);
#17044=EDGE_CURVE('',#13721,#13722,#7441,.T.);
#17045=EDGE_CURVE('',#13721,#13723,#7442,.T.);
#17046=EDGE_CURVE('',#13724,#13723,#7443,.T.);
#17047=EDGE_CURVE('',#13724,#13722,#7444,.T.);
#17048=EDGE_CURVE('',#13722,#13725,#12863,.T.);
#17049=EDGE_CURVE('',#13726,#13724,#7445,.T.);
#17050=EDGE_CURVE('',#13725,#13726,#12864,.T.);
#17051=EDGE_CURVE('',#13726,#13727,#7446,.T.);
#17052=EDGE_CURVE('',#13723,#13727,#7447,.T.);
#17053=EDGE_CURVE('',#13727,#13728,#12865,.T.);
#17054=EDGE_CURVE('',#13728,#13721,#12866,.T.);
#17055=EDGE_CURVE('',#13729,#13730,#7448,.T.);
#17056=EDGE_CURVE('',#13729,#13731,#7449,.T.);
#17057=EDGE_CURVE('',#13732,#13731,#7450,.T.);
#17058=EDGE_CURVE('',#13732,#13730,#7451,.T.);
#17059=EDGE_CURVE('',#13730,#13733,#12867,.T.);
#17060=EDGE_CURVE('',#13733,#13732,#7452,.T.);
#17061=EDGE_CURVE('',#13733,#13734,#7453,.T.);
#17062=EDGE_CURVE('',#13731,#13734,#7454,.T.);
#17063=EDGE_CURVE('',#13734,#13729,#12868,.T.);
#17064=EDGE_CURVE('',#13735,#13736,#7455,.T.);
#17065=EDGE_CURVE('',#13735,#13737,#7456,.T.);
#17066=EDGE_CURVE('',#13738,#13737,#7457,.T.);
#17067=EDGE_CURVE('',#13738,#13736,#7458,.T.);
#17068=EDGE_CURVE('',#13736,#13739,#12869,.T.);
#17069=EDGE_CURVE('',#13739,#13738,#7459,.T.);
#17070=EDGE_CURVE('',#13739,#13740,#7460,.T.);
#17071=EDGE_CURVE('',#13737,#13740,#7461,.T.);
#17072=EDGE_CURVE('',#13740,#13735,#12870,.T.);
#17073=EDGE_CURVE('',#13741,#13742,#7462,.T.);
#17074=EDGE_CURVE('',#13741,#13743,#7463,.T.);
#17075=EDGE_CURVE('',#13744,#13743,#7464,.T.);
#17076=EDGE_CURVE('',#13744,#13742,#7465,.T.);
#17077=EDGE_CURVE('',#13742,#13745,#12871,.T.);
#17078=EDGE_CURVE('',#13745,#13744,#7466,.T.);
#17079=EDGE_CURVE('',#13745,#13746,#7467,.T.);
#17080=EDGE_CURVE('',#13743,#13746,#7468,.T.);
#17081=EDGE_CURVE('',#13746,#13741,#12872,.T.);
#17082=EDGE_CURVE('',#13747,#13748,#7469,.T.);
#17083=EDGE_CURVE('',#13747,#13749,#7470,.T.);
#17084=EDGE_CURVE('',#13750,#13749,#7471,.T.);
#17085=EDGE_CURVE('',#13750,#13748,#7472,.T.);
#17086=EDGE_CURVE('',#13748,#13751,#12873,.T.);
#17087=EDGE_CURVE('',#13751,#13750,#7473,.T.);
#17088=EDGE_CURVE('',#13751,#13752,#7474,.T.);
#17089=EDGE_CURVE('',#13749,#13752,#7475,.T.);
#17090=EDGE_CURVE('',#13752,#13747,#12874,.T.);
#17091=EDGE_CURVE('',#13753,#13754,#7476,.T.);
#17092=EDGE_CURVE('',#13753,#13755,#7477,.T.);
#17093=EDGE_CURVE('',#13756,#13755,#7478,.T.);
#17094=EDGE_CURVE('',#13756,#13754,#7479,.T.);
#17095=EDGE_CURVE('',#13754,#13757,#12875,.T.);
#17096=EDGE_CURVE('',#13757,#13756,#7480,.T.);
#17097=EDGE_CURVE('',#13757,#13758,#7481,.T.);
#17098=EDGE_CURVE('',#13755,#13758,#7482,.T.);
#17099=EDGE_CURVE('',#13758,#13753,#12876,.T.);
#17100=EDGE_CURVE('',#13759,#13760,#7483,.T.);
#17101=EDGE_CURVE('',#13759,#13761,#7484,.T.);
#17102=EDGE_CURVE('',#13762,#13761,#7485,.T.);
#17103=EDGE_CURVE('',#13762,#13760,#7486,.T.);
#17104=EDGE_CURVE('',#13760,#13763,#12877,.T.);
#17105=EDGE_CURVE('',#13763,#13762,#7487,.T.);
#17106=EDGE_CURVE('',#13763,#13764,#7488,.T.);
#17107=EDGE_CURVE('',#13761,#13764,#7489,.T.);
#17108=EDGE_CURVE('',#13764,#13759,#12878,.T.);
#17109=EDGE_CURVE('',#13765,#13766,#7490,.T.);
#17110=EDGE_CURVE('',#13765,#13767,#7491,.T.);
#17111=EDGE_CURVE('',#13768,#13767,#7492,.T.);
#17112=EDGE_CURVE('',#13768,#13766,#7493,.T.);
#17113=EDGE_CURVE('',#13766,#13769,#12879,.T.);
#17114=EDGE_CURVE('',#13769,#13768,#7494,.T.);
#17115=EDGE_CURVE('',#13769,#13770,#7495,.T.);
#17116=EDGE_CURVE('',#13767,#13770,#7496,.T.);
#17117=EDGE_CURVE('',#13770,#13765,#12880,.T.);
#17118=EDGE_CURVE('',#13771,#13772,#7497,.T.);
#17119=EDGE_CURVE('',#13771,#13773,#7498,.T.);
#17120=EDGE_CURVE('',#13774,#13773,#7499,.T.);
#17121=EDGE_CURVE('',#13774,#13772,#7500,.T.);
#17122=EDGE_CURVE('',#13772,#13775,#12881,.T.);
#17123=EDGE_CURVE('',#13775,#13774,#7501,.T.);
#17124=EDGE_CURVE('',#13775,#13776,#7502,.T.);
#17125=EDGE_CURVE('',#13773,#13776,#7503,.T.);
#17126=EDGE_CURVE('',#13776,#13771,#12882,.T.);
#17127=EDGE_CURVE('',#13777,#13778,#7504,.T.);
#17128=EDGE_CURVE('',#13777,#13779,#7505,.T.);
#17129=EDGE_CURVE('',#13780,#13779,#7506,.T.);
#17130=EDGE_CURVE('',#13780,#13778,#7507,.T.);
#17131=EDGE_CURVE('',#13778,#13781,#12883,.T.);
#17132=EDGE_CURVE('',#13781,#13780,#7508,.T.);
#17133=EDGE_CURVE('',#13781,#13782,#7509,.T.);
#17134=EDGE_CURVE('',#13779,#13782,#7510,.T.);
#17135=EDGE_CURVE('',#13782,#13777,#12884,.T.);
#17136=EDGE_CURVE('',#13783,#13784,#7511,.T.);
#17137=EDGE_CURVE('',#13783,#13785,#7512,.T.);
#17138=EDGE_CURVE('',#13786,#13785,#7513,.T.);
#17139=EDGE_CURVE('',#13786,#13784,#7514,.T.);
#17140=EDGE_CURVE('',#13784,#13787,#12885,.T.);
#17141=EDGE_CURVE('',#13787,#13786,#7515,.T.);
#17142=EDGE_CURVE('',#13787,#13788,#7516,.T.);
#17143=EDGE_CURVE('',#13785,#13788,#7517,.T.);
#17144=EDGE_CURVE('',#13788,#13783,#12886,.T.);
#17145=EDGE_CURVE('',#13789,#13790,#7518,.T.);
#17146=EDGE_CURVE('',#13789,#13791,#7519,.T.);
#17147=EDGE_CURVE('',#13792,#13791,#7520,.T.);
#17148=EDGE_CURVE('',#13792,#13790,#7521,.T.);
#17149=EDGE_CURVE('',#13790,#13793,#12887,.T.);
#17150=EDGE_CURVE('',#13793,#13792,#7522,.T.);
#17151=EDGE_CURVE('',#13793,#13794,#7523,.T.);
#17152=EDGE_CURVE('',#13791,#13794,#7524,.T.);
#17153=EDGE_CURVE('',#13794,#13789,#12888,.T.);
#17154=EDGE_CURVE('',#13795,#13796,#7525,.T.);
#17155=EDGE_CURVE('',#13795,#13797,#7526,.T.);
#17156=EDGE_CURVE('',#13798,#13797,#7527,.T.);
#17157=EDGE_CURVE('',#13798,#13796,#7528,.T.);
#17158=EDGE_CURVE('',#13796,#13799,#12889,.T.);
#17159=EDGE_CURVE('',#13799,#13798,#7529,.T.);
#17160=EDGE_CURVE('',#13799,#13800,#7530,.T.);
#17161=EDGE_CURVE('',#13797,#13800,#7531,.T.);
#17162=EDGE_CURVE('',#13800,#13795,#12890,.T.);
#17163=EDGE_CURVE('',#13801,#13802,#7532,.T.);
#17164=EDGE_CURVE('',#13801,#13803,#7533,.T.);
#17165=EDGE_CURVE('',#13804,#13803,#7534,.T.);
#17166=EDGE_CURVE('',#13804,#13802,#7535,.T.);
#17167=EDGE_CURVE('',#13802,#13805,#12891,.T.);
#17168=EDGE_CURVE('',#13805,#13804,#7536,.T.);
#17169=EDGE_CURVE('',#13805,#13806,#7537,.T.);
#17170=EDGE_CURVE('',#13803,#13806,#7538,.T.);
#17171=EDGE_CURVE('',#13806,#13801,#12892,.T.);
#17172=EDGE_CURVE('',#13807,#13808,#7539,.T.);
#17173=EDGE_CURVE('',#13807,#13809,#7540,.T.);
#17174=EDGE_CURVE('',#13810,#13809,#7541,.T.);
#17175=EDGE_CURVE('',#13810,#13808,#7542,.T.);
#17176=EDGE_CURVE('',#13808,#13811,#12893,.T.);
#17177=EDGE_CURVE('',#13811,#13810,#7543,.T.);
#17178=EDGE_CURVE('',#13811,#13812,#7544,.T.);
#17179=EDGE_CURVE('',#13809,#13812,#7545,.T.);
#17180=EDGE_CURVE('',#13812,#13807,#12894,.T.);
#17181=EDGE_CURVE('',#13813,#13814,#7546,.T.);
#17182=EDGE_CURVE('',#13813,#13815,#7547,.T.);
#17183=EDGE_CURVE('',#13816,#13815,#7548,.T.);
#17184=EDGE_CURVE('',#13816,#13814,#7549,.T.);
#17185=EDGE_CURVE('',#13814,#13817,#12895,.T.);
#17186=EDGE_CURVE('',#13817,#13816,#7550,.T.);
#17187=EDGE_CURVE('',#13817,#13818,#7551,.T.);
#17188=EDGE_CURVE('',#13815,#13818,#7552,.T.);
#17189=EDGE_CURVE('',#13818,#13813,#12896,.T.);
#17190=EDGE_CURVE('',#13819,#13820,#7553,.T.);
#17191=EDGE_CURVE('',#13819,#13821,#7554,.T.);
#17192=EDGE_CURVE('',#13822,#13821,#7555,.T.);
#17193=EDGE_CURVE('',#13822,#13820,#7556,.T.);
#17194=EDGE_CURVE('',#13820,#13823,#12897,.T.);
#17195=EDGE_CURVE('',#13823,#13822,#7557,.T.);
#17196=EDGE_CURVE('',#13823,#13824,#7558,.T.);
#17197=EDGE_CURVE('',#13821,#13824,#7559,.T.);
#17198=EDGE_CURVE('',#13824,#13819,#12898,.T.);
#17199=EDGE_CURVE('',#13825,#13826,#7560,.T.);
#17200=EDGE_CURVE('',#13825,#13827,#7561,.T.);
#17201=EDGE_CURVE('',#13828,#13827,#7562,.T.);
#17202=EDGE_CURVE('',#13828,#13826,#7563,.T.);
#17203=EDGE_CURVE('',#13826,#13829,#12899,.T.);
#17204=EDGE_CURVE('',#13829,#13828,#7564,.T.);
#17205=EDGE_CURVE('',#13829,#13830,#7565,.T.);
#17206=EDGE_CURVE('',#13827,#13830,#7566,.T.);
#17207=EDGE_CURVE('',#13830,#13825,#12900,.T.);
#17208=EDGE_CURVE('',#13831,#13832,#7567,.T.);
#17209=EDGE_CURVE('',#13831,#13833,#7568,.T.);
#17210=EDGE_CURVE('',#13834,#13833,#7569,.T.);
#17211=EDGE_CURVE('',#13834,#13832,#7570,.T.);
#17212=EDGE_CURVE('',#13832,#13835,#12901,.T.);
#17213=EDGE_CURVE('',#13835,#13834,#7571,.T.);
#17214=EDGE_CURVE('',#13835,#13836,#7572,.T.);
#17215=EDGE_CURVE('',#13833,#13836,#7573,.T.);
#17216=EDGE_CURVE('',#13836,#13831,#12902,.T.);
#17217=EDGE_CURVE('',#13837,#13593,#7574,.T.);
#17218=EDGE_CURVE('',#13837,#13838,#7575,.T.);
#17219=EDGE_CURVE('',#13594,#13838,#7576,.T.);
#17220=EDGE_CURVE('',#13600,#13598,#12903,.T.);
#17221=EDGE_CURVE('',#13838,#13839,#7577,.T.);
#17222=EDGE_CURVE('',#13595,#13839,#7578,.T.);
#17223=EDGE_CURVE('',#13839,#13837,#12904,.T.);
#17224=EDGE_CURVE('',#13611,#13607,#12905,.T.);
#17225=EDGE_CURVE('',#13610,#13612,#12906,.T.);
#17226=EDGE_CURVE('',#13840,#13840,#12907,.T.);
#17227=EDGE_CURVE('',#13840,#13841,#7579,.T.);
#17228=EDGE_CURVE('',#13841,#13841,#12908,.T.);
#17229=EDGE_CURVE('',#13842,#13842,#12909,.T.);
#17230=EDGE_CURVE('',#13843,#13843,#12910,.T.);
#17231=EDGE_CURVE('',#13843,#13842,#7580,.T.);
#17232=EDGE_CURVE('',#13844,#13844,#12911,.T.);
#17233=EDGE_CURVE('',#13844,#13725,#7581,.T.);
#17234=EDGE_CURVE('',#13728,#13843,#7582,.T.);
#17235=EDGE_CURVE('',#13844,#13845,#7583,.T.);
#17236=EDGE_CURVE('',#13845,#13845,#12912,.T.);
#17237=EDGE_CURVE('',#13846,#13846,#12913,.T.);
#17238=EDGE_CURVE('',#13847,#13847,#12914,.T.);
#17239=EDGE_CURVE('',#13847,#13846,#7584,.T.);
#17240=EDGE_CURVE('',#13848,#13848,#12915,.T.);
#17241=EDGE_CURVE('',#13840,#13848,#7585,.T.);
#17242=EDGE_CURVE('',#13849,#13850,#820,.T.);
#17243=EDGE_CURVE('',#13849,#13851,#7586,.T.);
#17244=EDGE_CURVE('',#13851,#13852,#821,.T.);
#17245=EDGE_CURVE('',#13850,#13852,#7587,.T.);
#17246=EDGE_CURVE('',#13853,#13849,#822,.T.);
#17247=EDGE_CURVE('',#13853,#13854,#7588,.T.);
#17248=EDGE_CURVE('',#13854,#13851,#823,.T.);
#17249=EDGE_CURVE('',#13855,#13853,#824,.T.);
#17250=EDGE_CURVE('',#13855,#13856,#7589,.T.);
#17251=EDGE_CURVE('',#13856,#13854,#825,.T.);
#17252=EDGE_CURVE('',#13857,#13855,#826,.T.);
#17253=EDGE_CURVE('',#13857,#13858,#7590,.T.);
#17254=EDGE_CURVE('',#13858,#13856,#827,.T.);
#17255=EDGE_CURVE('',#13859,#13857,#828,.T.);
#17256=EDGE_CURVE('',#13859,#13860,#7591,.T.);
#17257=EDGE_CURVE('',#13860,#13858,#829,.T.);
#17258=EDGE_CURVE('',#13861,#13859,#830,.T.);
#17259=EDGE_CURVE('',#13861,#13862,#7592,.T.);
#17260=EDGE_CURVE('',#13862,#13860,#831,.T.);
#17261=EDGE_CURVE('',#13863,#13861,#832,.T.);
#17262=EDGE_CURVE('',#13863,#13864,#7593,.T.);
#17263=EDGE_CURVE('',#13864,#13862,#833,.T.);
#17264=EDGE_CURVE('',#13850,#13863,#834,.T.);
#17265=EDGE_CURVE('',#13852,#13864,#835,.T.);
#17266=EDGE_CURVE('',#13865,#13866,#836,.T.);
#17267=EDGE_CURVE('',#13865,#13867,#7594,.T.);
#17268=EDGE_CURVE('',#13867,#13868,#837,.T.);
#17269=EDGE_CURVE('',#13866,#13868,#7595,.T.);
#17270=EDGE_CURVE('',#13869,#13865,#838,.T.);
#17271=EDGE_CURVE('',#13869,#13870,#7596,.T.);
#17272=EDGE_CURVE('',#13870,#13867,#839,.T.);
#17273=EDGE_CURVE('',#13871,#13869,#840,.T.);
#17274=EDGE_CURVE('',#13871,#13872,#7597,.T.);
#17275=EDGE_CURVE('',#13872,#13870,#841,.T.);
#17276=EDGE_CURVE('',#13873,#13871,#842,.T.);
#17277=EDGE_CURVE('',#13873,#13874,#7598,.T.);
#17278=EDGE_CURVE('',#13874,#13872,#843,.T.);
#17279=EDGE_CURVE('',#13875,#13873,#844,.T.);
#17280=EDGE_CURVE('',#13875,#13876,#7599,.T.);
#17281=EDGE_CURVE('',#13876,#13874,#845,.T.);
#17282=EDGE_CURVE('',#13877,#13875,#846,.T.);
#17283=EDGE_CURVE('',#13877,#13878,#7600,.T.);
#17284=EDGE_CURVE('',#13878,#13876,#847,.T.);
#17285=EDGE_CURVE('',#13879,#13877,#848,.T.);
#17286=EDGE_CURVE('',#13879,#13880,#7601,.T.);
#17287=EDGE_CURVE('',#13880,#13878,#849,.T.);
#17288=EDGE_CURVE('',#13881,#13879,#850,.T.);
#17289=EDGE_CURVE('',#13881,#13882,#7602,.T.);
#17290=EDGE_CURVE('',#13882,#13880,#851,.T.);
#17291=EDGE_CURVE('',#13883,#13881,#852,.T.);
#17292=EDGE_CURVE('',#13883,#13884,#7603,.T.);
#17293=EDGE_CURVE('',#13884,#13882,#853,.T.);
#17294=EDGE_CURVE('',#13885,#13883,#854,.T.);
#17295=EDGE_CURVE('',#13885,#13886,#7604,.T.);
#17296=EDGE_CURVE('',#13886,#13884,#855,.T.);
#17297=EDGE_CURVE('',#13887,#13885,#856,.T.);
#17298=EDGE_CURVE('',#13887,#13888,#7605,.T.);
#17299=EDGE_CURVE('',#13888,#13886,#857,.T.);
#17300=EDGE_CURVE('',#13866,#13887,#858,.T.);
#17301=EDGE_CURVE('',#13868,#13888,#859,.T.);
#17302=EDGE_CURVE('',#13889,#13890,#7606,.T.);
#17303=EDGE_CURVE('',#13889,#13891,#7607,.T.);
#17304=EDGE_CURVE('',#13891,#13892,#7608,.T.);
#17305=EDGE_CURVE('',#13890,#13892,#7609,.T.);
#17306=EDGE_CURVE('',#13893,#13889,#7610,.T.);
#17307=EDGE_CURVE('',#13893,#13894,#7611,.T.);
#17308=EDGE_CURVE('',#13894,#13891,#7612,.T.);
#17309=EDGE_CURVE('',#13890,#13893,#7613,.T.);
#17310=EDGE_CURVE('',#13892,#13894,#7614,.T.);
#17311=EDGE_CURVE('',#13895,#13896,#7615,.T.);
#17312=EDGE_CURVE('',#13895,#13897,#7616,.T.);
#17313=EDGE_CURVE('',#13897,#13898,#7617,.T.);
#17314=EDGE_CURVE('',#13896,#13898,#7618,.T.);
#17315=EDGE_CURVE('',#13899,#13895,#7619,.T.);
#17316=EDGE_CURVE('',#13899,#13900,#7620,.T.);
#17317=EDGE_CURVE('',#13900,#13897,#7621,.T.);
#17318=EDGE_CURVE('',#13901,#13899,#7622,.T.);
#17319=EDGE_CURVE('',#13901,#13902,#7623,.T.);
#17320=EDGE_CURVE('',#13902,#13900,#7624,.T.);
#17321=EDGE_CURVE('',#13903,#13901,#7625,.T.);
#17322=EDGE_CURVE('',#13903,#13904,#7626,.T.);
#17323=EDGE_CURVE('',#13904,#13902,#7627,.T.);
#17324=EDGE_CURVE('',#13905,#13903,#7628,.T.);
#17325=EDGE_CURVE('',#13905,#13906,#7629,.T.);
#17326=EDGE_CURVE('',#13906,#13904,#7630,.T.);
#17327=EDGE_CURVE('',#13907,#13905,#7631,.T.);
#17328=EDGE_CURVE('',#13907,#13908,#7632,.T.);
#17329=EDGE_CURVE('',#13908,#13906,#7633,.T.);
#17330=EDGE_CURVE('',#13909,#13907,#7634,.T.);
#17331=EDGE_CURVE('',#13909,#13910,#7635,.T.);
#17332=EDGE_CURVE('',#13910,#13908,#7636,.T.);
#17333=EDGE_CURVE('',#13911,#13909,#7637,.T.);
#17334=EDGE_CURVE('',#13911,#13912,#7638,.T.);
#17335=EDGE_CURVE('',#13912,#13910,#7639,.T.);
#17336=EDGE_CURVE('',#13913,#13911,#7640,.T.);
#17337=EDGE_CURVE('',#13913,#13914,#7641,.T.);
#17338=EDGE_CURVE('',#13914,#13912,#7642,.T.);
#17339=EDGE_CURVE('',#13915,#13913,#7643,.T.);
#17340=EDGE_CURVE('',#13915,#13916,#7644,.T.);
#17341=EDGE_CURVE('',#13916,#13914,#7645,.T.);
#17342=EDGE_CURVE('',#13896,#13915,#7646,.T.);
#17343=EDGE_CURVE('',#13898,#13916,#7647,.T.);
#17344=EDGE_CURVE('',#13917,#13918,#860,.T.);
#17345=EDGE_CURVE('',#13917,#13919,#7648,.T.);
#17346=EDGE_CURVE('',#13919,#13920,#861,.T.);
#17347=EDGE_CURVE('',#13918,#13920,#7649,.T.);
#17348=EDGE_CURVE('',#13921,#13917,#862,.T.);
#17349=EDGE_CURVE('',#13921,#13922,#7650,.T.);
#17350=EDGE_CURVE('',#13922,#13919,#863,.T.);
#17351=EDGE_CURVE('',#13923,#13921,#864,.T.);
#17352=EDGE_CURVE('',#13923,#13924,#7651,.T.);
#17353=EDGE_CURVE('',#13924,#13922,#865,.T.);
#17354=EDGE_CURVE('',#13925,#13923,#866,.T.);
#17355=EDGE_CURVE('',#13925,#13926,#7652,.T.);
#17356=EDGE_CURVE('',#13926,#13924,#867,.T.);
#17357=EDGE_CURVE('',#13927,#13925,#868,.T.);
#17358=EDGE_CURVE('',#13927,#13928,#7653,.T.);
#17359=EDGE_CURVE('',#13928,#13926,#869,.T.);
#17360=EDGE_CURVE('',#13929,#13927,#870,.T.);
#17361=EDGE_CURVE('',#13929,#13930,#7654,.T.);
#17362=EDGE_CURVE('',#13930,#13928,#871,.T.);
#17363=EDGE_CURVE('',#13931,#13929,#872,.T.);
#17364=EDGE_CURVE('',#13931,#13932,#7655,.T.);
#17365=EDGE_CURVE('',#13932,#13930,#873,.T.);
#17366=EDGE_CURVE('',#13918,#13931,#874,.T.);
#17367=EDGE_CURVE('',#13920,#13932,#875,.T.);
#17368=EDGE_CURVE('',#13933,#13934,#876,.T.);
#17369=EDGE_CURVE('',#13933,#13935,#7656,.T.);
#17370=EDGE_CURVE('',#13935,#13936,#877,.T.);
#17371=EDGE_CURVE('',#13934,#13936,#7657,.T.);
#17372=EDGE_CURVE('',#13937,#13933,#878,.T.);
#17373=EDGE_CURVE('',#13937,#13938,#7658,.T.);
#17374=EDGE_CURVE('',#13938,#13935,#879,.T.);
#17375=EDGE_CURVE('',#13939,#13937,#880,.T.);
#17376=EDGE_CURVE('',#13939,#13940,#7659,.T.);
#17377=EDGE_CURVE('',#13940,#13938,#881,.T.);
#17378=EDGE_CURVE('',#13941,#13939,#882,.T.);
#17379=EDGE_CURVE('',#13941,#13942,#7660,.T.);
#17380=EDGE_CURVE('',#13942,#13940,#883,.T.);
#17381=EDGE_CURVE('',#13943,#13941,#884,.T.);
#17382=EDGE_CURVE('',#13943,#13944,#7661,.T.);
#17383=EDGE_CURVE('',#13944,#13942,#885,.T.);
#17384=EDGE_CURVE('',#13945,#13943,#886,.T.);
#17385=EDGE_CURVE('',#13945,#13946,#7662,.T.);
#17386=EDGE_CURVE('',#13946,#13944,#887,.T.);
#17387=EDGE_CURVE('',#13947,#13945,#888,.T.);
#17388=EDGE_CURVE('',#13947,#13948,#7663,.T.);
#17389=EDGE_CURVE('',#13948,#13946,#889,.T.);
#17390=EDGE_CURVE('',#13949,#13947,#890,.T.);
#17391=EDGE_CURVE('',#13949,#13950,#7664,.T.);
#17392=EDGE_CURVE('',#13950,#13948,#891,.T.);
#17393=EDGE_CURVE('',#13951,#13949,#892,.T.);
#17394=EDGE_CURVE('',#13951,#13952,#7665,.T.);
#17395=EDGE_CURVE('',#13952,#13950,#893,.T.);
#17396=EDGE_CURVE('',#13953,#13951,#894,.T.);
#17397=EDGE_CURVE('',#13953,#13954,#7666,.T.);
#17398=EDGE_CURVE('',#13954,#13952,#895,.T.);
#17399=EDGE_CURVE('',#13955,#13953,#896,.T.);
#17400=EDGE_CURVE('',#13955,#13956,#7667,.T.);
#17401=EDGE_CURVE('',#13956,#13954,#897,.T.);
#17402=EDGE_CURVE('',#13934,#13955,#898,.T.);
#17403=EDGE_CURVE('',#13936,#13956,#899,.T.);
#17404=EDGE_CURVE('',#13957,#13958,#900,.T.);
#17405=EDGE_CURVE('',#13957,#13959,#7668,.T.);
#17406=EDGE_CURVE('',#13959,#13960,#901,.T.);
#17407=EDGE_CURVE('',#13958,#13960,#7669,.T.);
#17408=EDGE_CURVE('',#13961,#13957,#902,.T.);
#17409=EDGE_CURVE('',#13961,#13962,#7670,.T.);
#17410=EDGE_CURVE('',#13962,#13959,#903,.T.);
#17411=EDGE_CURVE('',#13963,#13961,#904,.T.);
#17412=EDGE_CURVE('',#13963,#13964,#7671,.T.);
#17413=EDGE_CURVE('',#13964,#13962,#905,.T.);
#17414=EDGE_CURVE('',#13965,#13963,#906,.T.);
#17415=EDGE_CURVE('',#13965,#13966,#7672,.T.);
#17416=EDGE_CURVE('',#13966,#13964,#907,.T.);
#17417=EDGE_CURVE('',#13967,#13965,#908,.T.);
#17418=EDGE_CURVE('',#13967,#13968,#7673,.T.);
#17419=EDGE_CURVE('',#13968,#13966,#909,.T.);
#17420=EDGE_CURVE('',#13969,#13967,#910,.T.);
#17421=EDGE_CURVE('',#13969,#13970,#7674,.T.);
#17422=EDGE_CURVE('',#13970,#13968,#911,.T.);
#17423=EDGE_CURVE('',#13971,#13969,#912,.T.);
#17424=EDGE_CURVE('',#13971,#13972,#7675,.T.);
#17425=EDGE_CURVE('',#13972,#13970,#913,.T.);
#17426=EDGE_CURVE('',#13973,#13971,#914,.T.);
#17427=EDGE_CURVE('',#13973,#13974,#7676,.T.);
#17428=EDGE_CURVE('',#13974,#13972,#915,.T.);
#17429=EDGE_CURVE('',#13975,#13973,#916,.T.);
#17430=EDGE_CURVE('',#13975,#13976,#7677,.T.);
#17431=EDGE_CURVE('',#13976,#13974,#917,.T.);
#17432=EDGE_CURVE('',#13977,#13975,#918,.T.);
#17433=EDGE_CURVE('',#13977,#13978,#7678,.T.);
#17434=EDGE_CURVE('',#13978,#13976,#919,.T.);
#17435=EDGE_CURVE('',#13979,#13977,#920,.T.);
#17436=EDGE_CURVE('',#13979,#13980,#7679,.T.);
#17437=EDGE_CURVE('',#13980,#13978,#921,.T.);
#17438=EDGE_CURVE('',#13981,#13979,#922,.T.);
#17439=EDGE_CURVE('',#13981,#13982,#7680,.T.);
#17440=EDGE_CURVE('',#13982,#13980,#923,.T.);
#17441=EDGE_CURVE('',#13983,#13981,#7681,.T.);
#17442=EDGE_CURVE('',#13983,#13984,#7682,.T.);
#17443=EDGE_CURVE('',#13984,#13982,#7683,.T.);
#17444=EDGE_CURVE('',#13985,#13983,#924,.T.);
#17445=EDGE_CURVE('',#13985,#13986,#7684,.T.);
#17446=EDGE_CURVE('',#13986,#13984,#925,.T.);
#17447=EDGE_CURVE('',#13987,#13985,#926,.T.);
#17448=EDGE_CURVE('',#13987,#13988,#7685,.T.);
#17449=EDGE_CURVE('',#13988,#13986,#927,.T.);
#17450=EDGE_CURVE('',#13989,#13987,#928,.T.);
#17451=EDGE_CURVE('',#13989,#13990,#7686,.T.);
#17452=EDGE_CURVE('',#13990,#13988,#929,.T.);
#17453=EDGE_CURVE('',#13991,#13989,#930,.T.);
#17454=EDGE_CURVE('',#13991,#13992,#7687,.T.);
#17455=EDGE_CURVE('',#13992,#13990,#931,.T.);
#17456=EDGE_CURVE('',#13993,#13991,#932,.T.);
#17457=EDGE_CURVE('',#13993,#13994,#7688,.T.);
#17458=EDGE_CURVE('',#13994,#13992,#933,.T.);
#17459=EDGE_CURVE('',#13995,#13993,#934,.T.);
#17460=EDGE_CURVE('',#13995,#13996,#7689,.T.);
#17461=EDGE_CURVE('',#13996,#13994,#935,.T.);
#17462=EDGE_CURVE('',#13997,#13995,#936,.T.);
#17463=EDGE_CURVE('',#13997,#13998,#7690,.T.);
#17464=EDGE_CURVE('',#13998,#13996,#937,.T.);
#17465=EDGE_CURVE('',#13999,#13997,#7691,.T.);
#17466=EDGE_CURVE('',#13999,#14000,#7692,.T.);
#17467=EDGE_CURVE('',#14000,#13998,#7693,.T.);
#17468=EDGE_CURVE('',#14001,#13999,#938,.T.);
#17469=EDGE_CURVE('',#14001,#14002,#7694,.T.);
#17470=EDGE_CURVE('',#14002,#14000,#939,.T.);
#17471=EDGE_CURVE('',#14003,#14001,#940,.T.);
#17472=EDGE_CURVE('',#14003,#14004,#7695,.T.);
#17473=EDGE_CURVE('',#14004,#14002,#941,.T.);
#17474=EDGE_CURVE('',#14005,#14003,#942,.T.);
#17475=EDGE_CURVE('',#14005,#14006,#7696,.T.);
#17476=EDGE_CURVE('',#14006,#14004,#943,.T.);
#17477=EDGE_CURVE('',#14007,#14005,#944,.T.);
#17478=EDGE_CURVE('',#14007,#14008,#7697,.T.);
#17479=EDGE_CURVE('',#14008,#14006,#945,.T.);
#17480=EDGE_CURVE('',#14009,#14007,#946,.T.);
#17481=EDGE_CURVE('',#14009,#14010,#7698,.T.);
#17482=EDGE_CURVE('',#14010,#14008,#947,.T.);
#17483=EDGE_CURVE('',#14011,#14009,#948,.T.);
#17484=EDGE_CURVE('',#14011,#14012,#7699,.T.);
#17485=EDGE_CURVE('',#14012,#14010,#949,.T.);
#17486=EDGE_CURVE('',#14013,#14011,#950,.T.);
#17487=EDGE_CURVE('',#14013,#14014,#7700,.T.);
#17488=EDGE_CURVE('',#14014,#14012,#951,.T.);
#17489=EDGE_CURVE('',#14015,#14013,#7701,.T.);
#17490=EDGE_CURVE('',#14015,#14016,#7702,.T.);
#17491=EDGE_CURVE('',#14016,#14014,#7703,.T.);
#17492=EDGE_CURVE('',#13958,#14015,#952,.T.);
#17493=EDGE_CURVE('',#13960,#14016,#953,.T.);
#17494=EDGE_CURVE('',#14017,#14018,#954,.T.);
#17495=EDGE_CURVE('',#14017,#14019,#7704,.T.);
#17496=EDGE_CURVE('',#14019,#14020,#955,.T.);
#17497=EDGE_CURVE('',#14018,#14020,#7705,.T.);
#17498=EDGE_CURVE('',#14021,#14017,#956,.T.);
#17499=EDGE_CURVE('',#14021,#14022,#7706,.T.);
#17500=EDGE_CURVE('',#14022,#14019,#957,.T.);
#17501=EDGE_CURVE('',#14023,#14021,#958,.T.);
#17502=EDGE_CURVE('',#14023,#14024,#7707,.T.);
#17503=EDGE_CURVE('',#14024,#14022,#959,.T.);
#17504=EDGE_CURVE('',#14025,#14023,#960,.T.);
#17505=EDGE_CURVE('',#14025,#14026,#7708,.T.);
#17506=EDGE_CURVE('',#14026,#14024,#961,.T.);
#17507=EDGE_CURVE('',#14027,#14025,#962,.T.);
#17508=EDGE_CURVE('',#14027,#14028,#7709,.T.);
#17509=EDGE_CURVE('',#14028,#14026,#963,.T.);
#17510=EDGE_CURVE('',#14029,#14027,#964,.T.);
#17511=EDGE_CURVE('',#14029,#14030,#7710,.T.);
#17512=EDGE_CURVE('',#14030,#14028,#965,.T.);
#17513=EDGE_CURVE('',#14031,#14029,#966,.T.);
#17514=EDGE_CURVE('',#14031,#14032,#7711,.T.);
#17515=EDGE_CURVE('',#14032,#14030,#967,.T.);
#17516=EDGE_CURVE('',#14018,#14031,#968,.T.);
#17517=EDGE_CURVE('',#14020,#14032,#969,.T.);
#17518=EDGE_CURVE('',#14033,#14034,#970,.T.);
#17519=EDGE_CURVE('',#14033,#14035,#7712,.T.);
#17520=EDGE_CURVE('',#14035,#14036,#971,.T.);
#17521=EDGE_CURVE('',#14034,#14036,#7713,.T.);
#17522=EDGE_CURVE('',#14037,#14033,#972,.T.);
#17523=EDGE_CURVE('',#14037,#14038,#7714,.T.);
#17524=EDGE_CURVE('',#14038,#14035,#973,.T.);
#17525=EDGE_CURVE('',#14039,#14037,#974,.T.);
#17526=EDGE_CURVE('',#14039,#14040,#7715,.T.);
#17527=EDGE_CURVE('',#14040,#14038,#975,.T.);
#17528=EDGE_CURVE('',#14041,#14039,#976,.T.);
#17529=EDGE_CURVE('',#14041,#14042,#7716,.T.);
#17530=EDGE_CURVE('',#14042,#14040,#977,.T.);
#17531=EDGE_CURVE('',#14043,#14041,#978,.T.);
#17532=EDGE_CURVE('',#14043,#14044,#7717,.T.);
#17533=EDGE_CURVE('',#14044,#14042,#979,.T.);
#17534=EDGE_CURVE('',#14045,#14043,#980,.T.);
#17535=EDGE_CURVE('',#14045,#14046,#7718,.T.);
#17536=EDGE_CURVE('',#14046,#14044,#981,.T.);
#17537=EDGE_CURVE('',#14047,#14045,#982,.T.);
#17538=EDGE_CURVE('',#14047,#14048,#7719,.T.);
#17539=EDGE_CURVE('',#14048,#14046,#983,.T.);
#17540=EDGE_CURVE('',#14049,#14047,#984,.T.);
#17541=EDGE_CURVE('',#14049,#14050,#7720,.T.);
#17542=EDGE_CURVE('',#14050,#14048,#985,.T.);
#17543=EDGE_CURVE('',#14051,#14049,#986,.T.);
#17544=EDGE_CURVE('',#14051,#14052,#7721,.T.);
#17545=EDGE_CURVE('',#14052,#14050,#987,.T.);
#17546=EDGE_CURVE('',#14053,#14051,#988,.T.);
#17547=EDGE_CURVE('',#14053,#14054,#7722,.T.);
#17548=EDGE_CURVE('',#14054,#14052,#989,.T.);
#17549=EDGE_CURVE('',#14055,#14053,#990,.T.);
#17550=EDGE_CURVE('',#14055,#14056,#7723,.T.);
#17551=EDGE_CURVE('',#14056,#14054,#991,.T.);
#17552=EDGE_CURVE('',#14034,#14055,#992,.T.);
#17553=EDGE_CURVE('',#14036,#14056,#993,.T.);
#17554=EDGE_CURVE('',#14057,#14058,#994,.T.);
#17555=EDGE_CURVE('',#14057,#14059,#7724,.T.);
#17556=EDGE_CURVE('',#14059,#14060,#995,.T.);
#17557=EDGE_CURVE('',#14058,#14060,#7725,.T.);
#17558=EDGE_CURVE('',#14061,#14057,#996,.T.);
#17559=EDGE_CURVE('',#14061,#14062,#7726,.T.);
#17560=EDGE_CURVE('',#14062,#14059,#997,.T.);
#17561=EDGE_CURVE('',#14063,#14061,#998,.T.);
#17562=EDGE_CURVE('',#14063,#14064,#7727,.T.);
#17563=EDGE_CURVE('',#14064,#14062,#999,.T.);
#17564=EDGE_CURVE('',#14065,#14063,#1000,.T.);
#17565=EDGE_CURVE('',#14065,#14066,#7728,.T.);
#17566=EDGE_CURVE('',#14066,#14064,#1001,.T.);
#17567=EDGE_CURVE('',#14067,#14065,#1002,.T.);
#17568=EDGE_CURVE('',#14067,#14068,#7729,.T.);
#17569=EDGE_CURVE('',#14068,#14066,#1003,.T.);
#17570=EDGE_CURVE('',#14069,#14067,#1004,.T.);
#17571=EDGE_CURVE('',#14069,#14070,#7730,.T.);
#17572=EDGE_CURVE('',#14070,#14068,#1005,.T.);
#17573=EDGE_CURVE('',#14071,#14069,#1006,.T.);
#17574=EDGE_CURVE('',#14071,#14072,#7731,.T.);
#17575=EDGE_CURVE('',#14072,#14070,#1007,.T.);
#17576=EDGE_CURVE('',#14073,#14071,#1008,.T.);
#17577=EDGE_CURVE('',#14073,#14074,#7732,.T.);
#17578=EDGE_CURVE('',#14074,#14072,#1009,.T.);
#17579=EDGE_CURVE('',#14075,#14073,#1010,.T.);
#17580=EDGE_CURVE('',#14075,#14076,#7733,.T.);
#17581=EDGE_CURVE('',#14076,#14074,#1011,.T.);
#17582=EDGE_CURVE('',#14077,#14075,#7734,.T.);
#17583=EDGE_CURVE('',#14077,#14078,#7735,.T.);
#17584=EDGE_CURVE('',#14078,#14076,#7736,.T.);
#17585=EDGE_CURVE('',#14079,#14077,#1012,.T.);
#17586=EDGE_CURVE('',#14079,#14080,#7737,.T.);
#17587=EDGE_CURVE('',#14080,#14078,#1013,.T.);
#17588=EDGE_CURVE('',#14081,#14079,#1014,.T.);
#17589=EDGE_CURVE('',#14081,#14082,#7738,.T.);
#17590=EDGE_CURVE('',#14082,#14080,#1015,.T.);
#17591=EDGE_CURVE('',#14083,#14081,#1016,.T.);
#17592=EDGE_CURVE('',#14083,#14084,#7739,.T.);
#17593=EDGE_CURVE('',#14084,#14082,#1017,.T.);
#17594=EDGE_CURVE('',#14085,#14083,#1018,.T.);
#17595=EDGE_CURVE('',#14085,#14086,#7740,.T.);
#17596=EDGE_CURVE('',#14086,#14084,#1019,.T.);
#17597=EDGE_CURVE('',#14087,#14085,#1020,.T.);
#17598=EDGE_CURVE('',#14087,#14088,#7741,.T.);
#17599=EDGE_CURVE('',#14088,#14086,#1021,.T.);
#17600=EDGE_CURVE('',#14089,#14087,#1022,.T.);
#17601=EDGE_CURVE('',#14089,#14090,#7742,.T.);
#17602=EDGE_CURVE('',#14090,#14088,#1023,.T.);
#17603=EDGE_CURVE('',#14091,#14089,#1024,.T.);
#17604=EDGE_CURVE('',#14091,#14092,#7743,.T.);
#17605=EDGE_CURVE('',#14092,#14090,#1025,.T.);
#17606=EDGE_CURVE('',#14093,#14091,#1026,.T.);
#17607=EDGE_CURVE('',#14093,#14094,#7744,.T.);
#17608=EDGE_CURVE('',#14094,#14092,#1027,.T.);
#17609=EDGE_CURVE('',#14095,#14093,#1028,.T.);
#17610=EDGE_CURVE('',#14095,#14096,#7745,.T.);
#17611=EDGE_CURVE('',#14096,#14094,#1029,.T.);
#17612=EDGE_CURVE('',#14097,#14095,#7746,.T.);
#17613=EDGE_CURVE('',#14097,#14098,#7747,.T.);
#17614=EDGE_CURVE('',#14098,#14096,#7748,.T.);
#17615=EDGE_CURVE('',#14099,#14097,#7749,.T.);
#17616=EDGE_CURVE('',#14099,#14100,#7750,.T.);
#17617=EDGE_CURVE('',#14100,#14098,#7751,.T.);
#17618=EDGE_CURVE('',#14058,#14099,#7752,.T.);
#17619=EDGE_CURVE('',#14060,#14100,#7753,.T.);
#17620=EDGE_CURVE('',#14101,#14102,#1030,.T.);
#17621=EDGE_CURVE('',#14101,#14103,#7754,.T.);
#17622=EDGE_CURVE('',#14103,#14104,#1031,.T.);
#17623=EDGE_CURVE('',#14102,#14104,#7755,.T.);
#17624=EDGE_CURVE('',#14105,#14101,#1032,.T.);
#17625=EDGE_CURVE('',#14105,#14106,#7756,.T.);
#17626=EDGE_CURVE('',#14106,#14103,#1033,.T.);
#17627=EDGE_CURVE('',#14107,#14105,#1034,.T.);
#17628=EDGE_CURVE('',#14107,#14108,#7757,.T.);
#17629=EDGE_CURVE('',#14108,#14106,#1035,.T.);
#17630=EDGE_CURVE('',#14109,#14107,#1036,.T.);
#17631=EDGE_CURVE('',#14109,#14110,#7758,.T.);
#17632=EDGE_CURVE('',#14110,#14108,#1037,.T.);
#17633=EDGE_CURVE('',#14111,#14109,#1038,.T.);
#17634=EDGE_CURVE('',#14111,#14112,#7759,.T.);
#17635=EDGE_CURVE('',#14112,#14110,#1039,.T.);
#17636=EDGE_CURVE('',#14113,#14111,#1040,.T.);
#17637=EDGE_CURVE('',#14113,#14114,#7760,.T.);
#17638=EDGE_CURVE('',#14114,#14112,#1041,.T.);
#17639=EDGE_CURVE('',#14115,#14113,#1042,.T.);
#17640=EDGE_CURVE('',#14115,#14116,#7761,.T.);
#17641=EDGE_CURVE('',#14116,#14114,#1043,.T.);
#17642=EDGE_CURVE('',#14102,#14115,#1044,.T.);
#17643=EDGE_CURVE('',#14104,#14116,#1045,.T.);
#17644=EDGE_CURVE('',#14117,#14118,#1046,.T.);
#17645=EDGE_CURVE('',#14117,#14119,#7762,.T.);
#17646=EDGE_CURVE('',#14119,#14120,#1047,.T.);
#17647=EDGE_CURVE('',#14118,#14120,#7763,.T.);
#17648=EDGE_CURVE('',#14121,#14117,#1048,.T.);
#17649=EDGE_CURVE('',#14121,#14122,#7764,.T.);
#17650=EDGE_CURVE('',#14122,#14119,#1049,.T.);
#17651=EDGE_CURVE('',#14123,#14121,#1050,.T.);
#17652=EDGE_CURVE('',#14123,#14124,#7765,.T.);
#17653=EDGE_CURVE('',#14124,#14122,#1051,.T.);
#17654=EDGE_CURVE('',#14125,#14123,#1052,.T.);
#17655=EDGE_CURVE('',#14125,#14126,#7766,.T.);
#17656=EDGE_CURVE('',#14126,#14124,#1053,.T.);
#17657=EDGE_CURVE('',#14127,#14125,#1054,.T.);
#17658=EDGE_CURVE('',#14127,#14128,#7767,.T.);
#17659=EDGE_CURVE('',#14128,#14126,#1055,.T.);
#17660=EDGE_CURVE('',#14129,#14127,#1056,.T.);
#17661=EDGE_CURVE('',#14129,#14130,#7768,.T.);
#17662=EDGE_CURVE('',#14130,#14128,#1057,.T.);
#17663=EDGE_CURVE('',#14131,#14129,#1058,.T.);
#17664=EDGE_CURVE('',#14131,#14132,#7769,.T.);
#17665=EDGE_CURVE('',#14132,#14130,#1059,.T.);
#17666=EDGE_CURVE('',#14133,#14131,#1060,.T.);
#17667=EDGE_CURVE('',#14133,#14134,#7770,.T.);
#17668=EDGE_CURVE('',#14134,#14132,#1061,.T.);
#17669=EDGE_CURVE('',#14135,#14133,#1062,.T.);
#17670=EDGE_CURVE('',#14135,#14136,#7771,.T.);
#17671=EDGE_CURVE('',#14136,#14134,#1063,.T.);
#17672=EDGE_CURVE('',#14137,#14135,#1064,.T.);
#17673=EDGE_CURVE('',#14137,#14138,#7772,.T.);
#17674=EDGE_CURVE('',#14138,#14136,#1065,.T.);
#17675=EDGE_CURVE('',#14139,#14137,#1066,.T.);
#17676=EDGE_CURVE('',#14139,#14140,#7773,.T.);
#17677=EDGE_CURVE('',#14140,#14138,#1067,.T.);
#17678=EDGE_CURVE('',#14118,#14139,#1068,.T.);
#17679=EDGE_CURVE('',#14120,#14140,#1069,.T.);
#17680=EDGE_CURVE('',#14141,#14142,#7774,.T.);
#17681=EDGE_CURVE('',#14141,#14143,#7775,.T.);
#17682=EDGE_CURVE('',#14143,#14144,#7776,.T.);
#17683=EDGE_CURVE('',#14142,#14144,#7777,.T.);
#17684=EDGE_CURVE('',#14145,#14141,#1070,.T.);
#17685=EDGE_CURVE('',#14145,#14146,#7778,.T.);
#17686=EDGE_CURVE('',#14146,#14143,#1071,.T.);
#17687=EDGE_CURVE('',#14147,#14145,#1072,.T.);
#17688=EDGE_CURVE('',#14147,#14148,#7779,.T.);
#17689=EDGE_CURVE('',#14148,#14146,#1073,.T.);
#17690=EDGE_CURVE('',#14149,#14147,#7780,.T.);
#17691=EDGE_CURVE('',#14149,#14150,#7781,.T.);
#17692=EDGE_CURVE('',#14150,#14148,#7782,.T.);
#17693=EDGE_CURVE('',#14151,#14149,#1074,.T.);
#17694=EDGE_CURVE('',#14151,#14152,#7783,.T.);
#17695=EDGE_CURVE('',#14152,#14150,#1075,.T.);
#17696=EDGE_CURVE('',#14153,#14151,#1076,.T.);
#17697=EDGE_CURVE('',#14153,#14154,#7784,.T.);
#17698=EDGE_CURVE('',#14154,#14152,#1077,.T.);
#17699=EDGE_CURVE('',#14155,#14153,#7785,.T.);
#17700=EDGE_CURVE('',#14155,#14156,#7786,.T.);
#17701=EDGE_CURVE('',#14156,#14154,#7787,.T.);
#17702=EDGE_CURVE('',#14157,#14155,#7788,.T.);
#17703=EDGE_CURVE('',#14157,#14158,#7789,.T.);
#17704=EDGE_CURVE('',#14158,#14156,#7790,.T.);
#17705=EDGE_CURVE('',#14142,#14157,#7791,.T.);
#17706=EDGE_CURVE('',#14144,#14158,#7792,.T.);
#17707=EDGE_CURVE('',#14159,#14160,#1078,.T.);
#17708=EDGE_CURVE('',#14159,#14161,#7793,.T.);
#17709=EDGE_CURVE('',#14161,#14162,#1079,.T.);
#17710=EDGE_CURVE('',#14160,#14162,#7794,.T.);
#17711=EDGE_CURVE('',#14163,#14159,#1080,.T.);
#17712=EDGE_CURVE('',#14163,#14164,#7795,.T.);
#17713=EDGE_CURVE('',#14164,#14161,#1081,.T.);
#17714=EDGE_CURVE('',#14165,#14163,#1082,.T.);
#17715=EDGE_CURVE('',#14165,#14166,#7796,.T.);
#17716=EDGE_CURVE('',#14166,#14164,#1083,.T.);
#17717=EDGE_CURVE('',#14167,#14165,#1084,.T.);
#17718=EDGE_CURVE('',#14167,#14168,#7797,.T.);
#17719=EDGE_CURVE('',#14168,#14166,#1085,.T.);
#17720=EDGE_CURVE('',#14169,#14167,#1086,.T.);
#17721=EDGE_CURVE('',#14169,#14170,#7798,.T.);
#17722=EDGE_CURVE('',#14170,#14168,#1087,.T.);
#17723=EDGE_CURVE('',#14171,#14169,#1088,.T.);
#17724=EDGE_CURVE('',#14171,#14172,#7799,.T.);
#17725=EDGE_CURVE('',#14172,#14170,#1089,.T.);
#17726=EDGE_CURVE('',#14173,#14171,#1090,.T.);
#17727=EDGE_CURVE('',#14173,#14174,#7800,.T.);
#17728=EDGE_CURVE('',#14174,#14172,#1091,.T.);
#17729=EDGE_CURVE('',#14160,#14173,#1092,.T.);
#17730=EDGE_CURVE('',#14162,#14174,#1093,.T.);
#17731=EDGE_CURVE('',#14175,#14176,#1094,.T.);
#17732=EDGE_CURVE('',#14175,#14177,#7801,.T.);
#17733=EDGE_CURVE('',#14177,#14178,#1095,.T.);
#17734=EDGE_CURVE('',#14176,#14178,#7802,.T.);
#17735=EDGE_CURVE('',#14179,#14175,#1096,.T.);
#17736=EDGE_CURVE('',#14179,#14180,#7803,.T.);
#17737=EDGE_CURVE('',#14180,#14177,#1097,.T.);
#17738=EDGE_CURVE('',#14181,#14179,#1098,.T.);
#17739=EDGE_CURVE('',#14181,#14182,#7804,.T.);
#17740=EDGE_CURVE('',#14182,#14180,#1099,.T.);
#17741=EDGE_CURVE('',#14183,#14181,#1100,.T.);
#17742=EDGE_CURVE('',#14183,#14184,#7805,.T.);
#17743=EDGE_CURVE('',#14184,#14182,#1101,.T.);
#17744=EDGE_CURVE('',#14185,#14183,#1102,.T.);
#17745=EDGE_CURVE('',#14185,#14186,#7806,.T.);
#17746=EDGE_CURVE('',#14186,#14184,#1103,.T.);
#17747=EDGE_CURVE('',#14187,#14185,#1104,.T.);
#17748=EDGE_CURVE('',#14187,#14188,#7807,.T.);
#17749=EDGE_CURVE('',#14188,#14186,#1105,.T.);
#17750=EDGE_CURVE('',#14189,#14187,#1106,.T.);
#17751=EDGE_CURVE('',#14189,#14190,#7808,.T.);
#17752=EDGE_CURVE('',#14190,#14188,#1107,.T.);
#17753=EDGE_CURVE('',#14191,#14189,#1108,.T.);
#17754=EDGE_CURVE('',#14191,#14192,#7809,.T.);
#17755=EDGE_CURVE('',#14192,#14190,#1109,.T.);
#17756=EDGE_CURVE('',#14193,#14191,#1110,.T.);
#17757=EDGE_CURVE('',#14193,#14194,#7810,.T.);
#17758=EDGE_CURVE('',#14194,#14192,#1111,.T.);
#17759=EDGE_CURVE('',#14195,#14193,#1112,.T.);
#17760=EDGE_CURVE('',#14195,#14196,#7811,.T.);
#17761=EDGE_CURVE('',#14196,#14194,#1113,.T.);
#17762=EDGE_CURVE('',#14197,#14195,#1114,.T.);
#17763=EDGE_CURVE('',#14197,#14198,#7812,.T.);
#17764=EDGE_CURVE('',#14198,#14196,#1115,.T.);
#17765=EDGE_CURVE('',#14176,#14197,#1116,.T.);
#17766=EDGE_CURVE('',#14178,#14198,#1117,.T.);
#17767=EDGE_CURVE('',#14199,#14200,#1118,.T.);
#17768=EDGE_CURVE('',#14199,#14201,#7813,.T.);
#17769=EDGE_CURVE('',#14201,#14202,#1119,.T.);
#17770=EDGE_CURVE('',#14200,#14202,#7814,.T.);
#17771=EDGE_CURVE('',#14203,#14199,#1120,.T.);
#17772=EDGE_CURVE('',#14203,#14204,#7815,.T.);
#17773=EDGE_CURVE('',#14204,#14201,#1121,.T.);
#17774=EDGE_CURVE('',#14205,#14203,#1122,.T.);
#17775=EDGE_CURVE('',#14205,#14206,#7816,.T.);
#17776=EDGE_CURVE('',#14206,#14204,#1123,.T.);
#17777=EDGE_CURVE('',#14207,#14205,#1124,.T.);
#17778=EDGE_CURVE('',#14207,#14208,#7817,.T.);
#17779=EDGE_CURVE('',#14208,#14206,#1125,.T.);
#17780=EDGE_CURVE('',#14209,#14207,#1126,.T.);
#17781=EDGE_CURVE('',#14209,#14210,#7818,.T.);
#17782=EDGE_CURVE('',#14210,#14208,#1127,.T.);
#17783=EDGE_CURVE('',#14211,#14209,#1128,.T.);
#17784=EDGE_CURVE('',#14211,#14212,#7819,.T.);
#17785=EDGE_CURVE('',#14212,#14210,#1129,.T.);
#17786=EDGE_CURVE('',#14213,#14211,#1130,.T.);
#17787=EDGE_CURVE('',#14213,#14214,#7820,.T.);
#17788=EDGE_CURVE('',#14214,#14212,#1131,.T.);
#17789=EDGE_CURVE('',#14200,#14213,#1132,.T.);
#17790=EDGE_CURVE('',#14202,#14214,#1133,.T.);
#17791=EDGE_CURVE('',#14215,#14216,#1134,.T.);
#17792=EDGE_CURVE('',#14215,#14217,#7821,.T.);
#17793=EDGE_CURVE('',#14217,#14218,#1135,.T.);
#17794=EDGE_CURVE('',#14216,#14218,#7822,.T.);
#17795=EDGE_CURVE('',#14219,#14215,#1136,.T.);
#17796=EDGE_CURVE('',#14219,#14220,#7823,.T.);
#17797=EDGE_CURVE('',#14220,#14217,#1137,.T.);
#17798=EDGE_CURVE('',#14221,#14219,#1138,.T.);
#17799=EDGE_CURVE('',#14221,#14222,#7824,.T.);
#17800=EDGE_CURVE('',#14222,#14220,#1139,.T.);
#17801=EDGE_CURVE('',#14223,#14221,#1140,.T.);
#17802=EDGE_CURVE('',#14223,#14224,#7825,.T.);
#17803=EDGE_CURVE('',#14224,#14222,#1141,.T.);
#17804=EDGE_CURVE('',#14225,#14223,#1142,.T.);
#17805=EDGE_CURVE('',#14225,#14226,#7826,.T.);
#17806=EDGE_CURVE('',#14226,#14224,#1143,.T.);
#17807=EDGE_CURVE('',#14227,#14225,#1144,.T.);
#17808=EDGE_CURVE('',#14227,#14228,#7827,.T.);
#17809=EDGE_CURVE('',#14228,#14226,#1145,.T.);
#17810=EDGE_CURVE('',#14229,#14227,#1146,.T.);
#17811=EDGE_CURVE('',#14229,#14230,#7828,.T.);
#17812=EDGE_CURVE('',#14230,#14228,#1147,.T.);
#17813=EDGE_CURVE('',#14231,#14229,#1148,.T.);
#17814=EDGE_CURVE('',#14231,#14232,#7829,.T.);
#17815=EDGE_CURVE('',#14232,#14230,#1149,.T.);
#17816=EDGE_CURVE('',#14233,#14231,#1150,.T.);
#17817=EDGE_CURVE('',#14233,#14234,#7830,.T.);
#17818=EDGE_CURVE('',#14234,#14232,#1151,.T.);
#17819=EDGE_CURVE('',#14235,#14233,#1152,.T.);
#17820=EDGE_CURVE('',#14235,#14236,#7831,.T.);
#17821=EDGE_CURVE('',#14236,#14234,#1153,.T.);
#17822=EDGE_CURVE('',#14237,#14235,#1154,.T.);
#17823=EDGE_CURVE('',#14237,#14238,#7832,.T.);
#17824=EDGE_CURVE('',#14238,#14236,#1155,.T.);
#17825=EDGE_CURVE('',#14216,#14237,#1156,.T.);
#17826=EDGE_CURVE('',#14218,#14238,#1157,.T.);
#17827=EDGE_CURVE('',#14239,#14240,#7833,.T.);
#17828=EDGE_CURVE('',#14239,#14241,#7834,.T.);
#17829=EDGE_CURVE('',#14241,#14242,#7835,.T.);
#17830=EDGE_CURVE('',#14240,#14242,#7836,.T.);
#17831=EDGE_CURVE('',#14243,#14239,#1158,.T.);
#17832=EDGE_CURVE('',#14243,#14244,#7837,.T.);
#17833=EDGE_CURVE('',#14244,#14241,#1159,.T.);
#17834=EDGE_CURVE('',#14245,#14243,#1160,.T.);
#17835=EDGE_CURVE('',#14245,#14246,#7838,.T.);
#17836=EDGE_CURVE('',#14246,#14244,#1161,.T.);
#17837=EDGE_CURVE('',#14247,#14245,#7839,.T.);
#17838=EDGE_CURVE('',#14247,#14248,#7840,.T.);
#17839=EDGE_CURVE('',#14248,#14246,#7841,.T.);
#17840=EDGE_CURVE('',#14249,#14247,#1162,.T.);
#17841=EDGE_CURVE('',#14249,#14250,#7842,.T.);
#17842=EDGE_CURVE('',#14250,#14248,#1163,.T.);
#17843=EDGE_CURVE('',#14251,#14249,#1164,.T.);
#17844=EDGE_CURVE('',#14251,#14252,#7843,.T.);
#17845=EDGE_CURVE('',#14252,#14250,#1165,.T.);
#17846=EDGE_CURVE('',#14253,#14251,#7844,.T.);
#17847=EDGE_CURVE('',#14253,#14254,#7845,.T.);
#17848=EDGE_CURVE('',#14254,#14252,#7846,.T.);
#17849=EDGE_CURVE('',#14255,#14253,#7847,.T.);
#17850=EDGE_CURVE('',#14255,#14256,#7848,.T.);
#17851=EDGE_CURVE('',#14256,#14254,#7849,.T.);
#17852=EDGE_CURVE('',#14240,#14255,#7850,.T.);
#17853=EDGE_CURVE('',#14242,#14256,#7851,.T.);
#17854=EDGE_CURVE('',#14257,#14258,#1166,.T.);
#17855=EDGE_CURVE('',#14257,#14259,#7852,.T.);
#17856=EDGE_CURVE('',#14259,#14260,#1167,.T.);
#17857=EDGE_CURVE('',#14258,#14260,#7853,.T.);
#17858=EDGE_CURVE('',#14261,#14257,#1168,.T.);
#17859=EDGE_CURVE('',#14261,#14262,#7854,.T.);
#17860=EDGE_CURVE('',#14262,#14259,#1169,.T.);
#17861=EDGE_CURVE('',#14263,#14261,#1170,.T.);
#17862=EDGE_CURVE('',#14263,#14264,#7855,.T.);
#17863=EDGE_CURVE('',#14264,#14262,#1171,.T.);
#17864=EDGE_CURVE('',#14265,#14263,#1172,.T.);
#17865=EDGE_CURVE('',#14265,#14266,#7856,.T.);
#17866=EDGE_CURVE('',#14266,#14264,#1173,.T.);
#17867=EDGE_CURVE('',#14267,#14265,#1174,.T.);
#17868=EDGE_CURVE('',#14267,#14268,#7857,.T.);
#17869=EDGE_CURVE('',#14268,#14266,#1175,.T.);
#17870=EDGE_CURVE('',#14269,#14267,#1176,.T.);
#17871=EDGE_CURVE('',#14269,#14270,#7858,.T.);
#17872=EDGE_CURVE('',#14270,#14268,#1177,.T.);
#17873=EDGE_CURVE('',#14271,#14269,#1178,.T.);
#17874=EDGE_CURVE('',#14271,#14272,#7859,.T.);
#17875=EDGE_CURVE('',#14272,#14270,#1179,.T.);
#17876=EDGE_CURVE('',#14258,#14271,#1180,.T.);
#17877=EDGE_CURVE('',#14260,#14272,#1181,.T.);
#17878=EDGE_CURVE('',#14273,#14274,#1182,.T.);
#17879=EDGE_CURVE('',#14273,#14275,#7860,.T.);
#17880=EDGE_CURVE('',#14275,#14276,#1183,.T.);
#17881=EDGE_CURVE('',#14274,#14276,#7861,.T.);
#17882=EDGE_CURVE('',#14277,#14273,#1184,.T.);
#17883=EDGE_CURVE('',#14277,#14278,#7862,.T.);
#17884=EDGE_CURVE('',#14278,#14275,#1185,.T.);
#17885=EDGE_CURVE('',#14279,#14277,#1186,.T.);
#17886=EDGE_CURVE('',#14279,#14280,#7863,.T.);
#17887=EDGE_CURVE('',#14280,#14278,#1187,.T.);
#17888=EDGE_CURVE('',#14281,#14279,#1188,.T.);
#17889=EDGE_CURVE('',#14281,#14282,#7864,.T.);
#17890=EDGE_CURVE('',#14282,#14280,#1189,.T.);
#17891=EDGE_CURVE('',#14283,#14281,#1190,.T.);
#17892=EDGE_CURVE('',#14283,#14284,#7865,.T.);
#17893=EDGE_CURVE('',#14284,#14282,#1191,.T.);
#17894=EDGE_CURVE('',#14285,#14283,#1192,.T.);
#17895=EDGE_CURVE('',#14285,#14286,#7866,.T.);
#17896=EDGE_CURVE('',#14286,#14284,#1193,.T.);
#17897=EDGE_CURVE('',#14287,#14285,#1194,.T.);
#17898=EDGE_CURVE('',#14287,#14288,#7867,.T.);
#17899=EDGE_CURVE('',#14288,#14286,#1195,.T.);
#17900=EDGE_CURVE('',#14289,#14287,#1196,.T.);
#17901=EDGE_CURVE('',#14289,#14290,#7868,.T.);
#17902=EDGE_CURVE('',#14290,#14288,#1197,.T.);
#17903=EDGE_CURVE('',#14291,#14289,#1198,.T.);
#17904=EDGE_CURVE('',#14291,#14292,#7869,.T.);
#17905=EDGE_CURVE('',#14292,#14290,#1199,.T.);
#17906=EDGE_CURVE('',#14293,#14291,#1200,.T.);
#17907=EDGE_CURVE('',#14293,#14294,#7870,.T.);
#17908=EDGE_CURVE('',#14294,#14292,#1201,.T.);
#17909=EDGE_CURVE('',#14295,#14293,#1202,.T.);
#17910=EDGE_CURVE('',#14295,#14296,#7871,.T.);
#17911=EDGE_CURVE('',#14296,#14294,#1203,.T.);
#17912=EDGE_CURVE('',#14274,#14295,#1204,.T.);
#17913=EDGE_CURVE('',#14276,#14296,#1205,.T.);
#17914=EDGE_CURVE('',#14297,#14298,#1206,.T.);
#17915=EDGE_CURVE('',#14297,#14299,#7872,.T.);
#17916=EDGE_CURVE('',#14299,#14300,#1207,.T.);
#17917=EDGE_CURVE('',#14298,#14300,#7873,.T.);
#17918=EDGE_CURVE('',#14301,#14297,#1208,.T.);
#17919=EDGE_CURVE('',#14301,#14302,#7874,.T.);
#17920=EDGE_CURVE('',#14302,#14299,#1209,.T.);
#17921=EDGE_CURVE('',#14303,#14301,#1210,.T.);
#17922=EDGE_CURVE('',#14303,#14304,#7875,.T.);
#17923=EDGE_CURVE('',#14304,#14302,#1211,.T.);
#17924=EDGE_CURVE('',#14305,#14303,#1212,.T.);
#17925=EDGE_CURVE('',#14305,#14306,#7876,.T.);
#17926=EDGE_CURVE('',#14306,#14304,#1213,.T.);
#17927=EDGE_CURVE('',#14307,#14305,#1214,.T.);
#17928=EDGE_CURVE('',#14307,#14308,#7877,.T.);
#17929=EDGE_CURVE('',#14308,#14306,#1215,.T.);
#17930=EDGE_CURVE('',#14309,#14307,#1216,.T.);
#17931=EDGE_CURVE('',#14309,#14310,#7878,.T.);
#17932=EDGE_CURVE('',#14310,#14308,#1217,.T.);
#17933=EDGE_CURVE('',#14311,#14309,#1218,.T.);
#17934=EDGE_CURVE('',#14311,#14312,#7879,.T.);
#17935=EDGE_CURVE('',#14312,#14310,#1219,.T.);
#17936=EDGE_CURVE('',#14313,#14311,#1220,.T.);
#17937=EDGE_CURVE('',#14313,#14314,#7880,.T.);
#17938=EDGE_CURVE('',#14314,#14312,#1221,.T.);
#17939=EDGE_CURVE('',#14315,#14313,#1222,.T.);
#17940=EDGE_CURVE('',#14315,#14316,#7881,.T.);
#17941=EDGE_CURVE('',#14316,#14314,#1223,.T.);
#17942=EDGE_CURVE('',#14317,#14315,#7882,.T.);
#17943=EDGE_CURVE('',#14317,#14318,#7883,.T.);
#17944=EDGE_CURVE('',#14318,#14316,#7884,.T.);
#17945=EDGE_CURVE('',#14319,#14317,#1224,.T.);
#17946=EDGE_CURVE('',#14319,#14320,#7885,.T.);
#17947=EDGE_CURVE('',#14320,#14318,#1225,.T.);
#17948=EDGE_CURVE('',#14321,#14319,#1226,.T.);
#17949=EDGE_CURVE('',#14321,#14322,#7886,.T.);
#17950=EDGE_CURVE('',#14322,#14320,#1227,.T.);
#17951=EDGE_CURVE('',#14323,#14321,#1228,.T.);
#17952=EDGE_CURVE('',#14323,#14324,#7887,.T.);
#17953=EDGE_CURVE('',#14324,#14322,#1229,.T.);
#17954=EDGE_CURVE('',#14325,#14323,#1230,.T.);
#17955=EDGE_CURVE('',#14325,#14326,#7888,.T.);
#17956=EDGE_CURVE('',#14326,#14324,#1231,.T.);
#17957=EDGE_CURVE('',#14327,#14325,#1232,.T.);
#17958=EDGE_CURVE('',#14327,#14328,#7889,.T.);
#17959=EDGE_CURVE('',#14328,#14326,#1233,.T.);
#17960=EDGE_CURVE('',#14329,#14327,#1234,.T.);
#17961=EDGE_CURVE('',#14329,#14330,#7890,.T.);
#17962=EDGE_CURVE('',#14330,#14328,#1235,.T.);
#17963=EDGE_CURVE('',#14331,#14329,#1236,.T.);
#17964=EDGE_CURVE('',#14331,#14332,#7891,.T.);
#17965=EDGE_CURVE('',#14332,#14330,#1237,.T.);
#17966=EDGE_CURVE('',#14333,#14331,#1238,.T.);
#17967=EDGE_CURVE('',#14333,#14334,#7892,.T.);
#17968=EDGE_CURVE('',#14334,#14332,#1239,.T.);
#17969=EDGE_CURVE('',#14335,#14333,#1240,.T.);
#17970=EDGE_CURVE('',#14335,#14336,#7893,.T.);
#17971=EDGE_CURVE('',#14336,#14334,#1241,.T.);
#17972=EDGE_CURVE('',#14337,#14335,#7894,.T.);
#17973=EDGE_CURVE('',#14337,#14338,#7895,.T.);
#17974=EDGE_CURVE('',#14338,#14336,#7896,.T.);
#17975=EDGE_CURVE('',#14339,#14337,#7897,.T.);
#17976=EDGE_CURVE('',#14339,#14340,#7898,.T.);
#17977=EDGE_CURVE('',#14340,#14338,#7899,.T.);
#17978=EDGE_CURVE('',#14298,#14339,#7900,.T.);
#17979=EDGE_CURVE('',#14300,#14340,#7901,.T.);
#17980=EDGE_CURVE('',#14341,#14342,#1242,.T.);
#17981=EDGE_CURVE('',#14341,#14343,#7902,.T.);
#17982=EDGE_CURVE('',#14343,#14344,#1243,.T.);
#17983=EDGE_CURVE('',#14342,#14344,#7903,.T.);
#17984=EDGE_CURVE('',#14345,#14341,#1244,.T.);
#17985=EDGE_CURVE('',#14345,#14346,#7904,.T.);
#17986=EDGE_CURVE('',#14346,#14343,#1245,.T.);
#17987=EDGE_CURVE('',#14347,#14345,#1246,.T.);
#17988=EDGE_CURVE('',#14347,#14348,#7905,.T.);
#17989=EDGE_CURVE('',#14348,#14346,#1247,.T.);
#17990=EDGE_CURVE('',#14349,#14347,#1248,.T.);
#17991=EDGE_CURVE('',#14349,#14350,#7906,.T.);
#17992=EDGE_CURVE('',#14350,#14348,#1249,.T.);
#17993=EDGE_CURVE('',#14351,#14349,#1250,.T.);
#17994=EDGE_CURVE('',#14351,#14352,#7907,.T.);
#17995=EDGE_CURVE('',#14352,#14350,#1251,.T.);
#17996=EDGE_CURVE('',#14353,#14351,#1252,.T.);
#17997=EDGE_CURVE('',#14353,#14354,#7908,.T.);
#17998=EDGE_CURVE('',#14354,#14352,#1253,.T.);
#17999=EDGE_CURVE('',#14355,#14353,#1254,.T.);
#18000=EDGE_CURVE('',#14355,#14356,#7909,.T.);
#18001=EDGE_CURVE('',#14356,#14354,#1255,.T.);
#18002=EDGE_CURVE('',#14342,#14355,#1256,.T.);
#18003=EDGE_CURVE('',#14344,#14356,#1257,.T.);
#18004=EDGE_CURVE('',#14357,#14358,#1258,.T.);
#18005=EDGE_CURVE('',#14357,#14359,#7910,.T.);
#18006=EDGE_CURVE('',#14359,#14360,#1259,.T.);
#18007=EDGE_CURVE('',#14358,#14360,#7911,.T.);
#18008=EDGE_CURVE('',#14361,#14357,#1260,.T.);
#18009=EDGE_CURVE('',#14361,#14362,#7912,.T.);
#18010=EDGE_CURVE('',#14362,#14359,#1261,.T.);
#18011=EDGE_CURVE('',#14363,#14361,#1262,.T.);
#18012=EDGE_CURVE('',#14363,#14364,#7913,.T.);
#18013=EDGE_CURVE('',#14364,#14362,#1263,.T.);
#18014=EDGE_CURVE('',#14365,#14363,#1264,.T.);
#18015=EDGE_CURVE('',#14365,#14366,#7914,.T.);
#18016=EDGE_CURVE('',#14366,#14364,#1265,.T.);
#18017=EDGE_CURVE('',#14367,#14365,#1266,.T.);
#18018=EDGE_CURVE('',#14367,#14368,#7915,.T.);
#18019=EDGE_CURVE('',#14368,#14366,#1267,.T.);
#18020=EDGE_CURVE('',#14369,#14367,#1268,.T.);
#18021=EDGE_CURVE('',#14369,#14370,#7916,.T.);
#18022=EDGE_CURVE('',#14370,#14368,#1269,.T.);
#18023=EDGE_CURVE('',#14371,#14369,#1270,.T.);
#18024=EDGE_CURVE('',#14371,#14372,#7917,.T.);
#18025=EDGE_CURVE('',#14372,#14370,#1271,.T.);
#18026=EDGE_CURVE('',#14373,#14371,#1272,.T.);
#18027=EDGE_CURVE('',#14373,#14374,#7918,.T.);
#18028=EDGE_CURVE('',#14374,#14372,#1273,.T.);
#18029=EDGE_CURVE('',#14375,#14373,#1274,.T.);
#18030=EDGE_CURVE('',#14375,#14376,#7919,.T.);
#18031=EDGE_CURVE('',#14376,#14374,#1275,.T.);
#18032=EDGE_CURVE('',#14377,#14375,#1276,.T.);
#18033=EDGE_CURVE('',#14377,#14378,#7920,.T.);
#18034=EDGE_CURVE('',#14378,#14376,#1277,.T.);
#18035=EDGE_CURVE('',#14379,#14377,#1278,.T.);
#18036=EDGE_CURVE('',#14379,#14380,#7921,.T.);
#18037=EDGE_CURVE('',#14380,#14378,#1279,.T.);
#18038=EDGE_CURVE('',#14358,#14379,#1280,.T.);
#18039=EDGE_CURVE('',#14360,#14380,#1281,.T.);
#18040=EDGE_CURVE('',#14381,#14382,#1282,.T.);
#18041=EDGE_CURVE('',#14381,#14383,#7922,.T.);
#18042=EDGE_CURVE('',#14383,#14384,#1283,.T.);
#18043=EDGE_CURVE('',#14382,#14384,#7923,.T.);
#18044=EDGE_CURVE('',#14385,#14381,#1284,.T.);
#18045=EDGE_CURVE('',#14385,#14386,#7924,.T.);
#18046=EDGE_CURVE('',#14386,#14383,#1285,.T.);
#18047=EDGE_CURVE('',#14387,#14385,#1286,.T.);
#18048=EDGE_CURVE('',#14387,#14388,#7925,.T.);
#18049=EDGE_CURVE('',#14388,#14386,#1287,.T.);
#18050=EDGE_CURVE('',#14389,#14387,#1288,.T.);
#18051=EDGE_CURVE('',#14389,#14390,#7926,.T.);
#18052=EDGE_CURVE('',#14390,#14388,#1289,.T.);
#18053=EDGE_CURVE('',#14391,#14389,#1290,.T.);
#18054=EDGE_CURVE('',#14391,#14392,#7927,.T.);
#18055=EDGE_CURVE('',#14392,#14390,#1291,.T.);
#18056=EDGE_CURVE('',#14393,#14391,#1292,.T.);
#18057=EDGE_CURVE('',#14393,#14394,#7928,.T.);
#18058=EDGE_CURVE('',#14394,#14392,#1293,.T.);
#18059=EDGE_CURVE('',#14395,#14393,#1294,.T.);
#18060=EDGE_CURVE('',#14395,#14396,#7929,.T.);
#18061=EDGE_CURVE('',#14396,#14394,#1295,.T.);
#18062=EDGE_CURVE('',#14397,#14395,#1296,.T.);
#18063=EDGE_CURVE('',#14397,#14398,#7930,.T.);
#18064=EDGE_CURVE('',#14398,#14396,#1297,.T.);
#18065=EDGE_CURVE('',#14399,#14397,#1298,.T.);
#18066=EDGE_CURVE('',#14399,#14400,#7931,.T.);
#18067=EDGE_CURVE('',#14400,#14398,#1299,.T.);
#18068=EDGE_CURVE('',#14401,#14399,#1300,.T.);
#18069=EDGE_CURVE('',#14401,#14402,#7932,.T.);
#18070=EDGE_CURVE('',#14402,#14400,#1301,.T.);
#18071=EDGE_CURVE('',#14403,#14401,#1302,.T.);
#18072=EDGE_CURVE('',#14403,#14404,#7933,.T.);
#18073=EDGE_CURVE('',#14404,#14402,#1303,.T.);
#18074=EDGE_CURVE('',#14405,#14403,#1304,.T.);
#18075=EDGE_CURVE('',#14405,#14406,#7934,.T.);
#18076=EDGE_CURVE('',#14406,#14404,#1305,.T.);
#18077=EDGE_CURVE('',#14407,#14405,#7935,.T.);
#18078=EDGE_CURVE('',#14407,#14408,#7936,.T.);
#18079=EDGE_CURVE('',#14408,#14406,#7937,.T.);
#18080=EDGE_CURVE('',#14409,#14407,#1306,.T.);
#18081=EDGE_CURVE('',#14409,#14410,#7938,.T.);
#18082=EDGE_CURVE('',#14410,#14408,#1307,.T.);
#18083=EDGE_CURVE('',#14411,#14409,#1308,.T.);
#18084=EDGE_CURVE('',#14411,#14412,#7939,.T.);
#18085=EDGE_CURVE('',#14412,#14410,#1309,.T.);
#18086=EDGE_CURVE('',#14413,#14411,#1310,.T.);
#18087=EDGE_CURVE('',#14413,#14414,#7940,.T.);
#18088=EDGE_CURVE('',#14414,#14412,#1311,.T.);
#18089=EDGE_CURVE('',#14415,#14413,#1312,.T.);
#18090=EDGE_CURVE('',#14415,#14416,#7941,.T.);
#18091=EDGE_CURVE('',#14416,#14414,#1313,.T.);
#18092=EDGE_CURVE('',#14417,#14415,#1314,.T.);
#18093=EDGE_CURVE('',#14417,#14418,#7942,.T.);
#18094=EDGE_CURVE('',#14418,#14416,#1315,.T.);
#18095=EDGE_CURVE('',#14419,#14417,#1316,.T.);
#18096=EDGE_CURVE('',#14419,#14420,#7943,.T.);
#18097=EDGE_CURVE('',#14420,#14418,#1317,.T.);
#18098=EDGE_CURVE('',#14421,#14419,#1318,.T.);
#18099=EDGE_CURVE('',#14421,#14422,#7944,.T.);
#18100=EDGE_CURVE('',#14422,#14420,#1319,.T.);
#18101=EDGE_CURVE('',#14423,#14421,#7945,.T.);
#18102=EDGE_CURVE('',#14423,#14424,#7946,.T.);
#18103=EDGE_CURVE('',#14424,#14422,#7947,.T.);
#18104=EDGE_CURVE('',#14425,#14423,#1320,.T.);
#18105=EDGE_CURVE('',#14425,#14426,#7948,.T.);
#18106=EDGE_CURVE('',#14426,#14424,#1321,.T.);
#18107=EDGE_CURVE('',#14427,#14425,#1322,.T.);
#18108=EDGE_CURVE('',#14427,#14428,#7949,.T.);
#18109=EDGE_CURVE('',#14428,#14426,#1323,.T.);
#18110=EDGE_CURVE('',#14429,#14427,#1324,.T.);
#18111=EDGE_CURVE('',#14429,#14430,#7950,.T.);
#18112=EDGE_CURVE('',#14430,#14428,#1325,.T.);
#18113=EDGE_CURVE('',#14431,#14429,#1326,.T.);
#18114=EDGE_CURVE('',#14431,#14432,#7951,.T.);
#18115=EDGE_CURVE('',#14432,#14430,#1327,.T.);
#18116=EDGE_CURVE('',#14433,#14431,#1328,.T.);
#18117=EDGE_CURVE('',#14433,#14434,#7952,.T.);
#18118=EDGE_CURVE('',#14434,#14432,#1329,.T.);
#18119=EDGE_CURVE('',#14435,#14433,#1330,.T.);
#18120=EDGE_CURVE('',#14435,#14436,#7953,.T.);
#18121=EDGE_CURVE('',#14436,#14434,#1331,.T.);
#18122=EDGE_CURVE('',#14437,#14435,#1332,.T.);
#18123=EDGE_CURVE('',#14437,#14438,#7954,.T.);
#18124=EDGE_CURVE('',#14438,#14436,#1333,.T.);
#18125=EDGE_CURVE('',#14439,#14437,#7955,.T.);
#18126=EDGE_CURVE('',#14439,#14440,#7956,.T.);
#18127=EDGE_CURVE('',#14440,#14438,#7957,.T.);
#18128=EDGE_CURVE('',#14382,#14439,#1334,.T.);
#18129=EDGE_CURVE('',#14384,#14440,#1335,.T.);
#18130=EDGE_CURVE('',#14441,#14442,#1336,.T.);
#18131=EDGE_CURVE('',#14441,#14443,#7958,.T.);
#18132=EDGE_CURVE('',#14443,#14444,#1337,.T.);
#18133=EDGE_CURVE('',#14442,#14444,#7959,.T.);
#18134=EDGE_CURVE('',#14445,#14441,#1338,.T.);
#18135=EDGE_CURVE('',#14445,#14446,#7960,.T.);
#18136=EDGE_CURVE('',#14446,#14443,#1339,.T.);
#18137=EDGE_CURVE('',#14447,#14445,#1340,.T.);
#18138=EDGE_CURVE('',#14447,#14448,#7961,.T.);
#18139=EDGE_CURVE('',#14448,#14446,#1341,.T.);
#18140=EDGE_CURVE('',#14449,#14447,#1342,.T.);
#18141=EDGE_CURVE('',#14449,#14450,#7962,.T.);
#18142=EDGE_CURVE('',#14450,#14448,#1343,.T.);
#18143=EDGE_CURVE('',#14451,#14449,#1344,.T.);
#18144=EDGE_CURVE('',#14451,#14452,#7963,.T.);
#18145=EDGE_CURVE('',#14452,#14450,#1345,.T.);
#18146=EDGE_CURVE('',#14453,#14451,#1346,.T.);
#18147=EDGE_CURVE('',#14453,#14454,#7964,.T.);
#18148=EDGE_CURVE('',#14454,#14452,#1347,.T.);
#18149=EDGE_CURVE('',#14455,#14453,#1348,.T.);
#18150=EDGE_CURVE('',#14455,#14456,#7965,.T.);
#18151=EDGE_CURVE('',#14456,#14454,#1349,.T.);
#18152=EDGE_CURVE('',#14442,#14455,#1350,.T.);
#18153=EDGE_CURVE('',#14444,#14456,#1351,.T.);
#18154=EDGE_CURVE('',#14457,#14458,#1352,.T.);
#18155=EDGE_CURVE('',#14457,#14459,#7966,.T.);
#18156=EDGE_CURVE('',#14459,#14460,#1353,.T.);
#18157=EDGE_CURVE('',#14458,#14460,#7967,.T.);
#18158=EDGE_CURVE('',#14461,#14457,#1354,.T.);
#18159=EDGE_CURVE('',#14461,#14462,#7968,.T.);
#18160=EDGE_CURVE('',#14462,#14459,#1355,.T.);
#18161=EDGE_CURVE('',#14463,#14461,#1356,.T.);
#18162=EDGE_CURVE('',#14463,#14464,#7969,.T.);
#18163=EDGE_CURVE('',#14464,#14462,#1357,.T.);
#18164=EDGE_CURVE('',#14465,#14463,#1358,.T.);
#18165=EDGE_CURVE('',#14465,#14466,#7970,.T.);
#18166=EDGE_CURVE('',#14466,#14464,#1359,.T.);
#18167=EDGE_CURVE('',#14467,#14465,#1360,.T.);
#18168=EDGE_CURVE('',#14467,#14468,#7971,.T.);
#18169=EDGE_CURVE('',#14468,#14466,#1361,.T.);
#18170=EDGE_CURVE('',#14469,#14467,#1362,.T.);
#18171=EDGE_CURVE('',#14469,#14470,#7972,.T.);
#18172=EDGE_CURVE('',#14470,#14468,#1363,.T.);
#18173=EDGE_CURVE('',#14471,#14469,#1364,.T.);
#18174=EDGE_CURVE('',#14471,#14472,#7973,.T.);
#18175=EDGE_CURVE('',#14472,#14470,#1365,.T.);
#18176=EDGE_CURVE('',#14473,#14471,#1366,.T.);
#18177=EDGE_CURVE('',#14473,#14474,#7974,.T.);
#18178=EDGE_CURVE('',#14474,#14472,#1367,.T.);
#18179=EDGE_CURVE('',#14475,#14473,#1368,.T.);
#18180=EDGE_CURVE('',#14475,#14476,#7975,.T.);
#18181=EDGE_CURVE('',#14476,#14474,#1369,.T.);
#18182=EDGE_CURVE('',#14477,#14475,#1370,.T.);
#18183=EDGE_CURVE('',#14477,#14478,#7976,.T.);
#18184=EDGE_CURVE('',#14478,#14476,#1371,.T.);
#18185=EDGE_CURVE('',#14479,#14477,#1372,.T.);
#18186=EDGE_CURVE('',#14479,#14480,#7977,.T.);
#18187=EDGE_CURVE('',#14480,#14478,#1373,.T.);
#18188=EDGE_CURVE('',#14458,#14479,#1374,.T.);
#18189=EDGE_CURVE('',#14460,#14480,#1375,.T.);
#18190=EDGE_CURVE('',#14481,#14482,#7978,.T.);
#18191=EDGE_CURVE('',#14481,#14483,#7979,.T.);
#18192=EDGE_CURVE('',#14483,#14484,#7980,.T.);
#18193=EDGE_CURVE('',#14482,#14484,#7981,.T.);
#18194=EDGE_CURVE('',#14485,#14481,#7982,.T.);
#18195=EDGE_CURVE('',#14485,#14486,#7983,.T.);
#18196=EDGE_CURVE('',#14486,#14483,#7984,.T.);
#18197=EDGE_CURVE('',#14482,#14485,#7985,.T.);
#18198=EDGE_CURVE('',#14484,#14486,#7986,.T.);
#18199=EDGE_CURVE('',#14487,#14488,#7987,.T.);
#18200=EDGE_CURVE('',#14487,#14489,#7988,.T.);
#18201=EDGE_CURVE('',#14489,#14490,#7989,.T.);
#18202=EDGE_CURVE('',#14488,#14490,#7990,.T.);
#18203=EDGE_CURVE('',#14491,#14487,#7991,.T.);
#18204=EDGE_CURVE('',#14491,#14492,#7992,.T.);
#18205=EDGE_CURVE('',#14492,#14489,#7993,.T.);
#18206=EDGE_CURVE('',#14493,#14491,#7994,.T.);
#18207=EDGE_CURVE('',#14493,#14494,#7995,.T.);
#18208=EDGE_CURVE('',#14494,#14492,#7996,.T.);
#18209=EDGE_CURVE('',#14495,#14493,#7997,.T.);
#18210=EDGE_CURVE('',#14495,#14496,#7998,.T.);
#18211=EDGE_CURVE('',#14496,#14494,#7999,.T.);
#18212=EDGE_CURVE('',#14497,#14495,#8000,.T.);
#18213=EDGE_CURVE('',#14497,#14498,#8001,.T.);
#18214=EDGE_CURVE('',#14498,#14496,#8002,.T.);
#18215=EDGE_CURVE('',#14499,#14497,#8003,.T.);
#18216=EDGE_CURVE('',#14499,#14500,#8004,.T.);
#18217=EDGE_CURVE('',#14500,#14498,#8005,.T.);
#18218=EDGE_CURVE('',#14501,#14499,#8006,.T.);
#18219=EDGE_CURVE('',#14501,#14502,#8007,.T.);
#18220=EDGE_CURVE('',#14502,#14500,#8008,.T.);
#18221=EDGE_CURVE('',#14503,#14501,#8009,.T.);
#18222=EDGE_CURVE('',#14503,#14504,#8010,.T.);
#18223=EDGE_CURVE('',#14504,#14502,#8011,.T.);
#18224=EDGE_CURVE('',#14505,#14503,#8012,.T.);
#18225=EDGE_CURVE('',#14505,#14506,#8013,.T.);
#18226=EDGE_CURVE('',#14506,#14504,#8014,.T.);
#18227=EDGE_CURVE('',#14507,#14505,#8015,.T.);
#18228=EDGE_CURVE('',#14507,#14508,#8016,.T.);
#18229=EDGE_CURVE('',#14508,#14506,#8017,.T.);
#18230=EDGE_CURVE('',#14488,#14507,#8018,.T.);
#18231=EDGE_CURVE('',#14490,#14508,#8019,.T.);
#18232=EDGE_CURVE('',#14509,#14510,#8020,.T.);
#18233=EDGE_CURVE('',#14509,#14511,#8021,.T.);
#18234=EDGE_CURVE('',#14511,#14512,#8022,.T.);
#18235=EDGE_CURVE('',#14510,#14512,#8023,.T.);
#18236=EDGE_CURVE('',#14513,#14509,#8024,.T.);
#18237=EDGE_CURVE('',#14513,#14514,#8025,.T.);
#18238=EDGE_CURVE('',#14514,#14511,#8026,.T.);
#18239=EDGE_CURVE('',#14515,#14513,#8027,.T.);
#18240=EDGE_CURVE('',#14515,#14516,#8028,.T.);
#18241=EDGE_CURVE('',#14516,#14514,#8029,.T.);
#18242=EDGE_CURVE('',#14510,#14515,#8030,.T.);
#18243=EDGE_CURVE('',#14512,#14516,#8031,.T.);
#18244=EDGE_CURVE('',#14517,#14518,#8032,.T.);
#18245=EDGE_CURVE('',#14517,#14519,#8033,.T.);
#18246=EDGE_CURVE('',#14519,#14520,#8034,.T.);
#18247=EDGE_CURVE('',#14518,#14520,#8035,.T.);
#18248=EDGE_CURVE('',#14521,#14517,#8036,.T.);
#18249=EDGE_CURVE('',#14521,#14522,#8037,.T.);
#18250=EDGE_CURVE('',#14522,#14519,#8038,.T.);
#18251=EDGE_CURVE('',#14523,#14521,#8039,.T.);
#18252=EDGE_CURVE('',#14523,#14524,#8040,.T.);
#18253=EDGE_CURVE('',#14524,#14522,#8041,.T.);
#18254=EDGE_CURVE('',#14518,#14523,#8042,.T.);
#18255=EDGE_CURVE('',#14520,#14524,#8043,.T.);
#18256=EDGE_CURVE('',#14525,#14526,#8044,.T.);
#18257=EDGE_CURVE('',#14525,#14527,#8045,.T.);
#18258=EDGE_CURVE('',#14527,#14528,#8046,.T.);
#18259=EDGE_CURVE('',#14526,#14528,#8047,.T.);
#18260=EDGE_CURVE('',#14529,#14525,#8048,.T.);
#18261=EDGE_CURVE('',#14529,#14530,#8049,.T.);
#18262=EDGE_CURVE('',#14530,#14527,#8050,.T.);
#18263=EDGE_CURVE('',#14531,#14529,#8051,.T.);
#18264=EDGE_CURVE('',#14531,#14532,#8052,.T.);
#18265=EDGE_CURVE('',#14532,#14530,#8053,.T.);
#18266=EDGE_CURVE('',#14526,#14531,#8054,.T.);
#18267=EDGE_CURVE('',#14528,#14532,#8055,.T.);
#18268=EDGE_CURVE('',#14533,#14534,#8056,.T.);
#18269=EDGE_CURVE('',#14533,#14535,#8057,.T.);
#18270=EDGE_CURVE('',#14535,#14536,#8058,.T.);
#18271=EDGE_CURVE('',#14534,#14536,#8059,.T.);
#18272=EDGE_CURVE('',#14537,#14533,#8060,.T.);
#18273=EDGE_CURVE('',#14537,#14538,#8061,.T.);
#18274=EDGE_CURVE('',#14538,#14535,#8062,.T.);
#18275=EDGE_CURVE('',#14539,#14537,#8063,.T.);
#18276=EDGE_CURVE('',#14539,#14540,#8064,.T.);
#18277=EDGE_CURVE('',#14540,#14538,#8065,.T.);
#18278=EDGE_CURVE('',#14534,#14539,#8066,.T.);
#18279=EDGE_CURVE('',#14536,#14540,#8067,.T.);
#18280=EDGE_CURVE('',#14541,#14542,#8068,.T.);
#18281=EDGE_CURVE('',#14541,#14543,#8069,.T.);
#18282=EDGE_CURVE('',#14543,#14544,#8070,.T.);
#18283=EDGE_CURVE('',#14542,#14544,#8071,.T.);
#18284=EDGE_CURVE('',#14545,#14541,#8072,.T.);
#18285=EDGE_CURVE('',#14545,#14546,#8073,.T.);
#18286=EDGE_CURVE('',#14546,#14543,#8074,.T.);
#18287=EDGE_CURVE('',#14547,#14545,#8075,.T.);
#18288=EDGE_CURVE('',#14547,#14548,#8076,.T.);
#18289=EDGE_CURVE('',#14548,#14546,#8077,.T.);
#18290=EDGE_CURVE('',#14542,#14547,#8078,.T.);
#18291=EDGE_CURVE('',#14544,#14548,#8079,.T.);
#18292=EDGE_CURVE('',#14549,#14550,#8080,.T.);
#18293=EDGE_CURVE('',#14549,#14551,#8081,.T.);
#18294=EDGE_CURVE('',#14551,#14552,#8082,.T.);
#18295=EDGE_CURVE('',#14550,#14552,#8083,.T.);
#18296=EDGE_CURVE('',#14553,#14549,#8084,.T.);
#18297=EDGE_CURVE('',#14553,#14554,#8085,.T.);
#18298=EDGE_CURVE('',#14554,#14551,#8086,.T.);
#18299=EDGE_CURVE('',#14555,#14553,#8087,.T.);
#18300=EDGE_CURVE('',#14555,#14556,#8088,.T.);
#18301=EDGE_CURVE('',#14556,#14554,#8089,.T.);
#18302=EDGE_CURVE('',#14550,#14555,#8090,.T.);
#18303=EDGE_CURVE('',#14552,#14556,#8091,.T.);
#18304=EDGE_CURVE('',#14557,#14558,#8092,.T.);
#18305=EDGE_CURVE('',#14557,#14559,#8093,.T.);
#18306=EDGE_CURVE('',#14559,#14560,#8094,.T.);
#18307=EDGE_CURVE('',#14558,#14560,#8095,.T.);
#18308=EDGE_CURVE('',#14561,#14557,#8096,.T.);
#18309=EDGE_CURVE('',#14561,#14562,#8097,.T.);
#18310=EDGE_CURVE('',#14562,#14559,#8098,.T.);
#18311=EDGE_CURVE('',#14563,#14561,#8099,.T.);
#18312=EDGE_CURVE('',#14563,#14564,#8100,.T.);
#18313=EDGE_CURVE('',#14564,#14562,#8101,.T.);
#18314=EDGE_CURVE('',#14558,#14563,#8102,.T.);
#18315=EDGE_CURVE('',#14560,#14564,#8103,.T.);
#18316=EDGE_CURVE('',#14565,#14566,#8104,.T.);
#18317=EDGE_CURVE('',#14565,#14567,#8105,.T.);
#18318=EDGE_CURVE('',#14567,#14568,#8106,.T.);
#18319=EDGE_CURVE('',#14566,#14568,#8107,.T.);
#18320=EDGE_CURVE('',#14569,#14565,#8108,.T.);
#18321=EDGE_CURVE('',#14569,#14570,#8109,.T.);
#18322=EDGE_CURVE('',#14570,#14567,#8110,.T.);
#18323=EDGE_CURVE('',#14571,#14569,#8111,.T.);
#18324=EDGE_CURVE('',#14571,#14572,#8112,.T.);
#18325=EDGE_CURVE('',#14572,#14570,#8113,.T.);
#18326=EDGE_CURVE('',#14566,#14571,#8114,.T.);
#18327=EDGE_CURVE('',#14568,#14572,#8115,.T.);
#18328=EDGE_CURVE('',#14573,#14574,#8116,.T.);
#18329=EDGE_CURVE('',#14573,#14575,#8117,.T.);
#18330=EDGE_CURVE('',#14575,#14576,#8118,.T.);
#18331=EDGE_CURVE('',#14574,#14576,#8119,.T.);
#18332=EDGE_CURVE('',#14577,#14573,#8120,.T.);
#18333=EDGE_CURVE('',#14577,#14578,#8121,.T.);
#18334=EDGE_CURVE('',#14578,#14575,#8122,.T.);
#18335=EDGE_CURVE('',#14579,#14577,#8123,.T.);
#18336=EDGE_CURVE('',#14579,#14580,#8124,.T.);
#18337=EDGE_CURVE('',#14580,#14578,#8125,.T.);
#18338=EDGE_CURVE('',#14574,#14579,#8126,.T.);
#18339=EDGE_CURVE('',#14576,#14580,#8127,.T.);
#18340=EDGE_CURVE('',#14581,#14582,#8128,.T.);
#18341=EDGE_CURVE('',#14581,#14583,#8129,.T.);
#18342=EDGE_CURVE('',#14583,#14584,#8130,.T.);
#18343=EDGE_CURVE('',#14582,#14584,#8131,.T.);
#18344=EDGE_CURVE('',#14585,#14581,#8132,.T.);
#18345=EDGE_CURVE('',#14585,#14586,#8133,.T.);
#18346=EDGE_CURVE('',#14586,#14583,#8134,.T.);
#18347=EDGE_CURVE('',#14587,#14585,#8135,.T.);
#18348=EDGE_CURVE('',#14587,#14588,#8136,.T.);
#18349=EDGE_CURVE('',#14588,#14586,#8137,.T.);
#18350=EDGE_CURVE('',#14582,#14587,#8138,.T.);
#18351=EDGE_CURVE('',#14584,#14588,#8139,.T.);
#18352=EDGE_CURVE('',#14589,#14590,#8140,.T.);
#18353=EDGE_CURVE('',#14589,#14591,#8141,.T.);
#18354=EDGE_CURVE('',#14591,#14592,#8142,.T.);
#18355=EDGE_CURVE('',#14590,#14592,#8143,.T.);
#18356=EDGE_CURVE('',#14593,#14589,#8144,.T.);
#18357=EDGE_CURVE('',#14593,#14594,#8145,.T.);
#18358=EDGE_CURVE('',#14594,#14591,#8146,.T.);
#18359=EDGE_CURVE('',#14595,#14593,#8147,.T.);
#18360=EDGE_CURVE('',#14595,#14596,#8148,.T.);
#18361=EDGE_CURVE('',#14596,#14594,#8149,.T.);
#18362=EDGE_CURVE('',#14590,#14595,#8150,.T.);
#18363=EDGE_CURVE('',#14592,#14596,#8151,.T.);
#18364=EDGE_CURVE('',#14597,#14598,#8152,.T.);
#18365=EDGE_CURVE('',#14597,#14599,#8153,.T.);
#18366=EDGE_CURVE('',#14599,#14600,#8154,.T.);
#18367=EDGE_CURVE('',#14598,#14600,#8155,.T.);
#18368=EDGE_CURVE('',#14601,#14597,#8156,.T.);
#18369=EDGE_CURVE('',#14601,#14602,#8157,.T.);
#18370=EDGE_CURVE('',#14602,#14599,#8158,.T.);
#18371=EDGE_CURVE('',#14603,#14601,#8159,.T.);
#18372=EDGE_CURVE('',#14603,#14604,#8160,.T.);
#18373=EDGE_CURVE('',#14604,#14602,#8161,.T.);
#18374=EDGE_CURVE('',#14598,#14603,#8162,.T.);
#18375=EDGE_CURVE('',#14600,#14604,#8163,.T.);
#18376=EDGE_CURVE('',#14605,#14606,#8164,.T.);
#18377=EDGE_CURVE('',#14605,#14607,#8165,.T.);
#18378=EDGE_CURVE('',#14607,#14608,#8166,.T.);
#18379=EDGE_CURVE('',#14606,#14608,#8167,.T.);
#18380=EDGE_CURVE('',#14609,#14605,#8168,.T.);
#18381=EDGE_CURVE('',#14609,#14610,#8169,.T.);
#18382=EDGE_CURVE('',#14610,#14607,#8170,.T.);
#18383=EDGE_CURVE('',#14611,#14609,#8171,.T.);
#18384=EDGE_CURVE('',#14611,#14612,#8172,.T.);
#18385=EDGE_CURVE('',#14612,#14610,#8173,.T.);
#18386=EDGE_CURVE('',#14606,#14611,#8174,.T.);
#18387=EDGE_CURVE('',#14608,#14612,#8175,.T.);
#18388=EDGE_CURVE('',#14613,#14614,#8176,.T.);
#18389=EDGE_CURVE('',#14613,#14615,#8177,.T.);
#18390=EDGE_CURVE('',#14615,#14616,#8178,.T.);
#18391=EDGE_CURVE('',#14614,#14616,#8179,.T.);
#18392=EDGE_CURVE('',#14617,#14613,#8180,.T.);
#18393=EDGE_CURVE('',#14617,#14618,#8181,.T.);
#18394=EDGE_CURVE('',#14618,#14615,#8182,.T.);
#18395=EDGE_CURVE('',#14619,#14617,#8183,.T.);
#18396=EDGE_CURVE('',#14619,#14620,#8184,.T.);
#18397=EDGE_CURVE('',#14620,#14618,#8185,.T.);
#18398=EDGE_CURVE('',#14614,#14619,#8186,.T.);
#18399=EDGE_CURVE('',#14616,#14620,#8187,.T.);
#18400=EDGE_CURVE('',#14621,#14622,#8188,.T.);
#18401=EDGE_CURVE('',#14621,#14623,#8189,.T.);
#18402=EDGE_CURVE('',#14623,#14624,#8190,.T.);
#18403=EDGE_CURVE('',#14622,#14624,#8191,.T.);
#18404=EDGE_CURVE('',#14625,#14621,#8192,.T.);
#18405=EDGE_CURVE('',#14625,#14626,#8193,.T.);
#18406=EDGE_CURVE('',#14626,#14623,#8194,.T.);
#18407=EDGE_CURVE('',#14627,#14625,#8195,.T.);
#18408=EDGE_CURVE('',#14627,#14628,#8196,.T.);
#18409=EDGE_CURVE('',#14628,#14626,#8197,.T.);
#18410=EDGE_CURVE('',#14622,#14627,#8198,.T.);
#18411=EDGE_CURVE('',#14624,#14628,#8199,.T.);
#18412=EDGE_CURVE('',#14629,#14630,#8200,.T.);
#18413=EDGE_CURVE('',#14629,#14631,#8201,.T.);
#18414=EDGE_CURVE('',#14631,#14632,#8202,.T.);
#18415=EDGE_CURVE('',#14630,#14632,#8203,.T.);
#18416=EDGE_CURVE('',#14633,#14629,#8204,.T.);
#18417=EDGE_CURVE('',#14633,#14634,#8205,.T.);
#18418=EDGE_CURVE('',#14634,#14631,#8206,.T.);
#18419=EDGE_CURVE('',#14635,#14633,#8207,.T.);
#18420=EDGE_CURVE('',#14635,#14636,#8208,.T.);
#18421=EDGE_CURVE('',#14636,#14634,#8209,.T.);
#18422=EDGE_CURVE('',#14630,#14635,#8210,.T.);
#18423=EDGE_CURVE('',#14632,#14636,#8211,.T.);
#18424=EDGE_CURVE('',#14637,#14638,#8212,.T.);
#18425=EDGE_CURVE('',#14637,#14639,#8213,.T.);
#18426=EDGE_CURVE('',#14639,#14640,#8214,.T.);
#18427=EDGE_CURVE('',#14638,#14640,#8215,.T.);
#18428=EDGE_CURVE('',#14641,#14637,#8216,.T.);
#18429=EDGE_CURVE('',#14641,#14642,#8217,.T.);
#18430=EDGE_CURVE('',#14642,#14639,#8218,.T.);
#18431=EDGE_CURVE('',#14643,#14641,#8219,.T.);
#18432=EDGE_CURVE('',#14643,#14644,#8220,.T.);
#18433=EDGE_CURVE('',#14644,#14642,#8221,.T.);
#18434=EDGE_CURVE('',#14638,#14643,#8222,.T.);
#18435=EDGE_CURVE('',#14640,#14644,#8223,.T.);
#18436=EDGE_CURVE('',#14645,#14646,#8224,.T.);
#18437=EDGE_CURVE('',#14645,#14647,#8225,.T.);
#18438=EDGE_CURVE('',#14647,#14648,#8226,.T.);
#18439=EDGE_CURVE('',#14646,#14648,#8227,.T.);
#18440=EDGE_CURVE('',#14649,#14645,#8228,.T.);
#18441=EDGE_CURVE('',#14649,#14650,#8229,.T.);
#18442=EDGE_CURVE('',#14650,#14647,#8230,.T.);
#18443=EDGE_CURVE('',#14651,#14649,#8231,.T.);
#18444=EDGE_CURVE('',#14651,#14652,#8232,.T.);
#18445=EDGE_CURVE('',#14652,#14650,#8233,.T.);
#18446=EDGE_CURVE('',#14646,#14651,#8234,.T.);
#18447=EDGE_CURVE('',#14648,#14652,#8235,.T.);
#18448=EDGE_CURVE('',#14653,#14654,#8236,.T.);
#18449=EDGE_CURVE('',#14653,#14655,#8237,.T.);
#18450=EDGE_CURVE('',#14655,#14656,#8238,.T.);
#18451=EDGE_CURVE('',#14654,#14656,#8239,.T.);
#18452=EDGE_CURVE('',#14657,#14653,#8240,.T.);
#18453=EDGE_CURVE('',#14657,#14658,#8241,.T.);
#18454=EDGE_CURVE('',#14658,#14655,#8242,.T.);
#18455=EDGE_CURVE('',#14659,#14657,#8243,.T.);
#18456=EDGE_CURVE('',#14659,#14660,#8244,.T.);
#18457=EDGE_CURVE('',#14660,#14658,#8245,.T.);
#18458=EDGE_CURVE('',#14654,#14659,#8246,.T.);
#18459=EDGE_CURVE('',#14656,#14660,#8247,.T.);
#18460=EDGE_CURVE('',#14661,#14662,#8248,.T.);
#18461=EDGE_CURVE('',#14661,#14663,#8249,.T.);
#18462=EDGE_CURVE('',#14663,#14664,#8250,.T.);
#18463=EDGE_CURVE('',#14662,#14664,#8251,.T.);
#18464=EDGE_CURVE('',#14665,#14661,#8252,.T.);
#18465=EDGE_CURVE('',#14665,#14666,#8253,.T.);
#18466=EDGE_CURVE('',#14666,#14663,#8254,.T.);
#18467=EDGE_CURVE('',#14667,#14665,#8255,.T.);
#18468=EDGE_CURVE('',#14667,#14668,#8256,.T.);
#18469=EDGE_CURVE('',#14668,#14666,#8257,.T.);
#18470=EDGE_CURVE('',#14662,#14667,#8258,.T.);
#18471=EDGE_CURVE('',#14664,#14668,#8259,.T.);
#18472=EDGE_CURVE('',#14669,#14670,#8260,.T.);
#18473=EDGE_CURVE('',#14669,#14671,#8261,.T.);
#18474=EDGE_CURVE('',#14671,#14672,#8262,.T.);
#18475=EDGE_CURVE('',#14670,#14672,#8263,.T.);
#18476=EDGE_CURVE('',#14673,#14669,#8264,.T.);
#18477=EDGE_CURVE('',#14673,#14674,#8265,.T.);
#18478=EDGE_CURVE('',#14674,#14671,#8266,.T.);
#18479=EDGE_CURVE('',#14675,#14673,#8267,.T.);
#18480=EDGE_CURVE('',#14675,#14676,#8268,.T.);
#18481=EDGE_CURVE('',#14676,#14674,#8269,.T.);
#18482=EDGE_CURVE('',#14670,#14675,#8270,.T.);
#18483=EDGE_CURVE('',#14672,#14676,#8271,.T.);
#18484=EDGE_CURVE('',#14677,#14678,#8272,.T.);
#18485=EDGE_CURVE('',#14677,#14679,#8273,.T.);
#18486=EDGE_CURVE('',#14679,#14680,#8274,.T.);
#18487=EDGE_CURVE('',#14678,#14680,#8275,.T.);
#18488=EDGE_CURVE('',#14681,#14677,#8276,.T.);
#18489=EDGE_CURVE('',#14681,#14682,#8277,.T.);
#18490=EDGE_CURVE('',#14682,#14679,#8278,.T.);
#18491=EDGE_CURVE('',#14683,#14681,#8279,.T.);
#18492=EDGE_CURVE('',#14683,#14684,#8280,.T.);
#18493=EDGE_CURVE('',#14684,#14682,#8281,.T.);
#18494=EDGE_CURVE('',#14678,#14683,#8282,.T.);
#18495=EDGE_CURVE('',#14680,#14684,#8283,.T.);
#18496=EDGE_CURVE('',#14685,#14686,#8284,.T.);
#18497=EDGE_CURVE('',#14685,#14687,#8285,.T.);
#18498=EDGE_CURVE('',#14687,#14688,#8286,.T.);
#18499=EDGE_CURVE('',#14686,#14688,#8287,.T.);
#18500=EDGE_CURVE('',#14689,#14685,#8288,.T.);
#18501=EDGE_CURVE('',#14689,#14690,#8289,.T.);
#18502=EDGE_CURVE('',#14690,#14687,#8290,.T.);
#18503=EDGE_CURVE('',#14691,#14689,#8291,.T.);
#18504=EDGE_CURVE('',#14691,#14692,#8292,.T.);
#18505=EDGE_CURVE('',#14692,#14690,#8293,.T.);
#18506=EDGE_CURVE('',#14686,#14691,#8294,.T.);
#18507=EDGE_CURVE('',#14688,#14692,#8295,.T.);
#18508=EDGE_CURVE('',#14693,#14694,#8296,.T.);
#18509=EDGE_CURVE('',#14693,#14695,#8297,.T.);
#18510=EDGE_CURVE('',#14695,#14696,#8298,.T.);
#18511=EDGE_CURVE('',#14694,#14696,#8299,.T.);
#18512=EDGE_CURVE('',#14697,#14693,#8300,.T.);
#18513=EDGE_CURVE('',#14697,#14698,#8301,.T.);
#18514=EDGE_CURVE('',#14698,#14695,#8302,.T.);
#18515=EDGE_CURVE('',#14699,#14697,#8303,.T.);
#18516=EDGE_CURVE('',#14699,#14700,#8304,.T.);
#18517=EDGE_CURVE('',#14700,#14698,#8305,.T.);
#18518=EDGE_CURVE('',#14694,#14699,#8306,.T.);
#18519=EDGE_CURVE('',#14696,#14700,#8307,.T.);
#18520=EDGE_CURVE('',#14701,#14702,#8308,.T.);
#18521=EDGE_CURVE('',#14701,#14703,#8309,.T.);
#18522=EDGE_CURVE('',#14703,#14704,#8310,.T.);
#18523=EDGE_CURVE('',#14702,#14704,#8311,.T.);
#18524=EDGE_CURVE('',#14705,#14701,#8312,.T.);
#18525=EDGE_CURVE('',#14705,#14706,#8313,.T.);
#18526=EDGE_CURVE('',#14706,#14703,#8314,.T.);
#18527=EDGE_CURVE('',#14707,#14705,#8315,.T.);
#18528=EDGE_CURVE('',#14707,#14708,#8316,.T.);
#18529=EDGE_CURVE('',#14708,#14706,#8317,.T.);
#18530=EDGE_CURVE('',#14702,#14707,#8318,.T.);
#18531=EDGE_CURVE('',#14704,#14708,#8319,.T.);
#18532=EDGE_CURVE('',#14709,#14710,#8320,.T.);
#18533=EDGE_CURVE('',#14709,#14711,#8321,.T.);
#18534=EDGE_CURVE('',#14711,#14712,#8322,.T.);
#18535=EDGE_CURVE('',#14710,#14712,#8323,.T.);
#18536=EDGE_CURVE('',#14713,#14709,#8324,.T.);
#18537=EDGE_CURVE('',#14713,#14714,#8325,.T.);
#18538=EDGE_CURVE('',#14714,#14711,#8326,.T.);
#18539=EDGE_CURVE('',#14715,#14713,#8327,.T.);
#18540=EDGE_CURVE('',#14715,#14716,#8328,.T.);
#18541=EDGE_CURVE('',#14716,#14714,#8329,.T.);
#18542=EDGE_CURVE('',#14710,#14715,#8330,.T.);
#18543=EDGE_CURVE('',#14712,#14716,#8331,.T.);
#18544=EDGE_CURVE('',#14717,#14718,#8332,.T.);
#18545=EDGE_CURVE('',#14717,#14719,#8333,.T.);
#18546=EDGE_CURVE('',#14719,#14720,#8334,.T.);
#18547=EDGE_CURVE('',#14718,#14720,#8335,.T.);
#18548=EDGE_CURVE('',#14721,#14717,#8336,.T.);
#18549=EDGE_CURVE('',#14721,#14722,#8337,.T.);
#18550=EDGE_CURVE('',#14722,#14719,#8338,.T.);
#18551=EDGE_CURVE('',#14723,#14721,#8339,.T.);
#18552=EDGE_CURVE('',#14723,#14724,#8340,.T.);
#18553=EDGE_CURVE('',#14724,#14722,#8341,.T.);
#18554=EDGE_CURVE('',#14718,#14723,#8342,.T.);
#18555=EDGE_CURVE('',#14720,#14724,#8343,.T.);
#18556=EDGE_CURVE('',#14725,#14726,#8344,.T.);
#18557=EDGE_CURVE('',#14725,#14727,#8345,.T.);
#18558=EDGE_CURVE('',#14727,#14728,#8346,.T.);
#18559=EDGE_CURVE('',#14726,#14728,#8347,.T.);
#18560=EDGE_CURVE('',#14729,#14725,#8348,.T.);
#18561=EDGE_CURVE('',#14729,#14730,#8349,.T.);
#18562=EDGE_CURVE('',#14730,#14727,#8350,.T.);
#18563=EDGE_CURVE('',#14731,#14729,#8351,.T.);
#18564=EDGE_CURVE('',#14731,#14732,#8352,.T.);
#18565=EDGE_CURVE('',#14732,#14730,#8353,.T.);
#18566=EDGE_CURVE('',#14726,#14731,#8354,.T.);
#18567=EDGE_CURVE('',#14728,#14732,#8355,.T.);
#18568=EDGE_CURVE('',#14733,#14734,#8356,.T.);
#18569=EDGE_CURVE('',#14733,#14735,#8357,.T.);
#18570=EDGE_CURVE('',#14735,#14736,#8358,.T.);
#18571=EDGE_CURVE('',#14734,#14736,#8359,.T.);
#18572=EDGE_CURVE('',#14737,#14733,#8360,.T.);
#18573=EDGE_CURVE('',#14737,#14738,#8361,.T.);
#18574=EDGE_CURVE('',#14738,#14735,#8362,.T.);
#18575=EDGE_CURVE('',#14739,#14737,#8363,.T.);
#18576=EDGE_CURVE('',#14739,#14740,#8364,.T.);
#18577=EDGE_CURVE('',#14740,#14738,#8365,.T.);
#18578=EDGE_CURVE('',#14734,#14739,#8366,.T.);
#18579=EDGE_CURVE('',#14736,#14740,#8367,.T.);
#18580=EDGE_CURVE('',#14741,#14742,#8368,.T.);
#18581=EDGE_CURVE('',#14741,#14743,#8369,.T.);
#18582=EDGE_CURVE('',#14743,#14744,#8370,.T.);
#18583=EDGE_CURVE('',#14742,#14744,#8371,.T.);
#18584=EDGE_CURVE('',#14745,#14741,#8372,.T.);
#18585=EDGE_CURVE('',#14745,#14746,#8373,.T.);
#18586=EDGE_CURVE('',#14746,#14743,#8374,.T.);
#18587=EDGE_CURVE('',#14747,#14745,#8375,.T.);
#18588=EDGE_CURVE('',#14747,#14748,#8376,.T.);
#18589=EDGE_CURVE('',#14748,#14746,#8377,.T.);
#18590=EDGE_CURVE('',#14742,#14747,#8378,.T.);
#18591=EDGE_CURVE('',#14744,#14748,#8379,.T.);
#18592=EDGE_CURVE('',#14749,#14750,#8380,.T.);
#18593=EDGE_CURVE('',#14749,#14751,#8381,.T.);
#18594=EDGE_CURVE('',#14751,#14752,#8382,.T.);
#18595=EDGE_CURVE('',#14750,#14752,#8383,.T.);
#18596=EDGE_CURVE('',#14753,#14749,#8384,.T.);
#18597=EDGE_CURVE('',#14753,#14754,#8385,.T.);
#18598=EDGE_CURVE('',#14754,#14751,#8386,.T.);
#18599=EDGE_CURVE('',#14755,#14753,#8387,.T.);
#18600=EDGE_CURVE('',#14755,#14756,#8388,.T.);
#18601=EDGE_CURVE('',#14756,#14754,#8389,.T.);
#18602=EDGE_CURVE('',#14750,#14755,#8390,.T.);
#18603=EDGE_CURVE('',#14752,#14756,#8391,.T.);
#18604=EDGE_CURVE('',#14757,#14758,#8392,.T.);
#18605=EDGE_CURVE('',#14757,#14759,#8393,.T.);
#18606=EDGE_CURVE('',#14759,#14760,#8394,.T.);
#18607=EDGE_CURVE('',#14758,#14760,#8395,.T.);
#18608=EDGE_CURVE('',#14761,#14757,#8396,.T.);
#18609=EDGE_CURVE('',#14761,#14762,#8397,.T.);
#18610=EDGE_CURVE('',#14762,#14759,#8398,.T.);
#18611=EDGE_CURVE('',#14763,#14761,#8399,.T.);
#18612=EDGE_CURVE('',#14763,#14764,#8400,.T.);
#18613=EDGE_CURVE('',#14764,#14762,#8401,.T.);
#18614=EDGE_CURVE('',#14758,#14763,#8402,.T.);
#18615=EDGE_CURVE('',#14760,#14764,#8403,.T.);
#18616=EDGE_CURVE('',#14765,#14766,#8404,.T.);
#18617=EDGE_CURVE('',#14765,#14767,#8405,.T.);
#18618=EDGE_CURVE('',#14767,#14768,#8406,.T.);
#18619=EDGE_CURVE('',#14766,#14768,#8407,.T.);
#18620=EDGE_CURVE('',#14769,#14765,#8408,.T.);
#18621=EDGE_CURVE('',#14769,#14770,#8409,.T.);
#18622=EDGE_CURVE('',#14770,#14767,#8410,.T.);
#18623=EDGE_CURVE('',#14771,#14769,#8411,.T.);
#18624=EDGE_CURVE('',#14771,#14772,#8412,.T.);
#18625=EDGE_CURVE('',#14772,#14770,#8413,.T.);
#18626=EDGE_CURVE('',#14766,#14771,#8414,.T.);
#18627=EDGE_CURVE('',#14768,#14772,#8415,.T.);
#18628=EDGE_CURVE('',#14773,#14774,#8416,.T.);
#18629=EDGE_CURVE('',#14773,#14775,#8417,.T.);
#18630=EDGE_CURVE('',#14775,#14776,#8418,.T.);
#18631=EDGE_CURVE('',#14774,#14776,#8419,.T.);
#18632=EDGE_CURVE('',#14777,#14773,#8420,.T.);
#18633=EDGE_CURVE('',#14777,#14778,#8421,.T.);
#18634=EDGE_CURVE('',#14778,#14775,#8422,.T.);
#18635=EDGE_CURVE('',#14779,#14777,#8423,.T.);
#18636=EDGE_CURVE('',#14779,#14780,#8424,.T.);
#18637=EDGE_CURVE('',#14780,#14778,#8425,.T.);
#18638=EDGE_CURVE('',#14774,#14779,#8426,.T.);
#18639=EDGE_CURVE('',#14776,#14780,#8427,.T.);
#18640=EDGE_CURVE('',#14781,#14782,#8428,.T.);
#18641=EDGE_CURVE('',#14781,#14783,#8429,.T.);
#18642=EDGE_CURVE('',#14783,#14784,#8430,.T.);
#18643=EDGE_CURVE('',#14782,#14784,#8431,.T.);
#18644=EDGE_CURVE('',#14785,#14781,#8432,.T.);
#18645=EDGE_CURVE('',#14785,#14786,#8433,.T.);
#18646=EDGE_CURVE('',#14786,#14783,#8434,.T.);
#18647=EDGE_CURVE('',#14787,#14785,#8435,.T.);
#18648=EDGE_CURVE('',#14787,#14788,#8436,.T.);
#18649=EDGE_CURVE('',#14788,#14786,#8437,.T.);
#18650=EDGE_CURVE('',#14782,#14787,#8438,.T.);
#18651=EDGE_CURVE('',#14784,#14788,#8439,.T.);
#18652=EDGE_CURVE('',#14789,#14790,#8440,.T.);
#18653=EDGE_CURVE('',#14789,#14791,#8441,.T.);
#18654=EDGE_CURVE('',#14791,#14792,#8442,.T.);
#18655=EDGE_CURVE('',#14790,#14792,#8443,.T.);
#18656=EDGE_CURVE('',#14793,#14789,#8444,.T.);
#18657=EDGE_CURVE('',#14793,#14794,#8445,.T.);
#18658=EDGE_CURVE('',#14794,#14791,#8446,.T.);
#18659=EDGE_CURVE('',#14795,#14793,#8447,.T.);
#18660=EDGE_CURVE('',#14795,#14796,#8448,.T.);
#18661=EDGE_CURVE('',#14796,#14794,#8449,.T.);
#18662=EDGE_CURVE('',#14790,#14795,#8450,.T.);
#18663=EDGE_CURVE('',#14792,#14796,#8451,.T.);
#18664=EDGE_CURVE('',#14797,#14798,#8452,.T.);
#18665=EDGE_CURVE('',#14797,#14799,#8453,.T.);
#18666=EDGE_CURVE('',#14799,#14800,#8454,.T.);
#18667=EDGE_CURVE('',#14798,#14800,#8455,.T.);
#18668=EDGE_CURVE('',#14801,#14797,#8456,.T.);
#18669=EDGE_CURVE('',#14801,#14802,#8457,.T.);
#18670=EDGE_CURVE('',#14802,#14799,#8458,.T.);
#18671=EDGE_CURVE('',#14803,#14801,#8459,.T.);
#18672=EDGE_CURVE('',#14803,#14804,#8460,.T.);
#18673=EDGE_CURVE('',#14804,#14802,#8461,.T.);
#18674=EDGE_CURVE('',#14798,#14803,#8462,.T.);
#18675=EDGE_CURVE('',#14800,#14804,#8463,.T.);
#18676=EDGE_CURVE('',#14805,#14806,#8464,.T.);
#18677=EDGE_CURVE('',#14805,#14807,#8465,.T.);
#18678=EDGE_CURVE('',#14807,#14808,#8466,.T.);
#18679=EDGE_CURVE('',#14806,#14808,#8467,.T.);
#18680=EDGE_CURVE('',#14809,#14805,#8468,.T.);
#18681=EDGE_CURVE('',#14809,#14810,#8469,.T.);
#18682=EDGE_CURVE('',#14810,#14807,#8470,.T.);
#18683=EDGE_CURVE('',#14811,#14809,#8471,.T.);
#18684=EDGE_CURVE('',#14811,#14812,#8472,.T.);
#18685=EDGE_CURVE('',#14812,#14810,#8473,.T.);
#18686=EDGE_CURVE('',#14806,#14811,#8474,.T.);
#18687=EDGE_CURVE('',#14808,#14812,#8475,.T.);
#18688=EDGE_CURVE('',#14813,#14814,#8476,.T.);
#18689=EDGE_CURVE('',#14813,#14815,#8477,.T.);
#18690=EDGE_CURVE('',#14815,#14816,#8478,.T.);
#18691=EDGE_CURVE('',#14814,#14816,#8479,.T.);
#18692=EDGE_CURVE('',#14817,#14813,#8480,.T.);
#18693=EDGE_CURVE('',#14817,#14818,#8481,.T.);
#18694=EDGE_CURVE('',#14818,#14815,#8482,.T.);
#18695=EDGE_CURVE('',#14819,#14817,#8483,.T.);
#18696=EDGE_CURVE('',#14819,#14820,#8484,.T.);
#18697=EDGE_CURVE('',#14820,#14818,#8485,.T.);
#18698=EDGE_CURVE('',#14814,#14819,#8486,.T.);
#18699=EDGE_CURVE('',#14816,#14820,#8487,.T.);
#18700=EDGE_CURVE('',#14821,#14822,#8488,.T.);
#18701=EDGE_CURVE('',#14821,#14823,#8489,.T.);
#18702=EDGE_CURVE('',#14823,#14824,#8490,.T.);
#18703=EDGE_CURVE('',#14822,#14824,#8491,.T.);
#18704=EDGE_CURVE('',#14825,#14821,#8492,.T.);
#18705=EDGE_CURVE('',#14825,#14826,#8493,.T.);
#18706=EDGE_CURVE('',#14826,#14823,#8494,.T.);
#18707=EDGE_CURVE('',#14827,#14825,#8495,.T.);
#18708=EDGE_CURVE('',#14827,#14828,#8496,.T.);
#18709=EDGE_CURVE('',#14828,#14826,#8497,.T.);
#18710=EDGE_CURVE('',#14822,#14827,#8498,.T.);
#18711=EDGE_CURVE('',#14824,#14828,#8499,.T.);
#18712=EDGE_CURVE('',#14829,#14830,#8500,.T.);
#18713=EDGE_CURVE('',#14829,#14831,#8501,.T.);
#18714=EDGE_CURVE('',#14831,#14832,#8502,.T.);
#18715=EDGE_CURVE('',#14830,#14832,#8503,.T.);
#18716=EDGE_CURVE('',#14833,#14829,#8504,.T.);
#18717=EDGE_CURVE('',#14833,#14834,#8505,.T.);
#18718=EDGE_CURVE('',#14834,#14831,#8506,.T.);
#18719=EDGE_CURVE('',#14835,#14833,#8507,.T.);
#18720=EDGE_CURVE('',#14835,#14836,#8508,.T.);
#18721=EDGE_CURVE('',#14836,#14834,#8509,.T.);
#18722=EDGE_CURVE('',#14830,#14835,#8510,.T.);
#18723=EDGE_CURVE('',#14832,#14836,#8511,.T.);
#18724=EDGE_CURVE('',#14837,#14838,#8512,.T.);
#18725=EDGE_CURVE('',#14837,#14839,#8513,.T.);
#18726=EDGE_CURVE('',#14839,#14840,#8514,.T.);
#18727=EDGE_CURVE('',#14838,#14840,#8515,.T.);
#18728=EDGE_CURVE('',#14841,#14837,#8516,.T.);
#18729=EDGE_CURVE('',#14841,#14842,#8517,.T.);
#18730=EDGE_CURVE('',#14842,#14839,#8518,.T.);
#18731=EDGE_CURVE('',#14843,#14841,#8519,.T.);
#18732=EDGE_CURVE('',#14843,#14844,#8520,.T.);
#18733=EDGE_CURVE('',#14844,#14842,#8521,.T.);
#18734=EDGE_CURVE('',#14838,#14843,#8522,.T.);
#18735=EDGE_CURVE('',#14840,#14844,#8523,.T.);
#18736=EDGE_CURVE('',#14845,#14846,#8524,.T.);
#18737=EDGE_CURVE('',#14845,#14847,#8525,.T.);
#18738=EDGE_CURVE('',#14847,#14848,#8526,.T.);
#18739=EDGE_CURVE('',#14846,#14848,#8527,.T.);
#18740=EDGE_CURVE('',#14849,#14845,#8528,.T.);
#18741=EDGE_CURVE('',#14849,#14850,#8529,.T.);
#18742=EDGE_CURVE('',#14850,#14847,#8530,.T.);
#18743=EDGE_CURVE('',#14851,#14849,#8531,.T.);
#18744=EDGE_CURVE('',#14851,#14852,#8532,.T.);
#18745=EDGE_CURVE('',#14852,#14850,#8533,.T.);
#18746=EDGE_CURVE('',#14846,#14851,#8534,.T.);
#18747=EDGE_CURVE('',#14848,#14852,#8535,.T.);
#18748=EDGE_CURVE('',#14853,#14854,#8536,.T.);
#18749=EDGE_CURVE('',#14853,#14855,#8537,.T.);
#18750=EDGE_CURVE('',#14855,#14856,#8538,.T.);
#18751=EDGE_CURVE('',#14854,#14856,#8539,.T.);
#18752=EDGE_CURVE('',#14857,#14853,#8540,.T.);
#18753=EDGE_CURVE('',#14857,#14858,#8541,.T.);
#18754=EDGE_CURVE('',#14858,#14855,#8542,.T.);
#18755=EDGE_CURVE('',#14859,#14857,#8543,.T.);
#18756=EDGE_CURVE('',#14859,#14860,#8544,.T.);
#18757=EDGE_CURVE('',#14860,#14858,#8545,.T.);
#18758=EDGE_CURVE('',#14854,#14859,#8546,.T.);
#18759=EDGE_CURVE('',#14856,#14860,#8547,.T.);
#18760=EDGE_CURVE('',#14861,#14862,#8548,.T.);
#18761=EDGE_CURVE('',#14861,#14863,#8549,.T.);
#18762=EDGE_CURVE('',#14863,#14864,#8550,.T.);
#18763=EDGE_CURVE('',#14862,#14864,#8551,.T.);
#18764=EDGE_CURVE('',#14865,#14861,#8552,.T.);
#18765=EDGE_CURVE('',#14865,#14866,#8553,.T.);
#18766=EDGE_CURVE('',#14866,#14863,#8554,.T.);
#18767=EDGE_CURVE('',#14867,#14865,#8555,.T.);
#18768=EDGE_CURVE('',#14867,#14868,#8556,.T.);
#18769=EDGE_CURVE('',#14868,#14866,#8557,.T.);
#18770=EDGE_CURVE('',#14862,#14867,#8558,.T.);
#18771=EDGE_CURVE('',#14864,#14868,#8559,.T.);
#18772=EDGE_CURVE('',#14869,#14870,#8560,.T.);
#18773=EDGE_CURVE('',#14869,#14871,#8561,.T.);
#18774=EDGE_CURVE('',#14871,#14872,#8562,.T.);
#18775=EDGE_CURVE('',#14870,#14872,#8563,.T.);
#18776=EDGE_CURVE('',#14873,#14869,#8564,.T.);
#18777=EDGE_CURVE('',#14873,#14874,#8565,.T.);
#18778=EDGE_CURVE('',#14874,#14871,#8566,.T.);
#18779=EDGE_CURVE('',#14875,#14873,#8567,.T.);
#18780=EDGE_CURVE('',#14875,#14876,#8568,.T.);
#18781=EDGE_CURVE('',#14876,#14874,#8569,.T.);
#18782=EDGE_CURVE('',#14870,#14875,#8570,.T.);
#18783=EDGE_CURVE('',#14872,#14876,#8571,.T.);
#18784=EDGE_CURVE('',#14877,#14878,#8572,.T.);
#18785=EDGE_CURVE('',#14877,#14879,#8573,.T.);
#18786=EDGE_CURVE('',#14879,#14880,#8574,.T.);
#18787=EDGE_CURVE('',#14878,#14880,#8575,.T.);
#18788=EDGE_CURVE('',#14881,#14877,#8576,.T.);
#18789=EDGE_CURVE('',#14881,#14882,#8577,.T.);
#18790=EDGE_CURVE('',#14882,#14879,#8578,.T.);
#18791=EDGE_CURVE('',#14883,#14881,#8579,.T.);
#18792=EDGE_CURVE('',#14883,#14884,#8580,.T.);
#18793=EDGE_CURVE('',#14884,#14882,#8581,.T.);
#18794=EDGE_CURVE('',#14878,#14883,#8582,.T.);
#18795=EDGE_CURVE('',#14880,#14884,#8583,.T.);
#18796=EDGE_CURVE('',#14885,#14886,#8584,.T.);
#18797=EDGE_CURVE('',#14885,#14887,#8585,.T.);
#18798=EDGE_CURVE('',#14887,#14888,#8586,.T.);
#18799=EDGE_CURVE('',#14886,#14888,#8587,.T.);
#18800=EDGE_CURVE('',#14889,#14885,#8588,.T.);
#18801=EDGE_CURVE('',#14889,#14890,#8589,.T.);
#18802=EDGE_CURVE('',#14890,#14887,#8590,.T.);
#18803=EDGE_CURVE('',#14891,#14889,#8591,.T.);
#18804=EDGE_CURVE('',#14891,#14892,#8592,.T.);
#18805=EDGE_CURVE('',#14892,#14890,#8593,.T.);
#18806=EDGE_CURVE('',#14886,#14891,#8594,.T.);
#18807=EDGE_CURVE('',#14888,#14892,#8595,.T.);
#18808=EDGE_CURVE('',#14893,#14894,#8596,.T.);
#18809=EDGE_CURVE('',#14893,#14895,#8597,.T.);
#18810=EDGE_CURVE('',#14895,#14896,#8598,.T.);
#18811=EDGE_CURVE('',#14894,#14896,#8599,.T.);
#18812=EDGE_CURVE('',#14897,#14893,#8600,.T.);
#18813=EDGE_CURVE('',#14897,#14898,#8601,.T.);
#18814=EDGE_CURVE('',#14898,#14895,#8602,.T.);
#18815=EDGE_CURVE('',#14899,#14897,#8603,.T.);
#18816=EDGE_CURVE('',#14899,#14900,#8604,.T.);
#18817=EDGE_CURVE('',#14900,#14898,#8605,.T.);
#18818=EDGE_CURVE('',#14894,#14899,#8606,.T.);
#18819=EDGE_CURVE('',#14896,#14900,#8607,.T.);
#18820=EDGE_CURVE('',#14901,#14902,#8608,.T.);
#18821=EDGE_CURVE('',#14901,#14903,#8609,.T.);
#18822=EDGE_CURVE('',#14903,#14904,#8610,.T.);
#18823=EDGE_CURVE('',#14902,#14904,#8611,.T.);
#18824=EDGE_CURVE('',#14905,#14901,#8612,.T.);
#18825=EDGE_CURVE('',#14905,#14906,#8613,.T.);
#18826=EDGE_CURVE('',#14906,#14903,#8614,.T.);
#18827=EDGE_CURVE('',#14907,#14905,#8615,.T.);
#18828=EDGE_CURVE('',#14907,#14908,#8616,.T.);
#18829=EDGE_CURVE('',#14908,#14906,#8617,.T.);
#18830=EDGE_CURVE('',#14902,#14907,#8618,.T.);
#18831=EDGE_CURVE('',#14904,#14908,#8619,.T.);
#18832=EDGE_CURVE('',#14909,#14910,#8620,.T.);
#18833=EDGE_CURVE('',#14909,#14911,#8621,.T.);
#18834=EDGE_CURVE('',#14911,#14912,#8622,.T.);
#18835=EDGE_CURVE('',#14910,#14912,#8623,.T.);
#18836=EDGE_CURVE('',#14913,#14909,#8624,.T.);
#18837=EDGE_CURVE('',#14913,#14914,#8625,.T.);
#18838=EDGE_CURVE('',#14914,#14911,#8626,.T.);
#18839=EDGE_CURVE('',#14915,#14913,#8627,.T.);
#18840=EDGE_CURVE('',#14915,#14916,#8628,.T.);
#18841=EDGE_CURVE('',#14916,#14914,#8629,.T.);
#18842=EDGE_CURVE('',#14910,#14915,#8630,.T.);
#18843=EDGE_CURVE('',#14912,#14916,#8631,.T.);
#18844=EDGE_CURVE('',#14917,#14918,#8632,.T.);
#18845=EDGE_CURVE('',#14917,#14919,#8633,.T.);
#18846=EDGE_CURVE('',#14919,#14920,#8634,.T.);
#18847=EDGE_CURVE('',#14918,#14920,#8635,.T.);
#18848=EDGE_CURVE('',#14921,#14917,#8636,.T.);
#18849=EDGE_CURVE('',#14921,#14922,#8637,.T.);
#18850=EDGE_CURVE('',#14922,#14919,#8638,.T.);
#18851=EDGE_CURVE('',#14923,#14921,#8639,.T.);
#18852=EDGE_CURVE('',#14923,#14924,#8640,.T.);
#18853=EDGE_CURVE('',#14924,#14922,#8641,.T.);
#18854=EDGE_CURVE('',#14918,#14923,#8642,.T.);
#18855=EDGE_CURVE('',#14920,#14924,#8643,.T.);
#18856=EDGE_CURVE('',#14925,#14926,#8644,.T.);
#18857=EDGE_CURVE('',#14925,#14927,#8645,.T.);
#18858=EDGE_CURVE('',#14927,#14928,#8646,.T.);
#18859=EDGE_CURVE('',#14926,#14928,#8647,.T.);
#18860=EDGE_CURVE('',#14929,#14925,#8648,.T.);
#18861=EDGE_CURVE('',#14929,#14930,#8649,.T.);
#18862=EDGE_CURVE('',#14930,#14927,#8650,.T.);
#18863=EDGE_CURVE('',#14931,#14929,#8651,.T.);
#18864=EDGE_CURVE('',#14931,#14932,#8652,.T.);
#18865=EDGE_CURVE('',#14932,#14930,#8653,.T.);
#18866=EDGE_CURVE('',#14926,#14931,#8654,.T.);
#18867=EDGE_CURVE('',#14928,#14932,#8655,.T.);
#18868=EDGE_CURVE('',#14933,#14934,#8656,.T.);
#18869=EDGE_CURVE('',#14933,#14935,#8657,.T.);
#18870=EDGE_CURVE('',#14935,#14936,#8658,.T.);
#18871=EDGE_CURVE('',#14934,#14936,#8659,.T.);
#18872=EDGE_CURVE('',#14937,#14933,#8660,.T.);
#18873=EDGE_CURVE('',#14937,#14938,#8661,.T.);
#18874=EDGE_CURVE('',#14938,#14935,#8662,.T.);
#18875=EDGE_CURVE('',#14939,#14937,#8663,.T.);
#18876=EDGE_CURVE('',#14939,#14940,#8664,.T.);
#18877=EDGE_CURVE('',#14940,#14938,#8665,.T.);
#18878=EDGE_CURVE('',#14934,#14939,#8666,.T.);
#18879=EDGE_CURVE('',#14936,#14940,#8667,.T.);
#18880=EDGE_CURVE('',#14941,#14942,#8668,.T.);
#18881=EDGE_CURVE('',#14941,#14943,#8669,.T.);
#18882=EDGE_CURVE('',#14943,#14944,#8670,.T.);
#18883=EDGE_CURVE('',#14942,#14944,#8671,.T.);
#18884=EDGE_CURVE('',#14945,#14941,#8672,.T.);
#18885=EDGE_CURVE('',#14945,#14946,#8673,.T.);
#18886=EDGE_CURVE('',#14946,#14943,#8674,.T.);
#18887=EDGE_CURVE('',#14947,#14945,#8675,.T.);
#18888=EDGE_CURVE('',#14947,#14948,#8676,.T.);
#18889=EDGE_CURVE('',#14948,#14946,#8677,.T.);
#18890=EDGE_CURVE('',#14942,#14947,#8678,.T.);
#18891=EDGE_CURVE('',#14944,#14948,#8679,.T.);
#18892=EDGE_CURVE('',#14949,#14950,#8680,.T.);
#18893=EDGE_CURVE('',#14949,#14951,#8681,.T.);
#18894=EDGE_CURVE('',#14951,#14952,#8682,.T.);
#18895=EDGE_CURVE('',#14950,#14952,#8683,.T.);
#18896=EDGE_CURVE('',#14953,#14949,#8684,.T.);
#18897=EDGE_CURVE('',#14953,#14954,#8685,.T.);
#18898=EDGE_CURVE('',#14954,#14951,#8686,.T.);
#18899=EDGE_CURVE('',#14955,#14953,#8687,.T.);
#18900=EDGE_CURVE('',#14955,#14956,#8688,.T.);
#18901=EDGE_CURVE('',#14956,#14954,#8689,.T.);
#18902=EDGE_CURVE('',#14950,#14955,#8690,.T.);
#18903=EDGE_CURVE('',#14952,#14956,#8691,.T.);
#18904=EDGE_CURVE('',#14957,#14958,#8692,.T.);
#18905=EDGE_CURVE('',#14957,#14959,#8693,.T.);
#18906=EDGE_CURVE('',#14959,#14960,#8694,.T.);
#18907=EDGE_CURVE('',#14958,#14960,#8695,.T.);
#18908=EDGE_CURVE('',#14961,#14957,#8696,.T.);
#18909=EDGE_CURVE('',#14961,#14962,#8697,.T.);
#18910=EDGE_CURVE('',#14962,#14959,#8698,.T.);
#18911=EDGE_CURVE('',#14963,#14961,#8699,.T.);
#18912=EDGE_CURVE('',#14963,#14964,#8700,.T.);
#18913=EDGE_CURVE('',#14964,#14962,#8701,.T.);
#18914=EDGE_CURVE('',#14958,#14963,#8702,.T.);
#18915=EDGE_CURVE('',#14960,#14964,#8703,.T.);
#18916=EDGE_CURVE('',#14965,#14966,#8704,.T.);
#18917=EDGE_CURVE('',#14965,#14967,#8705,.T.);
#18918=EDGE_CURVE('',#14967,#14968,#8706,.T.);
#18919=EDGE_CURVE('',#14966,#14968,#8707,.T.);
#18920=EDGE_CURVE('',#14969,#14965,#8708,.T.);
#18921=EDGE_CURVE('',#14969,#14970,#8709,.T.);
#18922=EDGE_CURVE('',#14970,#14967,#8710,.T.);
#18923=EDGE_CURVE('',#14971,#14969,#8711,.T.);
#18924=EDGE_CURVE('',#14971,#14972,#8712,.T.);
#18925=EDGE_CURVE('',#14972,#14970,#8713,.T.);
#18926=EDGE_CURVE('',#14966,#14971,#8714,.T.);
#18927=EDGE_CURVE('',#14968,#14972,#8715,.T.);
#18928=EDGE_CURVE('',#14973,#14974,#8716,.T.);
#18929=EDGE_CURVE('',#14973,#14975,#8717,.T.);
#18930=EDGE_CURVE('',#14975,#14976,#8718,.T.);
#18931=EDGE_CURVE('',#14974,#14976,#8719,.T.);
#18932=EDGE_CURVE('',#14977,#14973,#8720,.T.);
#18933=EDGE_CURVE('',#14977,#14978,#8721,.T.);
#18934=EDGE_CURVE('',#14978,#14975,#8722,.T.);
#18935=EDGE_CURVE('',#14979,#14977,#8723,.T.);
#18936=EDGE_CURVE('',#14979,#14980,#8724,.T.);
#18937=EDGE_CURVE('',#14980,#14978,#8725,.T.);
#18938=EDGE_CURVE('',#14974,#14979,#8726,.T.);
#18939=EDGE_CURVE('',#14976,#14980,#8727,.T.);
#18940=EDGE_CURVE('',#14981,#14982,#8728,.T.);
#18941=EDGE_CURVE('',#14981,#14983,#8729,.T.);
#18942=EDGE_CURVE('',#14983,#14984,#8730,.T.);
#18943=EDGE_CURVE('',#14982,#14984,#8731,.T.);
#18944=EDGE_CURVE('',#14985,#14981,#8732,.T.);
#18945=EDGE_CURVE('',#14985,#14986,#8733,.T.);
#18946=EDGE_CURVE('',#14986,#14983,#8734,.T.);
#18947=EDGE_CURVE('',#14987,#14985,#8735,.T.);
#18948=EDGE_CURVE('',#14987,#14988,#8736,.T.);
#18949=EDGE_CURVE('',#14988,#14986,#8737,.T.);
#18950=EDGE_CURVE('',#14982,#14987,#8738,.T.);
#18951=EDGE_CURVE('',#14984,#14988,#8739,.T.);
#18952=EDGE_CURVE('',#14989,#14990,#8740,.T.);
#18953=EDGE_CURVE('',#14989,#14991,#8741,.T.);
#18954=EDGE_CURVE('',#14991,#14992,#8742,.T.);
#18955=EDGE_CURVE('',#14990,#14992,#8743,.T.);
#18956=EDGE_CURVE('',#14993,#14989,#8744,.T.);
#18957=EDGE_CURVE('',#14993,#14994,#8745,.T.);
#18958=EDGE_CURVE('',#14994,#14991,#8746,.T.);
#18959=EDGE_CURVE('',#14995,#14993,#8747,.T.);
#18960=EDGE_CURVE('',#14995,#14996,#8748,.T.);
#18961=EDGE_CURVE('',#14996,#14994,#8749,.T.);
#18962=EDGE_CURVE('',#14990,#14995,#8750,.T.);
#18963=EDGE_CURVE('',#14992,#14996,#8751,.T.);
#18964=EDGE_CURVE('',#14997,#14998,#8752,.T.);
#18965=EDGE_CURVE('',#14997,#14999,#8753,.T.);
#18966=EDGE_CURVE('',#14999,#15000,#8754,.T.);
#18967=EDGE_CURVE('',#14998,#15000,#8755,.T.);
#18968=EDGE_CURVE('',#15001,#14997,#8756,.T.);
#18969=EDGE_CURVE('',#15001,#15002,#8757,.T.);
#18970=EDGE_CURVE('',#15002,#14999,#8758,.T.);
#18971=EDGE_CURVE('',#15003,#15001,#8759,.T.);
#18972=EDGE_CURVE('',#15003,#15004,#8760,.T.);
#18973=EDGE_CURVE('',#15004,#15002,#8761,.T.);
#18974=EDGE_CURVE('',#14998,#15003,#8762,.T.);
#18975=EDGE_CURVE('',#15000,#15004,#8763,.T.);
#18976=EDGE_CURVE('',#15005,#15006,#8764,.T.);
#18977=EDGE_CURVE('',#15005,#15007,#8765,.T.);
#18978=EDGE_CURVE('',#15007,#15008,#8766,.T.);
#18979=EDGE_CURVE('',#15006,#15008,#8767,.T.);
#18980=EDGE_CURVE('',#15009,#15005,#8768,.T.);
#18981=EDGE_CURVE('',#15009,#15010,#8769,.T.);
#18982=EDGE_CURVE('',#15010,#15007,#8770,.T.);
#18983=EDGE_CURVE('',#15011,#15009,#8771,.T.);
#18984=EDGE_CURVE('',#15011,#15012,#8772,.T.);
#18985=EDGE_CURVE('',#15012,#15010,#8773,.T.);
#18986=EDGE_CURVE('',#15006,#15011,#8774,.T.);
#18987=EDGE_CURVE('',#15008,#15012,#8775,.T.);
#18988=EDGE_CURVE('',#15013,#15014,#8776,.T.);
#18989=EDGE_CURVE('',#15013,#15015,#8777,.T.);
#18990=EDGE_CURVE('',#15015,#15016,#8778,.T.);
#18991=EDGE_CURVE('',#15014,#15016,#8779,.T.);
#18992=EDGE_CURVE('',#15017,#15013,#8780,.T.);
#18993=EDGE_CURVE('',#15017,#15018,#8781,.T.);
#18994=EDGE_CURVE('',#15018,#15015,#8782,.T.);
#18995=EDGE_CURVE('',#15019,#15017,#8783,.T.);
#18996=EDGE_CURVE('',#15019,#15020,#8784,.T.);
#18997=EDGE_CURVE('',#15020,#15018,#8785,.T.);
#18998=EDGE_CURVE('',#15014,#15019,#8786,.T.);
#18999=EDGE_CURVE('',#15016,#15020,#8787,.T.);
#19000=EDGE_CURVE('',#15021,#15022,#8788,.T.);
#19001=EDGE_CURVE('',#15021,#15023,#8789,.T.);
#19002=EDGE_CURVE('',#15023,#15024,#8790,.T.);
#19003=EDGE_CURVE('',#15022,#15024,#8791,.T.);
#19004=EDGE_CURVE('',#15025,#15021,#8792,.T.);
#19005=EDGE_CURVE('',#15025,#15026,#8793,.T.);
#19006=EDGE_CURVE('',#15026,#15023,#8794,.T.);
#19007=EDGE_CURVE('',#15027,#15025,#8795,.T.);
#19008=EDGE_CURVE('',#15027,#15028,#8796,.T.);
#19009=EDGE_CURVE('',#15028,#15026,#8797,.T.);
#19010=EDGE_CURVE('',#15022,#15027,#8798,.T.);
#19011=EDGE_CURVE('',#15024,#15028,#8799,.T.);
#19012=EDGE_CURVE('',#15029,#15030,#8800,.T.);
#19013=EDGE_CURVE('',#15029,#15031,#8801,.T.);
#19014=EDGE_CURVE('',#15031,#15032,#8802,.T.);
#19015=EDGE_CURVE('',#15030,#15032,#8803,.T.);
#19016=EDGE_CURVE('',#15033,#15029,#8804,.T.);
#19017=EDGE_CURVE('',#15033,#15034,#8805,.T.);
#19018=EDGE_CURVE('',#15034,#15031,#8806,.T.);
#19019=EDGE_CURVE('',#15035,#15033,#8807,.T.);
#19020=EDGE_CURVE('',#15035,#15036,#8808,.T.);
#19021=EDGE_CURVE('',#15036,#15034,#8809,.T.);
#19022=EDGE_CURVE('',#15030,#15035,#8810,.T.);
#19023=EDGE_CURVE('',#15032,#15036,#8811,.T.);
#19024=EDGE_CURVE('',#15037,#15038,#8812,.T.);
#19025=EDGE_CURVE('',#15037,#15039,#8813,.T.);
#19026=EDGE_CURVE('',#15039,#15040,#8814,.T.);
#19027=EDGE_CURVE('',#15038,#15040,#8815,.T.);
#19028=EDGE_CURVE('',#15041,#15037,#8816,.T.);
#19029=EDGE_CURVE('',#15041,#15042,#8817,.T.);
#19030=EDGE_CURVE('',#15042,#15039,#8818,.T.);
#19031=EDGE_CURVE('',#15043,#15041,#8819,.T.);
#19032=EDGE_CURVE('',#15043,#15044,#8820,.T.);
#19033=EDGE_CURVE('',#15044,#15042,#8821,.T.);
#19034=EDGE_CURVE('',#15038,#15043,#8822,.T.);
#19035=EDGE_CURVE('',#15040,#15044,#8823,.T.);
#19036=EDGE_CURVE('',#15045,#15046,#8824,.T.);
#19037=EDGE_CURVE('',#15045,#15047,#8825,.T.);
#19038=EDGE_CURVE('',#15047,#15048,#8826,.T.);
#19039=EDGE_CURVE('',#15046,#15048,#8827,.T.);
#19040=EDGE_CURVE('',#15049,#15045,#8828,.T.);
#19041=EDGE_CURVE('',#15049,#15050,#8829,.T.);
#19042=EDGE_CURVE('',#15050,#15047,#8830,.T.);
#19043=EDGE_CURVE('',#15051,#15049,#8831,.T.);
#19044=EDGE_CURVE('',#15051,#15052,#8832,.T.);
#19045=EDGE_CURVE('',#15052,#15050,#8833,.T.);
#19046=EDGE_CURVE('',#15046,#15051,#8834,.T.);
#19047=EDGE_CURVE('',#15048,#15052,#8835,.T.);
#19048=EDGE_CURVE('',#15053,#15054,#8836,.T.);
#19049=EDGE_CURVE('',#15053,#15055,#8837,.T.);
#19050=EDGE_CURVE('',#15055,#15056,#8838,.T.);
#19051=EDGE_CURVE('',#15054,#15056,#8839,.T.);
#19052=EDGE_CURVE('',#15057,#15053,#8840,.T.);
#19053=EDGE_CURVE('',#15057,#15058,#8841,.T.);
#19054=EDGE_CURVE('',#15058,#15055,#8842,.T.);
#19055=EDGE_CURVE('',#15059,#15057,#8843,.T.);
#19056=EDGE_CURVE('',#15059,#15060,#8844,.T.);
#19057=EDGE_CURVE('',#15060,#15058,#8845,.T.);
#19058=EDGE_CURVE('',#15054,#15059,#8846,.T.);
#19059=EDGE_CURVE('',#15056,#15060,#8847,.T.);
#19060=EDGE_CURVE('',#15061,#15062,#8848,.T.);
#19061=EDGE_CURVE('',#15061,#15063,#8849,.T.);
#19062=EDGE_CURVE('',#15063,#15064,#8850,.T.);
#19063=EDGE_CURVE('',#15062,#15064,#8851,.T.);
#19064=EDGE_CURVE('',#15065,#15061,#8852,.T.);
#19065=EDGE_CURVE('',#15065,#15066,#8853,.T.);
#19066=EDGE_CURVE('',#15066,#15063,#8854,.T.);
#19067=EDGE_CURVE('',#15067,#15065,#8855,.T.);
#19068=EDGE_CURVE('',#15067,#15068,#8856,.T.);
#19069=EDGE_CURVE('',#15068,#15066,#8857,.T.);
#19070=EDGE_CURVE('',#15062,#15067,#8858,.T.);
#19071=EDGE_CURVE('',#15064,#15068,#8859,.T.);
#19072=EDGE_CURVE('',#15069,#15070,#8860,.T.);
#19073=EDGE_CURVE('',#15069,#15071,#8861,.T.);
#19074=EDGE_CURVE('',#15071,#15072,#8862,.T.);
#19075=EDGE_CURVE('',#15070,#15072,#8863,.T.);
#19076=EDGE_CURVE('',#15073,#15069,#8864,.T.);
#19077=EDGE_CURVE('',#15073,#15074,#8865,.T.);
#19078=EDGE_CURVE('',#15074,#15071,#8866,.T.);
#19079=EDGE_CURVE('',#15075,#15073,#8867,.T.);
#19080=EDGE_CURVE('',#15075,#15076,#8868,.T.);
#19081=EDGE_CURVE('',#15076,#15074,#8869,.T.);
#19082=EDGE_CURVE('',#15070,#15075,#8870,.T.);
#19083=EDGE_CURVE('',#15072,#15076,#8871,.T.);
#19084=EDGE_CURVE('',#15077,#15078,#8872,.T.);
#19085=EDGE_CURVE('',#15077,#15079,#8873,.T.);
#19086=EDGE_CURVE('',#15079,#15080,#8874,.T.);
#19087=EDGE_CURVE('',#15078,#15080,#8875,.T.);
#19088=EDGE_CURVE('',#15081,#15077,#8876,.T.);
#19089=EDGE_CURVE('',#15081,#15082,#8877,.T.);
#19090=EDGE_CURVE('',#15082,#15079,#8878,.T.);
#19091=EDGE_CURVE('',#15083,#15081,#8879,.T.);
#19092=EDGE_CURVE('',#15083,#15084,#8880,.T.);
#19093=EDGE_CURVE('',#15084,#15082,#8881,.T.);
#19094=EDGE_CURVE('',#15078,#15083,#8882,.T.);
#19095=EDGE_CURVE('',#15080,#15084,#8883,.T.);
#19096=EDGE_CURVE('',#15085,#15086,#8884,.T.);
#19097=EDGE_CURVE('',#15085,#15087,#8885,.T.);
#19098=EDGE_CURVE('',#15087,#15088,#8886,.T.);
#19099=EDGE_CURVE('',#15086,#15088,#8887,.T.);
#19100=EDGE_CURVE('',#15089,#15085,#8888,.T.);
#19101=EDGE_CURVE('',#15089,#15090,#8889,.T.);
#19102=EDGE_CURVE('',#15090,#15087,#8890,.T.);
#19103=EDGE_CURVE('',#15091,#15089,#8891,.T.);
#19104=EDGE_CURVE('',#15091,#15092,#8892,.T.);
#19105=EDGE_CURVE('',#15092,#15090,#8893,.T.);
#19106=EDGE_CURVE('',#15086,#15091,#8894,.T.);
#19107=EDGE_CURVE('',#15088,#15092,#8895,.T.);
#19108=EDGE_CURVE('',#15093,#15094,#8896,.T.);
#19109=EDGE_CURVE('',#15093,#15095,#8897,.T.);
#19110=EDGE_CURVE('',#15095,#15096,#8898,.T.);
#19111=EDGE_CURVE('',#15094,#15096,#8899,.T.);
#19112=EDGE_CURVE('',#15097,#15093,#8900,.T.);
#19113=EDGE_CURVE('',#15097,#15098,#8901,.T.);
#19114=EDGE_CURVE('',#15098,#15095,#8902,.T.);
#19115=EDGE_CURVE('',#15099,#15097,#8903,.T.);
#19116=EDGE_CURVE('',#15099,#15100,#8904,.T.);
#19117=EDGE_CURVE('',#15100,#15098,#8905,.T.);
#19118=EDGE_CURVE('',#15094,#15099,#8906,.T.);
#19119=EDGE_CURVE('',#15096,#15100,#8907,.T.);
#19120=EDGE_CURVE('',#15101,#15102,#8908,.T.);
#19121=EDGE_CURVE('',#15101,#15103,#8909,.T.);
#19122=EDGE_CURVE('',#15103,#15104,#8910,.T.);
#19123=EDGE_CURVE('',#15102,#15104,#8911,.T.);
#19124=EDGE_CURVE('',#15105,#15101,#8912,.T.);
#19125=EDGE_CURVE('',#15105,#15106,#8913,.T.);
#19126=EDGE_CURVE('',#15106,#15103,#8914,.T.);
#19127=EDGE_CURVE('',#15107,#15105,#8915,.T.);
#19128=EDGE_CURVE('',#15107,#15108,#8916,.T.);
#19129=EDGE_CURVE('',#15108,#15106,#8917,.T.);
#19130=EDGE_CURVE('',#15102,#15107,#8918,.T.);
#19131=EDGE_CURVE('',#15104,#15108,#8919,.T.);
#19132=EDGE_CURVE('',#15109,#15110,#8920,.T.);
#19133=EDGE_CURVE('',#15109,#15111,#8921,.T.);
#19134=EDGE_CURVE('',#15111,#15112,#8922,.T.);
#19135=EDGE_CURVE('',#15110,#15112,#8923,.T.);
#19136=EDGE_CURVE('',#15113,#15109,#8924,.T.);
#19137=EDGE_CURVE('',#15113,#15114,#8925,.T.);
#19138=EDGE_CURVE('',#15114,#15111,#8926,.T.);
#19139=EDGE_CURVE('',#15115,#15113,#8927,.T.);
#19140=EDGE_CURVE('',#15115,#15116,#8928,.T.);
#19141=EDGE_CURVE('',#15116,#15114,#8929,.T.);
#19142=EDGE_CURVE('',#15110,#15115,#8930,.T.);
#19143=EDGE_CURVE('',#15112,#15116,#8931,.T.);
#19144=EDGE_CURVE('',#15117,#15118,#8932,.T.);
#19145=EDGE_CURVE('',#15117,#15119,#8933,.T.);
#19146=EDGE_CURVE('',#15119,#15120,#8934,.T.);
#19147=EDGE_CURVE('',#15118,#15120,#8935,.T.);
#19148=EDGE_CURVE('',#15121,#15117,#8936,.T.);
#19149=EDGE_CURVE('',#15121,#15122,#8937,.T.);
#19150=EDGE_CURVE('',#15122,#15119,#8938,.T.);
#19151=EDGE_CURVE('',#15123,#15121,#8939,.T.);
#19152=EDGE_CURVE('',#15123,#15124,#8940,.T.);
#19153=EDGE_CURVE('',#15124,#15122,#8941,.T.);
#19154=EDGE_CURVE('',#15118,#15123,#8942,.T.);
#19155=EDGE_CURVE('',#15120,#15124,#8943,.T.);
#19156=EDGE_CURVE('',#15125,#15126,#8944,.T.);
#19157=EDGE_CURVE('',#15125,#15127,#8945,.T.);
#19158=EDGE_CURVE('',#15127,#15128,#8946,.T.);
#19159=EDGE_CURVE('',#15126,#15128,#8947,.T.);
#19160=EDGE_CURVE('',#15129,#15125,#8948,.T.);
#19161=EDGE_CURVE('',#15129,#15130,#8949,.T.);
#19162=EDGE_CURVE('',#15130,#15127,#8950,.T.);
#19163=EDGE_CURVE('',#15131,#15129,#8951,.T.);
#19164=EDGE_CURVE('',#15131,#15132,#8952,.T.);
#19165=EDGE_CURVE('',#15132,#15130,#8953,.T.);
#19166=EDGE_CURVE('',#15126,#15131,#8954,.T.);
#19167=EDGE_CURVE('',#15128,#15132,#8955,.T.);
#19168=EDGE_CURVE('',#15133,#15134,#8956,.T.);
#19169=EDGE_CURVE('',#15133,#15135,#8957,.T.);
#19170=EDGE_CURVE('',#15135,#15136,#8958,.T.);
#19171=EDGE_CURVE('',#15134,#15136,#8959,.T.);
#19172=EDGE_CURVE('',#15137,#15133,#8960,.T.);
#19173=EDGE_CURVE('',#15137,#15138,#8961,.T.);
#19174=EDGE_CURVE('',#15138,#15135,#8962,.T.);
#19175=EDGE_CURVE('',#15139,#15137,#8963,.T.);
#19176=EDGE_CURVE('',#15139,#15140,#8964,.T.);
#19177=EDGE_CURVE('',#15140,#15138,#8965,.T.);
#19178=EDGE_CURVE('',#15134,#15139,#8966,.T.);
#19179=EDGE_CURVE('',#15136,#15140,#8967,.T.);
#19180=EDGE_CURVE('',#15141,#15142,#8968,.T.);
#19181=EDGE_CURVE('',#15141,#15143,#8969,.T.);
#19182=EDGE_CURVE('',#15143,#15144,#8970,.T.);
#19183=EDGE_CURVE('',#15142,#15144,#8971,.T.);
#19184=EDGE_CURVE('',#15145,#15141,#8972,.T.);
#19185=EDGE_CURVE('',#15145,#15146,#8973,.T.);
#19186=EDGE_CURVE('',#15146,#15143,#8974,.T.);
#19187=EDGE_CURVE('',#15147,#15145,#8975,.T.);
#19188=EDGE_CURVE('',#15147,#15148,#8976,.T.);
#19189=EDGE_CURVE('',#15148,#15146,#8977,.T.);
#19190=EDGE_CURVE('',#15142,#15147,#8978,.T.);
#19191=EDGE_CURVE('',#15144,#15148,#8979,.T.);
#19192=EDGE_CURVE('',#15149,#15150,#8980,.T.);
#19193=EDGE_CURVE('',#15149,#15151,#8981,.T.);
#19194=EDGE_CURVE('',#15151,#15152,#8982,.T.);
#19195=EDGE_CURVE('',#15150,#15152,#8983,.T.);
#19196=EDGE_CURVE('',#15153,#15149,#8984,.T.);
#19197=EDGE_CURVE('',#15153,#15154,#8985,.T.);
#19198=EDGE_CURVE('',#15154,#15151,#8986,.T.);
#19199=EDGE_CURVE('',#15155,#15153,#8987,.T.);
#19200=EDGE_CURVE('',#15155,#15156,#8988,.T.);
#19201=EDGE_CURVE('',#15156,#15154,#8989,.T.);
#19202=EDGE_CURVE('',#15150,#15155,#8990,.T.);
#19203=EDGE_CURVE('',#15152,#15156,#8991,.T.);
#19204=EDGE_CURVE('',#15157,#15158,#8992,.T.);
#19205=EDGE_CURVE('',#15157,#15159,#8993,.T.);
#19206=EDGE_CURVE('',#15159,#15160,#8994,.T.);
#19207=EDGE_CURVE('',#15158,#15160,#8995,.T.);
#19208=EDGE_CURVE('',#15161,#15157,#8996,.T.);
#19209=EDGE_CURVE('',#15161,#15162,#8997,.T.);
#19210=EDGE_CURVE('',#15162,#15159,#8998,.T.);
#19211=EDGE_CURVE('',#15163,#15161,#8999,.T.);
#19212=EDGE_CURVE('',#15163,#15164,#9000,.T.);
#19213=EDGE_CURVE('',#15164,#15162,#9001,.T.);
#19214=EDGE_CURVE('',#15158,#15163,#9002,.T.);
#19215=EDGE_CURVE('',#15160,#15164,#9003,.T.);
#19216=EDGE_CURVE('',#15165,#15166,#9004,.T.);
#19217=EDGE_CURVE('',#15165,#15167,#9005,.T.);
#19218=EDGE_CURVE('',#15167,#15168,#9006,.T.);
#19219=EDGE_CURVE('',#15166,#15168,#9007,.T.);
#19220=EDGE_CURVE('',#15169,#15165,#9008,.T.);
#19221=EDGE_CURVE('',#15169,#15170,#9009,.T.);
#19222=EDGE_CURVE('',#15170,#15167,#9010,.T.);
#19223=EDGE_CURVE('',#15171,#15169,#9011,.T.);
#19224=EDGE_CURVE('',#15171,#15172,#9012,.T.);
#19225=EDGE_CURVE('',#15172,#15170,#9013,.T.);
#19226=EDGE_CURVE('',#15166,#15171,#9014,.T.);
#19227=EDGE_CURVE('',#15168,#15172,#9015,.T.);
#19228=EDGE_CURVE('',#15173,#15174,#9016,.T.);
#19229=EDGE_CURVE('',#15173,#15175,#9017,.T.);
#19230=EDGE_CURVE('',#15175,#15176,#9018,.T.);
#19231=EDGE_CURVE('',#15174,#15176,#9019,.T.);
#19232=EDGE_CURVE('',#15177,#15173,#9020,.T.);
#19233=EDGE_CURVE('',#15177,#15178,#9021,.T.);
#19234=EDGE_CURVE('',#15178,#15175,#9022,.T.);
#19235=EDGE_CURVE('',#15179,#15177,#9023,.T.);
#19236=EDGE_CURVE('',#15179,#15180,#9024,.T.);
#19237=EDGE_CURVE('',#15180,#15178,#9025,.T.);
#19238=EDGE_CURVE('',#15174,#15179,#9026,.T.);
#19239=EDGE_CURVE('',#15176,#15180,#9027,.T.);
#19240=EDGE_CURVE('',#15181,#15182,#9028,.T.);
#19241=EDGE_CURVE('',#15181,#15183,#9029,.T.);
#19242=EDGE_CURVE('',#15183,#15184,#9030,.T.);
#19243=EDGE_CURVE('',#15182,#15184,#9031,.T.);
#19244=EDGE_CURVE('',#15185,#15181,#9032,.T.);
#19245=EDGE_CURVE('',#15185,#15186,#9033,.T.);
#19246=EDGE_CURVE('',#15186,#15183,#9034,.T.);
#19247=EDGE_CURVE('',#15187,#15185,#9035,.T.);
#19248=EDGE_CURVE('',#15187,#15188,#9036,.T.);
#19249=EDGE_CURVE('',#15188,#15186,#9037,.T.);
#19250=EDGE_CURVE('',#15182,#15187,#9038,.T.);
#19251=EDGE_CURVE('',#15184,#15188,#9039,.T.);
#19252=EDGE_CURVE('',#15189,#15189,#12916,.T.);
#19253=EDGE_CURVE('',#15189,#15190,#9040,.T.);
#19254=EDGE_CURVE('',#15190,#15190,#12917,.T.);
#19255=EDGE_CURVE('',#15191,#15191,#12918,.T.);
#19256=EDGE_CURVE('',#15191,#15192,#9041,.T.);
#19257=EDGE_CURVE('',#15192,#15192,#12919,.T.);
#19258=EDGE_CURVE('',#15193,#15194,#9042,.T.);
#19259=EDGE_CURVE('',#15194,#15195,#9043,.T.);
#19260=EDGE_CURVE('',#15196,#15195,#9044,.T.);
#19261=EDGE_CURVE('',#15193,#15196,#9045,.T.);
#19262=EDGE_CURVE('',#15197,#15193,#12920,.T.);
#19263=EDGE_CURVE('',#15198,#15196,#12921,.T.);
#19264=EDGE_CURVE('',#15197,#15198,#9046,.T.);
#19265=EDGE_CURVE('',#15199,#15197,#9047,.T.);
#19266=EDGE_CURVE('',#15200,#15198,#9048,.T.);
#19267=EDGE_CURVE('',#15199,#15200,#9049,.T.);
#19268=EDGE_CURVE('',#15201,#15199,#12922,.T.);
#19269=EDGE_CURVE('',#15202,#15200,#12923,.T.);
#19270=EDGE_CURVE('',#15201,#15202,#9050,.T.);
#19271=EDGE_CURVE('',#15203,#15201,#9051,.T.);
#19272=EDGE_CURVE('',#15204,#15202,#9052,.T.);
#19273=EDGE_CURVE('',#15203,#15204,#9053,.T.);
#19274=EDGE_CURVE('',#15205,#15203,#12924,.T.);
#19275=EDGE_CURVE('',#15206,#15204,#12925,.T.);
#19276=EDGE_CURVE('',#15205,#15206,#9054,.T.);
#19277=EDGE_CURVE('',#15207,#15205,#9055,.T.);
#19278=EDGE_CURVE('',#15208,#15206,#9056,.T.);
#19279=EDGE_CURVE('',#15207,#15208,#9057,.T.);
#19280=EDGE_CURVE('',#15194,#15207,#12926,.T.);
#19281=EDGE_CURVE('',#15195,#15208,#12927,.T.);
#19282=EDGE_CURVE('',#15209,#15210,#9058,.T.);
#19283=EDGE_CURVE('',#15209,#15211,#9059,.T.);
#19284=EDGE_CURVE('',#15211,#15212,#9060,.T.);
#19285=EDGE_CURVE('',#15210,#15212,#9061,.T.);
#19286=EDGE_CURVE('',#15213,#15209,#9062,.T.);
#19287=EDGE_CURVE('',#15213,#15214,#9063,.T.);
#19288=EDGE_CURVE('',#15214,#15211,#9064,.T.);
#19289=EDGE_CURVE('',#15215,#15213,#9065,.T.);
#19290=EDGE_CURVE('',#15215,#15216,#9066,.T.);
#19291=EDGE_CURVE('',#15216,#15214,#9067,.T.);
#19292=EDGE_CURVE('',#15210,#15215,#9068,.T.);
#19293=EDGE_CURVE('',#15212,#15216,#9069,.T.);
#19294=EDGE_CURVE('',#15217,#15218,#9070,.T.);
#19295=EDGE_CURVE('',#15217,#15219,#9071,.T.);
#19296=EDGE_CURVE('',#15219,#15220,#9072,.T.);
#19297=EDGE_CURVE('',#15218,#15220,#9073,.T.);
#19298=EDGE_CURVE('',#15221,#15217,#9074,.T.);
#19299=EDGE_CURVE('',#15221,#15222,#9075,.T.);
#19300=EDGE_CURVE('',#15222,#15219,#9076,.T.);
#19301=EDGE_CURVE('',#15223,#15221,#9077,.T.);
#19302=EDGE_CURVE('',#15223,#15224,#9078,.T.);
#19303=EDGE_CURVE('',#15224,#15222,#9079,.T.);
#19304=EDGE_CURVE('',#15218,#15223,#9080,.T.);
#19305=EDGE_CURVE('',#15220,#15224,#9081,.T.);
#19306=EDGE_CURVE('',#15225,#15226,#9082,.T.);
#19307=EDGE_CURVE('',#15225,#15227,#9083,.T.);
#19308=EDGE_CURVE('',#15227,#15228,#9084,.T.);
#19309=EDGE_CURVE('',#15226,#15228,#9085,.T.);
#19310=EDGE_CURVE('',#15229,#15225,#9086,.T.);
#19311=EDGE_CURVE('',#15229,#15230,#9087,.T.);
#19312=EDGE_CURVE('',#15230,#15227,#9088,.T.);
#19313=EDGE_CURVE('',#15231,#15229,#9089,.T.);
#19314=EDGE_CURVE('',#15231,#15232,#9090,.T.);
#19315=EDGE_CURVE('',#15232,#15230,#9091,.T.);
#19316=EDGE_CURVE('',#15226,#15231,#9092,.T.);
#19317=EDGE_CURVE('',#15228,#15232,#9093,.T.);
#19318=EDGE_CURVE('',#15233,#15234,#9094,.T.);
#19319=EDGE_CURVE('',#15233,#15235,#9095,.T.);
#19320=EDGE_CURVE('',#15235,#15236,#9096,.T.);
#19321=EDGE_CURVE('',#15234,#15236,#9097,.T.);
#19322=EDGE_CURVE('',#15237,#15233,#9098,.T.);
#19323=EDGE_CURVE('',#15237,#15238,#9099,.T.);
#19324=EDGE_CURVE('',#15238,#15235,#9100,.T.);
#19325=EDGE_CURVE('',#15239,#15237,#9101,.T.);
#19326=EDGE_CURVE('',#15239,#15240,#9102,.T.);
#19327=EDGE_CURVE('',#15240,#15238,#9103,.T.);
#19328=EDGE_CURVE('',#15234,#15239,#9104,.T.);
#19329=EDGE_CURVE('',#15236,#15240,#9105,.T.);
#19330=EDGE_CURVE('',#15241,#15242,#9106,.T.);
#19331=EDGE_CURVE('',#15241,#15243,#9107,.T.);
#19332=EDGE_CURVE('',#15243,#15244,#9108,.T.);
#19333=EDGE_CURVE('',#15242,#15244,#9109,.T.);
#19334=EDGE_CURVE('',#15245,#15241,#9110,.T.);
#19335=EDGE_CURVE('',#15245,#15246,#9111,.T.);
#19336=EDGE_CURVE('',#15246,#15243,#9112,.T.);
#19337=EDGE_CURVE('',#15247,#15245,#9113,.T.);
#19338=EDGE_CURVE('',#15247,#15248,#9114,.T.);
#19339=EDGE_CURVE('',#15248,#15246,#9115,.T.);
#19340=EDGE_CURVE('',#15242,#15247,#9116,.T.);
#19341=EDGE_CURVE('',#15244,#15248,#9117,.T.);
#19342=EDGE_CURVE('',#15249,#15250,#9118,.T.);
#19343=EDGE_CURVE('',#15249,#15251,#9119,.T.);
#19344=EDGE_CURVE('',#15251,#15252,#9120,.T.);
#19345=EDGE_CURVE('',#15250,#15252,#9121,.T.);
#19346=EDGE_CURVE('',#15253,#15249,#9122,.T.);
#19347=EDGE_CURVE('',#15253,#15254,#9123,.T.);
#19348=EDGE_CURVE('',#15254,#15251,#9124,.T.);
#19349=EDGE_CURVE('',#15255,#15253,#9125,.T.);
#19350=EDGE_CURVE('',#15255,#15256,#9126,.T.);
#19351=EDGE_CURVE('',#15256,#15254,#9127,.T.);
#19352=EDGE_CURVE('',#15250,#15255,#9128,.T.);
#19353=EDGE_CURVE('',#15252,#15256,#9129,.T.);
#19354=EDGE_CURVE('',#15257,#15258,#9130,.T.);
#19355=EDGE_CURVE('',#15257,#15259,#9131,.T.);
#19356=EDGE_CURVE('',#15259,#15260,#9132,.T.);
#19357=EDGE_CURVE('',#15258,#15260,#9133,.T.);
#19358=EDGE_CURVE('',#15261,#15257,#9134,.T.);
#19359=EDGE_CURVE('',#15261,#15262,#9135,.T.);
#19360=EDGE_CURVE('',#15262,#15259,#9136,.T.);
#19361=EDGE_CURVE('',#15263,#15261,#9137,.T.);
#19362=EDGE_CURVE('',#15263,#15264,#9138,.T.);
#19363=EDGE_CURVE('',#15264,#15262,#9139,.T.);
#19364=EDGE_CURVE('',#15258,#15263,#9140,.T.);
#19365=EDGE_CURVE('',#15260,#15264,#9141,.T.);
#19366=EDGE_CURVE('',#15265,#15266,#9142,.T.);
#19367=EDGE_CURVE('',#15265,#15267,#9143,.T.);
#19368=EDGE_CURVE('',#15267,#15268,#9144,.T.);
#19369=EDGE_CURVE('',#15266,#15268,#9145,.T.);
#19370=EDGE_CURVE('',#15269,#15265,#9146,.T.);
#19371=EDGE_CURVE('',#15269,#15270,#9147,.T.);
#19372=EDGE_CURVE('',#15270,#15267,#9148,.T.);
#19373=EDGE_CURVE('',#15271,#15269,#9149,.T.);
#19374=EDGE_CURVE('',#15271,#15272,#9150,.T.);
#19375=EDGE_CURVE('',#15272,#15270,#9151,.T.);
#19376=EDGE_CURVE('',#15266,#15271,#9152,.T.);
#19377=EDGE_CURVE('',#15268,#15272,#9153,.T.);
#19378=EDGE_CURVE('',#15273,#15274,#9154,.T.);
#19379=EDGE_CURVE('',#15273,#15275,#9155,.T.);
#19380=EDGE_CURVE('',#15275,#15276,#9156,.T.);
#19381=EDGE_CURVE('',#15274,#15276,#9157,.T.);
#19382=EDGE_CURVE('',#15277,#15273,#9158,.T.);
#19383=EDGE_CURVE('',#15277,#15278,#9159,.T.);
#19384=EDGE_CURVE('',#15278,#15275,#9160,.T.);
#19385=EDGE_CURVE('',#15279,#15277,#9161,.T.);
#19386=EDGE_CURVE('',#15279,#15280,#9162,.T.);
#19387=EDGE_CURVE('',#15280,#15278,#9163,.T.);
#19388=EDGE_CURVE('',#15274,#15279,#9164,.T.);
#19389=EDGE_CURVE('',#15276,#15280,#9165,.T.);
#19390=EDGE_CURVE('',#15281,#15282,#9166,.T.);
#19391=EDGE_CURVE('',#15281,#15283,#9167,.T.);
#19392=EDGE_CURVE('',#15283,#15284,#9168,.T.);
#19393=EDGE_CURVE('',#15282,#15284,#9169,.T.);
#19394=EDGE_CURVE('',#15285,#15281,#9170,.T.);
#19395=EDGE_CURVE('',#15285,#15286,#9171,.T.);
#19396=EDGE_CURVE('',#15286,#15283,#9172,.T.);
#19397=EDGE_CURVE('',#15287,#15285,#9173,.T.);
#19398=EDGE_CURVE('',#15287,#15288,#9174,.T.);
#19399=EDGE_CURVE('',#15288,#15286,#9175,.T.);
#19400=EDGE_CURVE('',#15282,#15287,#9176,.T.);
#19401=EDGE_CURVE('',#15284,#15288,#9177,.T.);
#19402=EDGE_CURVE('',#15289,#15290,#9178,.T.);
#19403=EDGE_CURVE('',#15289,#15291,#9179,.T.);
#19404=EDGE_CURVE('',#15291,#15292,#9180,.T.);
#19405=EDGE_CURVE('',#15290,#15292,#9181,.T.);
#19406=EDGE_CURVE('',#15293,#15289,#9182,.T.);
#19407=EDGE_CURVE('',#15293,#15294,#9183,.T.);
#19408=EDGE_CURVE('',#15294,#15291,#9184,.T.);
#19409=EDGE_CURVE('',#15295,#15293,#9185,.T.);
#19410=EDGE_CURVE('',#15295,#15296,#9186,.T.);
#19411=EDGE_CURVE('',#15296,#15294,#9187,.T.);
#19412=EDGE_CURVE('',#15290,#15295,#9188,.T.);
#19413=EDGE_CURVE('',#15292,#15296,#9189,.T.);
#19414=EDGE_CURVE('',#15297,#15297,#12928,.T.);
#19415=EDGE_CURVE('',#15297,#15298,#9190,.T.);
#19416=EDGE_CURVE('',#15298,#15298,#12929,.T.);
#19417=EDGE_CURVE('',#15299,#15299,#12930,.T.);
#19418=EDGE_CURVE('',#15299,#15300,#9191,.T.);
#19419=EDGE_CURVE('',#15300,#15300,#12931,.T.);
#19420=EDGE_CURVE('',#15301,#15302,#9192,.T.);
#19421=EDGE_CURVE('',#15301,#15303,#9193,.T.);
#19422=EDGE_CURVE('',#15304,#15303,#9194,.T.);
#19423=EDGE_CURVE('',#15302,#15304,#9195,.T.);
#19424=EDGE_CURVE('',#15302,#15305,#9196,.T.);
#19425=EDGE_CURVE('',#15306,#15304,#9197,.T.);
#19426=EDGE_CURVE('',#15305,#15306,#9198,.T.);
#19427=EDGE_CURVE('',#15305,#15307,#9199,.T.);
#19428=EDGE_CURVE('',#15308,#15306,#9200,.T.);
#19429=EDGE_CURVE('',#15307,#15308,#9201,.T.);
#19430=EDGE_CURVE('',#15307,#15309,#9202,.T.);
#19431=EDGE_CURVE('',#15310,#15308,#9203,.T.);
#19432=EDGE_CURVE('',#15309,#15310,#9204,.T.);
#19433=EDGE_CURVE('',#15309,#15311,#9205,.T.);
#19434=EDGE_CURVE('',#15312,#15310,#9206,.T.);
#19435=EDGE_CURVE('',#15311,#15312,#9207,.T.);
#19436=EDGE_CURVE('',#15311,#15313,#9208,.T.);
#19437=EDGE_CURVE('',#15314,#15312,#9209,.T.);
#19438=EDGE_CURVE('',#15313,#15314,#9210,.T.);
#19439=EDGE_CURVE('',#15313,#15315,#9211,.T.);
#19440=EDGE_CURVE('',#15316,#15314,#9212,.T.);
#19441=EDGE_CURVE('',#15315,#15316,#9213,.T.);
#19442=EDGE_CURVE('',#15315,#15301,#9214,.T.);
#19443=EDGE_CURVE('',#15303,#15316,#9215,.T.);
#19444=EDGE_CURVE('',#15317,#15318,#100,.T.);
#19445=EDGE_CURVE('',#15318,#15319,#12932,.T.);
#19446=EDGE_CURVE('',#15319,#15320,#101,.T.);
#19447=EDGE_CURVE('',#15320,#15317,#12933,.T.);
#19448=EDGE_CURVE('',#15318,#15321,#9216,.T.);
#19449=EDGE_CURVE('',#15322,#15321,#12934,.T.);
#19450=EDGE_CURVE('',#15322,#15323,#9217,.T.);
#19451=EDGE_CURVE('',#15323,#15324,#9218,.T.);
#19452=EDGE_CURVE('',#15324,#15325,#9219,.T.);
#19453=EDGE_CURVE('',#15325,#15326,#9220,.T.);
#19454=EDGE_CURVE('',#15326,#15319,#9221,.T.);
#19455=EDGE_CURVE('',#15327,#15328,#9222,.T.);
#19456=EDGE_CURVE('',#15328,#15329,#12935,.T.);
#19457=EDGE_CURVE('',#15329,#15330,#9223,.T.);
#19458=EDGE_CURVE('',#15330,#15327,#12936,.T.);
#19459=EDGE_CURVE('',#15331,#15332,#9224,.T.);
#19460=EDGE_CURVE('',#15332,#15333,#12937,.T.);
#19461=EDGE_CURVE('',#15333,#15334,#9225,.T.);
#19462=EDGE_CURVE('',#15334,#15331,#12938,.T.);
#19463=EDGE_CURVE('',#15335,#15322,#102,.T.);
#19464=EDGE_CURVE('',#15321,#15336,#103,.T.);
#19465=EDGE_CURVE('',#15336,#15335,#12939,.T.);
#19466=EDGE_CURVE('',#15326,#15337,#9226,.T.);
#19467=EDGE_CURVE('',#15338,#15337,#9227,.T.);
#19468=EDGE_CURVE('',#15323,#15338,#9228,.T.);
#19469=EDGE_CURVE('',#15335,#15339,#9229,.T.);
#19470=EDGE_CURVE('',#15339,#15340,#9230,.T.);
#19471=EDGE_CURVE('',#15340,#15336,#9231,.T.);
#19472=EDGE_CURVE('',#15317,#15341,#9232,.T.);
#19473=EDGE_CURVE('',#15341,#15342,#9233,.T.);
#19474=EDGE_CURVE('',#15342,#15320,#9234,.T.);
#19475=EDGE_CURVE('',#15340,#15339,#12940,.T.);
#19476=EDGE_CURVE('',#15343,#15343,#12941,.T.);
#19477=EDGE_CURVE('',#15342,#15341,#12942,.T.);
#19478=EDGE_CURVE('',#15344,#15344,#12943,.T.);
#19479=EDGE_CURVE('',#15343,#15345,#9235,.T.);
#19480=EDGE_CURVE('',#15346,#15345,#12944,.T.);
#19481=EDGE_CURVE('',#15347,#15346,#300,.T.);
#19482=EDGE_CURVE('',#15345,#15347,#12945,.T.);
#19483=EDGE_CURVE('',#15344,#15348,#9236,.T.);
#19484=EDGE_CURVE('',#15349,#15348,#12946,.T.);
#19485=EDGE_CURVE('',#15350,#15349,#301,.T.);
#19486=EDGE_CURVE('',#15348,#15350,#12947,.T.);
#19487=EDGE_CURVE('',#15346,#15351,#9237,.T.);
#19488=EDGE_CURVE('',#15351,#15338,#9238,.T.);
#19489=EDGE_CURVE('',#15352,#15337,#9239,.T.);
#19490=EDGE_CURVE('',#15352,#15350,#9240,.T.);
#19491=EDGE_CURVE('',#15349,#15347,#9241,.T.);
#19492=EDGE_CURVE('',#15353,#15354,#9242,.T.);
#19493=EDGE_CURVE('',#15353,#15332,#9243,.T.);
#19494=EDGE_CURVE('',#15354,#15331,#9244,.T.);
#19495=EDGE_CURVE('',#15355,#15356,#302,.T.);
#19496=EDGE_CURVE('',#15357,#15355,#12948,.T.);
#19497=EDGE_CURVE('',#15357,#15333,#9245,.T.);
#19498=EDGE_CURVE('',#15356,#15353,#12949,.T.);
#19499=EDGE_CURVE('',#15358,#15357,#9246,.T.);
#19500=EDGE_CURVE('',#15358,#15334,#9247,.T.);
#19501=EDGE_CURVE('',#15354,#15358,#12950,.T.);
#19502=EDGE_CURVE('',#15359,#15360,#9248,.T.);
#19503=EDGE_CURVE('',#15359,#15328,#9249,.T.);
#19504=EDGE_CURVE('',#15360,#15327,#9250,.T.);
#19505=EDGE_CURVE('',#15361,#15362,#303,.T.);
#19506=EDGE_CURVE('',#15363,#15361,#12951,.T.);
#19507=EDGE_CURVE('',#15363,#15329,#9251,.T.);
#19508=EDGE_CURVE('',#15362,#15359,#12952,.T.);
#19509=EDGE_CURVE('',#15364,#15363,#9252,.T.);
#19510=EDGE_CURVE('',#15364,#15330,#9253,.T.);
#19511=EDGE_CURVE('',#15360,#15364,#12953,.T.);
#19512=EDGE_CURVE('',#15365,#15352,#9254,.T.);
#19513=EDGE_CURVE('',#15362,#15365,#9255,.T.);
#19514=EDGE_CURVE('',#15356,#15361,#9256,.T.);
#19515=EDGE_CURVE('',#15366,#15355,#9257,.T.);
#19516=EDGE_CURVE('',#15351,#15366,#9258,.T.);
#19517=EDGE_CURVE('',#15337,#15367,#9259,.T.);
#19518=EDGE_CURVE('',#15365,#15367,#9260,.T.);
#19519=EDGE_CURVE('',#15366,#15368,#9261,.T.);
#19520=EDGE_CURVE('',#15368,#15338,#9262,.T.);
#19521=EDGE_CURVE('',#15367,#15368,#9263,.T.);
#19522=EDGE_CURVE('',#15325,#15367,#9264,.T.);
#19523=EDGE_CURVE('',#15324,#15368,#9265,.T.);
#19524=EDGE_CURVE('',#15369,#15370,#9266,.T.);
#19525=EDGE_CURVE('',#15369,#15371,#1376,.F.);
#19526=EDGE_CURVE('',#15371,#15372,#12954,.T.);
#19527=EDGE_CURVE('',#15372,#15370,#1377,.T.);
#19528=EDGE_CURVE('',#15373,#15374,#9267,.T.);
#19529=EDGE_CURVE('',#15373,#15369,#1378,.F.);
#19530=EDGE_CURVE('',#15370,#15374,#1379,.T.);
#19531=EDGE_CURVE('',#15375,#15376,#9268,.T.);
#19532=EDGE_CURVE('',#15375,#15373,#1380,.T.);
#19533=EDGE_CURVE('',#15374,#15376,#1381,.T.);
#19534=EDGE_CURVE('',#15377,#15378,#9269,.T.);
#19535=EDGE_CURVE('',#15377,#15379,#1382,.T.);
#19536=EDGE_CURVE('',#15379,#15375,#1383,.T.);
#19537=EDGE_CURVE('',#15376,#15380,#1384,.T.);
#19538=EDGE_CURVE('',#15380,#15378,#1385,.T.);
#19539=EDGE_CURVE('',#15381,#15382,#9270,.T.);
#19540=EDGE_CURVE('',#15381,#15383,#1386,.T.);
#19541=EDGE_CURVE('',#15383,#15377,#1387,.T.);
#19542=EDGE_CURVE('',#15378,#15382,#1388,.T.);
#19543=EDGE_CURVE('',#15384,#15385,#9271,.T.);
#19544=EDGE_CURVE('',#15384,#15381,#1389,.T.);
#19545=EDGE_CURVE('',#15382,#15385,#1390,.T.);
#19546=EDGE_CURVE('',#15386,#15387,#9272,.T.);
#19547=EDGE_CURVE('',#15386,#15384,#1391,.T.);
#19548=EDGE_CURVE('',#15385,#15388,#1392,.T.);
#19549=EDGE_CURVE('',#15388,#15387,#1393,.T.);
#19550=EDGE_CURVE('',#15389,#15390,#9273,.T.);
#19551=EDGE_CURVE('',#15389,#15391,#1394,.T.);
#19552=EDGE_CURVE('',#15391,#15386,#1395,.T.);
#19553=EDGE_CURVE('',#15387,#15392,#1396,.T.);
#19554=EDGE_CURVE('',#15392,#15390,#1397,.T.);
#19555=EDGE_CURVE('',#15393,#15394,#9274,.T.);
#19556=EDGE_CURVE('',#15393,#15389,#1398,.T.);
#19557=EDGE_CURVE('',#15390,#15394,#1399,.T.);
#19558=EDGE_CURVE('',#15395,#15396,#9275,.T.);
#19559=EDGE_CURVE('',#15397,#15395,#1400,.F.);
#19560=EDGE_CURVE('',#15398,#15397,#12955,.T.);
#19561=EDGE_CURVE('',#15398,#15396,#1401,.T.);
#19562=EDGE_CURVE('',#15399,#15400,#9276,.T.);
#19563=EDGE_CURVE('',#15395,#15399,#1402,.F.);
#19564=EDGE_CURVE('',#15396,#15400,#1403,.T.);
#19565=EDGE_CURVE('',#15401,#15402,#9277,.T.);
#19566=EDGE_CURVE('',#15399,#15401,#1404,.F.);
#19567=EDGE_CURVE('',#15400,#15402,#1405,.T.);
#19568=EDGE_CURVE('',#15403,#15404,#9278,.T.);
#19569=EDGE_CURVE('',#15405,#15403,#1406,.F.);
#19570=EDGE_CURVE('',#15401,#15405,#1407,.F.);
#19571=EDGE_CURVE('',#15402,#15404,#1408,.T.);
#19572=EDGE_CURVE('',#15406,#15407,#9279,.T.);
#19573=EDGE_CURVE('',#15403,#15406,#1409,.F.);
#19574=EDGE_CURVE('',#15404,#15407,#1410,.T.);
#19575=EDGE_CURVE('',#15408,#15409,#9280,.T.);
#19576=EDGE_CURVE('',#15406,#15408,#1411,.F.);
#19577=EDGE_CURVE('',#15407,#15409,#1412,.T.);
#19578=EDGE_CURVE('',#15410,#15411,#9281,.T.);
#19579=EDGE_CURVE('',#15408,#15410,#1413,.F.);
#19580=EDGE_CURVE('',#15409,#15412,#1414,.T.);
#19581=EDGE_CURVE('',#15412,#15411,#1415,.T.);
#19582=EDGE_CURVE('',#15413,#15414,#9282,.T.);
#19583=EDGE_CURVE('',#15410,#15413,#1416,.F.);
#19584=EDGE_CURVE('',#15411,#15414,#1417,.T.);
#19585=EDGE_CURVE('',#15414,#15415,#1418,.T.);
#19586=EDGE_CURVE('',#15416,#15415,#12956,.T.);
#19587=EDGE_CURVE('',#15413,#15416,#1419,.F.);
#19588=EDGE_CURVE('',#15394,#15417,#1420,.T.);
#19589=EDGE_CURVE('',#15418,#15417,#12957,.F.);
#19590=EDGE_CURVE('',#15418,#15393,#1421,.T.);
#19591=EDGE_CURVE('',#15419,#15420,#12958,.F.);
#19592=EDGE_CURVE('',#15419,#15416,#1422,.T.);
#19593=EDGE_CURVE('',#15415,#15418,#1423,.T.);
#19594=EDGE_CURVE('',#15420,#15418,#12959,.F.);
#19595=EDGE_CURVE('',#15417,#15419,#1424,.T.);
#19596=EDGE_CURVE('',#15421,#15372,#1425,.T.);
#19597=EDGE_CURVE('',#15421,#15397,#1426,.T.);
#19598=EDGE_CURVE('',#15372,#15422,#12960,.T.);
#19599=EDGE_CURVE('',#15422,#15423,#12961,.T.);
#19600=EDGE_CURVE('',#15423,#15398,#1427,.T.);
#19601=EDGE_CURVE('',#15423,#15371,#1428,.T.);
#19602=EDGE_CURVE('',#15424,#15425,#104,.T.);
#19603=EDGE_CURVE('',#15426,#15424,#12962,.T.);
#19604=EDGE_CURVE('',#15427,#15426,#105,.T.);
#19605=EDGE_CURVE('',#15428,#15427,#106,.T.);
#19606=EDGE_CURVE('',#15429,#15428,#12963,.T.);
#19607=EDGE_CURVE('',#15430,#15429,#107,.T.);
#19608=EDGE_CURVE('',#15431,#15430,#108,.T.);
#19609=EDGE_CURVE('',#15432,#15431,#12964,.T.);
#19610=EDGE_CURVE('',#15433,#15432,#109,.T.);
#19611=EDGE_CURVE('',#15434,#15433,#110,.T.);
#19612=EDGE_CURVE('',#15435,#15434,#12965,.T.);
#19613=EDGE_CURVE('',#15436,#15435,#111,.T.);
#19614=EDGE_CURVE('',#15437,#15436,#112,.T.);
#19615=EDGE_CURVE('',#15438,#15437,#12966,.T.);
#19616=EDGE_CURVE('',#15439,#15438,#113,.T.);
#19617=EDGE_CURVE('',#15440,#15439,#114,.T.);
#19618=EDGE_CURVE('',#15441,#15440,#12967,.T.);
#19619=EDGE_CURVE('',#15425,#15441,#115,.T.);
#19620=EDGE_CURVE('',#15425,#15442,#9283,.T.);
#19621=EDGE_CURVE('',#15442,#15442,#12968,.T.);
#19622=EDGE_CURVE('',#15438,#15443,#9284,.T.);
#19623=EDGE_CURVE('',#15444,#15437,#9285,.T.);
#19624=EDGE_CURVE('',#15443,#15444,#12969,.T.);
#19625=EDGE_CURVE('',#15445,#15434,#9286,.T.);
#19626=EDGE_CURVE('',#15446,#15445,#12970,.T.);
#19627=EDGE_CURVE('',#15435,#15446,#9287,.T.);
#19628=EDGE_CURVE('',#15441,#15447,#9288,.T.);
#19629=EDGE_CURVE('',#15448,#15440,#9289,.T.);
#19630=EDGE_CURVE('',#15447,#15448,#12971,.T.);
#19631=EDGE_CURVE('',#15449,#15431,#9290,.T.);
#19632=EDGE_CURVE('',#15450,#15449,#12972,.T.);
#19633=EDGE_CURVE('',#15432,#15450,#9291,.T.);
#19634=EDGE_CURVE('',#15426,#15451,#9292,.T.);
#19635=EDGE_CURVE('',#15452,#15424,#9293,.T.);
#19636=EDGE_CURVE('',#15451,#15452,#12973,.T.);
#19637=EDGE_CURVE('',#15453,#15428,#9294,.T.);
#19638=EDGE_CURVE('',#15454,#15453,#12974,.T.);
#19639=EDGE_CURVE('',#15429,#15454,#9295,.T.);
#19640=EDGE_CURVE('',#15452,#15451,#9296,.T.);
#19641=EDGE_CURVE('',#15425,#15455,#9297,.T.);
#19642=EDGE_CURVE('',#15455,#15456,#9298,.T.);
#19643=EDGE_CURVE('',#15427,#15456,#9299,.T.);
#19644=EDGE_CURVE('',#15448,#15447,#9300,.T.);
#19645=EDGE_CURVE('',#15439,#15457,#9301,.T.);
#19646=EDGE_CURVE('',#15457,#15455,#9302,.T.);
#19647=EDGE_CURVE('',#15444,#15443,#9303,.T.);
#19648=EDGE_CURVE('',#15436,#15458,#9304,.T.);
#19649=EDGE_CURVE('',#15458,#15457,#9305,.T.);
#19650=EDGE_CURVE('',#15445,#15446,#9306,.T.);
#19651=EDGE_CURVE('',#15449,#15450,#9307,.T.);
#19652=EDGE_CURVE('',#15453,#15454,#9308,.T.);
#19653=EDGE_CURVE('',#15459,#15460,#9309,.T.);
#19654=EDGE_CURVE('',#15460,#15459,#12975,.T.);
#19655=EDGE_CURVE('',#15460,#15458,#9310,.T.);
#19656=EDGE_CURVE('',#15458,#15460,#12976,.T.);
#19657=EDGE_CURVE('',#15457,#15458,#12977,.T.);
#19658=EDGE_CURVE('',#15455,#15457,#12978,.T.);
#19659=EDGE_CURVE('',#15456,#15455,#12979,.T.);
#19660=EDGE_CURVE('',#15456,#15459,#9311,.T.);
#19661=EDGE_CURVE('',#15459,#15456,#12980,.T.);
#19662=EDGE_CURVE('',#15461,#15455,#9312,.T.);
#19663=EDGE_CURVE('',#15430,#15459,#9313,.T.);
#19664=EDGE_CURVE('',#15433,#15460,#9314,.T.);
#19665=EDGE_CURVE('',#15462,#15462,#12981,.T.);
#19666=EDGE_CURVE('',#15422,#15462,#9315,.T.);
#19667=EDGE_CURVE('',#15420,#15463,#9316,.T.);
#19668=EDGE_CURVE('',#15463,#15463,#12982,.T.);
#19669=EDGE_CURVE('',#15464,#15464,#12983,.T.);
#19670=EDGE_CURVE('',#15464,#15465,#9317,.T.);
#19671=EDGE_CURVE('',#15465,#15465,#12984,.T.);
#19672=EDGE_CURVE('',#15464,#15466,#9318,.T.);
#19673=EDGE_CURVE('',#15466,#15467,#12985,.T.);
#19674=EDGE_CURVE('',#15467,#15466,#12986,.T.);
#19675=EDGE_CURVE('',#15468,#15469,#9319,.T.);
#19676=EDGE_CURVE('',#15470,#15468,#9320,.T.);
#19677=EDGE_CURVE('',#15471,#15470,#9321,.T.);
#19678=EDGE_CURVE('',#15469,#15471,#9322,.T.);
#19679=EDGE_CURVE('',#15472,#15467,#9323,.T.);
#19680=EDGE_CURVE('',#15473,#15473,#12987,.T.);
#19681=EDGE_CURVE('',#15473,#15474,#9324,.T.);
#19682=EDGE_CURVE('',#15474,#15474,#12988,.T.);
#19683=EDGE_CURVE('',#15473,#15475,#9325,.T.);
#19684=EDGE_CURVE('',#15475,#15476,#12989,.T.);
#19685=EDGE_CURVE('',#15476,#15475,#12990,.T.);
#19686=EDGE_CURVE('',#15477,#15478,#9326,.T.);
#19687=EDGE_CURVE('',#15479,#15477,#9327,.T.);
#19688=EDGE_CURVE('',#15480,#15479,#9328,.T.);
#19689=EDGE_CURVE('',#15478,#15480,#9329,.T.);
#19690=EDGE_CURVE('',#15481,#15476,#9330,.T.);
#19691=EDGE_CURVE('',#15482,#15482,#12991,.T.);
#19692=EDGE_CURVE('',#15482,#15483,#9331,.T.);
#19693=EDGE_CURVE('',#15483,#15483,#12992,.T.);
#19694=EDGE_CURVE('',#15484,#15477,#9332,.T.);
#19695=EDGE_CURVE('',#15484,#15485,#9333,.T.);
#19696=EDGE_CURVE('',#15470,#15485,#9334,.T.);
#19697=EDGE_CURVE('',#15486,#15468,#9335,.T.);
#19698=EDGE_CURVE('',#15486,#15487,#9336,.T.);
#19699=EDGE_CURVE('',#15479,#15487,#9337,.T.);
#19700=EDGE_CURVE('',#15488,#15488,#12993,.T.);
#19701=EDGE_CURVE('',#15489,#15489,#12994,.T.);
#19702=EDGE_CURVE('',#15490,#15490,#12995,.T.);
#19703=EDGE_CURVE('',#15491,#15491,#12996,.T.);
#19704=EDGE_CURVE('',#15482,#15492,#9338,.T.);
#19705=EDGE_CURVE('',#15492,#15492,#12997,.T.);
#19706=EDGE_CURVE('',#15493,#15493,#12998,.T.);
#19707=EDGE_CURVE('',#15493,#15488,#9339,.T.);
#19708=EDGE_CURVE('',#15493,#15494,#9340,.T.);
#19709=EDGE_CURVE('',#15494,#15494,#12999,.T.);
#19710=EDGE_CURVE('',#15495,#15492,#9341,.T.);
#19711=EDGE_CURVE('',#15496,#15494,#9342,.T.);
#19712=EDGE_CURVE('',#15497,#15497,#13000,.T.);
#19713=EDGE_CURVE('',#15497,#15491,#9343,.T.);
#19714=EDGE_CURVE('',#15497,#15498,#9344,.T.);
#19715=EDGE_CURVE('',#15498,#15498,#13001,.T.);
#19716=EDGE_CURVE('',#15499,#15499,#13002,.T.);
#19717=EDGE_CURVE('',#15499,#15489,#9345,.T.);
#19718=EDGE_CURVE('',#15499,#15500,#9346,.T.);
#19719=EDGE_CURVE('',#15500,#15500,#13003,.T.);
#19720=EDGE_CURVE('',#15501,#15501,#13004,.T.);
#19721=EDGE_CURVE('',#15502,#15502,#13005,.T.);
#19722=EDGE_CURVE('',#15501,#15503,#9347,.T.);
#19723=EDGE_CURVE('',#15503,#15503,#13006,.T.);
#19724=EDGE_CURVE('',#15502,#15504,#9348,.T.);
#19725=EDGE_CURVE('',#15504,#15504,#13007,.T.);
#19726=EDGE_CURVE('',#15505,#15505,#13008,.T.);
#19727=EDGE_CURVE('',#15505,#15506,#9349,.T.);
#19728=EDGE_CURVE('',#15506,#15506,#13009,.T.);
#19729=EDGE_CURVE('',#15507,#15507,#13010,.T.);
#19730=EDGE_CURVE('',#15507,#15505,#9350,.T.);
#19731=EDGE_CURVE('',#15478,#15508,#9351,.T.);
#19732=EDGE_CURVE('',#15509,#15480,#9352,.T.);
#19733=EDGE_CURVE('',#15509,#15510,#9353,.T.);
#19734=EDGE_CURVE('',#15469,#15510,#9354,.T.);
#19735=EDGE_CURVE('',#15511,#15471,#9355,.T.);
#19736=EDGE_CURVE('',#15511,#15508,#9356,.T.);
#19737=EDGE_CURVE('',#15507,#15490,#9357,.T.);
#19738=EDGE_CURVE('',#15508,#15484,#9358,.T.);
#19739=EDGE_CURVE('',#15485,#15511,#9359,.T.);
#19740=EDGE_CURVE('',#15487,#15509,#9360,.T.);
#19741=EDGE_CURVE('',#15510,#15486,#9361,.T.);
#19742=EDGE_CURVE('',#15512,#15513,#9362,.T.);
#19743=EDGE_CURVE('',#15512,#15514,#1429,.T.);
#19744=EDGE_CURVE('',#15515,#15514,#13011,.T.);
#19745=EDGE_CURVE('',#15515,#15513,#1430,.T.);
#19746=EDGE_CURVE('',#15516,#15517,#9363,.T.);
#19747=EDGE_CURVE('',#15516,#15512,#1431,.T.);
#19748=EDGE_CURVE('',#15513,#15517,#1432,.T.);
#19749=EDGE_CURVE('',#15518,#15519,#9364,.T.);
#19750=EDGE_CURVE('',#15518,#15516,#1433,.T.);
#19751=EDGE_CURVE('',#15517,#15519,#1434,.T.);
#19752=EDGE_CURVE('',#15520,#15521,#9365,.T.);
#19753=EDGE_CURVE('',#15520,#15522,#1435,.T.);
#19754=EDGE_CURVE('',#15522,#15518,#1436,.T.);
#19755=EDGE_CURVE('',#15519,#15523,#1437,.T.);
#19756=EDGE_CURVE('',#15523,#15521,#1438,.T.);
#19757=EDGE_CURVE('',#15524,#15525,#9366,.T.);
#19758=EDGE_CURVE('',#15524,#15520,#1439,.T.);
#19759=EDGE_CURVE('',#15521,#15525,#1440,.T.);
#19760=EDGE_CURVE('',#15526,#15527,#9367,.T.);
#19761=EDGE_CURVE('',#15526,#15524,#1441,.T.);
#19762=EDGE_CURVE('',#15525,#15527,#1442,.T.);
#19763=EDGE_CURVE('',#15528,#15529,#9368,.T.);
#19764=EDGE_CURVE('',#15528,#15530,#1443,.T.);
#19765=EDGE_CURVE('',#15530,#15526,#1444,.T.);
#19766=EDGE_CURVE('',#15527,#15531,#1445,.T.);
#19767=EDGE_CURVE('',#15531,#15529,#1446,.T.);
#19768=EDGE_CURVE('',#15532,#15533,#9369,.T.);
#19769=EDGE_CURVE('',#15532,#15534,#1447,.T.);
#19770=EDGE_CURVE('',#15534,#15528,#1448,.T.);
#19771=EDGE_CURVE('',#15529,#15535,#1449,.T.);
#19772=EDGE_CURVE('',#15535,#15533,#1450,.T.);
#19773=EDGE_CURVE('',#15536,#15537,#9370,.T.);
#19774=EDGE_CURVE('',#15536,#15532,#1451,.T.);
#19775=EDGE_CURVE('',#15533,#15537,#1452,.T.);
#19776=EDGE_CURVE('',#15538,#15539,#9371,.T.);
#19777=EDGE_CURVE('',#15538,#15536,#1453,.T.);
#19778=EDGE_CURVE('',#15537,#15539,#1454,.T.);
#19779=EDGE_CURVE('',#15540,#15541,#9372,.T.);
#19780=EDGE_CURVE('',#15540,#15542,#1455,.T.);
#19781=EDGE_CURVE('',#15542,#15538,#1456,.T.);
#19782=EDGE_CURVE('',#15539,#15543,#1457,.T.);
#19783=EDGE_CURVE('',#15543,#15541,#1458,.T.);
#19784=EDGE_CURVE('',#15544,#15545,#9373,.T.);
#19785=EDGE_CURVE('',#15544,#15540,#1459,.T.);
#19786=EDGE_CURVE('',#15541,#15545,#1460,.T.);
#19787=EDGE_CURVE('',#15546,#15547,#9374,.T.);
#19788=EDGE_CURVE('',#15546,#15548,#1461,.T.);
#19789=EDGE_CURVE('',#15548,#15544,#1462,.T.);
#19790=EDGE_CURVE('',#15545,#15549,#1463,.T.);
#19791=EDGE_CURVE('',#15549,#15547,#1464,.T.);
#19792=EDGE_CURVE('',#15550,#15551,#9375,.T.);
#19793=EDGE_CURVE('',#15550,#15552,#1465,.T.);
#19794=EDGE_CURVE('',#15552,#15546,#1466,.T.);
#19795=EDGE_CURVE('',#15547,#15553,#1467,.T.);
#19796=EDGE_CURVE('',#15553,#15551,#1468,.T.);
#19797=EDGE_CURVE('',#15554,#15555,#9376,.T.);
#19798=EDGE_CURVE('',#15554,#15550,#1469,.T.);
#19799=EDGE_CURVE('',#15551,#15555,#1470,.T.);
#19800=EDGE_CURVE('',#15556,#15557,#9377,.T.);
#19801=EDGE_CURVE('',#15556,#15554,#1471,.T.);
#19802=EDGE_CURVE('',#15555,#15557,#1472,.T.);
#19803=EDGE_CURVE('',#15558,#15559,#9378,.T.);
#19804=EDGE_CURVE('',#15558,#15560,#1473,.T.);
#19805=EDGE_CURVE('',#15560,#15556,#1474,.T.);
#19806=EDGE_CURVE('',#15557,#15561,#1475,.T.);
#19807=EDGE_CURVE('',#15561,#15559,#1476,.T.);
#19808=EDGE_CURVE('',#15562,#15563,#9379,.T.);
#19809=EDGE_CURVE('',#15562,#15558,#1477,.T.);
#19810=EDGE_CURVE('',#15559,#15563,#1478,.T.);
#19811=EDGE_CURVE('',#15564,#15565,#9380,.T.);
#19812=EDGE_CURVE('',#15564,#15562,#1479,.T.);
#19813=EDGE_CURVE('',#15563,#15565,#1480,.T.);
#19814=EDGE_CURVE('',#15566,#15567,#9381,.T.);
#19815=EDGE_CURVE('',#15566,#15568,#1481,.T.);
#19816=EDGE_CURVE('',#15568,#15564,#1482,.T.);
#19817=EDGE_CURVE('',#15565,#15569,#1483,.T.);
#19818=EDGE_CURVE('',#15569,#15567,#1484,.T.);
#19819=EDGE_CURVE('',#15570,#15571,#9382,.T.);
#19820=EDGE_CURVE('',#15570,#15566,#1485,.T.);
#19821=EDGE_CURVE('',#15567,#15571,#1486,.T.);
#19822=EDGE_CURVE('',#15572,#15573,#9383,.T.);
#19823=EDGE_CURVE('',#15572,#15570,#1487,.T.);
#19824=EDGE_CURVE('',#15571,#15573,#1488,.T.);
#19825=EDGE_CURVE('',#15574,#15575,#9384,.T.);
#19826=EDGE_CURVE('',#15574,#15576,#1489,.T.);
#19827=EDGE_CURVE('',#15576,#15572,#1490,.T.);
#19828=EDGE_CURVE('',#15573,#15575,#1491,.T.);
#19829=EDGE_CURVE('',#15577,#15578,#9385,.T.);
#19830=EDGE_CURVE('',#15579,#15577,#1492,.F.);
#19831=EDGE_CURVE('',#15580,#15579,#13012,.T.);
#19832=EDGE_CURVE('',#15580,#15578,#1493,.T.);
#19833=EDGE_CURVE('',#15581,#15582,#9386,.T.);
#19834=EDGE_CURVE('',#15577,#15581,#1494,.F.);
#19835=EDGE_CURVE('',#15578,#15582,#1495,.T.);
#19836=EDGE_CURVE('',#15583,#15584,#9387,.T.);
#19837=EDGE_CURVE('',#15581,#15583,#1496,.F.);
#19838=EDGE_CURVE('',#15582,#15584,#1497,.T.);
#19839=EDGE_CURVE('',#15585,#15586,#9388,.T.);
#19840=EDGE_CURVE('',#15583,#15585,#1498,.F.);
#19841=EDGE_CURVE('',#15584,#15586,#1499,.T.);
#19842=EDGE_CURVE('',#15587,#15588,#9389,.T.);
#19843=EDGE_CURVE('',#15589,#15587,#1500,.F.);
#19844=EDGE_CURVE('',#15585,#15589,#1501,.F.);
#19845=EDGE_CURVE('',#15586,#15588,#1502,.T.);
#19846=EDGE_CURVE('',#15590,#15591,#9390,.T.);
#19847=EDGE_CURVE('',#15587,#15590,#1503,.F.);
#19848=EDGE_CURVE('',#15588,#15592,#1504,.T.);
#19849=EDGE_CURVE('',#15592,#15591,#1505,.T.);
#19850=EDGE_CURVE('',#15593,#15594,#9391,.T.);
#19851=EDGE_CURVE('',#15590,#15593,#1506,.F.);
#19852=EDGE_CURVE('',#15591,#15594,#1507,.T.);
#19853=EDGE_CURVE('',#15595,#15596,#9392,.T.);
#19854=EDGE_CURVE('',#15593,#15595,#1508,.F.);
#19855=EDGE_CURVE('',#15594,#15596,#1509,.T.);
#19856=EDGE_CURVE('',#15597,#15598,#9393,.T.);
#19857=EDGE_CURVE('',#15595,#15597,#1510,.F.);
#19858=EDGE_CURVE('',#15596,#15598,#1511,.T.);
#19859=EDGE_CURVE('',#15599,#15600,#9394,.T.);
#19860=EDGE_CURVE('',#15597,#15599,#1512,.F.);
#19861=EDGE_CURVE('',#15598,#15600,#1513,.T.);
#19862=EDGE_CURVE('',#15601,#15602,#9395,.T.);
#19863=EDGE_CURVE('',#15599,#15601,#1514,.F.);
#19864=EDGE_CURVE('',#15600,#15602,#1515,.T.);
#19865=EDGE_CURVE('',#15603,#15604,#9396,.T.);
#19866=EDGE_CURVE('',#15601,#15603,#1516,.F.);
#19867=EDGE_CURVE('',#15602,#15604,#1517,.T.);
#19868=EDGE_CURVE('',#15605,#15606,#9397,.T.);
#19869=EDGE_CURVE('',#15603,#15605,#1518,.F.);
#19870=EDGE_CURVE('',#15604,#15606,#1519,.T.);
#19871=EDGE_CURVE('',#15607,#15608,#9398,.T.);
#19872=EDGE_CURVE('',#15605,#15607,#1520,.F.);
#19873=EDGE_CURVE('',#15606,#15608,#1521,.T.);
#19874=EDGE_CURVE('',#15609,#15610,#9399,.T.);
#19875=EDGE_CURVE('',#15611,#15609,#1522,.F.);
#19876=EDGE_CURVE('',#15607,#15611,#1523,.F.);
#19877=EDGE_CURVE('',#15608,#15610,#1524,.T.);
#19878=EDGE_CURVE('',#15612,#15613,#9400,.T.);
#19879=EDGE_CURVE('',#15609,#15612,#1525,.F.);
#19880=EDGE_CURVE('',#15610,#15613,#1526,.T.);
#19881=EDGE_CURVE('',#15614,#15615,#9401,.T.);
#19882=EDGE_CURVE('',#15612,#15614,#1527,.F.);
#19883=EDGE_CURVE('',#15613,#15615,#1528,.T.);
#19884=EDGE_CURVE('',#15616,#15617,#9402,.T.);
#19885=EDGE_CURVE('',#15614,#15616,#1529,.F.);
#19886=EDGE_CURVE('',#15615,#15617,#1530,.T.);
#19887=EDGE_CURVE('',#15618,#15619,#9403,.T.);
#19888=EDGE_CURVE('',#15616,#15618,#1531,.F.);
#19889=EDGE_CURVE('',#15617,#15619,#1532,.T.);
#19890=EDGE_CURVE('',#15620,#15621,#9404,.T.);
#19891=EDGE_CURVE('',#15618,#15620,#1533,.F.);
#19892=EDGE_CURVE('',#15619,#15621,#1534,.T.);
#19893=EDGE_CURVE('',#15622,#15623,#9405,.T.);
#19894=EDGE_CURVE('',#15620,#15622,#1535,.F.);
#19895=EDGE_CURVE('',#15621,#15624,#1536,.T.);
#19896=EDGE_CURVE('',#15624,#15623,#1537,.T.);
#19897=EDGE_CURVE('',#15625,#15626,#9406,.T.);
#19898=EDGE_CURVE('',#15622,#15625,#1538,.F.);
#19899=EDGE_CURVE('',#15623,#15626,#1539,.T.);
#19900=EDGE_CURVE('',#15627,#15628,#9407,.T.);
#19901=EDGE_CURVE('',#15625,#15627,#1540,.F.);
#19902=EDGE_CURVE('',#15626,#15628,#1541,.T.);
#19903=EDGE_CURVE('',#15628,#15629,#1542,.T.);
#19904=EDGE_CURVE('',#15630,#15629,#13013,.T.);
#19905=EDGE_CURVE('',#15631,#15630,#1543,.T.);
#19906=EDGE_CURVE('',#15627,#15631,#1544,.T.);
#19907=EDGE_CURVE('',#15575,#15632,#1545,.T.);
#19908=EDGE_CURVE('',#15633,#15632,#13014,.T.);
#19909=EDGE_CURVE('',#15633,#15574,#1546,.T.);
#19910=EDGE_CURVE('',#15634,#15635,#13015,.T.);
#19911=EDGE_CURVE('',#15634,#15630,#1547,.T.);
#19912=EDGE_CURVE('',#15629,#15633,#1548,.T.);
#19913=EDGE_CURVE('',#15635,#15633,#13016,.T.);
#19914=EDGE_CURVE('',#15632,#15634,#1549,.T.);
#19915=EDGE_CURVE('',#15579,#15515,#1550,.F.);
#19916=EDGE_CURVE('',#15636,#15637,#13017,.T.);
#19917=EDGE_CURVE('',#15636,#15580,#1551,.T.);
#19918=EDGE_CURVE('',#15637,#15515,#13018,.T.);
#19919=EDGE_CURVE('',#15514,#15636,#1552,.T.);
#19920=EDGE_CURVE('',#15638,#15638,#13019,.T.);
#19921=EDGE_CURVE('',#15638,#15637,#13020,.T.);
#19922=EDGE_CURVE('',#15639,#15639,#13021,.T.);
#19923=EDGE_CURVE('',#15635,#15640,#9408,.T.);
#19924=EDGE_CURVE('',#15640,#15640,#13022,.T.);
#19925=EDGE_CURVE('',#15641,#15642,#13023,.T.);
#19926=EDGE_CURVE('',#15643,#15641,#9409,.T.);
#19927=EDGE_CURVE('',#15642,#15643,#9410,.T.);
#19928=EDGE_CURVE('',#15642,#15644,#9411,.T.);
#19929=EDGE_CURVE('',#15645,#15643,#9412,.T.);
#19930=EDGE_CURVE('',#15644,#15645,#116,.T.);
#19931=EDGE_CURVE('',#15646,#15641,#9413,.T.);
#19932=EDGE_CURVE('',#15645,#15646,#117,.T.);
#19933=EDGE_CURVE('',#15647,#15648,#13024,.T.);
#19934=EDGE_CURVE('',#15648,#15649,#9414,.T.);
#19935=EDGE_CURVE('',#15650,#15649,#13025,.T.);
#19936=EDGE_CURVE('',#15649,#15650,#13026,.T.);
#19937=EDGE_CURVE('',#15648,#15651,#13027,.T.);
#19938=EDGE_CURVE('',#15651,#15652,#9415,.T.);
#19939=EDGE_CURVE('',#15653,#15652,#13028,.T.);
#19940=EDGE_CURVE('',#15653,#15654,#9416,.T.);
#19941=EDGE_CURVE('',#15654,#15655,#13029,.T.);
#19942=EDGE_CURVE('',#15655,#15656,#9417,.T.);
#19943=EDGE_CURVE('',#15657,#15656,#13030,.T.);
#19944=EDGE_CURVE('',#15657,#15658,#9418,.T.);
#19945=EDGE_CURVE('',#15658,#15659,#13031,.T.);
#19946=EDGE_CURVE('',#15659,#15660,#9419,.T.);
#19947=EDGE_CURVE('',#15661,#15660,#13032,.T.);
#19948=EDGE_CURVE('',#15661,#15662,#9420,.T.);
#19949=EDGE_CURVE('',#15662,#15663,#13033,.T.);
#19950=EDGE_CURVE('',#15663,#15664,#9421,.T.);
#19951=EDGE_CURVE('',#15665,#15664,#13034,.T.);
#19952=EDGE_CURVE('',#15665,#15666,#9422,.T.);
#19953=EDGE_CURVE('',#15666,#15667,#13035,.T.);
#19954=EDGE_CURVE('',#15667,#15668,#9423,.T.);
#19955=EDGE_CURVE('',#15669,#15668,#13036,.T.);
#19956=EDGE_CURVE('',#15669,#15670,#9424,.T.);
#19957=EDGE_CURVE('',#15670,#15671,#13037,.T.);
#19958=EDGE_CURVE('',#15671,#15672,#9425,.T.);
#19959=EDGE_CURVE('',#15673,#15672,#13038,.T.);
#19960=EDGE_CURVE('',#15673,#15674,#9426,.T.);
#19961=EDGE_CURVE('',#15674,#15675,#13039,.T.);
#19962=EDGE_CURVE('',#15675,#15676,#9427,.T.);
#19963=EDGE_CURVE('',#15677,#15676,#13040,.T.);
#19964=EDGE_CURVE('',#15677,#15678,#9428,.T.);
#19965=EDGE_CURVE('',#15678,#15679,#13041,.T.);
#19966=EDGE_CURVE('',#15679,#15680,#9429,.T.);
#19967=EDGE_CURVE('',#15681,#15680,#13042,.T.);
#19968=EDGE_CURVE('',#15681,#15682,#9430,.T.);
#19969=EDGE_CURVE('',#15682,#15683,#13043,.T.);
#19970=EDGE_CURVE('',#15683,#15684,#9431,.T.);
#19971=EDGE_CURVE('',#15685,#15684,#13044,.T.);
#19972=EDGE_CURVE('',#15685,#15686,#9432,.T.);
#19973=EDGE_CURVE('',#15686,#15687,#13045,.T.);
#19974=EDGE_CURVE('',#15687,#15688,#9433,.T.);
#19975=EDGE_CURVE('',#15689,#15688,#13046,.T.);
#19976=EDGE_CURVE('',#15689,#15690,#9434,.T.);
#19977=EDGE_CURVE('',#15690,#15691,#13047,.T.);
#19978=EDGE_CURVE('',#15691,#15692,#9435,.T.);
#19979=EDGE_CURVE('',#15693,#15692,#13048,.T.);
#19980=EDGE_CURVE('',#15693,#15694,#9436,.T.);
#19981=EDGE_CURVE('',#15694,#15695,#13049,.T.);
#19982=EDGE_CURVE('',#15695,#15696,#9437,.T.);
#19983=EDGE_CURVE('',#15697,#15696,#13050,.T.);
#19984=EDGE_CURVE('',#15697,#15698,#9438,.T.);
#19985=EDGE_CURVE('',#15698,#15699,#13051,.T.);
#19986=EDGE_CURVE('',#15699,#15700,#9439,.T.);
#19987=EDGE_CURVE('',#15701,#15700,#13052,.T.);
#19988=EDGE_CURVE('',#15701,#15702,#9440,.T.);
#19989=EDGE_CURVE('',#15702,#15703,#13053,.T.);
#19990=EDGE_CURVE('',#15703,#15704,#9441,.T.);
#19991=EDGE_CURVE('',#15705,#15704,#13054,.T.);
#19992=EDGE_CURVE('',#15705,#15706,#9442,.T.);
#19993=EDGE_CURVE('',#15706,#15707,#13055,.T.);
#19994=EDGE_CURVE('',#15707,#15708,#9443,.T.);
#19995=EDGE_CURVE('',#15709,#15708,#13056,.T.);
#19996=EDGE_CURVE('',#15709,#15710,#9444,.T.);
#19997=EDGE_CURVE('',#15710,#15711,#13057,.T.);
#19998=EDGE_CURVE('',#15711,#15712,#9445,.T.);
#19999=EDGE_CURVE('',#15713,#15712,#13058,.T.);
#20000=EDGE_CURVE('',#15713,#15714,#9446,.T.);
#20001=EDGE_CURVE('',#15714,#15715,#13059,.T.);
#20002=EDGE_CURVE('',#15715,#15716,#9447,.T.);
#20003=EDGE_CURVE('',#15646,#15716,#13060,.T.);
#20004=EDGE_CURVE('',#15717,#15644,#13061,.T.);
#20005=EDGE_CURVE('',#15717,#15718,#9448,.T.);
#20006=EDGE_CURVE('',#15718,#15719,#13062,.T.);
#20007=EDGE_CURVE('',#15719,#15720,#9449,.T.);
#20008=EDGE_CURVE('',#15721,#15720,#13063,.T.);
#20009=EDGE_CURVE('',#15721,#15722,#9450,.T.);
#20010=EDGE_CURVE('',#15722,#15723,#13064,.T.);
#20011=EDGE_CURVE('',#15723,#15724,#9451,.T.);
#20012=EDGE_CURVE('',#15725,#15724,#13065,.T.);
#20013=EDGE_CURVE('',#15725,#15726,#9452,.T.);
#20014=EDGE_CURVE('',#15726,#15727,#13066,.T.);
#20015=EDGE_CURVE('',#15727,#15728,#9453,.T.);
#20016=EDGE_CURVE('',#15729,#15728,#13067,.T.);
#20017=EDGE_CURVE('',#15729,#15730,#9454,.T.);
#20018=EDGE_CURVE('',#15730,#15731,#13068,.T.);
#20019=EDGE_CURVE('',#15731,#15732,#9455,.T.);
#20020=EDGE_CURVE('',#15733,#15732,#13069,.T.);
#20021=EDGE_CURVE('',#15733,#15734,#9456,.T.);
#20022=EDGE_CURVE('',#15734,#15735,#13070,.T.);
#20023=EDGE_CURVE('',#15735,#15736,#9457,.T.);
#20024=EDGE_CURVE('',#15737,#15736,#13071,.T.);
#20025=EDGE_CURVE('',#15737,#15738,#9458,.T.);
#20026=EDGE_CURVE('',#15738,#15739,#13072,.T.);
#20027=EDGE_CURVE('',#15739,#15740,#9459,.T.);
#20028=EDGE_CURVE('',#15741,#15740,#13073,.T.);
#20029=EDGE_CURVE('',#15741,#15742,#9460,.T.);
#20030=EDGE_CURVE('',#15742,#15743,#13074,.T.);
#20031=EDGE_CURVE('',#15743,#15744,#9461,.T.);
#20032=EDGE_CURVE('',#15745,#15744,#13075,.T.);
#20033=EDGE_CURVE('',#15745,#15746,#9462,.T.);
#20034=EDGE_CURVE('',#15746,#15747,#13076,.T.);
#20035=EDGE_CURVE('',#15747,#15748,#9463,.T.);
#20036=EDGE_CURVE('',#15749,#15748,#13077,.T.);
#20037=EDGE_CURVE('',#15749,#15750,#9464,.T.);
#20038=EDGE_CURVE('',#15750,#15751,#13078,.T.);
#20039=EDGE_CURVE('',#15751,#15752,#9465,.T.);
#20040=EDGE_CURVE('',#15753,#15752,#13079,.T.);
#20041=EDGE_CURVE('',#15753,#15754,#9466,.T.);
#20042=EDGE_CURVE('',#15754,#15755,#13080,.T.);
#20043=EDGE_CURVE('',#15755,#15756,#9467,.T.);
#20044=EDGE_CURVE('',#15757,#15756,#13081,.T.);
#20045=EDGE_CURVE('',#15757,#15758,#9468,.T.);
#20046=EDGE_CURVE('',#15758,#15759,#13082,.T.);
#20047=EDGE_CURVE('',#15759,#15760,#9469,.T.);
#20048=EDGE_CURVE('',#15761,#15760,#13083,.T.);
#20049=EDGE_CURVE('',#15761,#15762,#9470,.T.);
#20050=EDGE_CURVE('',#15762,#15763,#13084,.T.);
#20051=EDGE_CURVE('',#15763,#15764,#9471,.T.);
#20052=EDGE_CURVE('',#15765,#15764,#13085,.T.);
#20053=EDGE_CURVE('',#15765,#15766,#9472,.T.);
#20054=EDGE_CURVE('',#15766,#15767,#13086,.T.);
#20055=EDGE_CURVE('',#15767,#15768,#9473,.T.);
#20056=EDGE_CURVE('',#15769,#15768,#13087,.T.);
#20057=EDGE_CURVE('',#15769,#15770,#9474,.T.);
#20058=EDGE_CURVE('',#15770,#15771,#13088,.T.);
#20059=EDGE_CURVE('',#15771,#15772,#9475,.T.);
#20060=EDGE_CURVE('',#15773,#15772,#13089,.T.);
#20061=EDGE_CURVE('',#15773,#15774,#9476,.T.);
#20062=EDGE_CURVE('',#15774,#15775,#13090,.T.);
#20063=EDGE_CURVE('',#15775,#15776,#9477,.T.);
#20064=EDGE_CURVE('',#15777,#15776,#13091,.T.);
#20065=EDGE_CURVE('',#15777,#15778,#9478,.T.);
#20066=EDGE_CURVE('',#15778,#15779,#13092,.T.);
#20067=EDGE_CURVE('',#15779,#15780,#9479,.T.);
#20068=EDGE_CURVE('',#15781,#15780,#13093,.T.);
#20069=EDGE_CURVE('',#15781,#15782,#9480,.T.);
#20070=EDGE_CURVE('',#15782,#15783,#13094,.T.);
#20071=EDGE_CURVE('',#15783,#15784,#9481,.T.);
#20072=EDGE_CURVE('',#15785,#15784,#13095,.T.);
#20073=EDGE_CURVE('',#15785,#15786,#9482,.T.);
#20074=EDGE_CURVE('',#15786,#15787,#13096,.T.);
#20075=EDGE_CURVE('',#15787,#15788,#9483,.T.);
#20076=EDGE_CURVE('',#15789,#15788,#13097,.T.);
#20077=EDGE_CURVE('',#15789,#15647,#9484,.T.);
#20078=EDGE_CURVE('',#15715,#15790,#9485,.T.);
#20079=EDGE_CURVE('',#15791,#15790,#9486,.T.);
#20080=EDGE_CURVE('',#15716,#15791,#118,.T.);
#20081=EDGE_CURVE('',#15791,#15713,#119,.T.);
#20082=EDGE_CURVE('',#15790,#15714,#9487,.T.);
#20083=EDGE_CURVE('',#15792,#15789,#120,.T.);
#20084=EDGE_CURVE('',#15788,#15793,#121,.T.);
#20085=EDGE_CURVE('',#15793,#15785,#122,.T.);
#20086=EDGE_CURVE('',#15784,#15794,#123,.T.);
#20087=EDGE_CURVE('',#15794,#15781,#124,.T.);
#20088=EDGE_CURVE('',#15780,#15795,#125,.T.);
#20089=EDGE_CURVE('',#15795,#15777,#126,.T.);
#20090=EDGE_CURVE('',#15776,#15796,#127,.T.);
#20091=EDGE_CURVE('',#15796,#15773,#128,.T.);
#20092=EDGE_CURVE('',#15772,#15797,#129,.T.);
#20093=EDGE_CURVE('',#15797,#15769,#130,.T.);
#20094=EDGE_CURVE('',#15768,#15798,#131,.T.);
#20095=EDGE_CURVE('',#15798,#15765,#132,.T.);
#20096=EDGE_CURVE('',#15764,#15799,#133,.T.);
#20097=EDGE_CURVE('',#15799,#15761,#134,.T.);
#20098=EDGE_CURVE('',#15760,#15800,#135,.T.);
#20099=EDGE_CURVE('',#15800,#15757,#136,.T.);
#20100=EDGE_CURVE('',#15756,#15801,#137,.T.);
#20101=EDGE_CURVE('',#15801,#15753,#138,.T.);
#20102=EDGE_CURVE('',#15752,#15802,#139,.T.);
#20103=EDGE_CURVE('',#15802,#15749,#140,.T.);
#20104=EDGE_CURVE('',#15748,#15803,#141,.T.);
#20105=EDGE_CURVE('',#15803,#15745,#142,.T.);
#20106=EDGE_CURVE('',#15744,#15804,#143,.T.);
#20107=EDGE_CURVE('',#15804,#15741,#144,.T.);
#20108=EDGE_CURVE('',#15740,#15805,#145,.T.);
#20109=EDGE_CURVE('',#15805,#15737,#146,.T.);
#20110=EDGE_CURVE('',#15736,#15806,#147,.T.);
#20111=EDGE_CURVE('',#15806,#15733,#148,.T.);
#20112=EDGE_CURVE('',#15732,#15807,#149,.T.);
#20113=EDGE_CURVE('',#15807,#15729,#150,.T.);
#20114=EDGE_CURVE('',#15728,#15808,#151,.T.);
#20115=EDGE_CURVE('',#15808,#15725,#152,.T.);
#20116=EDGE_CURVE('',#15724,#15809,#153,.T.);
#20117=EDGE_CURVE('',#15809,#15721,#154,.T.);
#20118=EDGE_CURVE('',#15720,#15810,#155,.T.);
#20119=EDGE_CURVE('',#15810,#15717,#156,.T.);
#20120=EDGE_CURVE('',#15712,#15811,#157,.T.);
#20121=EDGE_CURVE('',#15811,#15709,#158,.T.);
#20122=EDGE_CURVE('',#15708,#15812,#159,.T.);
#20123=EDGE_CURVE('',#15812,#15705,#160,.T.);
#20124=EDGE_CURVE('',#15704,#15813,#161,.T.);
#20125=EDGE_CURVE('',#15813,#15701,#162,.T.);
#20126=EDGE_CURVE('',#15700,#15814,#163,.T.);
#20127=EDGE_CURVE('',#15814,#15697,#164,.T.);
#20128=EDGE_CURVE('',#15696,#15815,#165,.T.);
#20129=EDGE_CURVE('',#15815,#15693,#166,.T.);
#20130=EDGE_CURVE('',#15692,#15816,#167,.T.);
#20131=EDGE_CURVE('',#15816,#15689,#168,.T.);
#20132=EDGE_CURVE('',#15688,#15817,#169,.T.);
#20133=EDGE_CURVE('',#15817,#15685,#170,.T.);
#20134=EDGE_CURVE('',#15684,#15818,#171,.T.);
#20135=EDGE_CURVE('',#15818,#15681,#172,.T.);
#20136=EDGE_CURVE('',#15680,#15819,#173,.T.);
#20137=EDGE_CURVE('',#15819,#15677,#174,.T.);
#20138=EDGE_CURVE('',#15676,#15820,#175,.T.);
#20139=EDGE_CURVE('',#15820,#15673,#176,.T.);
#20140=EDGE_CURVE('',#15672,#15821,#177,.T.);
#20141=EDGE_CURVE('',#15821,#15669,#178,.T.);
#20142=EDGE_CURVE('',#15668,#15822,#179,.T.);
#20143=EDGE_CURVE('',#15822,#15665,#180,.T.);
#20144=EDGE_CURVE('',#15664,#15823,#181,.T.);
#20145=EDGE_CURVE('',#15823,#15661,#182,.T.);
#20146=EDGE_CURVE('',#15660,#15824,#183,.T.);
#20147=EDGE_CURVE('',#15824,#15657,#184,.T.);
#20148=EDGE_CURVE('',#15656,#15825,#185,.T.);
#20149=EDGE_CURVE('',#15825,#15653,#186,.T.);
#20150=EDGE_CURVE('',#15652,#15792,#187,.T.);
#20151=EDGE_CURVE('',#15792,#15826,#9488,.T.);
#20152=EDGE_CURVE('',#15826,#15826,#13098,.T.);
#20153=EDGE_CURVE('',#15827,#15710,#9489,.T.);
#20154=EDGE_CURVE('',#15711,#15827,#9490,.T.);
#20155=EDGE_CURVE('',#15811,#15827,#9491,.T.);
#20156=EDGE_CURVE('',#15707,#15828,#9492,.T.);
#20157=EDGE_CURVE('',#15812,#15828,#9493,.T.);
#20158=EDGE_CURVE('',#15828,#15706,#9494,.T.);
#20159=EDGE_CURVE('',#15829,#15702,#9495,.T.);
#20160=EDGE_CURVE('',#15703,#15829,#9496,.T.);
#20161=EDGE_CURVE('',#15813,#15829,#9497,.T.);
#20162=EDGE_CURVE('',#15699,#15830,#9498,.T.);
#20163=EDGE_CURVE('',#15814,#15830,#9499,.T.);
#20164=EDGE_CURVE('',#15830,#15698,#9500,.T.);
#20165=EDGE_CURVE('',#15831,#15694,#9501,.T.);
#20166=EDGE_CURVE('',#15695,#15831,#9502,.T.);
#20167=EDGE_CURVE('',#15815,#15831,#9503,.T.);
#20168=EDGE_CURVE('',#15691,#15832,#9504,.T.);
#20169=EDGE_CURVE('',#15816,#15832,#9505,.T.);
#20170=EDGE_CURVE('',#15832,#15690,#9506,.T.);
#20171=EDGE_CURVE('',#15833,#15686,#9507,.T.);
#20172=EDGE_CURVE('',#15687,#15833,#9508,.T.);
#20173=EDGE_CURVE('',#15817,#15833,#9509,.T.);
#20174=EDGE_CURVE('',#15683,#15834,#9510,.T.);
#20175=EDGE_CURVE('',#15818,#15834,#9511,.T.);
#20176=EDGE_CURVE('',#15834,#15682,#9512,.T.);
#20177=EDGE_CURVE('',#15835,#15678,#9513,.T.);
#20178=EDGE_CURVE('',#15679,#15835,#9514,.T.);
#20179=EDGE_CURVE('',#15819,#15835,#9515,.T.);
#20180=EDGE_CURVE('',#15675,#15836,#9516,.T.);
#20181=EDGE_CURVE('',#15820,#15836,#9517,.T.);
#20182=EDGE_CURVE('',#15836,#15674,#9518,.T.);
#20183=EDGE_CURVE('',#15837,#15670,#9519,.T.);
#20184=EDGE_CURVE('',#15671,#15837,#9520,.T.);
#20185=EDGE_CURVE('',#15821,#15837,#9521,.T.);
#20186=EDGE_CURVE('',#15667,#15838,#9522,.T.);
#20187=EDGE_CURVE('',#15822,#15838,#9523,.T.);
#20188=EDGE_CURVE('',#15838,#15666,#9524,.T.);
#20189=EDGE_CURVE('',#15839,#15662,#9525,.T.);
#20190=EDGE_CURVE('',#15663,#15839,#9526,.T.);
#20191=EDGE_CURVE('',#15823,#15839,#9527,.T.);
#20192=EDGE_CURVE('',#15659,#15840,#9528,.T.);
#20193=EDGE_CURVE('',#15824,#15840,#9529,.T.);
#20194=EDGE_CURVE('',#15840,#15658,#9530,.T.);
#20195=EDGE_CURVE('',#15841,#15654,#9531,.T.);
#20196=EDGE_CURVE('',#15655,#15841,#9532,.T.);
#20197=EDGE_CURVE('',#15825,#15841,#9533,.T.);
#20198=EDGE_CURVE('',#15651,#15842,#9534,.T.);
#20199=EDGE_CURVE('',#15792,#15842,#9535,.T.);
#20200=EDGE_CURVE('',#15842,#15647,#9536,.T.);
#20201=EDGE_CURVE('',#15843,#15786,#9537,.T.);
#20202=EDGE_CURVE('',#15787,#15843,#9538,.T.);
#20203=EDGE_CURVE('',#15793,#15843,#9539,.T.);
#20204=EDGE_CURVE('',#15783,#15844,#9540,.T.);
#20205=EDGE_CURVE('',#15794,#15844,#9541,.T.);
#20206=EDGE_CURVE('',#15844,#15782,#9542,.T.);
#20207=EDGE_CURVE('',#15845,#15778,#9543,.T.);
#20208=EDGE_CURVE('',#15779,#15845,#9544,.T.);
#20209=EDGE_CURVE('',#15795,#15845,#9545,.T.);
#20210=EDGE_CURVE('',#15775,#15846,#9546,.T.);
#20211=EDGE_CURVE('',#15796,#15846,#9547,.T.);
#20212=EDGE_CURVE('',#15846,#15774,#9548,.T.);
#20213=EDGE_CURVE('',#15847,#15770,#9549,.T.);
#20214=EDGE_CURVE('',#15771,#15847,#9550,.T.);
#20215=EDGE_CURVE('',#15797,#15847,#9551,.T.);
#20216=EDGE_CURVE('',#15767,#15848,#9552,.T.);
#20217=EDGE_CURVE('',#15798,#15848,#9553,.T.);
#20218=EDGE_CURVE('',#15848,#15766,#9554,.T.);
#20219=EDGE_CURVE('',#15849,#15762,#9555,.T.);
#20220=EDGE_CURVE('',#15763,#15849,#9556,.T.);
#20221=EDGE_CURVE('',#15799,#15849,#9557,.T.);
#20222=EDGE_CURVE('',#15759,#15850,#9558,.T.);
#20223=EDGE_CURVE('',#15800,#15850,#9559,.T.);
#20224=EDGE_CURVE('',#15850,#15758,#9560,.T.);
#20225=EDGE_CURVE('',#15851,#15754,#9561,.T.);
#20226=EDGE_CURVE('',#15755,#15851,#9562,.T.);
#20227=EDGE_CURVE('',#15801,#15851,#9563,.T.);
#20228=EDGE_CURVE('',#15751,#15852,#9564,.T.);
#20229=EDGE_CURVE('',#15802,#15852,#9565,.T.);
#20230=EDGE_CURVE('',#15852,#15750,#9566,.T.);
#20231=EDGE_CURVE('',#15853,#15746,#9567,.T.);
#20232=EDGE_CURVE('',#15747,#15853,#9568,.T.);
#20233=EDGE_CURVE('',#15803,#15853,#9569,.T.);
#20234=EDGE_CURVE('',#15743,#15854,#9570,.T.);
#20235=EDGE_CURVE('',#15804,#15854,#9571,.T.);
#20236=EDGE_CURVE('',#15854,#15742,#9572,.T.);
#20237=EDGE_CURVE('',#15855,#15738,#9573,.T.);
#20238=EDGE_CURVE('',#15739,#15855,#9574,.T.);
#20239=EDGE_CURVE('',#15805,#15855,#9575,.T.);
#20240=EDGE_CURVE('',#15735,#15856,#9576,.T.);
#20241=EDGE_CURVE('',#15806,#15856,#9577,.T.);
#20242=EDGE_CURVE('',#15856,#15734,#9578,.T.);
#20243=EDGE_CURVE('',#15857,#15730,#9579,.T.);
#20244=EDGE_CURVE('',#15731,#15857,#9580,.T.);
#20245=EDGE_CURVE('',#15807,#15857,#9581,.T.);
#20246=EDGE_CURVE('',#15727,#15858,#9582,.T.);
#20247=EDGE_CURVE('',#15808,#15858,#9583,.T.);
#20248=EDGE_CURVE('',#15858,#15726,#9584,.T.);
#20249=EDGE_CURVE('',#15859,#15722,#9585,.T.);
#20250=EDGE_CURVE('',#15723,#15859,#9586,.T.);
#20251=EDGE_CURVE('',#15809,#15859,#9587,.T.);
#20252=EDGE_CURVE('',#15719,#15860,#9588,.T.);
#20253=EDGE_CURVE('',#15810,#15860,#9589,.T.);
#20254=EDGE_CURVE('',#15860,#15718,#9590,.T.);
#20255=EDGE_CURVE('',#15639,#15650,#13099,.T.);
#20256=EDGE_CURVE('',#15861,#15861,#13100,.T.);
#20257=EDGE_CURVE('',#15862,#15863,#188,.T.);
#20258=EDGE_CURVE('',#15864,#15862,#13101,.T.);
#20259=EDGE_CURVE('',#15865,#15864,#189,.T.);
#20260=EDGE_CURVE('',#15866,#15865,#190,.T.);
#20261=EDGE_CURVE('',#15867,#15866,#13102,.T.);
#20262=EDGE_CURVE('',#15868,#15867,#191,.T.);
#20263=EDGE_CURVE('',#15869,#15868,#192,.T.);
#20264=EDGE_CURVE('',#15870,#15869,#13103,.T.);
#20265=EDGE_CURVE('',#15871,#15870,#193,.T.);
#20266=EDGE_CURVE('',#15872,#15871,#194,.T.);
#20267=EDGE_CURVE('',#15873,#15872,#13104,.T.);
#20268=EDGE_CURVE('',#15874,#15873,#195,.T.);
#20269=EDGE_CURVE('',#15875,#15874,#196,.T.);
#20270=EDGE_CURVE('',#15876,#15875,#13105,.T.);
#20271=EDGE_CURVE('',#15877,#15876,#197,.T.);
#20272=EDGE_CURVE('',#15878,#15877,#198,.T.);
#20273=EDGE_CURVE('',#15879,#15878,#13106,.T.);
#20274=EDGE_CURVE('',#15863,#15879,#199,.T.);
#20275=EDGE_CURVE('',#15863,#15861,#9591,.T.);
#20276=EDGE_CURVE('',#15879,#15880,#9592,.T.);
#20277=EDGE_CURVE('',#15881,#15878,#9593,.T.);
#20278=EDGE_CURVE('',#15880,#15881,#13107,.T.);
#20279=EDGE_CURVE('',#15882,#15875,#9594,.T.);
#20280=EDGE_CURVE('',#15883,#15882,#13108,.T.);
#20281=EDGE_CURVE('',#15876,#15883,#9595,.T.);
#20282=EDGE_CURVE('',#15864,#15884,#9596,.T.);
#20283=EDGE_CURVE('',#15885,#15862,#9597,.T.);
#20284=EDGE_CURVE('',#15884,#15885,#13109,.T.);
#20285=EDGE_CURVE('',#15886,#15872,#9598,.T.);
#20286=EDGE_CURVE('',#15887,#15886,#13110,.T.);
#20287=EDGE_CURVE('',#15873,#15887,#9599,.T.);
#20288=EDGE_CURVE('',#15867,#15888,#9600,.T.);
#20289=EDGE_CURVE('',#15889,#15866,#9601,.T.);
#20290=EDGE_CURVE('',#15888,#15889,#13111,.T.);
#20291=EDGE_CURVE('',#15890,#15869,#9602,.T.);
#20292=EDGE_CURVE('',#15891,#15890,#13112,.T.);
#20293=EDGE_CURVE('',#15870,#15891,#9603,.T.);
#20294=EDGE_CURVE('',#15889,#15888,#9604,.T.);
#20295=EDGE_CURVE('',#15865,#15892,#9605,.T.);
#20296=EDGE_CURVE('',#15892,#15893,#9606,.T.);
#20297=EDGE_CURVE('',#15868,#15893,#9607,.T.);
#20298=EDGE_CURVE('',#15885,#15884,#9608,.T.);
#20299=EDGE_CURVE('',#15863,#15894,#9609,.T.);
#20300=EDGE_CURVE('',#15894,#15892,#9610,.T.);
#20301=EDGE_CURVE('',#15881,#15880,#9611,.T.);
#20302=EDGE_CURVE('',#15877,#15895,#9612,.T.);
#20303=EDGE_CURVE('',#15895,#15894,#9613,.T.);
#20304=EDGE_CURVE('',#15882,#15883,#9614,.T.);
#20305=EDGE_CURVE('',#15886,#15887,#9615,.T.);
#20306=EDGE_CURVE('',#15890,#15891,#9616,.T.);
#20307=EDGE_CURVE('',#15896,#15897,#9617,.T.);
#20308=EDGE_CURVE('',#15897,#15896,#13113,.T.);
#20309=EDGE_CURVE('',#15897,#15895,#9618,.T.);
#20310=EDGE_CURVE('',#15895,#15897,#13114,.T.);
#20311=EDGE_CURVE('',#15894,#15895,#13115,.T.);
#20312=EDGE_CURVE('',#15892,#15894,#13116,.T.);
#20313=EDGE_CURVE('',#15893,#15892,#13117,.T.);
#20314=EDGE_CURVE('',#15893,#15896,#9619,.T.);
#20315=EDGE_CURVE('',#15896,#15893,#13118,.T.);
#20316=EDGE_CURVE('',#15898,#15894,#9620,.T.);
#20317=EDGE_CURVE('',#15871,#15896,#9621,.T.);
#20318=EDGE_CURVE('',#15874,#15897,#9622,.T.);
#20319=EDGE_CURVE('',#15899,#15900,#9623,.T.);
#20320=EDGE_CURVE('',#15899,#15901,#1553,.T.);
#20321=EDGE_CURVE('',#15902,#15901,#13119,.T.);
#20322=EDGE_CURVE('',#15902,#15900,#1554,.T.);
#20323=EDGE_CURVE('',#15903,#15904,#9624,.T.);
#20324=EDGE_CURVE('',#15903,#15899,#1555,.T.);
#20325=EDGE_CURVE('',#15900,#15904,#1556,.T.);
#20326=EDGE_CURVE('',#15905,#15906,#9625,.T.);
#20327=EDGE_CURVE('',#15905,#15903,#1557,.T.);
#20328=EDGE_CURVE('',#15904,#15906,#1558,.T.);
#20329=EDGE_CURVE('',#15907,#15908,#9626,.T.);
#20330=EDGE_CURVE('',#15907,#15905,#1559,.T.);
#20331=EDGE_CURVE('',#15906,#15909,#1560,.T.);
#20332=EDGE_CURVE('',#15909,#15908,#1561,.T.);
#20333=EDGE_CURVE('',#15910,#15911,#9627,.T.);
#20334=EDGE_CURVE('',#15910,#15907,#1562,.T.);
#20335=EDGE_CURVE('',#15908,#15911,#1563,.T.);
#20336=EDGE_CURVE('',#15912,#15913,#9628,.T.);
#20337=EDGE_CURVE('',#15912,#15910,#1564,.T.);
#20338=EDGE_CURVE('',#15911,#15913,#1565,.T.);
#20339=EDGE_CURVE('',#15914,#15915,#9629,.T.);
#20340=EDGE_CURVE('',#15914,#15916,#1566,.T.);
#20341=EDGE_CURVE('',#15916,#15912,#1567,.T.);
#20342=EDGE_CURVE('',#15913,#15915,#1568,.T.);
#20343=EDGE_CURVE('',#15917,#15918,#9630,.T.);
#20344=EDGE_CURVE('',#15917,#15914,#1569,.T.);
#20345=EDGE_CURVE('',#15915,#15918,#1570,.T.);
#20346=EDGE_CURVE('',#15919,#15920,#9631,.T.);
#20347=EDGE_CURVE('',#15919,#15917,#1571,.T.);
#20348=EDGE_CURVE('',#15918,#15920,#1572,.T.);
#20349=EDGE_CURVE('',#15921,#15922,#9632,.T.);
#20350=EDGE_CURVE('',#15921,#15919,#1573,.T.);
#20351=EDGE_CURVE('',#15920,#15923,#1574,.T.);
#20352=EDGE_CURVE('',#15923,#15922,#1575,.T.);
#20353=EDGE_CURVE('',#15924,#15925,#9633,.T.);
#20354=EDGE_CURVE('',#15924,#15921,#1576,.T.);
#20355=EDGE_CURVE('',#15922,#15925,#1577,.T.);
#20356=EDGE_CURVE('',#15926,#15927,#9634,.T.);
#20357=EDGE_CURVE('',#15926,#15924,#1578,.T.);
#20358=EDGE_CURVE('',#15925,#15927,#1579,.T.);
#20359=EDGE_CURVE('',#15928,#15929,#9635,.T.);
#20360=EDGE_CURVE('',#15928,#15926,#1580,.T.);
#20361=EDGE_CURVE('',#15927,#15929,#1581,.T.);
#20362=EDGE_CURVE('',#15930,#15931,#9636,.T.);
#20363=EDGE_CURVE('',#15930,#15928,#1582,.T.);
#20364=EDGE_CURVE('',#15929,#15931,#1583,.T.);
#20365=EDGE_CURVE('',#15932,#15933,#9637,.T.);
#20366=EDGE_CURVE('',#15932,#15930,#1584,.T.);
#20367=EDGE_CURVE('',#15931,#15933,#1585,.T.);
#20368=EDGE_CURVE('',#15934,#15935,#9638,.T.);
#20369=EDGE_CURVE('',#15934,#15936,#1586,.T.);
#20370=EDGE_CURVE('',#15936,#15932,#1587,.T.);
#20371=EDGE_CURVE('',#15933,#15935,#1588,.T.);
#20372=EDGE_CURVE('',#15937,#15938,#9639,.T.);
#20373=EDGE_CURVE('',#15937,#15934,#1589,.T.);
#20374=EDGE_CURVE('',#15935,#15938,#1590,.T.);
#20375=EDGE_CURVE('',#15939,#15940,#9640,.T.);
#20376=EDGE_CURVE('',#15939,#15937,#1591,.T.);
#20377=EDGE_CURVE('',#15938,#15940,#1592,.T.);
#20378=EDGE_CURVE('',#15941,#15942,#9641,.T.);
#20379=EDGE_CURVE('',#15941,#15939,#1593,.T.);
#20380=EDGE_CURVE('',#15940,#15942,#1594,.T.);
#20381=EDGE_CURVE('',#15943,#15944,#9642,.T.);
#20382=EDGE_CURVE('',#15945,#15943,#1595,.T.);
#20383=EDGE_CURVE('',#15946,#15945,#13120,.T.);
#20384=EDGE_CURVE('',#15946,#15944,#1596,.T.);
#20385=EDGE_CURVE('',#15947,#15948,#9643,.T.);
#20386=EDGE_CURVE('',#15949,#15947,#1597,.F.);
#20387=EDGE_CURVE('',#15943,#15949,#1598,.T.);
#20388=EDGE_CURVE('',#15944,#15948,#1599,.T.);
#20389=EDGE_CURVE('',#15950,#15951,#9644,.T.);
#20390=EDGE_CURVE('',#15947,#15950,#1600,.F.);
#20391=EDGE_CURVE('',#15948,#15951,#1601,.T.);
#20392=EDGE_CURVE('',#15952,#15953,#9645,.T.);
#20393=EDGE_CURVE('',#15950,#15952,#1602,.F.);
#20394=EDGE_CURVE('',#15951,#15953,#1603,.T.);
#20395=EDGE_CURVE('',#15954,#15955,#9646,.T.);
#20396=EDGE_CURVE('',#15952,#15954,#1604,.F.);
#20397=EDGE_CURVE('',#15953,#15955,#1605,.T.);
#20398=EDGE_CURVE('',#15956,#15957,#9647,.T.);
#20399=EDGE_CURVE('',#15958,#15956,#1606,.F.);
#20400=EDGE_CURVE('',#15954,#15958,#1607,.F.);
#20401=EDGE_CURVE('',#15955,#15957,#1608,.T.);
#20402=EDGE_CURVE('',#15959,#15960,#9648,.T.);
#20403=EDGE_CURVE('',#15956,#15959,#1609,.F.);
#20404=EDGE_CURVE('',#15957,#15960,#1610,.T.);
#20405=EDGE_CURVE('',#15961,#15962,#9649,.T.);
#20406=EDGE_CURVE('',#15959,#15961,#1611,.F.);
#20407=EDGE_CURVE('',#15960,#15962,#1612,.T.);
#20408=EDGE_CURVE('',#15963,#15964,#9650,.T.);
#20409=EDGE_CURVE('',#15961,#15963,#1613,.F.);
#20410=EDGE_CURVE('',#15962,#15964,#1614,.T.);
#20411=EDGE_CURVE('',#15965,#15966,#9651,.T.);
#20412=EDGE_CURVE('',#15963,#15965,#1615,.F.);
#20413=EDGE_CURVE('',#15964,#15966,#1616,.T.);
#20414=EDGE_CURVE('',#15967,#15968,#9652,.T.);
#20415=EDGE_CURVE('',#15965,#15967,#1617,.F.);
#20416=EDGE_CURVE('',#15966,#15968,#1618,.T.);
#20417=EDGE_CURVE('',#15969,#15970,#9653,.T.);
#20418=EDGE_CURVE('',#15967,#15969,#1619,.F.);
#20419=EDGE_CURVE('',#15968,#15970,#1620,.T.);
#20420=EDGE_CURVE('',#15971,#15972,#9654,.T.);
#20421=EDGE_CURVE('',#15969,#15971,#1621,.F.);
#20422=EDGE_CURVE('',#15970,#15972,#1622,.T.);
#20423=EDGE_CURVE('',#15973,#15974,#9655,.T.);
#20424=EDGE_CURVE('',#15971,#15973,#1623,.F.);
#20425=EDGE_CURVE('',#15972,#15974,#1624,.T.);
#20426=EDGE_CURVE('',#15975,#15976,#9656,.T.);
#20427=EDGE_CURVE('',#15977,#15975,#1625,.F.);
#20428=EDGE_CURVE('',#15973,#15977,#1626,.F.);
#20429=EDGE_CURVE('',#15974,#15976,#1627,.T.);
#20430=EDGE_CURVE('',#15978,#15979,#9657,.T.);
#20431=EDGE_CURVE('',#15975,#15978,#1628,.F.);
#20432=EDGE_CURVE('',#15976,#15979,#1629,.T.);
#20433=EDGE_CURVE('',#15980,#15981,#9658,.T.);
#20434=EDGE_CURVE('',#15978,#15980,#1630,.F.);
#20435=EDGE_CURVE('',#15979,#15981,#1631,.T.);
#20436=EDGE_CURVE('',#15982,#15983,#9659,.T.);
#20437=EDGE_CURVE('',#15980,#15982,#1632,.F.);
#20438=EDGE_CURVE('',#15981,#15984,#1633,.T.);
#20439=EDGE_CURVE('',#15984,#15983,#1634,.T.);
#20440=EDGE_CURVE('',#15985,#15986,#9660,.T.);
#20441=EDGE_CURVE('',#15982,#15985,#1635,.F.);
#20442=EDGE_CURVE('',#15983,#15986,#1636,.T.);
#20443=EDGE_CURVE('',#15986,#15987,#1637,.T.);
#20444=EDGE_CURVE('',#15988,#15987,#13121,.T.);
#20445=EDGE_CURVE('',#15989,#15988,#1638,.T.);
#20446=EDGE_CURVE('',#15985,#15989,#1639,.T.);
#20447=EDGE_CURVE('',#15942,#15990,#1640,.T.);
#20448=EDGE_CURVE('',#15991,#15990,#13122,.T.);
#20449=EDGE_CURVE('',#15991,#15941,#1641,.T.);
#20450=EDGE_CURVE('',#15992,#15993,#13123,.T.);
#20451=EDGE_CURVE('',#15992,#15988,#1642,.T.);
#20452=EDGE_CURVE('',#15987,#15991,#1643,.T.);
#20453=EDGE_CURVE('',#15993,#15991,#13124,.T.);
#20454=EDGE_CURVE('',#15990,#15992,#1644,.T.);
#20455=EDGE_CURVE('',#15994,#15902,#1645,.T.);
#20456=EDGE_CURVE('',#15994,#15945,#1646,.T.);
#20457=EDGE_CURVE('',#15995,#15996,#13125,.T.);
#20458=EDGE_CURVE('',#15995,#15946,#1647,.T.);
#20459=EDGE_CURVE('',#15996,#15902,#13126,.T.);
#20460=EDGE_CURVE('',#15901,#15995,#1648,.T.);
#20461=EDGE_CURVE('',#15997,#15997,#13127,.T.);
#20462=EDGE_CURVE('',#15997,#15996,#13128,.T.);
#20463=EDGE_CURVE('',#15998,#15998,#13129,.T.);
#20464=EDGE_CURVE('',#15993,#15999,#9661,.T.);
#20465=EDGE_CURVE('',#15999,#15999,#13130,.T.);
#20466=EDGE_CURVE('',#16000,#16001,#13131,.T.);
#20467=EDGE_CURVE('',#16002,#16000,#9662,.T.);
#20468=EDGE_CURVE('',#16001,#16002,#9663,.T.);
#20469=EDGE_CURVE('',#16001,#16003,#9664,.T.);
#20470=EDGE_CURVE('',#16004,#16002,#9665,.T.);
#20471=EDGE_CURVE('',#16003,#16004,#200,.T.);
#20472=EDGE_CURVE('',#16005,#16000,#9666,.T.);
#20473=EDGE_CURVE('',#16004,#16005,#201,.T.);
#20474=EDGE_CURVE('',#16006,#16007,#13132,.T.);
#20475=EDGE_CURVE('',#16007,#16008,#9667,.T.);
#20476=EDGE_CURVE('',#16009,#16008,#13133,.T.);
#20477=EDGE_CURVE('',#16008,#16009,#13134,.T.);
#20478=EDGE_CURVE('',#16007,#16010,#13135,.T.);
#20479=EDGE_CURVE('',#16010,#16011,#9668,.T.);
#20480=EDGE_CURVE('',#16012,#16011,#13136,.T.);
#20481=EDGE_CURVE('',#16012,#16013,#9669,.T.);
#20482=EDGE_CURVE('',#16013,#16014,#13137,.T.);
#20483=EDGE_CURVE('',#16014,#16015,#9670,.T.);
#20484=EDGE_CURVE('',#16016,#16015,#13138,.T.);
#20485=EDGE_CURVE('',#16016,#16017,#9671,.T.);
#20486=EDGE_CURVE('',#16017,#16018,#13139,.T.);
#20487=EDGE_CURVE('',#16018,#16019,#9672,.T.);
#20488=EDGE_CURVE('',#16020,#16019,#13140,.T.);
#20489=EDGE_CURVE('',#16020,#16021,#9673,.T.);
#20490=EDGE_CURVE('',#16021,#16022,#13141,.T.);
#20491=EDGE_CURVE('',#16022,#16023,#9674,.T.);
#20492=EDGE_CURVE('',#16024,#16023,#13142,.T.);
#20493=EDGE_CURVE('',#16024,#16025,#9675,.T.);
#20494=EDGE_CURVE('',#16025,#16026,#13143,.T.);
#20495=EDGE_CURVE('',#16026,#16027,#9676,.T.);
#20496=EDGE_CURVE('',#16028,#16027,#13144,.T.);
#20497=EDGE_CURVE('',#16028,#16029,#9677,.T.);
#20498=EDGE_CURVE('',#16029,#16030,#13145,.T.);
#20499=EDGE_CURVE('',#16030,#16031,#9678,.T.);
#20500=EDGE_CURVE('',#16032,#16031,#13146,.T.);
#20501=EDGE_CURVE('',#16032,#16033,#9679,.T.);
#20502=EDGE_CURVE('',#16033,#16034,#13147,.T.);
#20503=EDGE_CURVE('',#16034,#16035,#9680,.T.);
#20504=EDGE_CURVE('',#16036,#16035,#13148,.T.);
#20505=EDGE_CURVE('',#16036,#16037,#9681,.T.);
#20506=EDGE_CURVE('',#16037,#16038,#13149,.T.);
#20507=EDGE_CURVE('',#16038,#16039,#9682,.T.);
#20508=EDGE_CURVE('',#16040,#16039,#13150,.T.);
#20509=EDGE_CURVE('',#16040,#16041,#9683,.T.);
#20510=EDGE_CURVE('',#16041,#16042,#13151,.T.);
#20511=EDGE_CURVE('',#16042,#16043,#9684,.T.);
#20512=EDGE_CURVE('',#16044,#16043,#13152,.T.);
#20513=EDGE_CURVE('',#16044,#16045,#9685,.T.);
#20514=EDGE_CURVE('',#16045,#16046,#13153,.T.);
#20515=EDGE_CURVE('',#16046,#16047,#9686,.T.);
#20516=EDGE_CURVE('',#16048,#16047,#13154,.T.);
#20517=EDGE_CURVE('',#16048,#16049,#9687,.T.);
#20518=EDGE_CURVE('',#16049,#16050,#13155,.T.);
#20519=EDGE_CURVE('',#16050,#16051,#9688,.T.);
#20520=EDGE_CURVE('',#16052,#16051,#13156,.T.);
#20521=EDGE_CURVE('',#16052,#16053,#9689,.T.);
#20522=EDGE_CURVE('',#16053,#16054,#13157,.T.);
#20523=EDGE_CURVE('',#16054,#16055,#9690,.T.);
#20524=EDGE_CURVE('',#16056,#16055,#13158,.T.);
#20525=EDGE_CURVE('',#16056,#16057,#9691,.T.);
#20526=EDGE_CURVE('',#16057,#16058,#13159,.T.);
#20527=EDGE_CURVE('',#16058,#16059,#9692,.T.);
#20528=EDGE_CURVE('',#16060,#16059,#13160,.T.);
#20529=EDGE_CURVE('',#16060,#16061,#9693,.T.);
#20530=EDGE_CURVE('',#16061,#16062,#13161,.T.);
#20531=EDGE_CURVE('',#16062,#16063,#9694,.T.);
#20532=EDGE_CURVE('',#16064,#16063,#13162,.T.);
#20533=EDGE_CURVE('',#16064,#16065,#9695,.T.);
#20534=EDGE_CURVE('',#16065,#16066,#13163,.T.);
#20535=EDGE_CURVE('',#16066,#16067,#9696,.T.);
#20536=EDGE_CURVE('',#16068,#16067,#13164,.T.);
#20537=EDGE_CURVE('',#16068,#16069,#9697,.T.);
#20538=EDGE_CURVE('',#16069,#16070,#13165,.T.);
#20539=EDGE_CURVE('',#16070,#16071,#9698,.T.);
#20540=EDGE_CURVE('',#16072,#16071,#13166,.T.);
#20541=EDGE_CURVE('',#16072,#16073,#9699,.T.);
#20542=EDGE_CURVE('',#16073,#16074,#13167,.T.);
#20543=EDGE_CURVE('',#16074,#16075,#9700,.T.);
#20544=EDGE_CURVE('',#16005,#16075,#13168,.T.);
#20545=EDGE_CURVE('',#16076,#16003,#13169,.T.);
#20546=EDGE_CURVE('',#16076,#16077,#9701,.T.);
#20547=EDGE_CURVE('',#16077,#16078,#13170,.T.);
#20548=EDGE_CURVE('',#16078,#16079,#9702,.T.);
#20549=EDGE_CURVE('',#16080,#16079,#13171,.T.);
#20550=EDGE_CURVE('',#16080,#16081,#9703,.T.);
#20551=EDGE_CURVE('',#16081,#16082,#13172,.T.);
#20552=EDGE_CURVE('',#16082,#16083,#9704,.T.);
#20553=EDGE_CURVE('',#16084,#16083,#13173,.T.);
#20554=EDGE_CURVE('',#16084,#16085,#9705,.T.);
#20555=EDGE_CURVE('',#16085,#16086,#13174,.T.);
#20556=EDGE_CURVE('',#16086,#16087,#9706,.T.);
#20557=EDGE_CURVE('',#16088,#16087,#13175,.T.);
#20558=EDGE_CURVE('',#16088,#16089,#9707,.T.);
#20559=EDGE_CURVE('',#16089,#16090,#13176,.T.);
#20560=EDGE_CURVE('',#16090,#16091,#9708,.T.);
#20561=EDGE_CURVE('',#16092,#16091,#13177,.T.);
#20562=EDGE_CURVE('',#16092,#16093,#9709,.T.);
#20563=EDGE_CURVE('',#16093,#16094,#13178,.T.);
#20564=EDGE_CURVE('',#16094,#16095,#9710,.T.);
#20565=EDGE_CURVE('',#16096,#16095,#13179,.T.);
#20566=EDGE_CURVE('',#16096,#16097,#9711,.T.);
#20567=EDGE_CURVE('',#16097,#16098,#13180,.T.);
#20568=EDGE_CURVE('',#16098,#16099,#9712,.T.);
#20569=EDGE_CURVE('',#16100,#16099,#13181,.T.);
#20570=EDGE_CURVE('',#16100,#16101,#9713,.T.);
#20571=EDGE_CURVE('',#16101,#16102,#13182,.T.);
#20572=EDGE_CURVE('',#16102,#16103,#9714,.T.);
#20573=EDGE_CURVE('',#16104,#16103,#13183,.T.);
#20574=EDGE_CURVE('',#16104,#16105,#9715,.T.);
#20575=EDGE_CURVE('',#16105,#16106,#13184,.T.);
#20576=EDGE_CURVE('',#16106,#16107,#9716,.T.);
#20577=EDGE_CURVE('',#16108,#16107,#13185,.T.);
#20578=EDGE_CURVE('',#16108,#16109,#9717,.T.);
#20579=EDGE_CURVE('',#16109,#16110,#13186,.T.);
#20580=EDGE_CURVE('',#16110,#16111,#9718,.T.);
#20581=EDGE_CURVE('',#16112,#16111,#13187,.T.);
#20582=EDGE_CURVE('',#16112,#16113,#9719,.T.);
#20583=EDGE_CURVE('',#16113,#16114,#13188,.T.);
#20584=EDGE_CURVE('',#16114,#16115,#9720,.T.);
#20585=EDGE_CURVE('',#16116,#16115,#13189,.T.);
#20586=EDGE_CURVE('',#16116,#16117,#9721,.T.);
#20587=EDGE_CURVE('',#16117,#16118,#13190,.T.);
#20588=EDGE_CURVE('',#16118,#16119,#9722,.T.);
#20589=EDGE_CURVE('',#16120,#16119,#13191,.T.);
#20590=EDGE_CURVE('',#16120,#16121,#9723,.T.);
#20591=EDGE_CURVE('',#16121,#16122,#13192,.T.);
#20592=EDGE_CURVE('',#16122,#16123,#9724,.T.);
#20593=EDGE_CURVE('',#16124,#16123,#13193,.T.);
#20594=EDGE_CURVE('',#16124,#16125,#9725,.T.);
#20595=EDGE_CURVE('',#16125,#16126,#13194,.T.);
#20596=EDGE_CURVE('',#16126,#16127,#9726,.T.);
#20597=EDGE_CURVE('',#16128,#16127,#13195,.T.);
#20598=EDGE_CURVE('',#16128,#16129,#9727,.T.);
#20599=EDGE_CURVE('',#16129,#16130,#13196,.T.);
#20600=EDGE_CURVE('',#16130,#16131,#9728,.T.);
#20601=EDGE_CURVE('',#16132,#16131,#13197,.T.);
#20602=EDGE_CURVE('',#16132,#16133,#9729,.T.);
#20603=EDGE_CURVE('',#16133,#16134,#13198,.T.);
#20604=EDGE_CURVE('',#16134,#16135,#9730,.T.);
#20605=EDGE_CURVE('',#16136,#16135,#13199,.T.);
#20606=EDGE_CURVE('',#16136,#16137,#9731,.T.);
#20607=EDGE_CURVE('',#16137,#16138,#13200,.T.);
#20608=EDGE_CURVE('',#16138,#16139,#9732,.T.);
#20609=EDGE_CURVE('',#16140,#16139,#13201,.T.);
#20610=EDGE_CURVE('',#16140,#16141,#9733,.T.);
#20611=EDGE_CURVE('',#16141,#16142,#13202,.T.);
#20612=EDGE_CURVE('',#16142,#16143,#9734,.T.);
#20613=EDGE_CURVE('',#16144,#16143,#13203,.T.);
#20614=EDGE_CURVE('',#16144,#16145,#9735,.T.);
#20615=EDGE_CURVE('',#16145,#16146,#13204,.T.);
#20616=EDGE_CURVE('',#16146,#16147,#9736,.T.);
#20617=EDGE_CURVE('',#16148,#16147,#13205,.T.);
#20618=EDGE_CURVE('',#16148,#16006,#9737,.T.);
#20619=EDGE_CURVE('',#16074,#16149,#9738,.T.);
#20620=EDGE_CURVE('',#16150,#16149,#9739,.T.);
#20621=EDGE_CURVE('',#16075,#16150,#202,.T.);
#20622=EDGE_CURVE('',#16150,#16072,#203,.T.);
#20623=EDGE_CURVE('',#16149,#16073,#9740,.T.);
#20624=EDGE_CURVE('',#16151,#16148,#204,.T.);
#20625=EDGE_CURVE('',#16147,#16152,#205,.T.);
#20626=EDGE_CURVE('',#16152,#16144,#206,.T.);
#20627=EDGE_CURVE('',#16143,#16153,#207,.T.);
#20628=EDGE_CURVE('',#16153,#16140,#208,.T.);
#20629=EDGE_CURVE('',#16139,#16154,#209,.T.);
#20630=EDGE_CURVE('',#16154,#16136,#210,.T.);
#20631=EDGE_CURVE('',#16135,#16155,#211,.T.);
#20632=EDGE_CURVE('',#16155,#16132,#212,.T.);
#20633=EDGE_CURVE('',#16131,#16156,#213,.T.);
#20634=EDGE_CURVE('',#16156,#16128,#214,.T.);
#20635=EDGE_CURVE('',#16127,#16157,#215,.T.);
#20636=EDGE_CURVE('',#16157,#16124,#216,.T.);
#20637=EDGE_CURVE('',#16123,#16158,#217,.T.);
#20638=EDGE_CURVE('',#16158,#16120,#218,.T.);
#20639=EDGE_CURVE('',#16119,#16159,#219,.T.);
#20640=EDGE_CURVE('',#16159,#16116,#220,.T.);
#20641=EDGE_CURVE('',#16115,#16160,#221,.T.);
#20642=EDGE_CURVE('',#16160,#16112,#222,.T.);
#20643=EDGE_CURVE('',#16111,#16161,#223,.T.);
#20644=EDGE_CURVE('',#16161,#16108,#224,.T.);
#20645=EDGE_CURVE('',#16107,#16162,#225,.T.);
#20646=EDGE_CURVE('',#16162,#16104,#226,.T.);
#20647=EDGE_CURVE('',#16103,#16163,#227,.T.);
#20648=EDGE_CURVE('',#16163,#16100,#228,.T.);
#20649=EDGE_CURVE('',#16099,#16164,#229,.T.);
#20650=EDGE_CURVE('',#16164,#16096,#230,.T.);
#20651=EDGE_CURVE('',#16095,#16165,#231,.T.);
#20652=EDGE_CURVE('',#16165,#16092,#232,.T.);
#20653=EDGE_CURVE('',#16091,#16166,#233,.T.);
#20654=EDGE_CURVE('',#16166,#16088,#234,.T.);
#20655=EDGE_CURVE('',#16087,#16167,#235,.T.);
#20656=EDGE_CURVE('',#16167,#16084,#236,.T.);
#20657=EDGE_CURVE('',#16083,#16168,#237,.T.);
#20658=EDGE_CURVE('',#16168,#16080,#238,.T.);
#20659=EDGE_CURVE('',#16079,#16169,#239,.T.);
#20660=EDGE_CURVE('',#16169,#16076,#240,.T.);
#20661=EDGE_CURVE('',#16071,#16170,#241,.T.);
#20662=EDGE_CURVE('',#16170,#16068,#242,.T.);
#20663=EDGE_CURVE('',#16067,#16171,#243,.T.);
#20664=EDGE_CURVE('',#16171,#16064,#244,.T.);
#20665=EDGE_CURVE('',#16063,#16172,#245,.T.);
#20666=EDGE_CURVE('',#16172,#16060,#246,.T.);
#20667=EDGE_CURVE('',#16059,#16173,#247,.T.);
#20668=EDGE_CURVE('',#16173,#16056,#248,.T.);
#20669=EDGE_CURVE('',#16055,#16174,#249,.T.);
#20670=EDGE_CURVE('',#16174,#16052,#250,.T.);
#20671=EDGE_CURVE('',#16051,#16175,#251,.T.);
#20672=EDGE_CURVE('',#16175,#16048,#252,.T.);
#20673=EDGE_CURVE('',#16047,#16176,#253,.T.);
#20674=EDGE_CURVE('',#16176,#16044,#254,.T.);
#20675=EDGE_CURVE('',#16043,#16177,#255,.T.);
#20676=EDGE_CURVE('',#16177,#16040,#256,.T.);
#20677=EDGE_CURVE('',#16039,#16178,#257,.T.);
#20678=EDGE_CURVE('',#16178,#16036,#258,.T.);
#20679=EDGE_CURVE('',#16035,#16179,#259,.T.);
#20680=EDGE_CURVE('',#16179,#16032,#260,.T.);
#20681=EDGE_CURVE('',#16031,#16180,#261,.T.);
#20682=EDGE_CURVE('',#16180,#16028,#262,.T.);
#20683=EDGE_CURVE('',#16027,#16181,#263,.T.);
#20684=EDGE_CURVE('',#16181,#16024,#264,.T.);
#20685=EDGE_CURVE('',#16023,#16182,#265,.T.);
#20686=EDGE_CURVE('',#16182,#16020,#266,.T.);
#20687=EDGE_CURVE('',#16019,#16183,#267,.T.);
#20688=EDGE_CURVE('',#16183,#16016,#268,.T.);
#20689=EDGE_CURVE('',#16015,#16184,#269,.T.);
#20690=EDGE_CURVE('',#16184,#16012,#270,.T.);
#20691=EDGE_CURVE('',#16011,#16151,#271,.T.);
#20692=EDGE_CURVE('',#16151,#16185,#9741,.T.);
#20693=EDGE_CURVE('',#16185,#16185,#13206,.T.);
#20694=EDGE_CURVE('',#16186,#16069,#9742,.T.);
#20695=EDGE_CURVE('',#16070,#16186,#9743,.T.);
#20696=EDGE_CURVE('',#16170,#16186,#9744,.T.);
#20697=EDGE_CURVE('',#16066,#16187,#9745,.T.);
#20698=EDGE_CURVE('',#16171,#16187,#9746,.T.);
#20699=EDGE_CURVE('',#16187,#16065,#9747,.T.);
#20700=EDGE_CURVE('',#16188,#16061,#9748,.T.);
#20701=EDGE_CURVE('',#16062,#16188,#9749,.T.);
#20702=EDGE_CURVE('',#16172,#16188,#9750,.T.);
#20703=EDGE_CURVE('',#16058,#16189,#9751,.T.);
#20704=EDGE_CURVE('',#16173,#16189,#9752,.T.);
#20705=EDGE_CURVE('',#16189,#16057,#9753,.T.);
#20706=EDGE_CURVE('',#16190,#16053,#9754,.T.);
#20707=EDGE_CURVE('',#16054,#16190,#9755,.T.);
#20708=EDGE_CURVE('',#16174,#16190,#9756,.T.);
#20709=EDGE_CURVE('',#16050,#16191,#9757,.T.);
#20710=EDGE_CURVE('',#16175,#16191,#9758,.T.);
#20711=EDGE_CURVE('',#16191,#16049,#9759,.T.);
#20712=EDGE_CURVE('',#16192,#16045,#9760,.T.);
#20713=EDGE_CURVE('',#16046,#16192,#9761,.T.);
#20714=EDGE_CURVE('',#16176,#16192,#9762,.T.);
#20715=EDGE_CURVE('',#16042,#16193,#9763,.T.);
#20716=EDGE_CURVE('',#16177,#16193,#9764,.T.);
#20717=EDGE_CURVE('',#16193,#16041,#9765,.T.);
#20718=EDGE_CURVE('',#16194,#16037,#9766,.T.);
#20719=EDGE_CURVE('',#16038,#16194,#9767,.T.);
#20720=EDGE_CURVE('',#16178,#16194,#9768,.T.);
#20721=EDGE_CURVE('',#16034,#16195,#9769,.T.);
#20722=EDGE_CURVE('',#16179,#16195,#9770,.T.);
#20723=EDGE_CURVE('',#16195,#16033,#9771,.T.);
#20724=EDGE_CURVE('',#16196,#16029,#9772,.T.);
#20725=EDGE_CURVE('',#16030,#16196,#9773,.T.);
#20726=EDGE_CURVE('',#16180,#16196,#9774,.T.);
#20727=EDGE_CURVE('',#16026,#16197,#9775,.T.);
#20728=EDGE_CURVE('',#16181,#16197,#9776,.T.);
#20729=EDGE_CURVE('',#16197,#16025,#9777,.T.);
#20730=EDGE_CURVE('',#16198,#16021,#9778,.T.);
#20731=EDGE_CURVE('',#16022,#16198,#9779,.T.);
#20732=EDGE_CURVE('',#16182,#16198,#9780,.T.);
#20733=EDGE_CURVE('',#16018,#16199,#9781,.T.);
#20734=EDGE_CURVE('',#16183,#16199,#9782,.T.);
#20735=EDGE_CURVE('',#16199,#16017,#9783,.T.);
#20736=EDGE_CURVE('',#16200,#16013,#9784,.T.);
#20737=EDGE_CURVE('',#16014,#16200,#9785,.T.);
#20738=EDGE_CURVE('',#16184,#16200,#9786,.T.);
#20739=EDGE_CURVE('',#16010,#16201,#9787,.T.);
#20740=EDGE_CURVE('',#16151,#16201,#9788,.T.);
#20741=EDGE_CURVE('',#16201,#16006,#9789,.T.);
#20742=EDGE_CURVE('',#16202,#16145,#9790,.T.);
#20743=EDGE_CURVE('',#16146,#16202,#9791,.T.);
#20744=EDGE_CURVE('',#16152,#16202,#9792,.T.);
#20745=EDGE_CURVE('',#16142,#16203,#9793,.T.);
#20746=EDGE_CURVE('',#16153,#16203,#9794,.T.);
#20747=EDGE_CURVE('',#16203,#16141,#9795,.T.);
#20748=EDGE_CURVE('',#16204,#16137,#9796,.T.);
#20749=EDGE_CURVE('',#16138,#16204,#9797,.T.);
#20750=EDGE_CURVE('',#16154,#16204,#9798,.T.);
#20751=EDGE_CURVE('',#16134,#16205,#9799,.T.);
#20752=EDGE_CURVE('',#16155,#16205,#9800,.T.);
#20753=EDGE_CURVE('',#16205,#16133,#9801,.T.);
#20754=EDGE_CURVE('',#16206,#16129,#9802,.T.);
#20755=EDGE_CURVE('',#16130,#16206,#9803,.T.);
#20756=EDGE_CURVE('',#16156,#16206,#9804,.T.);
#20757=EDGE_CURVE('',#16126,#16207,#9805,.T.);
#20758=EDGE_CURVE('',#16157,#16207,#9806,.T.);
#20759=EDGE_CURVE('',#16207,#16125,#9807,.T.);
#20760=EDGE_CURVE('',#16208,#16121,#9808,.T.);
#20761=EDGE_CURVE('',#16122,#16208,#9809,.T.);
#20762=EDGE_CURVE('',#16158,#16208,#9810,.T.);
#20763=EDGE_CURVE('',#16118,#16209,#9811,.T.);
#20764=EDGE_CURVE('',#16159,#16209,#9812,.T.);
#20765=EDGE_CURVE('',#16209,#16117,#9813,.T.);
#20766=EDGE_CURVE('',#16210,#16113,#9814,.T.);
#20767=EDGE_CURVE('',#16114,#16210,#9815,.T.);
#20768=EDGE_CURVE('',#16160,#16210,#9816,.T.);
#20769=EDGE_CURVE('',#16110,#16211,#9817,.T.);
#20770=EDGE_CURVE('',#16161,#16211,#9818,.T.);
#20771=EDGE_CURVE('',#16211,#16109,#9819,.T.);
#20772=EDGE_CURVE('',#16212,#16105,#9820,.T.);
#20773=EDGE_CURVE('',#16106,#16212,#9821,.T.);
#20774=EDGE_CURVE('',#16162,#16212,#9822,.T.);
#20775=EDGE_CURVE('',#16102,#16213,#9823,.T.);
#20776=EDGE_CURVE('',#16163,#16213,#9824,.T.);
#20777=EDGE_CURVE('',#16213,#16101,#9825,.T.);
#20778=EDGE_CURVE('',#16214,#16097,#9826,.T.);
#20779=EDGE_CURVE('',#16098,#16214,#9827,.T.);
#20780=EDGE_CURVE('',#16164,#16214,#9828,.T.);
#20781=EDGE_CURVE('',#16094,#16215,#9829,.T.);
#20782=EDGE_CURVE('',#16165,#16215,#9830,.T.);
#20783=EDGE_CURVE('',#16215,#16093,#9831,.T.);
#20784=EDGE_CURVE('',#16216,#16089,#9832,.T.);
#20785=EDGE_CURVE('',#16090,#16216,#9833,.T.);
#20786=EDGE_CURVE('',#16166,#16216,#9834,.T.);
#20787=EDGE_CURVE('',#16086,#16217,#9835,.T.);
#20788=EDGE_CURVE('',#16167,#16217,#9836,.T.);
#20789=EDGE_CURVE('',#16217,#16085,#9837,.T.);
#20790=EDGE_CURVE('',#16218,#16081,#9838,.T.);
#20791=EDGE_CURVE('',#16082,#16218,#9839,.T.);
#20792=EDGE_CURVE('',#16168,#16218,#9840,.T.);
#20793=EDGE_CURVE('',#16078,#16219,#9841,.T.);
#20794=EDGE_CURVE('',#16169,#16219,#9842,.T.);
#20795=EDGE_CURVE('',#16219,#16077,#9843,.T.);
#20796=EDGE_CURVE('',#15998,#16009,#13207,.T.);
#20797=EDGE_CURVE('',#16220,#16220,#13208,.T.);
#20798=EDGE_CURVE('',#16221,#16222,#272,.T.);
#20799=EDGE_CURVE('',#16223,#16221,#13209,.T.);
#20800=EDGE_CURVE('',#16224,#16223,#273,.T.);
#20801=EDGE_CURVE('',#16225,#16224,#274,.T.);
#20802=EDGE_CURVE('',#16226,#16225,#13210,.T.);
#20803=EDGE_CURVE('',#16227,#16226,#275,.T.);
#20804=EDGE_CURVE('',#16228,#16227,#276,.T.);
#20805=EDGE_CURVE('',#16229,#16228,#13211,.T.);
#20806=EDGE_CURVE('',#16230,#16229,#277,.T.);
#20807=EDGE_CURVE('',#16231,#16230,#278,.T.);
#20808=EDGE_CURVE('',#16232,#16231,#13212,.T.);
#20809=EDGE_CURVE('',#16233,#16232,#279,.T.);
#20810=EDGE_CURVE('',#16234,#16233,#280,.T.);
#20811=EDGE_CURVE('',#16235,#16234,#13213,.T.);
#20812=EDGE_CURVE('',#16236,#16235,#281,.T.);
#20813=EDGE_CURVE('',#16237,#16236,#282,.T.);
#20814=EDGE_CURVE('',#16238,#16237,#13214,.T.);
#20815=EDGE_CURVE('',#16222,#16238,#283,.T.);
#20816=EDGE_CURVE('',#16222,#16220,#9844,.T.);
#20817=EDGE_CURVE('',#16238,#16239,#9845,.T.);
#20818=EDGE_CURVE('',#16240,#16237,#9846,.T.);
#20819=EDGE_CURVE('',#16239,#16240,#13215,.T.);
#20820=EDGE_CURVE('',#16241,#16234,#9847,.T.);
#20821=EDGE_CURVE('',#16242,#16241,#13216,.T.);
#20822=EDGE_CURVE('',#16235,#16242,#9848,.T.);
#20823=EDGE_CURVE('',#16223,#16243,#9849,.T.);
#20824=EDGE_CURVE('',#16244,#16221,#9850,.T.);
#20825=EDGE_CURVE('',#16243,#16244,#13217,.T.);
#20826=EDGE_CURVE('',#16245,#16231,#9851,.T.);
#20827=EDGE_CURVE('',#16246,#16245,#13218,.T.);
#20828=EDGE_CURVE('',#16232,#16246,#9852,.T.);
#20829=EDGE_CURVE('',#16226,#16247,#9853,.T.);
#20830=EDGE_CURVE('',#16248,#16225,#9854,.T.);
#20831=EDGE_CURVE('',#16247,#16248,#13219,.T.);
#20832=EDGE_CURVE('',#16249,#16228,#9855,.T.);
#20833=EDGE_CURVE('',#16250,#16249,#13220,.T.);
#20834=EDGE_CURVE('',#16229,#16250,#9856,.T.);
#20835=EDGE_CURVE('',#16248,#16247,#9857,.T.);
#20836=EDGE_CURVE('',#16224,#16251,#9858,.T.);
#20837=EDGE_CURVE('',#16251,#16252,#9859,.T.);
#20838=EDGE_CURVE('',#16227,#16252,#9860,.T.);
#20839=EDGE_CURVE('',#16244,#16243,#9861,.T.);
#20840=EDGE_CURVE('',#16222,#16253,#9862,.T.);
#20841=EDGE_CURVE('',#16253,#16251,#9863,.T.);
#20842=EDGE_CURVE('',#16240,#16239,#9864,.T.);
#20843=EDGE_CURVE('',#16236,#16254,#9865,.T.);
#20844=EDGE_CURVE('',#16254,#16253,#9866,.T.);
#20845=EDGE_CURVE('',#16241,#16242,#9867,.T.);
#20846=EDGE_CURVE('',#16245,#16246,#9868,.T.);
#20847=EDGE_CURVE('',#16249,#16250,#9869,.T.);
#20848=EDGE_CURVE('',#16255,#16256,#9870,.T.);
#20849=EDGE_CURVE('',#16256,#16255,#13221,.T.);
#20850=EDGE_CURVE('',#16256,#16254,#9871,.T.);
#20851=EDGE_CURVE('',#16254,#16256,#13222,.T.);
#20852=EDGE_CURVE('',#16253,#16254,#13223,.T.);
#20853=EDGE_CURVE('',#16251,#16253,#13224,.T.);
#20854=EDGE_CURVE('',#16252,#16251,#13225,.T.);
#20855=EDGE_CURVE('',#16252,#16255,#9872,.T.);
#20856=EDGE_CURVE('',#16255,#16252,#13226,.T.);
#20857=EDGE_CURVE('',#16257,#16253,#9873,.T.);
#20858=EDGE_CURVE('',#16230,#16255,#9874,.T.);
#20859=EDGE_CURVE('',#16233,#16256,#9875,.T.);
#20860=EDGE_CURVE('',#16258,#16259,#9876,.T.);
#20861=EDGE_CURVE('',#16258,#16260,#1649,.T.);
#20862=EDGE_CURVE('',#16260,#16261,#13227,.T.);
#20863=EDGE_CURVE('',#16261,#16259,#1650,.T.);
#20864=EDGE_CURVE('',#16262,#16263,#9877,.T.);
#20865=EDGE_CURVE('',#16262,#16258,#1651,.T.);
#20866=EDGE_CURVE('',#16259,#16263,#1652,.T.);
#20867=EDGE_CURVE('',#16264,#16265,#9878,.T.);
#20868=EDGE_CURVE('',#16264,#16262,#1653,.T.);
#20869=EDGE_CURVE('',#16263,#16265,#1654,.T.);
#20870=EDGE_CURVE('',#16266,#16267,#9879,.T.);
#20871=EDGE_CURVE('',#16266,#16264,#1655,.T.);
#20872=EDGE_CURVE('',#16265,#16267,#1656,.T.);
#20873=EDGE_CURVE('',#16268,#16269,#9880,.T.);
#20874=EDGE_CURVE('',#16268,#16266,#1657,.T.);
#20875=EDGE_CURVE('',#16267,#16269,#1658,.T.);
#20876=EDGE_CURVE('',#16270,#16271,#9881,.T.);
#20877=EDGE_CURVE('',#16270,#16268,#1659,.T.);
#20878=EDGE_CURVE('',#16269,#16271,#1660,.T.);
#20879=EDGE_CURVE('',#16272,#16273,#9882,.T.);
#20880=EDGE_CURVE('',#16272,#16270,#1661,.T.);
#20881=EDGE_CURVE('',#16271,#16273,#1662,.T.);
#20882=EDGE_CURVE('',#16274,#16275,#9883,.T.);
#20883=EDGE_CURVE('',#16274,#16272,#1663,.T.);
#20884=EDGE_CURVE('',#16273,#16275,#1664,.T.);
#20885=EDGE_CURVE('',#16276,#16277,#9884,.T.);
#20886=EDGE_CURVE('',#16276,#16274,#1665,.T.);
#20887=EDGE_CURVE('',#16275,#16277,#1666,.T.);
#20888=EDGE_CURVE('',#16278,#16279,#9885,.T.);
#20889=EDGE_CURVE('',#16278,#16276,#1667,.T.);
#20890=EDGE_CURVE('',#16277,#16279,#1668,.T.);
#20891=EDGE_CURVE('',#16280,#16281,#9886,.T.);
#20892=EDGE_CURVE('',#16280,#16278,#1669,.T.);
#20893=EDGE_CURVE('',#16279,#16281,#1670,.T.);
#20894=EDGE_CURVE('',#16282,#16283,#9887,.T.);
#20895=EDGE_CURVE('',#16284,#16282,#1671,.F.);
#20896=EDGE_CURVE('',#16285,#16284,#13228,.T.);
#20897=EDGE_CURVE('',#16285,#16283,#1672,.T.);
#20898=EDGE_CURVE('',#16286,#16287,#9888,.T.);
#20899=EDGE_CURVE('',#16282,#16286,#1673,.F.);
#20900=EDGE_CURVE('',#16283,#16288,#1674,.T.);
#20901=EDGE_CURVE('',#16288,#16287,#1675,.T.);
#20902=EDGE_CURVE('',#16289,#16290,#9889,.T.);
#20903=EDGE_CURVE('',#16286,#16289,#1676,.F.);
#20904=EDGE_CURVE('',#16287,#16291,#1677,.T.);
#20905=EDGE_CURVE('',#16291,#16290,#1678,.T.);
#20906=EDGE_CURVE('',#16292,#16293,#9890,.T.);
#20907=EDGE_CURVE('',#16289,#16292,#1679,.F.);
#20908=EDGE_CURVE('',#16290,#16294,#1680,.T.);
#20909=EDGE_CURVE('',#16294,#16293,#1681,.T.);
#20910=EDGE_CURVE('',#16295,#16296,#9891,.T.);
#20911=EDGE_CURVE('',#16292,#16295,#1682,.F.);
#20912=EDGE_CURVE('',#16293,#16297,#1683,.T.);
#20913=EDGE_CURVE('',#16297,#16296,#1684,.T.);
#20914=EDGE_CURVE('',#16298,#16299,#9892,.T.);
#20915=EDGE_CURVE('',#16295,#16298,#1685,.F.);
#20916=EDGE_CURVE('',#16296,#16300,#1686,.T.);
#20917=EDGE_CURVE('',#16300,#16299,#1687,.T.);
#20918=EDGE_CURVE('',#16301,#16302,#9893,.T.);
#20919=EDGE_CURVE('',#16298,#16301,#1688,.F.);
#20920=EDGE_CURVE('',#16299,#16303,#1689,.T.);
#20921=EDGE_CURVE('',#16303,#16302,#1690,.T.);
#20922=EDGE_CURVE('',#16304,#16305,#9894,.T.);
#20923=EDGE_CURVE('',#16301,#16304,#1691,.F.);
#20924=EDGE_CURVE('',#16302,#16306,#1692,.T.);
#20925=EDGE_CURVE('',#16306,#16305,#1693,.T.);
#20926=EDGE_CURVE('',#16307,#16308,#9895,.T.);
#20927=EDGE_CURVE('',#16304,#16307,#1694,.F.);
#20928=EDGE_CURVE('',#16305,#16309,#1695,.T.);
#20929=EDGE_CURVE('',#16309,#16308,#1696,.T.);
#20930=EDGE_CURVE('',#16310,#16311,#9896,.T.);
#20931=EDGE_CURVE('',#16307,#16310,#1697,.F.);
#20932=EDGE_CURVE('',#16308,#16312,#1698,.T.);
#20933=EDGE_CURVE('',#16312,#16311,#1699,.T.);
#20934=EDGE_CURVE('',#16311,#16313,#1700,.T.);
#20935=EDGE_CURVE('',#16313,#16314,#1701,.T.);
#20936=EDGE_CURVE('',#16315,#16314,#13229,.T.);
#20937=EDGE_CURVE('',#16316,#16315,#1702,.T.);
#20938=EDGE_CURVE('',#16310,#16316,#1703,.F.);
#20939=EDGE_CURVE('',#16281,#16317,#1704,.T.);
#20940=EDGE_CURVE('',#16318,#16317,#13230,.T.);
#20941=EDGE_CURVE('',#16318,#16280,#1705,.T.);
#20942=EDGE_CURVE('',#16284,#16319,#1706,.F.);
#20943=EDGE_CURVE('',#16320,#16315,#1707,.T.);
#20944=EDGE_CURVE('',#16317,#16320,#1708,.T.);
#20945=EDGE_CURVE('',#16319,#16261,#1709,.F.);
#20946=EDGE_CURVE('',#16320,#16321,#13231,.T.);
#20947=EDGE_CURVE('',#16314,#16322,#1710,.T.);
#20948=EDGE_CURVE('',#16322,#16318,#1711,.T.);
#20949=EDGE_CURVE('',#16321,#16318,#13232,.T.);
#20950=EDGE_CURVE('',#16260,#16285,#1712,.T.);
#20951=EDGE_CURVE('',#16323,#16323,#13233,.T.);
#20952=EDGE_CURVE('',#16323,#16321,#13234,.T.);
#20953=EDGE_CURVE('',#16324,#16324,#13235,.T.);
#20954=EDGE_CURVE('',#16325,#16326,#13236,.T.);
#20955=EDGE_CURVE('',#16327,#16325,#9897,.T.);
#20956=EDGE_CURVE('',#16328,#16327,#13237,.T.);
#20957=EDGE_CURVE('',#16329,#16328,#9898,.T.);
#20958=EDGE_CURVE('',#16326,#16329,#13238,.T.);
#20959=EDGE_CURVE('',#16329,#16330,#9899,.T.);
#20960=EDGE_CURVE('',#16331,#16328,#9900,.T.);
#20961=EDGE_CURVE('',#16332,#16331,#284,.T.);
#20962=EDGE_CURVE('',#16333,#16332,#9901,.T.);
#20963=EDGE_CURVE('',#16330,#16333,#285,.T.);
#20964=EDGE_CURVE('',#16334,#16325,#9902,.T.);
#20965=EDGE_CURVE('',#16335,#16334,#286,.T.);
#20966=EDGE_CURVE('',#16336,#16335,#9903,.T.);
#20967=EDGE_CURVE('',#16337,#16336,#287,.T.);
#20968=EDGE_CURVE('',#16327,#16337,#9904,.T.);
#20969=EDGE_CURVE('',#16326,#16324,#9905,.T.);
#20970=EDGE_CURVE('',#16331,#16330,#13239,.T.);
#20971=EDGE_CURVE('',#16334,#16337,#13240,.T.);
#20972=EDGE_CURVE('',#16332,#16333,#13241,.T.);
#20973=EDGE_CURVE('',#16335,#16336,#13242,.T.);
#20974=EDGE_CURVE('',#16338,#16338,#13243,.T.);
#20975=EDGE_CURVE('',#16338,#16319,#9906,.T.);
#20976=ORIENTED_EDGE('',*,*,#16339,.T.);
#20977=ORIENTED_EDGE('',*,*,#16340,.T.);
#20978=ORIENTED_EDGE('',*,*,#16341,.T.);
#20979=ORIENTED_EDGE('',*,*,#16340,.F.);
#20980=ORIENTED_EDGE('',*,*,#16342,.F.);
#20981=ORIENTED_EDGE('',*,*,#16343,.T.);
#20982=ORIENTED_EDGE('',*,*,#16344,.T.);
#20983=ORIENTED_EDGE('',*,*,#16345,.T.);
#20984=ORIENTED_EDGE('',*,*,#16346,.T.);
#20985=ORIENTED_EDGE('',*,*,#16347,.T.);
#20986=ORIENTED_EDGE('',*,*,#16348,.F.);
#20987=ORIENTED_EDGE('',*,*,#16349,.T.);
#20988=ORIENTED_EDGE('',*,*,#16350,.F.);
#20989=ORIENTED_EDGE('',*,*,#16351,.T.);
#20990=ORIENTED_EDGE('',*,*,#16352,.F.);
#20991=ORIENTED_EDGE('',*,*,#16353,.T.);
#20992=ORIENTED_EDGE('',*,*,#16354,.F.);
#20993=ORIENTED_EDGE('',*,*,#16355,.T.);
#20994=ORIENTED_EDGE('',*,*,#16356,.F.);
#20995=ORIENTED_EDGE('',*,*,#16357,.T.);
#20996=ORIENTED_EDGE('',*,*,#16358,.F.);
#20997=ORIENTED_EDGE('',*,*,#16341,.F.);
#20998=ORIENTED_EDGE('',*,*,#16339,.F.);
#20999=ORIENTED_EDGE('',*,*,#16359,.T.);
#21000=ORIENTED_EDGE('',*,*,#16360,.T.);
#21001=ORIENTED_EDGE('',*,*,#16359,.F.);
#21002=ORIENTED_EDGE('',*,*,#16361,.T.);
#21003=ORIENTED_EDGE('',*,*,#16362,.T.);
#21004=ORIENTED_EDGE('',*,*,#16358,.T.);
#21005=ORIENTED_EDGE('',*,*,#16362,.F.);
#21006=ORIENTED_EDGE('',*,*,#16361,.F.);
#21007=ORIENTED_EDGE('',*,*,#16363,.T.);
#21008=ORIENTED_EDGE('',*,*,#16364,.T.);
#21009=ORIENTED_EDGE('',*,*,#16363,.F.);
#21010=ORIENTED_EDGE('',*,*,#16365,.T.);
#21011=ORIENTED_EDGE('',*,*,#16360,.F.);
#21012=ORIENTED_EDGE('',*,*,#16365,.F.);
#21013=ORIENTED_EDGE('',*,*,#16366,.T.);
#21014=ORIENTED_EDGE('',*,*,#16364,.F.);
#21015=ORIENTED_EDGE('',*,*,#16366,.F.);
#21016=ORIENTED_EDGE('',*,*,#16367,.T.);
#21017=ORIENTED_EDGE('',*,*,#16368,.T.);
#21018=ORIENTED_EDGE('',*,*,#16369,.T.);
#21019=ORIENTED_EDGE('',*,*,#16368,.F.);
#21020=ORIENTED_EDGE('',*,*,#16370,.F.);
#21021=ORIENTED_EDGE('',*,*,#16371,.T.);
#21022=ORIENTED_EDGE('',*,*,#16372,.F.);
#21023=ORIENTED_EDGE('',*,*,#16373,.T.);
#21024=ORIENTED_EDGE('',*,*,#16374,.F.);
#21025=ORIENTED_EDGE('',*,*,#16375,.T.);
#21026=ORIENTED_EDGE('',*,*,#16376,.F.);
#21027=ORIENTED_EDGE('',*,*,#16377,.T.);
#21028=ORIENTED_EDGE('',*,*,#16378,.F.);
#21029=ORIENTED_EDGE('',*,*,#16379,.T.);
#21030=ORIENTED_EDGE('',*,*,#16380,.F.);
#21031=ORIENTED_EDGE('',*,*,#16381,.T.);
#21032=ORIENTED_EDGE('',*,*,#16382,.T.);
#21033=ORIENTED_EDGE('',*,*,#16383,.T.);
#21034=ORIENTED_EDGE('',*,*,#16384,.T.);
#21035=ORIENTED_EDGE('',*,*,#16385,.T.);
#21036=ORIENTED_EDGE('',*,*,#16386,.F.);
#21037=ORIENTED_EDGE('',*,*,#16369,.F.);
#21038=ORIENTED_EDGE('',*,*,#16367,.F.);
#21039=ORIENTED_EDGE('',*,*,#16387,.T.);
#21040=ORIENTED_EDGE('',*,*,#16388,.T.);
#21041=ORIENTED_EDGE('',*,*,#16387,.F.);
#21042=ORIENTED_EDGE('',*,*,#16389,.T.);
#21043=ORIENTED_EDGE('',*,*,#16390,.T.);
#21044=ORIENTED_EDGE('',*,*,#16386,.T.);
#21045=ORIENTED_EDGE('',*,*,#16390,.F.);
#21046=ORIENTED_EDGE('',*,*,#16389,.F.);
#21047=ORIENTED_EDGE('',*,*,#16391,.T.);
#21048=ORIENTED_EDGE('',*,*,#16392,.T.);
#21049=ORIENTED_EDGE('',*,*,#16391,.F.);
#21050=ORIENTED_EDGE('',*,*,#16393,.T.);
#21051=ORIENTED_EDGE('',*,*,#16388,.F.);
#21052=ORIENTED_EDGE('',*,*,#16393,.F.);
#21053=ORIENTED_EDGE('',*,*,#16394,.T.);
#21054=ORIENTED_EDGE('',*,*,#16392,.F.);
#21055=ORIENTED_EDGE('',*,*,#16394,.F.);
#21056=ORIENTED_EDGE('',*,*,#16342,.T.);
#21057=ORIENTED_EDGE('',*,*,#16395,.T.);
#21058=ORIENTED_EDGE('',*,*,#16370,.T.);
#21059=ORIENTED_EDGE('',*,*,#16396,.T.);
#21060=ORIENTED_EDGE('',*,*,#16395,.F.);
#21061=ORIENTED_EDGE('',*,*,#16357,.F.);
#21062=ORIENTED_EDGE('',*,*,#16397,.F.);
#21063=ORIENTED_EDGE('',*,*,#16371,.F.);
#21064=ORIENTED_EDGE('',*,*,#16348,.T.);
#21065=ORIENTED_EDGE('',*,*,#16398,.T.);
#21066=ORIENTED_EDGE('',*,*,#16380,.T.);
#21067=ORIENTED_EDGE('',*,*,#16399,.T.);
#21068=ORIENTED_EDGE('',*,*,#16399,.F.);
#21069=ORIENTED_EDGE('',*,*,#16379,.F.);
#21070=ORIENTED_EDGE('',*,*,#16400,.F.);
#21071=ORIENTED_EDGE('',*,*,#16349,.F.);
#21072=ORIENTED_EDGE('',*,*,#16350,.T.);
#21073=ORIENTED_EDGE('',*,*,#16400,.T.);
#21074=ORIENTED_EDGE('',*,*,#16378,.T.);
#21075=ORIENTED_EDGE('',*,*,#16401,.T.);
#21076=ORIENTED_EDGE('',*,*,#16352,.T.);
#21077=ORIENTED_EDGE('',*,*,#16402,.T.);
#21078=ORIENTED_EDGE('',*,*,#16376,.T.);
#21079=ORIENTED_EDGE('',*,*,#16403,.T.);
#21080=ORIENTED_EDGE('',*,*,#16403,.F.);
#21081=ORIENTED_EDGE('',*,*,#16375,.F.);
#21082=ORIENTED_EDGE('',*,*,#16404,.F.);
#21083=ORIENTED_EDGE('',*,*,#16353,.F.);
#21084=ORIENTED_EDGE('',*,*,#16354,.T.);
#21085=ORIENTED_EDGE('',*,*,#16404,.T.);
#21086=ORIENTED_EDGE('',*,*,#16374,.T.);
#21087=ORIENTED_EDGE('',*,*,#16405,.T.);
#21088=ORIENTED_EDGE('',*,*,#16356,.T.);
#21089=ORIENTED_EDGE('',*,*,#16406,.T.);
#21090=ORIENTED_EDGE('',*,*,#16372,.T.);
#21091=ORIENTED_EDGE('',*,*,#16397,.T.);
#21092=ORIENTED_EDGE('',*,*,#16405,.F.);
#21093=ORIENTED_EDGE('',*,*,#16373,.F.);
#21094=ORIENTED_EDGE('',*,*,#16406,.F.);
#21095=ORIENTED_EDGE('',*,*,#16355,.F.);
#21096=ORIENTED_EDGE('',*,*,#16401,.F.);
#21097=ORIENTED_EDGE('',*,*,#16377,.F.);
#21098=ORIENTED_EDGE('',*,*,#16402,.F.);
#21099=ORIENTED_EDGE('',*,*,#16351,.F.);
#21100=ORIENTED_EDGE('',*,*,#16398,.F.);
#21101=ORIENTED_EDGE('',*,*,#16347,.F.);
#21102=ORIENTED_EDGE('',*,*,#16407,.F.);
#21103=ORIENTED_EDGE('',*,*,#16381,.F.);
#21104=ORIENTED_EDGE('',*,*,#16382,.F.);
#21105=ORIENTED_EDGE('',*,*,#16407,.T.);
#21106=ORIENTED_EDGE('',*,*,#16346,.F.);
#21107=ORIENTED_EDGE('',*,*,#16408,.F.);
#21108=ORIENTED_EDGE('',*,*,#16383,.F.);
#21109=ORIENTED_EDGE('',*,*,#16408,.T.);
#21110=ORIENTED_EDGE('',*,*,#16345,.F.);
#21111=ORIENTED_EDGE('',*,*,#16409,.F.);
#21112=ORIENTED_EDGE('',*,*,#16384,.F.);
#21113=ORIENTED_EDGE('',*,*,#16409,.T.);
#21114=ORIENTED_EDGE('',*,*,#16344,.F.);
#21115=ORIENTED_EDGE('',*,*,#16410,.F.);
#21116=ORIENTED_EDGE('',*,*,#16396,.F.);
#21117=ORIENTED_EDGE('',*,*,#16385,.F.);
#21118=ORIENTED_EDGE('',*,*,#16410,.T.);
#21119=ORIENTED_EDGE('',*,*,#16343,.F.);
#21120=ORIENTED_EDGE('',*,*,#16411,.T.);
#21121=ORIENTED_EDGE('',*,*,#16412,.T.);
#21122=ORIENTED_EDGE('',*,*,#16413,.T.);
#21123=ORIENTED_EDGE('',*,*,#16412,.F.);
#21124=ORIENTED_EDGE('',*,*,#16414,.F.);
#21125=ORIENTED_EDGE('',*,*,#16415,.F.);
#21126=ORIENTED_EDGE('',*,*,#16416,.T.);
#21127=ORIENTED_EDGE('',*,*,#16417,.F.);
#21128=ORIENTED_EDGE('',*,*,#16418,.F.);
#21129=ORIENTED_EDGE('',*,*,#16413,.F.);
#21130=ORIENTED_EDGE('',*,*,#16411,.F.);
#21131=ORIENTED_EDGE('',*,*,#16419,.T.);
#21132=ORIENTED_EDGE('',*,*,#16420,.T.);
#21133=ORIENTED_EDGE('',*,*,#16421,.T.);
#21134=ORIENTED_EDGE('',*,*,#16419,.F.);
#21135=ORIENTED_EDGE('',*,*,#16422,.T.);
#21136=ORIENTED_EDGE('',*,*,#16423,.T.);
#21137=ORIENTED_EDGE('',*,*,#16418,.T.);
#21138=ORIENTED_EDGE('',*,*,#16423,.F.);
#21139=ORIENTED_EDGE('',*,*,#16422,.F.);
#21140=ORIENTED_EDGE('',*,*,#16424,.T.);
#21141=ORIENTED_EDGE('',*,*,#16425,.T.);
#21142=ORIENTED_EDGE('',*,*,#16426,.T.);
#21143=ORIENTED_EDGE('',*,*,#16424,.F.);
#21144=ORIENTED_EDGE('',*,*,#16427,.T.);
#21145=ORIENTED_EDGE('',*,*,#16420,.F.);
#21146=ORIENTED_EDGE('',*,*,#16421,.F.);
#21147=ORIENTED_EDGE('',*,*,#16427,.F.);
#21148=ORIENTED_EDGE('',*,*,#16428,.T.);
#21149=ORIENTED_EDGE('',*,*,#16425,.F.);
#21150=ORIENTED_EDGE('',*,*,#16426,.F.);
#21151=ORIENTED_EDGE('',*,*,#16428,.F.);
#21152=ORIENTED_EDGE('',*,*,#16429,.T.);
#21153=ORIENTED_EDGE('',*,*,#16430,.T.);
#21154=ORIENTED_EDGE('',*,*,#16431,.T.);
#21155=ORIENTED_EDGE('',*,*,#16430,.F.);
#21156=ORIENTED_EDGE('',*,*,#16432,.F.);
#21157=ORIENTED_EDGE('',*,*,#16433,.F.);
#21158=ORIENTED_EDGE('',*,*,#16434,.F.);
#21159=ORIENTED_EDGE('',*,*,#16435,.F.);
#21160=ORIENTED_EDGE('',*,*,#16436,.F.);
#21161=ORIENTED_EDGE('',*,*,#16437,.F.);
#21162=ORIENTED_EDGE('',*,*,#16438,.F.);
#21163=ORIENTED_EDGE('',*,*,#16439,.F.);
#21164=ORIENTED_EDGE('',*,*,#16440,.F.);
#21165=ORIENTED_EDGE('',*,*,#16441,.F.);
#21166=ORIENTED_EDGE('',*,*,#16442,.F.);
#21167=ORIENTED_EDGE('',*,*,#16443,.F.);
#21168=ORIENTED_EDGE('',*,*,#16444,.F.);
#21169=ORIENTED_EDGE('',*,*,#16431,.F.);
#21170=ORIENTED_EDGE('',*,*,#16429,.F.);
#21171=ORIENTED_EDGE('',*,*,#16445,.T.);
#21172=ORIENTED_EDGE('',*,*,#16446,.T.);
#21173=ORIENTED_EDGE('',*,*,#16445,.F.);
#21174=ORIENTED_EDGE('',*,*,#16447,.T.);
#21175=ORIENTED_EDGE('',*,*,#16448,.T.);
#21176=ORIENTED_EDGE('',*,*,#16436,.T.);
#21177=ORIENTED_EDGE('',*,*,#16448,.F.);
#21178=ORIENTED_EDGE('',*,*,#16447,.F.);
#21179=ORIENTED_EDGE('',*,*,#16449,.T.);
#21180=ORIENTED_EDGE('',*,*,#16450,.T.);
#21181=ORIENTED_EDGE('',*,*,#16449,.F.);
#21182=ORIENTED_EDGE('',*,*,#16451,.T.);
#21183=ORIENTED_EDGE('',*,*,#16452,.T.);
#21184=ORIENTED_EDGE('',*,*,#16444,.T.);
#21185=ORIENTED_EDGE('',*,*,#16452,.F.);
#21186=ORIENTED_EDGE('',*,*,#16451,.F.);
#21187=ORIENTED_EDGE('',*,*,#16453,.T.);
#21188=ORIENTED_EDGE('',*,*,#16454,.T.);
#21189=ORIENTED_EDGE('',*,*,#16453,.F.);
#21190=ORIENTED_EDGE('',*,*,#16455,.T.);
#21191=ORIENTED_EDGE('',*,*,#16456,.T.);
#21192=ORIENTED_EDGE('',*,*,#16437,.T.);
#21193=ORIENTED_EDGE('',*,*,#16456,.F.);
#21194=ORIENTED_EDGE('',*,*,#16455,.F.);
#21195=ORIENTED_EDGE('',*,*,#16457,.T.);
#21196=ORIENTED_EDGE('',*,*,#16458,.T.);
#21197=ORIENTED_EDGE('',*,*,#16457,.F.);
#21198=ORIENTED_EDGE('',*,*,#16459,.T.);
#21199=ORIENTED_EDGE('',*,*,#16446,.F.);
#21200=ORIENTED_EDGE('',*,*,#16459,.F.);
#21201=ORIENTED_EDGE('',*,*,#16460,.T.);
#21202=ORIENTED_EDGE('',*,*,#16458,.F.);
#21203=ORIENTED_EDGE('',*,*,#16460,.F.);
#21204=ORIENTED_EDGE('',*,*,#16461,.T.);
#21205=ORIENTED_EDGE('',*,*,#16454,.F.);
#21206=ORIENTED_EDGE('',*,*,#16461,.F.);
#21207=ORIENTED_EDGE('',*,*,#16462,.T.);
#21208=ORIENTED_EDGE('',*,*,#16450,.F.);
#21209=ORIENTED_EDGE('',*,*,#16462,.F.);
#21210=ORIENTED_EDGE('',*,*,#16463,.T.);
#21211=ORIENTED_EDGE('',*,*,#16464,.T.);
#21212=ORIENTED_EDGE('',*,*,#16438,.T.);
#21213=ORIENTED_EDGE('',*,*,#16464,.F.);
#21214=ORIENTED_EDGE('',*,*,#16463,.F.);
#21215=ORIENTED_EDGE('',*,*,#16465,.T.);
#21216=ORIENTED_EDGE('',*,*,#16466,.T.);
#21217=ORIENTED_EDGE('',*,*,#16465,.F.);
#21218=ORIENTED_EDGE('',*,*,#16467,.T.);
#21219=ORIENTED_EDGE('',*,*,#16468,.T.);
#21220=ORIENTED_EDGE('',*,*,#16443,.T.);
#21221=ORIENTED_EDGE('',*,*,#16468,.F.);
#21222=ORIENTED_EDGE('',*,*,#16467,.F.);
#21223=ORIENTED_EDGE('',*,*,#16469,.T.);
#21224=ORIENTED_EDGE('',*,*,#16470,.T.);
#21225=ORIENTED_EDGE('',*,*,#16469,.F.);
#21226=ORIENTED_EDGE('',*,*,#16471,.T.);
#21227=ORIENTED_EDGE('',*,*,#16472,.T.);
#21228=ORIENTED_EDGE('',*,*,#16439,.T.);
#21229=ORIENTED_EDGE('',*,*,#16472,.F.);
#21230=ORIENTED_EDGE('',*,*,#16471,.F.);
#21231=ORIENTED_EDGE('',*,*,#16473,.T.);
#21232=ORIENTED_EDGE('',*,*,#16474,.T.);
#21233=ORIENTED_EDGE('',*,*,#16473,.F.);
#21234=ORIENTED_EDGE('',*,*,#16475,.T.);
#21235=ORIENTED_EDGE('',*,*,#16476,.T.);
#21236=ORIENTED_EDGE('',*,*,#16442,.T.);
#21237=ORIENTED_EDGE('',*,*,#16476,.F.);
#21238=ORIENTED_EDGE('',*,*,#16475,.F.);
#21239=ORIENTED_EDGE('',*,*,#16477,.T.);
#21240=ORIENTED_EDGE('',*,*,#16478,.T.);
#21241=ORIENTED_EDGE('',*,*,#16477,.F.);
#21242=ORIENTED_EDGE('',*,*,#16479,.T.);
#21243=ORIENTED_EDGE('',*,*,#16480,.T.);
#21244=ORIENTED_EDGE('',*,*,#16440,.T.);
#21245=ORIENTED_EDGE('',*,*,#16480,.F.);
#21246=ORIENTED_EDGE('',*,*,#16479,.F.);
#21247=ORIENTED_EDGE('',*,*,#16481,.T.);
#21248=ORIENTED_EDGE('',*,*,#16482,.T.);
#21249=ORIENTED_EDGE('',*,*,#16481,.F.);
#21250=ORIENTED_EDGE('',*,*,#16483,.T.);
#21251=ORIENTED_EDGE('',*,*,#16484,.T.);
#21252=ORIENTED_EDGE('',*,*,#16441,.T.);
#21253=ORIENTED_EDGE('',*,*,#16484,.F.);
#21254=ORIENTED_EDGE('',*,*,#16483,.F.);
#21255=ORIENTED_EDGE('',*,*,#16485,.T.);
#21256=ORIENTED_EDGE('',*,*,#16486,.T.);
#21257=ORIENTED_EDGE('',*,*,#16485,.F.);
#21258=ORIENTED_EDGE('',*,*,#16487,.T.);
#21259=ORIENTED_EDGE('',*,*,#16466,.F.);
#21260=ORIENTED_EDGE('',*,*,#16487,.F.);
#21261=ORIENTED_EDGE('',*,*,#16488,.T.);
#21262=ORIENTED_EDGE('',*,*,#16486,.F.);
#21263=ORIENTED_EDGE('',*,*,#16488,.F.);
#21264=ORIENTED_EDGE('',*,*,#16489,.T.);
#21265=ORIENTED_EDGE('',*,*,#16470,.F.);
#21266=ORIENTED_EDGE('',*,*,#16489,.F.);
#21267=ORIENTED_EDGE('',*,*,#16490,.T.);
#21268=ORIENTED_EDGE('',*,*,#16474,.F.);
#21269=ORIENTED_EDGE('',*,*,#16490,.F.);
#21270=ORIENTED_EDGE('',*,*,#16491,.T.);
#21271=ORIENTED_EDGE('',*,*,#16478,.F.);
#21272=ORIENTED_EDGE('',*,*,#16491,.F.);
#21273=ORIENTED_EDGE('',*,*,#16492,.T.);
#21274=ORIENTED_EDGE('',*,*,#16482,.F.);
#21275=ORIENTED_EDGE('',*,*,#16492,.F.);
#21276=ORIENTED_EDGE('',*,*,#16493,.F.);
#21277=ORIENTED_EDGE('',*,*,#16494,.F.);
#21278=ORIENTED_EDGE('',*,*,#16495,.F.);
#21279=ORIENTED_EDGE('',*,*,#16496,.F.);
#21280=ORIENTED_EDGE('',*,*,#16496,.T.);
#21281=ORIENTED_EDGE('',*,*,#16497,.T.);
#21282=ORIENTED_EDGE('',*,*,#16498,.T.);
#21283=ORIENTED_EDGE('',*,*,#16499,.F.);
#21284=ORIENTED_EDGE('',*,*,#16417,.T.);
#21285=ORIENTED_EDGE('',*,*,#16500,.T.);
#21286=ORIENTED_EDGE('',*,*,#16495,.T.);
#21287=ORIENTED_EDGE('',*,*,#16501,.T.);
#21288=ORIENTED_EDGE('',*,*,#16502,.T.);
#21289=ORIENTED_EDGE('',*,*,#16503,.T.);
#21290=ORIENTED_EDGE('',*,*,#16504,.T.);
#21291=ORIENTED_EDGE('',*,*,#16505,.T.);
#21292=ORIENTED_EDGE('',*,*,#16506,.T.);
#21293=ORIENTED_EDGE('',*,*,#16507,.F.);
#21294=ORIENTED_EDGE('',*,*,#16508,.T.);
#21295=ORIENTED_EDGE('',*,*,#16497,.F.);
#21296=ORIENTED_EDGE('',*,*,#16509,.F.);
#21297=ORIENTED_EDGE('',*,*,#16510,.F.);
#21298=ORIENTED_EDGE('',*,*,#16506,.F.);
#21299=ORIENTED_EDGE('',*,*,#16511,.F.);
#21300=ORIENTED_EDGE('',*,*,#16511,.T.);
#21301=ORIENTED_EDGE('',*,*,#16505,.F.);
#21302=ORIENTED_EDGE('',*,*,#16512,.T.);
#21303=ORIENTED_EDGE('',*,*,#16513,.F.);
#21304=ORIENTED_EDGE('',*,*,#16494,.T.);
#21305=ORIENTED_EDGE('',*,*,#16514,.F.);
#21306=ORIENTED_EDGE('',*,*,#16515,.F.);
#21307=ORIENTED_EDGE('',*,*,#16501,.F.);
#21308=ORIENTED_EDGE('',*,*,#16516,.F.);
#21309=ORIENTED_EDGE('',*,*,#16512,.F.);
#21310=ORIENTED_EDGE('',*,*,#16517,.F.);
#21311=ORIENTED_EDGE('',*,*,#16518,.T.);
#21312=ORIENTED_EDGE('',*,*,#16519,.F.);
#21313=ORIENTED_EDGE('',*,*,#16515,.T.);
#21314=ORIENTED_EDGE('',*,*,#16520,.F.);
#21315=ORIENTED_EDGE('',*,*,#16518,.F.);
#21316=ORIENTED_EDGE('',*,*,#16432,.T.);
#21317=ORIENTED_EDGE('',*,*,#16521,.T.);
#21318=ORIENTED_EDGE('',*,*,#16522,.T.);
#21319=ORIENTED_EDGE('',*,*,#16523,.T.);
#21320=ORIENTED_EDGE('',*,*,#16524,.T.);
#21321=ORIENTED_EDGE('',*,*,#16521,.F.);
#21322=ORIENTED_EDGE('',*,*,#16435,.T.);
#21323=ORIENTED_EDGE('',*,*,#16525,.T.);
#21324=ORIENTED_EDGE('',*,*,#16499,.T.);
#21325=ORIENTED_EDGE('',*,*,#16525,.F.);
#21326=ORIENTED_EDGE('',*,*,#16434,.T.);
#21327=ORIENTED_EDGE('',*,*,#16526,.F.);
#21328=ORIENTED_EDGE('',*,*,#16433,.T.);
#21329=ORIENTED_EDGE('',*,*,#16523,.F.);
#21330=ORIENTED_EDGE('',*,*,#16414,.T.);
#21331=ORIENTED_EDGE('',*,*,#16526,.T.);
#21332=ORIENTED_EDGE('',*,*,#16510,.T.);
#21333=ORIENTED_EDGE('',*,*,#16527,.T.);
#21334=ORIENTED_EDGE('',*,*,#16415,.T.);
#21335=ORIENTED_EDGE('',*,*,#16522,.F.);
#21336=ORIENTED_EDGE('',*,*,#16528,.T.);
#21337=ORIENTED_EDGE('',*,*,#16507,.T.);
#21338=ORIENTED_EDGE('',*,*,#16519,.T.);
#21339=ORIENTED_EDGE('',*,*,#16520,.T.);
#21340=ORIENTED_EDGE('',*,*,#16529,.F.);
#21341=ORIENTED_EDGE('',*,*,#16530,.T.);
#21342=ORIENTED_EDGE('',*,*,#16531,.T.);
#21343=ORIENTED_EDGE('',*,*,#16532,.T.);
#21344=ORIENTED_EDGE('',*,*,#16533,.T.);
#21345=ORIENTED_EDGE('',*,*,#16534,.T.);
#21346=ORIENTED_EDGE('',*,*,#16502,.F.);
#21347=ORIENTED_EDGE('',*,*,#16535,.F.);
#21348=ORIENTED_EDGE('',*,*,#16503,.F.);
#21349=ORIENTED_EDGE('',*,*,#16534,.F.);
#21350=ORIENTED_EDGE('',*,*,#16536,.F.);
#21351=ORIENTED_EDGE('',*,*,#16537,.F.);
#21352=ORIENTED_EDGE('',*,*,#16536,.T.);
#21353=ORIENTED_EDGE('',*,*,#16533,.F.);
#21354=ORIENTED_EDGE('',*,*,#16538,.F.);
#21355=ORIENTED_EDGE('',*,*,#16539,.F.);
#21356=ORIENTED_EDGE('',*,*,#16538,.T.);
#21357=ORIENTED_EDGE('',*,*,#16532,.F.);
#21358=ORIENTED_EDGE('',*,*,#16540,.F.);
#21359=ORIENTED_EDGE('',*,*,#16541,.F.);
#21360=ORIENTED_EDGE('',*,*,#16540,.T.);
#21361=ORIENTED_EDGE('',*,*,#16531,.F.);
#21362=ORIENTED_EDGE('',*,*,#16542,.F.);
#21363=ORIENTED_EDGE('',*,*,#16543,.F.);
#21364=ORIENTED_EDGE('',*,*,#16542,.T.);
#21365=ORIENTED_EDGE('',*,*,#16530,.F.);
#21366=ORIENTED_EDGE('',*,*,#16544,.F.);
#21367=ORIENTED_EDGE('',*,*,#16516,.T.);
#21368=ORIENTED_EDGE('',*,*,#16517,.T.);
#21369=ORIENTED_EDGE('',*,*,#16504,.F.);
#21370=ORIENTED_EDGE('',*,*,#16535,.T.);
#21371=ORIENTED_EDGE('',*,*,#16537,.T.);
#21372=ORIENTED_EDGE('',*,*,#16539,.T.);
#21373=ORIENTED_EDGE('',*,*,#16541,.T.);
#21374=ORIENTED_EDGE('',*,*,#16543,.T.);
#21375=ORIENTED_EDGE('',*,*,#16545,.F.);
#21376=ORIENTED_EDGE('',*,*,#16524,.F.);
#21377=ORIENTED_EDGE('',*,*,#16498,.F.);
#21378=ORIENTED_EDGE('',*,*,#16508,.F.);
#21379=ORIENTED_EDGE('',*,*,#16528,.F.);
#21380=ORIENTED_EDGE('',*,*,#16493,.T.);
#21381=ORIENTED_EDGE('',*,*,#16500,.F.);
#21382=ORIENTED_EDGE('',*,*,#16416,.F.);
#21383=ORIENTED_EDGE('',*,*,#16527,.F.);
#21384=ORIENTED_EDGE('',*,*,#16509,.T.);
#21385=ORIENTED_EDGE('',*,*,#16513,.T.);
#21386=ORIENTED_EDGE('',*,*,#16545,.T.);
#21387=ORIENTED_EDGE('',*,*,#16544,.T.);
#21388=ORIENTED_EDGE('',*,*,#16529,.T.);
#21389=ORIENTED_EDGE('',*,*,#16514,.T.);
#21390=ORIENTED_EDGE('',*,*,#16546,.T.);
#21391=ORIENTED_EDGE('',*,*,#16547,.T.);
#21392=ORIENTED_EDGE('',*,*,#16548,.T.);
#21393=ORIENTED_EDGE('',*,*,#16547,.F.);
#21394=ORIENTED_EDGE('',*,*,#16549,.T.);
#21395=ORIENTED_EDGE('',*,*,#16546,.F.);
#21396=ORIENTED_EDGE('',*,*,#16550,.T.);
#21397=ORIENTED_EDGE('',*,*,#16551,.F.);
#21398=ORIENTED_EDGE('',*,*,#16552,.F.);
#21399=ORIENTED_EDGE('',*,*,#16550,.F.);
#21400=ORIENTED_EDGE('',*,*,#16549,.F.);
#21401=ORIENTED_EDGE('',*,*,#16553,.F.);
#21402=ORIENTED_EDGE('',*,*,#16548,.F.);
#21403=ORIENTED_EDGE('',*,*,#16551,.T.);
#21404=ORIENTED_EDGE('',*,*,#16552,.T.);
#21405=ORIENTED_EDGE('',*,*,#16554,.T.);
#21406=ORIENTED_EDGE('',*,*,#16555,.T.);
#21407=ORIENTED_EDGE('',*,*,#16554,.F.);
#21408=ORIENTED_EDGE('',*,*,#16556,.T.);
#21409=ORIENTED_EDGE('',*,*,#16555,.F.);
#21410=ORIENTED_EDGE('',*,*,#16557,.F.);
#21411=ORIENTED_EDGE('',*,*,#16558,.T.);
#21412=ORIENTED_EDGE('',*,*,#16553,.T.);
#21413=ORIENTED_EDGE('',*,*,#16558,.F.);
#21414=ORIENTED_EDGE('',*,*,#16559,.F.);
#21415=ORIENTED_EDGE('',*,*,#16560,.T.);
#21416=ORIENTED_EDGE('',*,*,#16557,.T.);
#21417=ORIENTED_EDGE('',*,*,#16560,.F.);
#21418=ORIENTED_EDGE('',*,*,#16559,.T.);
#21419=ORIENTED_EDGE('',*,*,#16561,.T.);
#21420=ORIENTED_EDGE('',*,*,#16556,.F.);
#21421=ORIENTED_EDGE('',*,*,#16561,.F.);
#21422=ORIENTED_EDGE('',*,*,#16562,.T.);
#21423=ORIENTED_EDGE('',*,*,#16563,.T.);
#21424=ORIENTED_EDGE('',*,*,#16562,.F.);
#21425=ORIENTED_EDGE('',*,*,#16564,.T.);
#21426=ORIENTED_EDGE('',*,*,#16565,.T.);
#21427=ORIENTED_EDGE('',*,*,#16566,.T.);
#21428=ORIENTED_EDGE('',*,*,#16567,.T.);
#21429=ORIENTED_EDGE('',*,*,#16568,.T.);
#21430=ORIENTED_EDGE('',*,*,#16569,.T.);
#21431=ORIENTED_EDGE('',*,*,#16570,.T.);
#21432=ORIENTED_EDGE('',*,*,#16571,.T.);
#21433=ORIENTED_EDGE('',*,*,#16572,.T.);
#21434=ORIENTED_EDGE('',*,*,#16566,.F.);
#21435=ORIENTED_EDGE('',*,*,#16573,.T.);
#21436=ORIENTED_EDGE('',*,*,#16574,.T.);
#21437=ORIENTED_EDGE('',*,*,#16575,.T.);
#21438=ORIENTED_EDGE('',*,*,#16576,.T.);
#21439=ORIENTED_EDGE('',*,*,#16571,.F.);
#21440=ORIENTED_EDGE('',*,*,#16577,.T.);
#21441=ORIENTED_EDGE('',*,*,#16578,.T.);
#21442=ORIENTED_EDGE('',*,*,#16579,.T.);
#21443=ORIENTED_EDGE('',*,*,#16580,.T.);
#21444=ORIENTED_EDGE('',*,*,#16575,.F.);
#21445=ORIENTED_EDGE('',*,*,#16581,.T.);
#21446=ORIENTED_EDGE('',*,*,#16582,.T.);
#21447=ORIENTED_EDGE('',*,*,#16583,.T.);
#21448=ORIENTED_EDGE('',*,*,#16584,.T.);
#21449=ORIENTED_EDGE('',*,*,#16585,.T.);
#21450=ORIENTED_EDGE('',*,*,#16578,.F.);
#21451=ORIENTED_EDGE('',*,*,#16586,.T.);
#21452=ORIENTED_EDGE('',*,*,#16587,.T.);
#21453=ORIENTED_EDGE('',*,*,#16588,.T.);
#21454=ORIENTED_EDGE('',*,*,#16589,.T.);
#21455=ORIENTED_EDGE('',*,*,#16583,.F.);
#21456=ORIENTED_EDGE('',*,*,#16590,.T.);
#21457=ORIENTED_EDGE('',*,*,#16591,.T.);
#21458=ORIENTED_EDGE('',*,*,#16592,.T.);
#21459=ORIENTED_EDGE('',*,*,#16593,.T.);
#21460=ORIENTED_EDGE('',*,*,#16587,.F.);
#21461=ORIENTED_EDGE('',*,*,#16594,.T.);
#21462=ORIENTED_EDGE('',*,*,#16595,.T.);
#21463=ORIENTED_EDGE('',*,*,#16596,.T.);
#21464=ORIENTED_EDGE('',*,*,#16597,.T.);
#21465=ORIENTED_EDGE('',*,*,#16591,.F.);
#21466=ORIENTED_EDGE('',*,*,#16598,.T.);
#21467=ORIENTED_EDGE('',*,*,#16599,.T.);
#21468=ORIENTED_EDGE('',*,*,#16596,.F.);
#21469=ORIENTED_EDGE('',*,*,#16600,.T.);
#21470=ORIENTED_EDGE('',*,*,#16601,.T.);
#21471=ORIENTED_EDGE('',*,*,#16602,.T.);
#21472=ORIENTED_EDGE('',*,*,#16603,.T.);
#21473=ORIENTED_EDGE('',*,*,#16604,.T.);
#21474=ORIENTED_EDGE('',*,*,#16605,.T.);
#21475=ORIENTED_EDGE('',*,*,#16606,.T.);
#21476=ORIENTED_EDGE('',*,*,#16602,.F.);
#21477=ORIENTED_EDGE('',*,*,#16607,.T.);
#21478=ORIENTED_EDGE('',*,*,#16608,.T.);
#21479=ORIENTED_EDGE('',*,*,#16609,.T.);
#21480=ORIENTED_EDGE('',*,*,#16610,.T.);
#21481=ORIENTED_EDGE('',*,*,#16611,.T.);
#21482=ORIENTED_EDGE('',*,*,#16612,.T.);
#21483=ORIENTED_EDGE('',*,*,#16605,.F.);
#21484=ORIENTED_EDGE('',*,*,#16613,.T.);
#21485=ORIENTED_EDGE('',*,*,#16614,.T.);
#21486=ORIENTED_EDGE('',*,*,#16615,.T.);
#21487=ORIENTED_EDGE('',*,*,#16616,.T.);
#21488=ORIENTED_EDGE('',*,*,#16610,.F.);
#21489=ORIENTED_EDGE('',*,*,#16617,.T.);
#21490=ORIENTED_EDGE('',*,*,#16618,.T.);
#21491=ORIENTED_EDGE('',*,*,#16619,.T.);
#21492=ORIENTED_EDGE('',*,*,#16620,.T.);
#21493=ORIENTED_EDGE('',*,*,#16621,.T.);
#21494=ORIENTED_EDGE('',*,*,#16622,.T.);
#21495=ORIENTED_EDGE('',*,*,#16614,.F.);
#21496=ORIENTED_EDGE('',*,*,#16623,.T.);
#21497=ORIENTED_EDGE('',*,*,#16624,.T.);
#21498=ORIENTED_EDGE('',*,*,#16625,.T.);
#21499=ORIENTED_EDGE('',*,*,#16620,.F.);
#21500=ORIENTED_EDGE('',*,*,#16626,.T.);
#21501=ORIENTED_EDGE('',*,*,#16627,.T.);
#21502=ORIENTED_EDGE('',*,*,#16628,.T.);
#21503=ORIENTED_EDGE('',*,*,#16629,.T.);
#21504=ORIENTED_EDGE('',*,*,#16630,.T.);
#21505=ORIENTED_EDGE('',*,*,#16627,.F.);
#21506=ORIENTED_EDGE('',*,*,#16631,.T.);
#21507=ORIENTED_EDGE('',*,*,#16632,.T.);
#21508=ORIENTED_EDGE('',*,*,#16633,.T.);
#21509=ORIENTED_EDGE('',*,*,#16634,.T.);
#21510=ORIENTED_EDGE('',*,*,#16628,.F.);
#21511=ORIENTED_EDGE('',*,*,#16635,.T.);
#21512=ORIENTED_EDGE('',*,*,#16636,.T.);
#21513=ORIENTED_EDGE('',*,*,#16637,.T.);
#21514=ORIENTED_EDGE('',*,*,#16638,.T.);
#21515=ORIENTED_EDGE('',*,*,#16633,.F.);
#21516=ORIENTED_EDGE('',*,*,#16639,.T.);
#21517=ORIENTED_EDGE('',*,*,#16640,.T.);
#21518=ORIENTED_EDGE('',*,*,#16641,.T.);
#21519=ORIENTED_EDGE('',*,*,#16642,.T.);
#21520=ORIENTED_EDGE('',*,*,#16636,.F.);
#21521=ORIENTED_EDGE('',*,*,#16643,.T.);
#21522=ORIENTED_EDGE('',*,*,#16644,.T.);
#21523=ORIENTED_EDGE('',*,*,#16645,.T.);
#21524=ORIENTED_EDGE('',*,*,#16646,.T.);
#21525=ORIENTED_EDGE('',*,*,#16641,.F.);
#21526=ORIENTED_EDGE('',*,*,#16647,.T.);
#21527=ORIENTED_EDGE('',*,*,#16645,.F.);
#21528=ORIENTED_EDGE('',*,*,#16648,.T.);
#21529=ORIENTED_EDGE('',*,*,#16649,.T.);
#21530=ORIENTED_EDGE('',*,*,#16650,.T.);
#21531=ORIENTED_EDGE('',*,*,#16651,.T.);
#21532=ORIENTED_EDGE('',*,*,#16652,.T.);
#21533=ORIENTED_EDGE('',*,*,#16653,.T.);
#21534=ORIENTED_EDGE('',*,*,#16654,.T.);
#21535=ORIENTED_EDGE('',*,*,#16650,.F.);
#21536=ORIENTED_EDGE('',*,*,#16655,.T.);
#21537=ORIENTED_EDGE('',*,*,#16656,.T.);
#21538=ORIENTED_EDGE('',*,*,#16657,.T.);
#21539=ORIENTED_EDGE('',*,*,#16658,.T.);
#21540=ORIENTED_EDGE('',*,*,#16659,.T.);
#21541=ORIENTED_EDGE('',*,*,#16660,.T.);
#21542=ORIENTED_EDGE('',*,*,#16653,.F.);
#21543=ORIENTED_EDGE('',*,*,#16661,.T.);
#21544=ORIENTED_EDGE('',*,*,#16662,.T.);
#21545=ORIENTED_EDGE('',*,*,#16663,.T.);
#21546=ORIENTED_EDGE('',*,*,#16664,.T.);
#21547=ORIENTED_EDGE('',*,*,#16665,.T.);
#21548=ORIENTED_EDGE('',*,*,#16657,.F.);
#21549=ORIENTED_EDGE('',*,*,#16666,.T.);
#21550=ORIENTED_EDGE('',*,*,#16667,.T.);
#21551=ORIENTED_EDGE('',*,*,#16668,.T.);
#21552=ORIENTED_EDGE('',*,*,#16669,.T.);
#21553=ORIENTED_EDGE('',*,*,#16663,.F.);
#21554=ORIENTED_EDGE('',*,*,#16670,.T.);
#21555=ORIENTED_EDGE('',*,*,#16671,.T.);
#21556=ORIENTED_EDGE('',*,*,#16672,.T.);
#21557=ORIENTED_EDGE('',*,*,#16673,.T.);
#21558=ORIENTED_EDGE('',*,*,#16674,.T.);
#21559=ORIENTED_EDGE('',*,*,#16668,.F.);
#21560=ORIENTED_EDGE('',*,*,#16675,.T.);
#21561=ORIENTED_EDGE('',*,*,#16676,.T.);
#21562=ORIENTED_EDGE('',*,*,#16671,.F.);
#21563=ORIENTED_EDGE('',*,*,#16677,.T.);
#21564=ORIENTED_EDGE('',*,*,#16678,.T.);
#21565=ORIENTED_EDGE('',*,*,#16679,.T.);
#21566=ORIENTED_EDGE('',*,*,#16680,.T.);
#21567=ORIENTED_EDGE('',*,*,#16681,.T.);
#21568=ORIENTED_EDGE('',*,*,#16682,.T.);
#21569=ORIENTED_EDGE('',*,*,#16679,.F.);
#21570=ORIENTED_EDGE('',*,*,#16683,.T.);
#21571=ORIENTED_EDGE('',*,*,#16684,.T.);
#21572=ORIENTED_EDGE('',*,*,#16685,.T.);
#21573=ORIENTED_EDGE('',*,*,#16686,.T.);
#21574=ORIENTED_EDGE('',*,*,#16681,.F.);
#21575=ORIENTED_EDGE('',*,*,#16687,.T.);
#21576=ORIENTED_EDGE('',*,*,#16688,.T.);
#21577=ORIENTED_EDGE('',*,*,#16689,.T.);
#21578=ORIENTED_EDGE('',*,*,#16690,.T.);
#21579=ORIENTED_EDGE('',*,*,#16684,.F.);
#21580=ORIENTED_EDGE('',*,*,#16691,.T.);
#21581=ORIENTED_EDGE('',*,*,#16692,.T.);
#21582=ORIENTED_EDGE('',*,*,#16693,.T.);
#21583=ORIENTED_EDGE('',*,*,#16694,.T.);
#21584=ORIENTED_EDGE('',*,*,#16689,.F.);
#21585=ORIENTED_EDGE('',*,*,#16695,.T.);
#21586=ORIENTED_EDGE('',*,*,#16692,.F.);
#21587=ORIENTED_EDGE('',*,*,#16696,.T.);
#21588=ORIENTED_EDGE('',*,*,#16697,.T.);
#21589=ORIENTED_EDGE('',*,*,#16698,.T.);
#21590=ORIENTED_EDGE('',*,*,#16699,.T.);
#21591=ORIENTED_EDGE('',*,*,#16700,.T.);
#21592=ORIENTED_EDGE('',*,*,#16701,.T.);
#21593=ORIENTED_EDGE('',*,*,#16702,.T.);
#21594=ORIENTED_EDGE('',*,*,#16698,.F.);
#21595=ORIENTED_EDGE('',*,*,#16703,.T.);
#21596=ORIENTED_EDGE('',*,*,#16704,.T.);
#21597=ORIENTED_EDGE('',*,*,#16705,.T.);
#21598=ORIENTED_EDGE('',*,*,#16706,.T.);
#21599=ORIENTED_EDGE('',*,*,#16701,.F.);
#21600=ORIENTED_EDGE('',*,*,#16707,.T.);
#21601=ORIENTED_EDGE('',*,*,#16708,.T.);
#21602=ORIENTED_EDGE('',*,*,#16709,.T.);
#21603=ORIENTED_EDGE('',*,*,#16710,.T.);
#21604=ORIENTED_EDGE('',*,*,#16711,.T.);
#21605=ORIENTED_EDGE('',*,*,#16712,.T.);
#21606=ORIENTED_EDGE('',*,*,#16705,.F.);
#21607=ORIENTED_EDGE('',*,*,#16713,.T.);
#21608=ORIENTED_EDGE('',*,*,#16714,.T.);
#21609=ORIENTED_EDGE('',*,*,#16715,.T.);
#21610=ORIENTED_EDGE('',*,*,#16716,.T.);
#21611=ORIENTED_EDGE('',*,*,#16717,.T.);
#21612=ORIENTED_EDGE('',*,*,#16709,.F.);
#21613=ORIENTED_EDGE('',*,*,#16718,.T.);
#21614=ORIENTED_EDGE('',*,*,#16719,.T.);
#21615=ORIENTED_EDGE('',*,*,#16720,.T.);
#21616=ORIENTED_EDGE('',*,*,#16721,.T.);
#21617=ORIENTED_EDGE('',*,*,#16715,.F.);
#21618=ORIENTED_EDGE('',*,*,#16722,.T.);
#21619=ORIENTED_EDGE('',*,*,#16723,.T.);
#21620=ORIENTED_EDGE('',*,*,#16724,.T.);
#21621=ORIENTED_EDGE('',*,*,#16725,.T.);
#21622=ORIENTED_EDGE('',*,*,#16726,.T.);
#21623=ORIENTED_EDGE('',*,*,#16719,.F.);
#21624=ORIENTED_EDGE('',*,*,#16727,.T.);
#21625=ORIENTED_EDGE('',*,*,#16728,.T.);
#21626=ORIENTED_EDGE('',*,*,#16729,.T.);
#21627=ORIENTED_EDGE('',*,*,#16730,.T.);
#21628=ORIENTED_EDGE('',*,*,#16725,.F.);
#21629=ORIENTED_EDGE('',*,*,#16731,.T.);
#21630=ORIENTED_EDGE('',*,*,#16732,.T.);
#21631=ORIENTED_EDGE('',*,*,#16733,.T.);
#21632=ORIENTED_EDGE('',*,*,#16727,.F.);
#21633=ORIENTED_EDGE('',*,*,#16734,.T.);
#21634=ORIENTED_EDGE('',*,*,#16735,.T.);
#21635=ORIENTED_EDGE('',*,*,#16736,.T.);
#21636=ORIENTED_EDGE('',*,*,#16737,.T.);
#21637=ORIENTED_EDGE('',*,*,#16738,.T.);
#21638=ORIENTED_EDGE('',*,*,#16739,.T.);
#21639=ORIENTED_EDGE('',*,*,#16732,.F.);
#21640=ORIENTED_EDGE('',*,*,#16740,.T.);
#21641=ORIENTED_EDGE('',*,*,#16741,.T.);
#21642=ORIENTED_EDGE('',*,*,#16742,.T.);
#21643=ORIENTED_EDGE('',*,*,#16736,.F.);
#21644=ORIENTED_EDGE('',*,*,#16743,.T.);
#21645=ORIENTED_EDGE('',*,*,#16744,.T.);
#21646=ORIENTED_EDGE('',*,*,#16745,.T.);
#21647=ORIENTED_EDGE('',*,*,#16746,.T.);
#21648=ORIENTED_EDGE('',*,*,#16747,.T.);
#21649=ORIENTED_EDGE('',*,*,#16748,.T.);
#21650=ORIENTED_EDGE('',*,*,#16749,.T.);
#21651=ORIENTED_EDGE('',*,*,#16741,.F.);
#21652=ORIENTED_EDGE('',*,*,#16750,.T.);
#21653=ORIENTED_EDGE('',*,*,#16751,.T.);
#21654=ORIENTED_EDGE('',*,*,#16752,.T.);
#21655=ORIENTED_EDGE('',*,*,#16753,.T.);
#21656=ORIENTED_EDGE('',*,*,#16754,.T.);
#21657=ORIENTED_EDGE('',*,*,#16755,.T.);
#21658=ORIENTED_EDGE('',*,*,#16745,.F.);
#21659=ORIENTED_EDGE('',*,*,#16756,.T.);
#21660=ORIENTED_EDGE('',*,*,#16757,.T.);
#21661=ORIENTED_EDGE('',*,*,#16758,.T.);
#21662=ORIENTED_EDGE('',*,*,#16759,.T.);
#21663=ORIENTED_EDGE('',*,*,#16753,.F.);
#21664=ORIENTED_EDGE('',*,*,#16760,.T.);
#21665=ORIENTED_EDGE('',*,*,#16761,.T.);
#21666=ORIENTED_EDGE('',*,*,#16762,.T.);
#21667=ORIENTED_EDGE('',*,*,#16763,.T.);
#21668=ORIENTED_EDGE('',*,*,#16757,.F.);
#21669=ORIENTED_EDGE('',*,*,#16764,.T.);
#21670=ORIENTED_EDGE('',*,*,#16765,.T.);
#21671=ORIENTED_EDGE('',*,*,#16766,.T.);
#21672=ORIENTED_EDGE('',*,*,#16767,.T.);
#21673=ORIENTED_EDGE('',*,*,#16762,.F.);
#21674=ORIENTED_EDGE('',*,*,#16768,.T.);
#21675=ORIENTED_EDGE('',*,*,#16769,.F.);
#21676=ORIENTED_EDGE('',*,*,#16770,.T.);
#21677=ORIENTED_EDGE('',*,*,#16771,.T.);
#21678=ORIENTED_EDGE('',*,*,#16772,.T.);
#21679=ORIENTED_EDGE('',*,*,#16773,.F.);
#21680=ORIENTED_EDGE('',*,*,#16774,.T.);
#21681=ORIENTED_EDGE('',*,*,#16775,.T.);
#21682=ORIENTED_EDGE('',*,*,#16776,.T.);
#21683=ORIENTED_EDGE('',*,*,#16770,.F.);
#21684=ORIENTED_EDGE('',*,*,#16773,.T.);
#21685=ORIENTED_EDGE('',*,*,#16777,.T.);
#21686=ORIENTED_EDGE('',*,*,#16778,.T.);
#21687=ORIENTED_EDGE('',*,*,#16765,.F.);
#21688=ORIENTED_EDGE('',*,*,#16779,.T.);
#21689=ORIENTED_EDGE('',*,*,#16780,.F.);
#21690=ORIENTED_EDGE('',*,*,#16781,.T.);
#21691=ORIENTED_EDGE('',*,*,#16782,.T.);
#21692=ORIENTED_EDGE('',*,*,#16783,.F.);
#21693=ORIENTED_EDGE('',*,*,#16784,.F.);
#21694=ORIENTED_EDGE('',*,*,#16785,.F.);
#21695=ORIENTED_EDGE('',*,*,#16786,.F.);
#21696=ORIENTED_EDGE('',*,*,#16787,.F.);
#21697=ORIENTED_EDGE('',*,*,#16786,.T.);
#21698=ORIENTED_EDGE('',*,*,#16788,.F.);
#21699=ORIENTED_EDGE('',*,*,#16784,.T.);
#21700=ORIENTED_EDGE('',*,*,#16569,.F.);
#21701=ORIENTED_EDGE('',*,*,#16789,.F.);
#21702=ORIENTED_EDGE('',*,*,#16790,.F.);
#21703=ORIENTED_EDGE('',*,*,#16791,.F.);
#21704=ORIENTED_EDGE('',*,*,#16565,.F.);
#21705=ORIENTED_EDGE('',*,*,#16792,.T.);
#21706=ORIENTED_EDGE('',*,*,#16790,.T.);
#21707=ORIENTED_EDGE('',*,*,#16793,.F.);
#21708=ORIENTED_EDGE('',*,*,#16573,.F.);
#21709=ORIENTED_EDGE('',*,*,#16772,.F.);
#21710=ORIENTED_EDGE('',*,*,#16794,.F.);
#21711=ORIENTED_EDGE('',*,*,#16795,.F.);
#21712=ORIENTED_EDGE('',*,*,#16796,.T.);
#21713=ORIENTED_EDGE('',*,*,#16777,.F.);
#21714=ORIENTED_EDGE('',*,*,#16738,.F.);
#21715=ORIENTED_EDGE('',*,*,#16797,.F.);
#21716=ORIENTED_EDGE('',*,*,#16750,.F.);
#21717=ORIENTED_EDGE('',*,*,#16744,.F.);
#21718=ORIENTED_EDGE('',*,*,#16798,.T.);
#21719=ORIENTED_EDGE('',*,*,#16729,.F.);
#21720=ORIENTED_EDGE('',*,*,#16728,.F.);
#21721=ORIENTED_EDGE('',*,*,#16733,.F.);
#21722=ORIENTED_EDGE('',*,*,#16739,.F.);
#21723=ORIENTED_EDGE('',*,*,#16700,.F.);
#21724=ORIENTED_EDGE('',*,*,#16799,.F.);
#21725=ORIENTED_EDGE('',*,*,#16713,.F.);
#21726=ORIENTED_EDGE('',*,*,#16708,.F.);
#21727=ORIENTED_EDGE('',*,*,#16800,.T.);
#21728=ORIENTED_EDGE('',*,*,#16693,.F.);
#21729=ORIENTED_EDGE('',*,*,#16665,.F.);
#21730=ORIENTED_EDGE('',*,*,#16801,.F.);
#21731=ORIENTED_EDGE('',*,*,#16677,.F.);
#21732=ORIENTED_EDGE('',*,*,#16676,.F.);
#21733=ORIENTED_EDGE('',*,*,#16802,.T.);
#21734=ORIENTED_EDGE('',*,*,#16658,.F.);
#21735=ORIENTED_EDGE('',*,*,#16630,.F.);
#21736=ORIENTED_EDGE('',*,*,#16803,.F.);
#21737=ORIENTED_EDGE('',*,*,#16643,.F.);
#21738=ORIENTED_EDGE('',*,*,#16640,.F.);
#21739=ORIENTED_EDGE('',*,*,#16804,.T.);
#21740=ORIENTED_EDGE('',*,*,#16624,.F.);
#21741=ORIENTED_EDGE('',*,*,#16568,.F.);
#21742=ORIENTED_EDGE('',*,*,#16805,.F.);
#21743=ORIENTED_EDGE('',*,*,#16581,.F.);
#21744=ORIENTED_EDGE('',*,*,#16577,.F.);
#21745=ORIENTED_EDGE('',*,*,#16574,.F.);
#21746=ORIENTED_EDGE('',*,*,#16793,.T.);
#21747=ORIENTED_EDGE('',*,*,#16789,.T.);
#21748=ORIENTED_EDGE('',*,*,#16776,.F.);
#21749=ORIENTED_EDGE('',*,*,#16806,.F.);
#21750=ORIENTED_EDGE('',*,*,#16794,.T.);
#21751=ORIENTED_EDGE('',*,*,#16771,.F.);
#21752=ORIENTED_EDGE('',*,*,#16748,.F.);
#21753=ORIENTED_EDGE('',*,*,#16807,.F.);
#21754=ORIENTED_EDGE('',*,*,#16760,.F.);
#21755=ORIENTED_EDGE('',*,*,#16756,.F.);
#21756=ORIENTED_EDGE('',*,*,#16752,.F.);
#21757=ORIENTED_EDGE('',*,*,#16751,.F.);
#21758=ORIENTED_EDGE('',*,*,#16797,.T.);
#21759=ORIENTED_EDGE('',*,*,#16737,.F.);
#21760=ORIENTED_EDGE('',*,*,#16742,.F.);
#21761=ORIENTED_EDGE('',*,*,#16749,.F.);
#21762=ORIENTED_EDGE('',*,*,#16711,.F.);
#21763=ORIENTED_EDGE('',*,*,#16808,.F.);
#21764=ORIENTED_EDGE('',*,*,#16722,.F.);
#21765=ORIENTED_EDGE('',*,*,#16718,.F.);
#21766=ORIENTED_EDGE('',*,*,#16714,.F.);
#21767=ORIENTED_EDGE('',*,*,#16799,.T.);
#21768=ORIENTED_EDGE('',*,*,#16699,.F.);
#21769=ORIENTED_EDGE('',*,*,#16702,.F.);
#21770=ORIENTED_EDGE('',*,*,#16706,.F.);
#21771=ORIENTED_EDGE('',*,*,#16712,.F.);
#21772=ORIENTED_EDGE('',*,*,#16673,.F.);
#21773=ORIENTED_EDGE('',*,*,#16809,.F.);
#21774=ORIENTED_EDGE('',*,*,#16687,.F.);
#21775=ORIENTED_EDGE('',*,*,#16683,.F.);
#21776=ORIENTED_EDGE('',*,*,#16678,.F.);
#21777=ORIENTED_EDGE('',*,*,#16801,.T.);
#21778=ORIENTED_EDGE('',*,*,#16664,.F.);
#21779=ORIENTED_EDGE('',*,*,#16669,.F.);
#21780=ORIENTED_EDGE('',*,*,#16674,.F.);
#21781=ORIENTED_EDGE('',*,*,#16638,.F.);
#21782=ORIENTED_EDGE('',*,*,#16810,.F.);
#21783=ORIENTED_EDGE('',*,*,#16648,.F.);
#21784=ORIENTED_EDGE('',*,*,#16647,.F.);
#21785=ORIENTED_EDGE('',*,*,#16644,.F.);
#21786=ORIENTED_EDGE('',*,*,#16803,.T.);
#21787=ORIENTED_EDGE('',*,*,#16629,.F.);
#21788=ORIENTED_EDGE('',*,*,#16634,.F.);
#21789=ORIENTED_EDGE('',*,*,#16604,.F.);
#21790=ORIENTED_EDGE('',*,*,#16811,.F.);
#21791=ORIENTED_EDGE('',*,*,#16618,.F.);
#21792=ORIENTED_EDGE('',*,*,#16617,.F.);
#21793=ORIENTED_EDGE('',*,*,#16613,.F.);
#21794=ORIENTED_EDGE('',*,*,#16609,.F.);
#21795=ORIENTED_EDGE('',*,*,#16608,.F.);
#21796=ORIENTED_EDGE('',*,*,#16812,.T.);
#21797=ORIENTED_EDGE('',*,*,#16592,.F.);
#21798=ORIENTED_EDGE('',*,*,#16597,.F.);
#21799=ORIENTED_EDGE('',*,*,#16813,.F.);
#21800=ORIENTED_EDGE('',*,*,#16779,.F.);
#21801=ORIENTED_EDGE('',*,*,#16768,.F.);
#21802=ORIENTED_EDGE('',*,*,#16764,.F.);
#21803=ORIENTED_EDGE('',*,*,#16761,.F.);
#21804=ORIENTED_EDGE('',*,*,#16807,.T.);
#21805=ORIENTED_EDGE('',*,*,#16747,.F.);
#21806=ORIENTED_EDGE('',*,*,#16746,.F.);
#21807=ORIENTED_EDGE('',*,*,#16755,.F.);
#21808=ORIENTED_EDGE('',*,*,#16754,.F.);
#21809=ORIENTED_EDGE('',*,*,#16759,.F.);
#21810=ORIENTED_EDGE('',*,*,#16723,.F.);
#21811=ORIENTED_EDGE('',*,*,#16808,.T.);
#21812=ORIENTED_EDGE('',*,*,#16710,.F.);
#21813=ORIENTED_EDGE('',*,*,#16717,.F.);
#21814=ORIENTED_EDGE('',*,*,#16716,.F.);
#21815=ORIENTED_EDGE('',*,*,#16721,.F.);
#21816=ORIENTED_EDGE('',*,*,#16814,.F.);
#21817=ORIENTED_EDGE('',*,*,#16734,.F.);
#21818=ORIENTED_EDGE('',*,*,#16731,.F.);
#21819=ORIENTED_EDGE('',*,*,#16724,.F.);
#21820=ORIENTED_EDGE('',*,*,#16680,.F.);
#21821=ORIENTED_EDGE('',*,*,#16682,.F.);
#21822=ORIENTED_EDGE('',*,*,#16686,.F.);
#21823=ORIENTED_EDGE('',*,*,#16815,.F.);
#21824=ORIENTED_EDGE('',*,*,#16696,.F.);
#21825=ORIENTED_EDGE('',*,*,#16695,.F.);
#21826=ORIENTED_EDGE('',*,*,#16691,.F.);
#21827=ORIENTED_EDGE('',*,*,#16688,.F.);
#21828=ORIENTED_EDGE('',*,*,#16809,.T.);
#21829=ORIENTED_EDGE('',*,*,#16672,.F.);
#21830=ORIENTED_EDGE('',*,*,#16652,.F.);
#21831=ORIENTED_EDGE('',*,*,#16816,.F.);
#21832=ORIENTED_EDGE('',*,*,#16666,.F.);
#21833=ORIENTED_EDGE('',*,*,#16662,.F.);
#21834=ORIENTED_EDGE('',*,*,#16661,.F.);
#21835=ORIENTED_EDGE('',*,*,#16656,.F.);
#21836=ORIENTED_EDGE('',*,*,#16655,.F.);
#21837=ORIENTED_EDGE('',*,*,#16649,.F.);
#21838=ORIENTED_EDGE('',*,*,#16810,.T.);
#21839=ORIENTED_EDGE('',*,*,#16637,.F.);
#21840=ORIENTED_EDGE('',*,*,#16642,.F.);
#21841=ORIENTED_EDGE('',*,*,#16646,.F.);
#21842=ORIENTED_EDGE('',*,*,#16616,.F.);
#21843=ORIENTED_EDGE('',*,*,#16817,.F.);
#21844=ORIENTED_EDGE('',*,*,#16631,.F.);
#21845=ORIENTED_EDGE('',*,*,#16626,.F.);
#21846=ORIENTED_EDGE('',*,*,#16623,.F.);
#21847=ORIENTED_EDGE('',*,*,#16619,.F.);
#21848=ORIENTED_EDGE('',*,*,#16811,.T.);
#21849=ORIENTED_EDGE('',*,*,#16603,.F.);
#21850=ORIENTED_EDGE('',*,*,#16606,.F.);
#21851=ORIENTED_EDGE('',*,*,#16612,.F.);
#21852=ORIENTED_EDGE('',*,*,#16611,.F.);
#21853=ORIENTED_EDGE('',*,*,#16570,.F.);
#21854=ORIENTED_EDGE('',*,*,#16791,.T.);
#21855=ORIENTED_EDGE('',*,*,#16792,.F.);
#21856=ORIENTED_EDGE('',*,*,#16564,.F.);
#21857=ORIENTED_EDGE('',*,*,#16778,.F.);
#21858=ORIENTED_EDGE('',*,*,#16796,.F.);
#21859=ORIENTED_EDGE('',*,*,#16818,.F.);
#21860=ORIENTED_EDGE('',*,*,#16774,.F.);
#21861=ORIENTED_EDGE('',*,*,#16782,.F.);
#21862=ORIENTED_EDGE('',*,*,#16781,.F.);
#21863=ORIENTED_EDGE('',*,*,#16780,.T.);
#21864=ORIENTED_EDGE('',*,*,#16813,.T.);
#21865=ORIENTED_EDGE('',*,*,#16758,.F.);
#21866=ORIENTED_EDGE('',*,*,#16763,.F.);
#21867=ORIENTED_EDGE('',*,*,#16767,.F.);
#21868=ORIENTED_EDGE('',*,*,#16766,.F.);
#21869=ORIENTED_EDGE('',*,*,#16730,.F.);
#21870=ORIENTED_EDGE('',*,*,#16798,.F.);
#21871=ORIENTED_EDGE('',*,*,#16743,.F.);
#21872=ORIENTED_EDGE('',*,*,#16740,.F.);
#21873=ORIENTED_EDGE('',*,*,#16735,.F.);
#21874=ORIENTED_EDGE('',*,*,#16814,.T.);
#21875=ORIENTED_EDGE('',*,*,#16720,.F.);
#21876=ORIENTED_EDGE('',*,*,#16726,.F.);
#21877=ORIENTED_EDGE('',*,*,#16694,.F.);
#21878=ORIENTED_EDGE('',*,*,#16800,.F.);
#21879=ORIENTED_EDGE('',*,*,#16707,.F.);
#21880=ORIENTED_EDGE('',*,*,#16704,.F.);
#21881=ORIENTED_EDGE('',*,*,#16703,.F.);
#21882=ORIENTED_EDGE('',*,*,#16697,.F.);
#21883=ORIENTED_EDGE('',*,*,#16815,.T.);
#21884=ORIENTED_EDGE('',*,*,#16685,.F.);
#21885=ORIENTED_EDGE('',*,*,#16690,.F.);
#21886=ORIENTED_EDGE('',*,*,#16659,.F.);
#21887=ORIENTED_EDGE('',*,*,#16802,.F.);
#21888=ORIENTED_EDGE('',*,*,#16675,.F.);
#21889=ORIENTED_EDGE('',*,*,#16670,.F.);
#21890=ORIENTED_EDGE('',*,*,#16667,.F.);
#21891=ORIENTED_EDGE('',*,*,#16816,.T.);
#21892=ORIENTED_EDGE('',*,*,#16651,.F.);
#21893=ORIENTED_EDGE('',*,*,#16654,.F.);
#21894=ORIENTED_EDGE('',*,*,#16660,.F.);
#21895=ORIENTED_EDGE('',*,*,#16635,.F.);
#21896=ORIENTED_EDGE('',*,*,#16632,.F.);
#21897=ORIENTED_EDGE('',*,*,#16817,.T.);
#21898=ORIENTED_EDGE('',*,*,#16615,.F.);
#21899=ORIENTED_EDGE('',*,*,#16622,.F.);
#21900=ORIENTED_EDGE('',*,*,#16621,.F.);
#21901=ORIENTED_EDGE('',*,*,#16625,.F.);
#21902=ORIENTED_EDGE('',*,*,#16804,.F.);
#21903=ORIENTED_EDGE('',*,*,#16639,.F.);
#21904=ORIENTED_EDGE('',*,*,#16593,.F.);
#21905=ORIENTED_EDGE('',*,*,#16812,.F.);
#21906=ORIENTED_EDGE('',*,*,#16607,.F.);
#21907=ORIENTED_EDGE('',*,*,#16601,.F.);
#21908=ORIENTED_EDGE('',*,*,#16819,.T.);
#21909=ORIENTED_EDGE('',*,*,#16588,.F.);
#21910=ORIENTED_EDGE('',*,*,#16589,.F.);
#21911=ORIENTED_EDGE('',*,*,#16819,.F.);
#21912=ORIENTED_EDGE('',*,*,#16600,.F.);
#21913=ORIENTED_EDGE('',*,*,#16599,.F.);
#21914=ORIENTED_EDGE('',*,*,#16598,.F.);
#21915=ORIENTED_EDGE('',*,*,#16595,.F.);
#21916=ORIENTED_EDGE('',*,*,#16820,.T.);
#21917=ORIENTED_EDGE('',*,*,#16579,.F.);
#21918=ORIENTED_EDGE('',*,*,#16585,.F.);
#21919=ORIENTED_EDGE('',*,*,#16584,.F.);
#21920=ORIENTED_EDGE('',*,*,#16580,.F.);
#21921=ORIENTED_EDGE('',*,*,#16820,.F.);
#21922=ORIENTED_EDGE('',*,*,#16594,.F.);
#21923=ORIENTED_EDGE('',*,*,#16590,.F.);
#21924=ORIENTED_EDGE('',*,*,#16586,.F.);
#21925=ORIENTED_EDGE('',*,*,#16582,.F.);
#21926=ORIENTED_EDGE('',*,*,#16805,.T.);
#21927=ORIENTED_EDGE('',*,*,#16567,.F.);
#21928=ORIENTED_EDGE('',*,*,#16572,.F.);
#21929=ORIENTED_EDGE('',*,*,#16576,.F.);
#21930=ORIENTED_EDGE('',*,*,#16775,.F.);
#21931=ORIENTED_EDGE('',*,*,#16818,.T.);
#21932=ORIENTED_EDGE('',*,*,#16795,.T.);
#21933=ORIENTED_EDGE('',*,*,#16806,.T.);
#21934=ORIENTED_EDGE('',*,*,#16821,.F.);
#21935=ORIENTED_EDGE('',*,*,#16822,.F.);
#21936=ORIENTED_EDGE('',*,*,#16823,.T.);
#21937=ORIENTED_EDGE('',*,*,#16821,.T.);
#21938=ORIENTED_EDGE('',*,*,#16823,.F.);
#21939=ORIENTED_EDGE('',*,*,#16824,.F.);
#21940=ORIENTED_EDGE('',*,*,#16825,.T.);
#21941=ORIENTED_EDGE('',*,*,#16822,.T.);
#21942=ORIENTED_EDGE('',*,*,#16825,.F.);
#21943=ORIENTED_EDGE('',*,*,#16785,.T.);
#21944=ORIENTED_EDGE('',*,*,#16787,.T.);
#21945=ORIENTED_EDGE('',*,*,#16783,.T.);
#21946=ORIENTED_EDGE('',*,*,#16788,.T.);
#21947=ORIENTED_EDGE('',*,*,#16563,.F.);
#21948=ORIENTED_EDGE('',*,*,#16824,.T.);
#21949=ORIENTED_EDGE('',*,*,#16769,.T.);
#21950=ORIENTED_EDGE('',*,*,#16826,.T.);
#21951=ORIENTED_EDGE('',*,*,#16827,.F.);
#21952=ORIENTED_EDGE('',*,*,#16826,.F.);
#21953=ORIENTED_EDGE('',*,*,#16827,.T.);
#21954=ORIENTED_EDGE('',*,*,#16828,.F.);
#21955=ORIENTED_EDGE('',*,*,#16829,.F.);
#21956=ORIENTED_EDGE('',*,*,#16830,.T.);
#21957=ORIENTED_EDGE('',*,*,#16828,.T.);
#21958=ORIENTED_EDGE('',*,*,#16830,.F.);
#21959=ORIENTED_EDGE('',*,*,#16829,.T.);
#21960=ORIENTED_EDGE('',*,*,#16831,.T.);
#21961=ORIENTED_EDGE('',*,*,#16832,.F.);
#21962=ORIENTED_EDGE('',*,*,#16831,.F.);
#21963=ORIENTED_EDGE('',*,*,#16832,.T.);
#21964=ORIENTED_EDGE('',*,*,#16833,.F.);
#21965=ORIENTED_EDGE('',*,*,#16834,.F.);
#21966=ORIENTED_EDGE('',*,*,#16835,.F.);
#21967=ORIENTED_EDGE('',*,*,#16836,.F.);
#21968=ORIENTED_EDGE('',*,*,#16837,.F.);
#21969=ORIENTED_EDGE('',*,*,#16838,.F.);
#21970=ORIENTED_EDGE('',*,*,#16839,.F.);
#21971=ORIENTED_EDGE('',*,*,#16840,.F.);
#21972=ORIENTED_EDGE('',*,*,#16841,.F.);
#21973=ORIENTED_EDGE('',*,*,#16842,.F.);
#21974=ORIENTED_EDGE('',*,*,#16843,.F.);
#21975=ORIENTED_EDGE('',*,*,#16844,.F.);
#21976=ORIENTED_EDGE('',*,*,#16845,.F.);
#21977=ORIENTED_EDGE('',*,*,#16846,.F.);
#21978=ORIENTED_EDGE('',*,*,#16847,.F.);
#21979=ORIENTED_EDGE('',*,*,#16848,.F.);
#21980=ORIENTED_EDGE('',*,*,#16849,.F.);
#21981=ORIENTED_EDGE('',*,*,#16850,.F.);
#21982=ORIENTED_EDGE('',*,*,#16851,.F.);
#21983=ORIENTED_EDGE('',*,*,#16852,.T.);
#21984=ORIENTED_EDGE('',*,*,#16853,.F.);
#21985=ORIENTED_EDGE('',*,*,#16854,.F.);
#21986=ORIENTED_EDGE('',*,*,#16852,.F.);
#21987=ORIENTED_EDGE('',*,*,#16834,.T.);
#21988=ORIENTED_EDGE('',*,*,#16855,.F.);
#21989=ORIENTED_EDGE('',*,*,#16856,.T.);
#21990=ORIENTED_EDGE('',*,*,#16857,.T.);
#21991=ORIENTED_EDGE('',*,*,#16835,.T.);
#21992=ORIENTED_EDGE('',*,*,#16857,.F.);
#21993=ORIENTED_EDGE('',*,*,#16858,.T.);
#21994=ORIENTED_EDGE('',*,*,#16859,.F.);
#21995=ORIENTED_EDGE('',*,*,#16841,.T.);
#21996=ORIENTED_EDGE('',*,*,#16860,.F.);
#21997=ORIENTED_EDGE('',*,*,#16861,.T.);
#21998=ORIENTED_EDGE('',*,*,#16862,.F.);
#21999=ORIENTED_EDGE('',*,*,#16843,.T.);
#22000=ORIENTED_EDGE('',*,*,#16863,.F.);
#22001=ORIENTED_EDGE('',*,*,#16864,.T.);
#22002=ORIENTED_EDGE('',*,*,#16865,.F.);
#22003=ORIENTED_EDGE('',*,*,#16840,.T.);
#22004=ORIENTED_EDGE('',*,*,#16866,.F.);
#22005=ORIENTED_EDGE('',*,*,#16867,.T.);
#22006=ORIENTED_EDGE('',*,*,#16860,.T.);
#22007=ORIENTED_EDGE('',*,*,#16844,.T.);
#22008=ORIENTED_EDGE('',*,*,#16865,.T.);
#22009=ORIENTED_EDGE('',*,*,#16868,.T.);
#22010=ORIENTED_EDGE('',*,*,#16869,.F.);
#22011=ORIENTED_EDGE('',*,*,#16837,.T.);
#22012=ORIENTED_EDGE('',*,*,#16870,.F.);
#22013=ORIENTED_EDGE('',*,*,#16871,.T.);
#22014=ORIENTED_EDGE('',*,*,#16872,.T.);
#22015=ORIENTED_EDGE('',*,*,#16847,.T.);
#22016=ORIENTED_EDGE('',*,*,#16873,.T.);
#22017=ORIENTED_EDGE('',*,*,#16874,.T.);
#22018=ORIENTED_EDGE('',*,*,#16875,.F.);
#22019=ORIENTED_EDGE('',*,*,#16838,.T.);
#22020=ORIENTED_EDGE('',*,*,#16872,.F.);
#22021=ORIENTED_EDGE('',*,*,#16876,.T.);
#22022=ORIENTED_EDGE('',*,*,#16877,.F.);
#22023=ORIENTED_EDGE('',*,*,#16846,.T.);
#22024=ORIENTED_EDGE('',*,*,#16878,.F.);
#22025=ORIENTED_EDGE('',*,*,#16879,.T.);
#22026=ORIENTED_EDGE('',*,*,#16873,.F.);
#22027=ORIENTED_EDGE('',*,*,#16880,.F.);
#22028=ORIENTED_EDGE('',*,*,#16861,.F.);
#22029=ORIENTED_EDGE('',*,*,#16867,.F.);
#22030=ORIENTED_EDGE('',*,*,#16881,.F.);
#22031=ORIENTED_EDGE('',*,*,#16868,.F.);
#22032=ORIENTED_EDGE('',*,*,#16864,.F.);
#22033=ORIENTED_EDGE('',*,*,#16882,.F.);
#22034=ORIENTED_EDGE('',*,*,#16883,.T.);
#22035=ORIENTED_EDGE('',*,*,#16884,.F.);
#22036=ORIENTED_EDGE('',*,*,#16885,.T.);
#22037=ORIENTED_EDGE('',*,*,#16886,.F.);
#22038=ORIENTED_EDGE('',*,*,#16885,.F.);
#22039=ORIENTED_EDGE('',*,*,#16887,.F.);
#22040=ORIENTED_EDGE('',*,*,#16888,.F.);
#22041=ORIENTED_EDGE('',*,*,#16887,.T.);
#22042=ORIENTED_EDGE('',*,*,#16884,.T.);
#22043=ORIENTED_EDGE('',*,*,#16889,.T.);
#22044=ORIENTED_EDGE('',*,*,#16890,.F.);
#22045=ORIENTED_EDGE('',*,*,#16889,.F.);
#22046=ORIENTED_EDGE('',*,*,#16883,.F.);
#22047=ORIENTED_EDGE('',*,*,#16891,.F.);
#22048=ORIENTED_EDGE('',*,*,#16892,.T.);
#22049=ORIENTED_EDGE('',*,*,#16893,.F.);
#22050=ORIENTED_EDGE('',*,*,#16894,.T.);
#22051=ORIENTED_EDGE('',*,*,#16895,.F.);
#22052=ORIENTED_EDGE('',*,*,#16894,.F.);
#22053=ORIENTED_EDGE('',*,*,#16896,.F.);
#22054=ORIENTED_EDGE('',*,*,#16897,.F.);
#22055=ORIENTED_EDGE('',*,*,#16896,.T.);
#22056=ORIENTED_EDGE('',*,*,#16893,.T.);
#22057=ORIENTED_EDGE('',*,*,#16898,.T.);
#22058=ORIENTED_EDGE('',*,*,#16899,.F.);
#22059=ORIENTED_EDGE('',*,*,#16898,.F.);
#22060=ORIENTED_EDGE('',*,*,#16892,.F.);
#22061=ORIENTED_EDGE('',*,*,#16900,.F.);
#22062=ORIENTED_EDGE('',*,*,#16901,.T.);
#22063=ORIENTED_EDGE('',*,*,#16902,.F.);
#22064=ORIENTED_EDGE('',*,*,#16903,.T.);
#22065=ORIENTED_EDGE('',*,*,#16904,.F.);
#22066=ORIENTED_EDGE('',*,*,#16903,.F.);
#22067=ORIENTED_EDGE('',*,*,#16905,.F.);
#22068=ORIENTED_EDGE('',*,*,#16906,.F.);
#22069=ORIENTED_EDGE('',*,*,#16905,.T.);
#22070=ORIENTED_EDGE('',*,*,#16902,.T.);
#22071=ORIENTED_EDGE('',*,*,#16907,.T.);
#22072=ORIENTED_EDGE('',*,*,#16908,.F.);
#22073=ORIENTED_EDGE('',*,*,#16907,.F.);
#22074=ORIENTED_EDGE('',*,*,#16901,.F.);
#22075=ORIENTED_EDGE('',*,*,#16909,.F.);
#22076=ORIENTED_EDGE('',*,*,#16910,.T.);
#22077=ORIENTED_EDGE('',*,*,#16911,.F.);
#22078=ORIENTED_EDGE('',*,*,#16912,.T.);
#22079=ORIENTED_EDGE('',*,*,#16913,.F.);
#22080=ORIENTED_EDGE('',*,*,#16912,.F.);
#22081=ORIENTED_EDGE('',*,*,#16914,.F.);
#22082=ORIENTED_EDGE('',*,*,#16915,.F.);
#22083=ORIENTED_EDGE('',*,*,#16914,.T.);
#22084=ORIENTED_EDGE('',*,*,#16911,.T.);
#22085=ORIENTED_EDGE('',*,*,#16916,.T.);
#22086=ORIENTED_EDGE('',*,*,#16917,.F.);
#22087=ORIENTED_EDGE('',*,*,#16916,.F.);
#22088=ORIENTED_EDGE('',*,*,#16910,.F.);
#22089=ORIENTED_EDGE('',*,*,#16918,.F.);
#22090=ORIENTED_EDGE('',*,*,#16919,.T.);
#22091=ORIENTED_EDGE('',*,*,#16920,.F.);
#22092=ORIENTED_EDGE('',*,*,#16921,.T.);
#22093=ORIENTED_EDGE('',*,*,#16922,.F.);
#22094=ORIENTED_EDGE('',*,*,#16921,.F.);
#22095=ORIENTED_EDGE('',*,*,#16923,.F.);
#22096=ORIENTED_EDGE('',*,*,#16924,.F.);
#22097=ORIENTED_EDGE('',*,*,#16923,.T.);
#22098=ORIENTED_EDGE('',*,*,#16920,.T.);
#22099=ORIENTED_EDGE('',*,*,#16925,.T.);
#22100=ORIENTED_EDGE('',*,*,#16926,.F.);
#22101=ORIENTED_EDGE('',*,*,#16925,.F.);
#22102=ORIENTED_EDGE('',*,*,#16919,.F.);
#22103=ORIENTED_EDGE('',*,*,#16927,.F.);
#22104=ORIENTED_EDGE('',*,*,#16928,.T.);
#22105=ORIENTED_EDGE('',*,*,#16929,.F.);
#22106=ORIENTED_EDGE('',*,*,#16930,.T.);
#22107=ORIENTED_EDGE('',*,*,#16931,.F.);
#22108=ORIENTED_EDGE('',*,*,#16930,.F.);
#22109=ORIENTED_EDGE('',*,*,#16932,.F.);
#22110=ORIENTED_EDGE('',*,*,#16933,.F.);
#22111=ORIENTED_EDGE('',*,*,#16932,.T.);
#22112=ORIENTED_EDGE('',*,*,#16929,.T.);
#22113=ORIENTED_EDGE('',*,*,#16934,.T.);
#22114=ORIENTED_EDGE('',*,*,#16935,.F.);
#22115=ORIENTED_EDGE('',*,*,#16934,.F.);
#22116=ORIENTED_EDGE('',*,*,#16928,.F.);
#22117=ORIENTED_EDGE('',*,*,#16936,.F.);
#22118=ORIENTED_EDGE('',*,*,#16937,.T.);
#22119=ORIENTED_EDGE('',*,*,#16938,.F.);
#22120=ORIENTED_EDGE('',*,*,#16939,.T.);
#22121=ORIENTED_EDGE('',*,*,#16940,.F.);
#22122=ORIENTED_EDGE('',*,*,#16939,.F.);
#22123=ORIENTED_EDGE('',*,*,#16941,.F.);
#22124=ORIENTED_EDGE('',*,*,#16942,.F.);
#22125=ORIENTED_EDGE('',*,*,#16941,.T.);
#22126=ORIENTED_EDGE('',*,*,#16938,.T.);
#22127=ORIENTED_EDGE('',*,*,#16943,.T.);
#22128=ORIENTED_EDGE('',*,*,#16944,.F.);
#22129=ORIENTED_EDGE('',*,*,#16943,.F.);
#22130=ORIENTED_EDGE('',*,*,#16937,.F.);
#22131=ORIENTED_EDGE('',*,*,#16945,.F.);
#22132=ORIENTED_EDGE('',*,*,#16946,.T.);
#22133=ORIENTED_EDGE('',*,*,#16947,.F.);
#22134=ORIENTED_EDGE('',*,*,#16948,.T.);
#22135=ORIENTED_EDGE('',*,*,#16949,.F.);
#22136=ORIENTED_EDGE('',*,*,#16948,.F.);
#22137=ORIENTED_EDGE('',*,*,#16950,.F.);
#22138=ORIENTED_EDGE('',*,*,#16951,.F.);
#22139=ORIENTED_EDGE('',*,*,#16950,.T.);
#22140=ORIENTED_EDGE('',*,*,#16947,.T.);
#22141=ORIENTED_EDGE('',*,*,#16952,.T.);
#22142=ORIENTED_EDGE('',*,*,#16953,.F.);
#22143=ORIENTED_EDGE('',*,*,#16952,.F.);
#22144=ORIENTED_EDGE('',*,*,#16946,.F.);
#22145=ORIENTED_EDGE('',*,*,#16954,.F.);
#22146=ORIENTED_EDGE('',*,*,#16955,.T.);
#22147=ORIENTED_EDGE('',*,*,#16956,.F.);
#22148=ORIENTED_EDGE('',*,*,#16957,.T.);
#22149=ORIENTED_EDGE('',*,*,#16958,.F.);
#22150=ORIENTED_EDGE('',*,*,#16957,.F.);
#22151=ORIENTED_EDGE('',*,*,#16959,.F.);
#22152=ORIENTED_EDGE('',*,*,#16960,.F.);
#22153=ORIENTED_EDGE('',*,*,#16959,.T.);
#22154=ORIENTED_EDGE('',*,*,#16956,.T.);
#22155=ORIENTED_EDGE('',*,*,#16961,.T.);
#22156=ORIENTED_EDGE('',*,*,#16962,.F.);
#22157=ORIENTED_EDGE('',*,*,#16961,.F.);
#22158=ORIENTED_EDGE('',*,*,#16955,.F.);
#22159=ORIENTED_EDGE('',*,*,#16963,.F.);
#22160=ORIENTED_EDGE('',*,*,#16964,.T.);
#22161=ORIENTED_EDGE('',*,*,#16965,.F.);
#22162=ORIENTED_EDGE('',*,*,#16966,.T.);
#22163=ORIENTED_EDGE('',*,*,#16967,.F.);
#22164=ORIENTED_EDGE('',*,*,#16966,.F.);
#22165=ORIENTED_EDGE('',*,*,#16968,.F.);
#22166=ORIENTED_EDGE('',*,*,#16969,.F.);
#22167=ORIENTED_EDGE('',*,*,#16968,.T.);
#22168=ORIENTED_EDGE('',*,*,#16965,.T.);
#22169=ORIENTED_EDGE('',*,*,#16970,.T.);
#22170=ORIENTED_EDGE('',*,*,#16971,.F.);
#22171=ORIENTED_EDGE('',*,*,#16970,.F.);
#22172=ORIENTED_EDGE('',*,*,#16964,.F.);
#22173=ORIENTED_EDGE('',*,*,#16972,.F.);
#22174=ORIENTED_EDGE('',*,*,#16973,.T.);
#22175=ORIENTED_EDGE('',*,*,#16974,.F.);
#22176=ORIENTED_EDGE('',*,*,#16975,.T.);
#22177=ORIENTED_EDGE('',*,*,#16976,.F.);
#22178=ORIENTED_EDGE('',*,*,#16975,.F.);
#22179=ORIENTED_EDGE('',*,*,#16977,.F.);
#22180=ORIENTED_EDGE('',*,*,#16978,.F.);
#22181=ORIENTED_EDGE('',*,*,#16977,.T.);
#22182=ORIENTED_EDGE('',*,*,#16974,.T.);
#22183=ORIENTED_EDGE('',*,*,#16979,.T.);
#22184=ORIENTED_EDGE('',*,*,#16980,.F.);
#22185=ORIENTED_EDGE('',*,*,#16979,.F.);
#22186=ORIENTED_EDGE('',*,*,#16973,.F.);
#22187=ORIENTED_EDGE('',*,*,#16981,.F.);
#22188=ORIENTED_EDGE('',*,*,#16982,.T.);
#22189=ORIENTED_EDGE('',*,*,#16983,.F.);
#22190=ORIENTED_EDGE('',*,*,#16984,.T.);
#22191=ORIENTED_EDGE('',*,*,#16985,.F.);
#22192=ORIENTED_EDGE('',*,*,#16984,.F.);
#22193=ORIENTED_EDGE('',*,*,#16986,.F.);
#22194=ORIENTED_EDGE('',*,*,#16987,.F.);
#22195=ORIENTED_EDGE('',*,*,#16986,.T.);
#22196=ORIENTED_EDGE('',*,*,#16983,.T.);
#22197=ORIENTED_EDGE('',*,*,#16988,.T.);
#22198=ORIENTED_EDGE('',*,*,#16989,.F.);
#22199=ORIENTED_EDGE('',*,*,#16988,.F.);
#22200=ORIENTED_EDGE('',*,*,#16982,.F.);
#22201=ORIENTED_EDGE('',*,*,#16990,.F.);
#22202=ORIENTED_EDGE('',*,*,#16991,.T.);
#22203=ORIENTED_EDGE('',*,*,#16992,.F.);
#22204=ORIENTED_EDGE('',*,*,#16993,.T.);
#22205=ORIENTED_EDGE('',*,*,#16994,.F.);
#22206=ORIENTED_EDGE('',*,*,#16993,.F.);
#22207=ORIENTED_EDGE('',*,*,#16995,.F.);
#22208=ORIENTED_EDGE('',*,*,#16996,.F.);
#22209=ORIENTED_EDGE('',*,*,#16995,.T.);
#22210=ORIENTED_EDGE('',*,*,#16992,.T.);
#22211=ORIENTED_EDGE('',*,*,#16997,.T.);
#22212=ORIENTED_EDGE('',*,*,#16998,.F.);
#22213=ORIENTED_EDGE('',*,*,#16997,.F.);
#22214=ORIENTED_EDGE('',*,*,#16991,.F.);
#22215=ORIENTED_EDGE('',*,*,#16999,.F.);
#22216=ORIENTED_EDGE('',*,*,#17000,.T.);
#22217=ORIENTED_EDGE('',*,*,#17001,.F.);
#22218=ORIENTED_EDGE('',*,*,#17002,.T.);
#22219=ORIENTED_EDGE('',*,*,#17003,.F.);
#22220=ORIENTED_EDGE('',*,*,#17002,.F.);
#22221=ORIENTED_EDGE('',*,*,#17004,.F.);
#22222=ORIENTED_EDGE('',*,*,#17005,.F.);
#22223=ORIENTED_EDGE('',*,*,#17004,.T.);
#22224=ORIENTED_EDGE('',*,*,#17001,.T.);
#22225=ORIENTED_EDGE('',*,*,#17006,.T.);
#22226=ORIENTED_EDGE('',*,*,#17007,.F.);
#22227=ORIENTED_EDGE('',*,*,#17006,.F.);
#22228=ORIENTED_EDGE('',*,*,#17000,.F.);
#22229=ORIENTED_EDGE('',*,*,#17008,.F.);
#22230=ORIENTED_EDGE('',*,*,#17009,.T.);
#22231=ORIENTED_EDGE('',*,*,#17010,.F.);
#22232=ORIENTED_EDGE('',*,*,#17011,.T.);
#22233=ORIENTED_EDGE('',*,*,#17012,.F.);
#22234=ORIENTED_EDGE('',*,*,#17011,.F.);
#22235=ORIENTED_EDGE('',*,*,#17013,.F.);
#22236=ORIENTED_EDGE('',*,*,#17014,.F.);
#22237=ORIENTED_EDGE('',*,*,#17013,.T.);
#22238=ORIENTED_EDGE('',*,*,#17010,.T.);
#22239=ORIENTED_EDGE('',*,*,#17015,.T.);
#22240=ORIENTED_EDGE('',*,*,#17016,.F.);
#22241=ORIENTED_EDGE('',*,*,#17015,.F.);
#22242=ORIENTED_EDGE('',*,*,#17009,.F.);
#22243=ORIENTED_EDGE('',*,*,#17017,.F.);
#22244=ORIENTED_EDGE('',*,*,#17018,.T.);
#22245=ORIENTED_EDGE('',*,*,#17019,.F.);
#22246=ORIENTED_EDGE('',*,*,#17020,.T.);
#22247=ORIENTED_EDGE('',*,*,#17021,.F.);
#22248=ORIENTED_EDGE('',*,*,#17020,.F.);
#22249=ORIENTED_EDGE('',*,*,#17022,.F.);
#22250=ORIENTED_EDGE('',*,*,#17023,.F.);
#22251=ORIENTED_EDGE('',*,*,#17022,.T.);
#22252=ORIENTED_EDGE('',*,*,#17019,.T.);
#22253=ORIENTED_EDGE('',*,*,#17024,.T.);
#22254=ORIENTED_EDGE('',*,*,#17025,.F.);
#22255=ORIENTED_EDGE('',*,*,#17024,.F.);
#22256=ORIENTED_EDGE('',*,*,#17018,.F.);
#22257=ORIENTED_EDGE('',*,*,#17026,.F.);
#22258=ORIENTED_EDGE('',*,*,#17027,.T.);
#22259=ORIENTED_EDGE('',*,*,#17028,.F.);
#22260=ORIENTED_EDGE('',*,*,#17029,.T.);
#22261=ORIENTED_EDGE('',*,*,#17030,.F.);
#22262=ORIENTED_EDGE('',*,*,#17029,.F.);
#22263=ORIENTED_EDGE('',*,*,#17031,.F.);
#22264=ORIENTED_EDGE('',*,*,#17032,.F.);
#22265=ORIENTED_EDGE('',*,*,#17031,.T.);
#22266=ORIENTED_EDGE('',*,*,#17028,.T.);
#22267=ORIENTED_EDGE('',*,*,#17033,.T.);
#22268=ORIENTED_EDGE('',*,*,#17034,.F.);
#22269=ORIENTED_EDGE('',*,*,#17033,.F.);
#22270=ORIENTED_EDGE('',*,*,#17027,.F.);
#22271=ORIENTED_EDGE('',*,*,#17035,.F.);
#22272=ORIENTED_EDGE('',*,*,#17036,.T.);
#22273=ORIENTED_EDGE('',*,*,#17037,.F.);
#22274=ORIENTED_EDGE('',*,*,#17038,.T.);
#22275=ORIENTED_EDGE('',*,*,#17039,.F.);
#22276=ORIENTED_EDGE('',*,*,#17038,.F.);
#22277=ORIENTED_EDGE('',*,*,#17040,.F.);
#22278=ORIENTED_EDGE('',*,*,#17041,.F.);
#22279=ORIENTED_EDGE('',*,*,#17040,.T.);
#22280=ORIENTED_EDGE('',*,*,#17037,.T.);
#22281=ORIENTED_EDGE('',*,*,#17042,.T.);
#22282=ORIENTED_EDGE('',*,*,#17043,.F.);
#22283=ORIENTED_EDGE('',*,*,#17042,.F.);
#22284=ORIENTED_EDGE('',*,*,#17036,.F.);
#22285=ORIENTED_EDGE('',*,*,#17044,.F.);
#22286=ORIENTED_EDGE('',*,*,#17045,.T.);
#22287=ORIENTED_EDGE('',*,*,#17046,.F.);
#22288=ORIENTED_EDGE('',*,*,#17047,.T.);
#22289=ORIENTED_EDGE('',*,*,#17048,.F.);
#22290=ORIENTED_EDGE('',*,*,#17047,.F.);
#22291=ORIENTED_EDGE('',*,*,#17049,.F.);
#22292=ORIENTED_EDGE('',*,*,#17050,.F.);
#22293=ORIENTED_EDGE('',*,*,#17051,.F.);
#22294=ORIENTED_EDGE('',*,*,#17049,.T.);
#22295=ORIENTED_EDGE('',*,*,#17046,.T.);
#22296=ORIENTED_EDGE('',*,*,#17052,.T.);
#22297=ORIENTED_EDGE('',*,*,#17053,.F.);
#22298=ORIENTED_EDGE('',*,*,#17052,.F.);
#22299=ORIENTED_EDGE('',*,*,#17045,.F.);
#22300=ORIENTED_EDGE('',*,*,#17054,.F.);
#22301=ORIENTED_EDGE('',*,*,#17055,.F.);
#22302=ORIENTED_EDGE('',*,*,#17056,.T.);
#22303=ORIENTED_EDGE('',*,*,#17057,.F.);
#22304=ORIENTED_EDGE('',*,*,#17058,.T.);
#22305=ORIENTED_EDGE('',*,*,#17059,.F.);
#22306=ORIENTED_EDGE('',*,*,#17058,.F.);
#22307=ORIENTED_EDGE('',*,*,#17060,.F.);
#22308=ORIENTED_EDGE('',*,*,#17061,.F.);
#22309=ORIENTED_EDGE('',*,*,#17060,.T.);
#22310=ORIENTED_EDGE('',*,*,#17057,.T.);
#22311=ORIENTED_EDGE('',*,*,#17062,.T.);
#22312=ORIENTED_EDGE('',*,*,#17063,.F.);
#22313=ORIENTED_EDGE('',*,*,#17062,.F.);
#22314=ORIENTED_EDGE('',*,*,#17056,.F.);
#22315=ORIENTED_EDGE('',*,*,#17064,.F.);
#22316=ORIENTED_EDGE('',*,*,#17065,.T.);
#22317=ORIENTED_EDGE('',*,*,#17066,.F.);
#22318=ORIENTED_EDGE('',*,*,#17067,.T.);
#22319=ORIENTED_EDGE('',*,*,#17068,.F.);
#22320=ORIENTED_EDGE('',*,*,#17067,.F.);
#22321=ORIENTED_EDGE('',*,*,#17069,.F.);
#22322=ORIENTED_EDGE('',*,*,#17070,.F.);
#22323=ORIENTED_EDGE('',*,*,#17069,.T.);
#22324=ORIENTED_EDGE('',*,*,#17066,.T.);
#22325=ORIENTED_EDGE('',*,*,#17071,.T.);
#22326=ORIENTED_EDGE('',*,*,#17072,.F.);
#22327=ORIENTED_EDGE('',*,*,#17071,.F.);
#22328=ORIENTED_EDGE('',*,*,#17065,.F.);
#22329=ORIENTED_EDGE('',*,*,#17073,.F.);
#22330=ORIENTED_EDGE('',*,*,#17074,.T.);
#22331=ORIENTED_EDGE('',*,*,#17075,.F.);
#22332=ORIENTED_EDGE('',*,*,#17076,.T.);
#22333=ORIENTED_EDGE('',*,*,#17077,.F.);
#22334=ORIENTED_EDGE('',*,*,#17076,.F.);
#22335=ORIENTED_EDGE('',*,*,#17078,.F.);
#22336=ORIENTED_EDGE('',*,*,#17079,.F.);
#22337=ORIENTED_EDGE('',*,*,#17078,.T.);
#22338=ORIENTED_EDGE('',*,*,#17075,.T.);
#22339=ORIENTED_EDGE('',*,*,#17080,.T.);
#22340=ORIENTED_EDGE('',*,*,#17081,.F.);
#22341=ORIENTED_EDGE('',*,*,#17080,.F.);
#22342=ORIENTED_EDGE('',*,*,#17074,.F.);
#22343=ORIENTED_EDGE('',*,*,#17082,.F.);
#22344=ORIENTED_EDGE('',*,*,#17083,.T.);
#22345=ORIENTED_EDGE('',*,*,#17084,.F.);
#22346=ORIENTED_EDGE('',*,*,#17085,.T.);
#22347=ORIENTED_EDGE('',*,*,#17086,.F.);
#22348=ORIENTED_EDGE('',*,*,#17085,.F.);
#22349=ORIENTED_EDGE('',*,*,#17087,.F.);
#22350=ORIENTED_EDGE('',*,*,#17088,.F.);
#22351=ORIENTED_EDGE('',*,*,#17087,.T.);
#22352=ORIENTED_EDGE('',*,*,#17084,.T.);
#22353=ORIENTED_EDGE('',*,*,#17089,.T.);
#22354=ORIENTED_EDGE('',*,*,#17090,.F.);
#22355=ORIENTED_EDGE('',*,*,#17089,.F.);
#22356=ORIENTED_EDGE('',*,*,#17083,.F.);
#22357=ORIENTED_EDGE('',*,*,#17091,.F.);
#22358=ORIENTED_EDGE('',*,*,#17092,.T.);
#22359=ORIENTED_EDGE('',*,*,#17093,.F.);
#22360=ORIENTED_EDGE('',*,*,#17094,.T.);
#22361=ORIENTED_EDGE('',*,*,#17095,.F.);
#22362=ORIENTED_EDGE('',*,*,#17094,.F.);
#22363=ORIENTED_EDGE('',*,*,#17096,.F.);
#22364=ORIENTED_EDGE('',*,*,#17097,.F.);
#22365=ORIENTED_EDGE('',*,*,#17096,.T.);
#22366=ORIENTED_EDGE('',*,*,#17093,.T.);
#22367=ORIENTED_EDGE('',*,*,#17098,.T.);
#22368=ORIENTED_EDGE('',*,*,#17099,.F.);
#22369=ORIENTED_EDGE('',*,*,#17098,.F.);
#22370=ORIENTED_EDGE('',*,*,#17092,.F.);
#22371=ORIENTED_EDGE('',*,*,#17100,.F.);
#22372=ORIENTED_EDGE('',*,*,#17101,.T.);
#22373=ORIENTED_EDGE('',*,*,#17102,.F.);
#22374=ORIENTED_EDGE('',*,*,#17103,.T.);
#22375=ORIENTED_EDGE('',*,*,#17104,.F.);
#22376=ORIENTED_EDGE('',*,*,#17103,.F.);
#22377=ORIENTED_EDGE('',*,*,#17105,.F.);
#22378=ORIENTED_EDGE('',*,*,#17106,.F.);
#22379=ORIENTED_EDGE('',*,*,#17105,.T.);
#22380=ORIENTED_EDGE('',*,*,#17102,.T.);
#22381=ORIENTED_EDGE('',*,*,#17107,.T.);
#22382=ORIENTED_EDGE('',*,*,#17108,.F.);
#22383=ORIENTED_EDGE('',*,*,#17107,.F.);
#22384=ORIENTED_EDGE('',*,*,#17101,.F.);
#22385=ORIENTED_EDGE('',*,*,#17109,.F.);
#22386=ORIENTED_EDGE('',*,*,#17110,.T.);
#22387=ORIENTED_EDGE('',*,*,#17111,.F.);
#22388=ORIENTED_EDGE('',*,*,#17112,.T.);
#22389=ORIENTED_EDGE('',*,*,#17113,.F.);
#22390=ORIENTED_EDGE('',*,*,#17112,.F.);
#22391=ORIENTED_EDGE('',*,*,#17114,.F.);
#22392=ORIENTED_EDGE('',*,*,#17115,.F.);
#22393=ORIENTED_EDGE('',*,*,#17114,.T.);
#22394=ORIENTED_EDGE('',*,*,#17111,.T.);
#22395=ORIENTED_EDGE('',*,*,#17116,.T.);
#22396=ORIENTED_EDGE('',*,*,#17117,.F.);
#22397=ORIENTED_EDGE('',*,*,#17116,.F.);
#22398=ORIENTED_EDGE('',*,*,#17110,.F.);
#22399=ORIENTED_EDGE('',*,*,#17118,.F.);
#22400=ORIENTED_EDGE('',*,*,#17119,.T.);
#22401=ORIENTED_EDGE('',*,*,#17120,.F.);
#22402=ORIENTED_EDGE('',*,*,#17121,.T.);
#22403=ORIENTED_EDGE('',*,*,#17122,.F.);
#22404=ORIENTED_EDGE('',*,*,#17121,.F.);
#22405=ORIENTED_EDGE('',*,*,#17123,.F.);
#22406=ORIENTED_EDGE('',*,*,#17124,.F.);
#22407=ORIENTED_EDGE('',*,*,#17123,.T.);
#22408=ORIENTED_EDGE('',*,*,#17120,.T.);
#22409=ORIENTED_EDGE('',*,*,#17125,.T.);
#22410=ORIENTED_EDGE('',*,*,#17126,.F.);
#22411=ORIENTED_EDGE('',*,*,#17125,.F.);
#22412=ORIENTED_EDGE('',*,*,#17119,.F.);
#22413=ORIENTED_EDGE('',*,*,#17127,.F.);
#22414=ORIENTED_EDGE('',*,*,#17128,.T.);
#22415=ORIENTED_EDGE('',*,*,#17129,.F.);
#22416=ORIENTED_EDGE('',*,*,#17130,.T.);
#22417=ORIENTED_EDGE('',*,*,#17131,.F.);
#22418=ORIENTED_EDGE('',*,*,#17130,.F.);
#22419=ORIENTED_EDGE('',*,*,#17132,.F.);
#22420=ORIENTED_EDGE('',*,*,#17133,.F.);
#22421=ORIENTED_EDGE('',*,*,#17132,.T.);
#22422=ORIENTED_EDGE('',*,*,#17129,.T.);
#22423=ORIENTED_EDGE('',*,*,#17134,.T.);
#22424=ORIENTED_EDGE('',*,*,#17135,.F.);
#22425=ORIENTED_EDGE('',*,*,#17134,.F.);
#22426=ORIENTED_EDGE('',*,*,#17128,.F.);
#22427=ORIENTED_EDGE('',*,*,#17136,.F.);
#22428=ORIENTED_EDGE('',*,*,#17137,.T.);
#22429=ORIENTED_EDGE('',*,*,#17138,.F.);
#22430=ORIENTED_EDGE('',*,*,#17139,.T.);
#22431=ORIENTED_EDGE('',*,*,#17140,.F.);
#22432=ORIENTED_EDGE('',*,*,#17139,.F.);
#22433=ORIENTED_EDGE('',*,*,#17141,.F.);
#22434=ORIENTED_EDGE('',*,*,#17142,.F.);
#22435=ORIENTED_EDGE('',*,*,#17141,.T.);
#22436=ORIENTED_EDGE('',*,*,#17138,.T.);
#22437=ORIENTED_EDGE('',*,*,#17143,.T.);
#22438=ORIENTED_EDGE('',*,*,#17144,.F.);
#22439=ORIENTED_EDGE('',*,*,#17143,.F.);
#22440=ORIENTED_EDGE('',*,*,#17137,.F.);
#22441=ORIENTED_EDGE('',*,*,#17145,.F.);
#22442=ORIENTED_EDGE('',*,*,#17146,.T.);
#22443=ORIENTED_EDGE('',*,*,#17147,.F.);
#22444=ORIENTED_EDGE('',*,*,#17148,.T.);
#22445=ORIENTED_EDGE('',*,*,#17149,.F.);
#22446=ORIENTED_EDGE('',*,*,#17148,.F.);
#22447=ORIENTED_EDGE('',*,*,#17150,.F.);
#22448=ORIENTED_EDGE('',*,*,#17151,.F.);
#22449=ORIENTED_EDGE('',*,*,#17150,.T.);
#22450=ORIENTED_EDGE('',*,*,#17147,.T.);
#22451=ORIENTED_EDGE('',*,*,#17152,.T.);
#22452=ORIENTED_EDGE('',*,*,#17153,.F.);
#22453=ORIENTED_EDGE('',*,*,#17152,.F.);
#22454=ORIENTED_EDGE('',*,*,#17146,.F.);
#22455=ORIENTED_EDGE('',*,*,#17154,.F.);
#22456=ORIENTED_EDGE('',*,*,#17155,.T.);
#22457=ORIENTED_EDGE('',*,*,#17156,.F.);
#22458=ORIENTED_EDGE('',*,*,#17157,.T.);
#22459=ORIENTED_EDGE('',*,*,#17158,.F.);
#22460=ORIENTED_EDGE('',*,*,#17157,.F.);
#22461=ORIENTED_EDGE('',*,*,#17159,.F.);
#22462=ORIENTED_EDGE('',*,*,#17160,.F.);
#22463=ORIENTED_EDGE('',*,*,#17159,.T.);
#22464=ORIENTED_EDGE('',*,*,#17156,.T.);
#22465=ORIENTED_EDGE('',*,*,#17161,.T.);
#22466=ORIENTED_EDGE('',*,*,#17162,.F.);
#22467=ORIENTED_EDGE('',*,*,#17161,.F.);
#22468=ORIENTED_EDGE('',*,*,#17155,.F.);
#22469=ORIENTED_EDGE('',*,*,#17163,.F.);
#22470=ORIENTED_EDGE('',*,*,#17164,.T.);
#22471=ORIENTED_EDGE('',*,*,#17165,.F.);
#22472=ORIENTED_EDGE('',*,*,#17166,.T.);
#22473=ORIENTED_EDGE('',*,*,#17167,.F.);
#22474=ORIENTED_EDGE('',*,*,#17166,.F.);
#22475=ORIENTED_EDGE('',*,*,#17168,.F.);
#22476=ORIENTED_EDGE('',*,*,#17169,.F.);
#22477=ORIENTED_EDGE('',*,*,#17168,.T.);
#22478=ORIENTED_EDGE('',*,*,#17165,.T.);
#22479=ORIENTED_EDGE('',*,*,#17170,.T.);
#22480=ORIENTED_EDGE('',*,*,#17171,.F.);
#22481=ORIENTED_EDGE('',*,*,#17170,.F.);
#22482=ORIENTED_EDGE('',*,*,#17164,.F.);
#22483=ORIENTED_EDGE('',*,*,#17172,.F.);
#22484=ORIENTED_EDGE('',*,*,#17173,.T.);
#22485=ORIENTED_EDGE('',*,*,#17174,.F.);
#22486=ORIENTED_EDGE('',*,*,#17175,.T.);
#22487=ORIENTED_EDGE('',*,*,#17176,.F.);
#22488=ORIENTED_EDGE('',*,*,#17175,.F.);
#22489=ORIENTED_EDGE('',*,*,#17177,.F.);
#22490=ORIENTED_EDGE('',*,*,#17178,.F.);
#22491=ORIENTED_EDGE('',*,*,#17177,.T.);
#22492=ORIENTED_EDGE('',*,*,#17174,.T.);
#22493=ORIENTED_EDGE('',*,*,#17179,.T.);
#22494=ORIENTED_EDGE('',*,*,#17180,.F.);
#22495=ORIENTED_EDGE('',*,*,#17179,.F.);
#22496=ORIENTED_EDGE('',*,*,#17173,.F.);
#22497=ORIENTED_EDGE('',*,*,#17181,.F.);
#22498=ORIENTED_EDGE('',*,*,#17182,.T.);
#22499=ORIENTED_EDGE('',*,*,#17183,.F.);
#22500=ORIENTED_EDGE('',*,*,#17184,.T.);
#22501=ORIENTED_EDGE('',*,*,#17185,.F.);
#22502=ORIENTED_EDGE('',*,*,#17184,.F.);
#22503=ORIENTED_EDGE('',*,*,#17186,.F.);
#22504=ORIENTED_EDGE('',*,*,#17187,.F.);
#22505=ORIENTED_EDGE('',*,*,#17186,.T.);
#22506=ORIENTED_EDGE('',*,*,#17183,.T.);
#22507=ORIENTED_EDGE('',*,*,#17188,.T.);
#22508=ORIENTED_EDGE('',*,*,#17189,.F.);
#22509=ORIENTED_EDGE('',*,*,#17188,.F.);
#22510=ORIENTED_EDGE('',*,*,#17182,.F.);
#22511=ORIENTED_EDGE('',*,*,#17190,.F.);
#22512=ORIENTED_EDGE('',*,*,#17191,.T.);
#22513=ORIENTED_EDGE('',*,*,#17192,.F.);
#22514=ORIENTED_EDGE('',*,*,#17193,.T.);
#22515=ORIENTED_EDGE('',*,*,#17194,.F.);
#22516=ORIENTED_EDGE('',*,*,#17193,.F.);
#22517=ORIENTED_EDGE('',*,*,#17195,.F.);
#22518=ORIENTED_EDGE('',*,*,#17196,.F.);
#22519=ORIENTED_EDGE('',*,*,#17195,.T.);
#22520=ORIENTED_EDGE('',*,*,#17192,.T.);
#22521=ORIENTED_EDGE('',*,*,#17197,.T.);
#22522=ORIENTED_EDGE('',*,*,#17198,.F.);
#22523=ORIENTED_EDGE('',*,*,#17197,.F.);
#22524=ORIENTED_EDGE('',*,*,#17191,.F.);
#22525=ORIENTED_EDGE('',*,*,#17199,.F.);
#22526=ORIENTED_EDGE('',*,*,#17200,.T.);
#22527=ORIENTED_EDGE('',*,*,#17201,.F.);
#22528=ORIENTED_EDGE('',*,*,#17202,.T.);
#22529=ORIENTED_EDGE('',*,*,#17203,.F.);
#22530=ORIENTED_EDGE('',*,*,#17202,.F.);
#22531=ORIENTED_EDGE('',*,*,#17204,.F.);
#22532=ORIENTED_EDGE('',*,*,#17205,.F.);
#22533=ORIENTED_EDGE('',*,*,#17204,.T.);
#22534=ORIENTED_EDGE('',*,*,#17201,.T.);
#22535=ORIENTED_EDGE('',*,*,#17206,.T.);
#22536=ORIENTED_EDGE('',*,*,#17207,.F.);
#22537=ORIENTED_EDGE('',*,*,#17206,.F.);
#22538=ORIENTED_EDGE('',*,*,#17200,.F.);
#22539=ORIENTED_EDGE('',*,*,#17208,.F.);
#22540=ORIENTED_EDGE('',*,*,#17209,.T.);
#22541=ORIENTED_EDGE('',*,*,#17210,.F.);
#22542=ORIENTED_EDGE('',*,*,#17211,.T.);
#22543=ORIENTED_EDGE('',*,*,#17212,.F.);
#22544=ORIENTED_EDGE('',*,*,#17211,.F.);
#22545=ORIENTED_EDGE('',*,*,#17213,.F.);
#22546=ORIENTED_EDGE('',*,*,#17214,.F.);
#22547=ORIENTED_EDGE('',*,*,#17213,.T.);
#22548=ORIENTED_EDGE('',*,*,#17210,.T.);
#22549=ORIENTED_EDGE('',*,*,#17215,.T.);
#22550=ORIENTED_EDGE('',*,*,#17216,.F.);
#22551=ORIENTED_EDGE('',*,*,#17215,.F.);
#22552=ORIENTED_EDGE('',*,*,#17209,.F.);
#22553=ORIENTED_EDGE('',*,*,#16849,.T.);
#22554=ORIENTED_EDGE('',*,*,#17217,.F.);
#22555=ORIENTED_EDGE('',*,*,#17218,.T.);
#22556=ORIENTED_EDGE('',*,*,#17219,.F.);
#22557=ORIENTED_EDGE('',*,*,#17220,.F.);
#22558=ORIENTED_EDGE('',*,*,#16858,.F.);
#22559=ORIENTED_EDGE('',*,*,#16856,.F.);
#22560=ORIENTED_EDGE('',*,*,#16850,.T.);
#22561=ORIENTED_EDGE('',*,*,#17219,.T.);
#22562=ORIENTED_EDGE('',*,*,#17221,.T.);
#22563=ORIENTED_EDGE('',*,*,#17222,.F.);
#22564=ORIENTED_EDGE('',*,*,#17223,.F.);
#22565=ORIENTED_EDGE('',*,*,#17221,.F.);
#22566=ORIENTED_EDGE('',*,*,#17218,.F.);
#22567=ORIENTED_EDGE('',*,*,#17224,.F.);
#22568=ORIENTED_EDGE('',*,*,#16876,.F.);
#22569=ORIENTED_EDGE('',*,*,#16871,.F.);
#22570=ORIENTED_EDGE('',*,*,#17225,.F.);
#22571=ORIENTED_EDGE('',*,*,#16874,.F.);
#22572=ORIENTED_EDGE('',*,*,#16879,.F.);
#22573=ORIENTED_EDGE('',*,*,#17226,.F.);
#22574=ORIENTED_EDGE('',*,*,#17227,.T.);
#22575=ORIENTED_EDGE('',*,*,#17228,.F.);
#22576=ORIENTED_EDGE('',*,*,#17227,.F.);
#22577=ORIENTED_EDGE('',*,*,#17229,.F.);
#22578=ORIENTED_EDGE('',*,*,#17228,.T.);
#22579=ORIENTED_EDGE('',*,*,#17230,.F.);
#22580=ORIENTED_EDGE('',*,*,#17231,.T.);
#22581=ORIENTED_EDGE('',*,*,#17229,.T.);
#22582=ORIENTED_EDGE('',*,*,#17231,.F.);
#22583=ORIENTED_EDGE('',*,*,#17232,.F.);
#22584=ORIENTED_EDGE('',*,*,#17233,.T.);
#22585=ORIENTED_EDGE('',*,*,#17050,.T.);
#22586=ORIENTED_EDGE('',*,*,#17051,.T.);
#22587=ORIENTED_EDGE('',*,*,#17053,.T.);
#22588=ORIENTED_EDGE('',*,*,#17234,.T.);
#22589=ORIENTED_EDGE('',*,*,#17230,.T.);
#22590=ORIENTED_EDGE('',*,*,#17234,.F.);
#22591=ORIENTED_EDGE('',*,*,#17054,.T.);
#22592=ORIENTED_EDGE('',*,*,#17044,.T.);
#22593=ORIENTED_EDGE('',*,*,#17048,.T.);
#22594=ORIENTED_EDGE('',*,*,#17233,.F.);
#22595=ORIENTED_EDGE('',*,*,#16848,.T.);
#22596=ORIENTED_EDGE('',*,*,#16875,.T.);
#22597=ORIENTED_EDGE('',*,*,#17225,.T.);
#22598=ORIENTED_EDGE('',*,*,#16878,.T.);
#22599=ORIENTED_EDGE('',*,*,#16845,.T.);
#22600=ORIENTED_EDGE('',*,*,#16869,.T.);
#22601=ORIENTED_EDGE('',*,*,#16881,.T.);
#22602=ORIENTED_EDGE('',*,*,#16863,.T.);
#22603=ORIENTED_EDGE('',*,*,#16842,.T.);
#22604=ORIENTED_EDGE('',*,*,#16862,.T.);
#22605=ORIENTED_EDGE('',*,*,#16880,.T.);
#22606=ORIENTED_EDGE('',*,*,#16866,.T.);
#22607=ORIENTED_EDGE('',*,*,#16839,.T.);
#22608=ORIENTED_EDGE('',*,*,#16877,.T.);
#22609=ORIENTED_EDGE('',*,*,#17224,.T.);
#22610=ORIENTED_EDGE('',*,*,#16870,.T.);
#22611=ORIENTED_EDGE('',*,*,#16836,.T.);
#22612=ORIENTED_EDGE('',*,*,#16859,.T.);
#22613=ORIENTED_EDGE('',*,*,#17220,.T.);
#22614=ORIENTED_EDGE('',*,*,#16855,.T.);
#22615=ORIENTED_EDGE('',*,*,#16833,.T.);
#22616=ORIENTED_EDGE('',*,*,#16851,.T.);
#22617=ORIENTED_EDGE('',*,*,#17222,.T.);
#22618=ORIENTED_EDGE('',*,*,#17223,.T.);
#22619=ORIENTED_EDGE('',*,*,#17217,.T.);
#22620=ORIENTED_EDGE('',*,*,#16888,.T.);
#22621=ORIENTED_EDGE('',*,*,#16890,.T.);
#22622=ORIENTED_EDGE('',*,*,#16882,.T.);
#22623=ORIENTED_EDGE('',*,*,#16886,.T.);
#22624=ORIENTED_EDGE('',*,*,#16897,.T.);
#22625=ORIENTED_EDGE('',*,*,#16899,.T.);
#22626=ORIENTED_EDGE('',*,*,#16891,.T.);
#22627=ORIENTED_EDGE('',*,*,#16895,.T.);
#22628=ORIENTED_EDGE('',*,*,#16906,.T.);
#22629=ORIENTED_EDGE('',*,*,#16908,.T.);
#22630=ORIENTED_EDGE('',*,*,#16900,.T.);
#22631=ORIENTED_EDGE('',*,*,#16904,.T.);
#22632=ORIENTED_EDGE('',*,*,#16915,.T.);
#22633=ORIENTED_EDGE('',*,*,#16917,.T.);
#22634=ORIENTED_EDGE('',*,*,#16909,.T.);
#22635=ORIENTED_EDGE('',*,*,#16913,.T.);
#22636=ORIENTED_EDGE('',*,*,#16924,.T.);
#22637=ORIENTED_EDGE('',*,*,#16926,.T.);
#22638=ORIENTED_EDGE('',*,*,#16918,.T.);
#22639=ORIENTED_EDGE('',*,*,#16922,.T.);
#22640=ORIENTED_EDGE('',*,*,#16933,.T.);
#22641=ORIENTED_EDGE('',*,*,#16935,.T.);
#22642=ORIENTED_EDGE('',*,*,#16927,.T.);
#22643=ORIENTED_EDGE('',*,*,#16931,.T.);
#22644=ORIENTED_EDGE('',*,*,#16942,.T.);
#22645=ORIENTED_EDGE('',*,*,#16944,.T.);
#22646=ORIENTED_EDGE('',*,*,#16936,.T.);
#22647=ORIENTED_EDGE('',*,*,#16940,.T.);
#22648=ORIENTED_EDGE('',*,*,#16951,.T.);
#22649=ORIENTED_EDGE('',*,*,#16953,.T.);
#22650=ORIENTED_EDGE('',*,*,#16945,.T.);
#22651=ORIENTED_EDGE('',*,*,#16949,.T.);
#22652=ORIENTED_EDGE('',*,*,#16960,.T.);
#22653=ORIENTED_EDGE('',*,*,#16962,.T.);
#22654=ORIENTED_EDGE('',*,*,#16954,.T.);
#22655=ORIENTED_EDGE('',*,*,#16958,.T.);
#22656=ORIENTED_EDGE('',*,*,#16969,.T.);
#22657=ORIENTED_EDGE('',*,*,#16971,.T.);
#22658=ORIENTED_EDGE('',*,*,#16963,.T.);
#22659=ORIENTED_EDGE('',*,*,#16967,.T.);
#22660=ORIENTED_EDGE('',*,*,#16978,.T.);
#22661=ORIENTED_EDGE('',*,*,#16980,.T.);
#22662=ORIENTED_EDGE('',*,*,#16972,.T.);
#22663=ORIENTED_EDGE('',*,*,#16976,.T.);
#22664=ORIENTED_EDGE('',*,*,#16987,.T.);
#22665=ORIENTED_EDGE('',*,*,#16989,.T.);
#22666=ORIENTED_EDGE('',*,*,#16981,.T.);
#22667=ORIENTED_EDGE('',*,*,#16985,.T.);
#22668=ORIENTED_EDGE('',*,*,#16996,.T.);
#22669=ORIENTED_EDGE('',*,*,#16998,.T.);
#22670=ORIENTED_EDGE('',*,*,#16990,.T.);
#22671=ORIENTED_EDGE('',*,*,#16994,.T.);
#22672=ORIENTED_EDGE('',*,*,#17005,.T.);
#22673=ORIENTED_EDGE('',*,*,#17007,.T.);
#22674=ORIENTED_EDGE('',*,*,#16999,.T.);
#22675=ORIENTED_EDGE('',*,*,#17003,.T.);
#22676=ORIENTED_EDGE('',*,*,#17014,.T.);
#22677=ORIENTED_EDGE('',*,*,#17016,.T.);
#22678=ORIENTED_EDGE('',*,*,#17008,.T.);
#22679=ORIENTED_EDGE('',*,*,#17012,.T.);
#22680=ORIENTED_EDGE('',*,*,#17023,.T.);
#22681=ORIENTED_EDGE('',*,*,#17025,.T.);
#22682=ORIENTED_EDGE('',*,*,#17017,.T.);
#22683=ORIENTED_EDGE('',*,*,#17021,.T.);
#22684=ORIENTED_EDGE('',*,*,#17032,.T.);
#22685=ORIENTED_EDGE('',*,*,#17034,.T.);
#22686=ORIENTED_EDGE('',*,*,#17026,.T.);
#22687=ORIENTED_EDGE('',*,*,#17030,.T.);
#22688=ORIENTED_EDGE('',*,*,#17041,.T.);
#22689=ORIENTED_EDGE('',*,*,#17043,.T.);
#22690=ORIENTED_EDGE('',*,*,#17035,.T.);
#22691=ORIENTED_EDGE('',*,*,#17039,.T.);
#22692=ORIENTED_EDGE('',*,*,#17061,.T.);
#22693=ORIENTED_EDGE('',*,*,#17063,.T.);
#22694=ORIENTED_EDGE('',*,*,#17055,.T.);
#22695=ORIENTED_EDGE('',*,*,#17059,.T.);
#22696=ORIENTED_EDGE('',*,*,#17070,.T.);
#22697=ORIENTED_EDGE('',*,*,#17072,.T.);
#22698=ORIENTED_EDGE('',*,*,#17064,.T.);
#22699=ORIENTED_EDGE('',*,*,#17068,.T.);
#22700=ORIENTED_EDGE('',*,*,#17079,.T.);
#22701=ORIENTED_EDGE('',*,*,#17081,.T.);
#22702=ORIENTED_EDGE('',*,*,#17073,.T.);
#22703=ORIENTED_EDGE('',*,*,#17077,.T.);
#22704=ORIENTED_EDGE('',*,*,#17088,.T.);
#22705=ORIENTED_EDGE('',*,*,#17090,.T.);
#22706=ORIENTED_EDGE('',*,*,#17082,.T.);
#22707=ORIENTED_EDGE('',*,*,#17086,.T.);
#22708=ORIENTED_EDGE('',*,*,#17097,.T.);
#22709=ORIENTED_EDGE('',*,*,#17099,.T.);
#22710=ORIENTED_EDGE('',*,*,#17091,.T.);
#22711=ORIENTED_EDGE('',*,*,#17095,.T.);
#22712=ORIENTED_EDGE('',*,*,#17106,.T.);
#22713=ORIENTED_EDGE('',*,*,#17108,.T.);
#22714=ORIENTED_EDGE('',*,*,#17100,.T.);
#22715=ORIENTED_EDGE('',*,*,#17104,.T.);
#22716=ORIENTED_EDGE('',*,*,#17115,.T.);
#22717=ORIENTED_EDGE('',*,*,#17117,.T.);
#22718=ORIENTED_EDGE('',*,*,#17109,.T.);
#22719=ORIENTED_EDGE('',*,*,#17113,.T.);
#22720=ORIENTED_EDGE('',*,*,#17124,.T.);
#22721=ORIENTED_EDGE('',*,*,#17126,.T.);
#22722=ORIENTED_EDGE('',*,*,#17118,.T.);
#22723=ORIENTED_EDGE('',*,*,#17122,.T.);
#22724=ORIENTED_EDGE('',*,*,#17133,.T.);
#22725=ORIENTED_EDGE('',*,*,#17135,.T.);
#22726=ORIENTED_EDGE('',*,*,#17127,.T.);
#22727=ORIENTED_EDGE('',*,*,#17131,.T.);
#22728=ORIENTED_EDGE('',*,*,#17142,.T.);
#22729=ORIENTED_EDGE('',*,*,#17144,.T.);
#22730=ORIENTED_EDGE('',*,*,#17136,.T.);
#22731=ORIENTED_EDGE('',*,*,#17140,.T.);
#22732=ORIENTED_EDGE('',*,*,#17151,.T.);
#22733=ORIENTED_EDGE('',*,*,#17153,.T.);
#22734=ORIENTED_EDGE('',*,*,#17145,.T.);
#22735=ORIENTED_EDGE('',*,*,#17149,.T.);
#22736=ORIENTED_EDGE('',*,*,#17160,.T.);
#22737=ORIENTED_EDGE('',*,*,#17162,.T.);
#22738=ORIENTED_EDGE('',*,*,#17154,.T.);
#22739=ORIENTED_EDGE('',*,*,#17158,.T.);
#22740=ORIENTED_EDGE('',*,*,#17169,.T.);
#22741=ORIENTED_EDGE('',*,*,#17171,.T.);
#22742=ORIENTED_EDGE('',*,*,#17163,.T.);
#22743=ORIENTED_EDGE('',*,*,#17167,.T.);
#22744=ORIENTED_EDGE('',*,*,#17178,.T.);
#22745=ORIENTED_EDGE('',*,*,#17180,.T.);
#22746=ORIENTED_EDGE('',*,*,#17172,.T.);
#22747=ORIENTED_EDGE('',*,*,#17176,.T.);
#22748=ORIENTED_EDGE('',*,*,#17187,.T.);
#22749=ORIENTED_EDGE('',*,*,#17189,.T.);
#22750=ORIENTED_EDGE('',*,*,#17181,.T.);
#22751=ORIENTED_EDGE('',*,*,#17185,.T.);
#22752=ORIENTED_EDGE('',*,*,#17196,.T.);
#22753=ORIENTED_EDGE('',*,*,#17198,.T.);
#22754=ORIENTED_EDGE('',*,*,#17190,.T.);
#22755=ORIENTED_EDGE('',*,*,#17194,.T.);
#22756=ORIENTED_EDGE('',*,*,#17205,.T.);
#22757=ORIENTED_EDGE('',*,*,#17207,.T.);
#22758=ORIENTED_EDGE('',*,*,#17199,.T.);
#22759=ORIENTED_EDGE('',*,*,#17203,.T.);
#22760=ORIENTED_EDGE('',*,*,#17214,.T.);
#22761=ORIENTED_EDGE('',*,*,#17216,.T.);
#22762=ORIENTED_EDGE('',*,*,#17208,.T.);
#22763=ORIENTED_EDGE('',*,*,#17212,.T.);
#22764=ORIENTED_EDGE('',*,*,#17232,.T.);
#22765=ORIENTED_EDGE('',*,*,#17235,.T.);
#22766=ORIENTED_EDGE('',*,*,#17236,.F.);
#22767=ORIENTED_EDGE('',*,*,#17235,.F.);
#22768=ORIENTED_EDGE('',*,*,#17236,.T.);
#22769=ORIENTED_EDGE('',*,*,#17237,.F.);
#22770=ORIENTED_EDGE('',*,*,#17238,.F.);
#22771=ORIENTED_EDGE('',*,*,#17239,.T.);
#22772=ORIENTED_EDGE('',*,*,#17237,.T.);
#22773=ORIENTED_EDGE('',*,*,#17239,.F.);
#22774=ORIENTED_EDGE('',*,*,#17238,.T.);
#22775=ORIENTED_EDGE('',*,*,#17240,.F.);
#22776=ORIENTED_EDGE('',*,*,#17226,.T.);
#22777=ORIENTED_EDGE('',*,*,#17241,.T.);
#22778=ORIENTED_EDGE('',*,*,#17240,.T.);
#22779=ORIENTED_EDGE('',*,*,#17241,.F.);
#22780=ORIENTED_EDGE('',*,*,#16853,.T.);
#22781=ORIENTED_EDGE('',*,*,#16854,.T.);
#22782=ORIENTED_EDGE('',*,*,#17242,.F.);
#22783=ORIENTED_EDGE('',*,*,#17243,.T.);
#22784=ORIENTED_EDGE('',*,*,#17244,.T.);
#22785=ORIENTED_EDGE('',*,*,#17245,.F.);
#22786=ORIENTED_EDGE('',*,*,#17246,.F.);
#22787=ORIENTED_EDGE('',*,*,#17247,.T.);
#22788=ORIENTED_EDGE('',*,*,#17248,.T.);
#22789=ORIENTED_EDGE('',*,*,#17243,.F.);
#22790=ORIENTED_EDGE('',*,*,#17249,.F.);
#22791=ORIENTED_EDGE('',*,*,#17250,.T.);
#22792=ORIENTED_EDGE('',*,*,#17251,.T.);
#22793=ORIENTED_EDGE('',*,*,#17247,.F.);
#22794=ORIENTED_EDGE('',*,*,#17252,.F.);
#22795=ORIENTED_EDGE('',*,*,#17253,.T.);
#22796=ORIENTED_EDGE('',*,*,#17254,.T.);
#22797=ORIENTED_EDGE('',*,*,#17250,.F.);
#22798=ORIENTED_EDGE('',*,*,#17255,.F.);
#22799=ORIENTED_EDGE('',*,*,#17256,.T.);
#22800=ORIENTED_EDGE('',*,*,#17257,.T.);
#22801=ORIENTED_EDGE('',*,*,#17253,.F.);
#22802=ORIENTED_EDGE('',*,*,#17258,.F.);
#22803=ORIENTED_EDGE('',*,*,#17259,.T.);
#22804=ORIENTED_EDGE('',*,*,#17260,.T.);
#22805=ORIENTED_EDGE('',*,*,#17256,.F.);
#22806=ORIENTED_EDGE('',*,*,#17261,.F.);
#22807=ORIENTED_EDGE('',*,*,#17262,.T.);
#22808=ORIENTED_EDGE('',*,*,#17263,.T.);
#22809=ORIENTED_EDGE('',*,*,#17259,.F.);
#22810=ORIENTED_EDGE('',*,*,#17264,.F.);
#22811=ORIENTED_EDGE('',*,*,#17245,.T.);
#22812=ORIENTED_EDGE('',*,*,#17265,.T.);
#22813=ORIENTED_EDGE('',*,*,#17262,.F.);
#22814=ORIENTED_EDGE('',*,*,#17266,.F.);
#22815=ORIENTED_EDGE('',*,*,#17267,.T.);
#22816=ORIENTED_EDGE('',*,*,#17268,.T.);
#22817=ORIENTED_EDGE('',*,*,#17269,.F.);
#22818=ORIENTED_EDGE('',*,*,#17270,.F.);
#22819=ORIENTED_EDGE('',*,*,#17271,.T.);
#22820=ORIENTED_EDGE('',*,*,#17272,.T.);
#22821=ORIENTED_EDGE('',*,*,#17267,.F.);
#22822=ORIENTED_EDGE('',*,*,#17273,.F.);
#22823=ORIENTED_EDGE('',*,*,#17274,.T.);
#22824=ORIENTED_EDGE('',*,*,#17275,.T.);
#22825=ORIENTED_EDGE('',*,*,#17271,.F.);
#22826=ORIENTED_EDGE('',*,*,#17276,.F.);
#22827=ORIENTED_EDGE('',*,*,#17277,.T.);
#22828=ORIENTED_EDGE('',*,*,#17278,.T.);
#22829=ORIENTED_EDGE('',*,*,#17274,.F.);
#22830=ORIENTED_EDGE('',*,*,#17279,.F.);
#22831=ORIENTED_EDGE('',*,*,#17280,.T.);
#22832=ORIENTED_EDGE('',*,*,#17281,.T.);
#22833=ORIENTED_EDGE('',*,*,#17277,.F.);
#22834=ORIENTED_EDGE('',*,*,#17282,.F.);
#22835=ORIENTED_EDGE('',*,*,#17283,.T.);
#22836=ORIENTED_EDGE('',*,*,#17284,.T.);
#22837=ORIENTED_EDGE('',*,*,#17280,.F.);
#22838=ORIENTED_EDGE('',*,*,#17285,.F.);
#22839=ORIENTED_EDGE('',*,*,#17286,.T.);
#22840=ORIENTED_EDGE('',*,*,#17287,.T.);
#22841=ORIENTED_EDGE('',*,*,#17283,.F.);
#22842=ORIENTED_EDGE('',*,*,#17288,.F.);
#22843=ORIENTED_EDGE('',*,*,#17289,.T.);
#22844=ORIENTED_EDGE('',*,*,#17290,.T.);
#22845=ORIENTED_EDGE('',*,*,#17286,.F.);
#22846=ORIENTED_EDGE('',*,*,#17291,.F.);
#22847=ORIENTED_EDGE('',*,*,#17292,.T.);
#22848=ORIENTED_EDGE('',*,*,#17293,.T.);
#22849=ORIENTED_EDGE('',*,*,#17289,.F.);
#22850=ORIENTED_EDGE('',*,*,#17294,.F.);
#22851=ORIENTED_EDGE('',*,*,#17295,.T.);
#22852=ORIENTED_EDGE('',*,*,#17296,.T.);
#22853=ORIENTED_EDGE('',*,*,#17292,.F.);
#22854=ORIENTED_EDGE('',*,*,#17297,.F.);
#22855=ORIENTED_EDGE('',*,*,#17298,.T.);
#22856=ORIENTED_EDGE('',*,*,#17299,.T.);
#22857=ORIENTED_EDGE('',*,*,#17295,.F.);
#22858=ORIENTED_EDGE('',*,*,#17300,.F.);
#22859=ORIENTED_EDGE('',*,*,#17269,.T.);
#22860=ORIENTED_EDGE('',*,*,#17301,.T.);
#22861=ORIENTED_EDGE('',*,*,#17298,.F.);
#22862=ORIENTED_EDGE('',*,*,#17301,.F.);
#22863=ORIENTED_EDGE('',*,*,#17268,.F.);
#22864=ORIENTED_EDGE('',*,*,#17272,.F.);
#22865=ORIENTED_EDGE('',*,*,#17275,.F.);
#22866=ORIENTED_EDGE('',*,*,#17278,.F.);
#22867=ORIENTED_EDGE('',*,*,#17281,.F.);
#22868=ORIENTED_EDGE('',*,*,#17284,.F.);
#22869=ORIENTED_EDGE('',*,*,#17287,.F.);
#22870=ORIENTED_EDGE('',*,*,#17290,.F.);
#22871=ORIENTED_EDGE('',*,*,#17293,.F.);
#22872=ORIENTED_EDGE('',*,*,#17296,.F.);
#22873=ORIENTED_EDGE('',*,*,#17299,.F.);
#22874=ORIENTED_EDGE('',*,*,#17265,.F.);
#22875=ORIENTED_EDGE('',*,*,#17244,.F.);
#22876=ORIENTED_EDGE('',*,*,#17248,.F.);
#22877=ORIENTED_EDGE('',*,*,#17251,.F.);
#22878=ORIENTED_EDGE('',*,*,#17254,.F.);
#22879=ORIENTED_EDGE('',*,*,#17257,.F.);
#22880=ORIENTED_EDGE('',*,*,#17260,.F.);
#22881=ORIENTED_EDGE('',*,*,#17263,.F.);
#22882=ORIENTED_EDGE('',*,*,#17302,.F.);
#22883=ORIENTED_EDGE('',*,*,#17303,.T.);
#22884=ORIENTED_EDGE('',*,*,#17304,.T.);
#22885=ORIENTED_EDGE('',*,*,#17305,.F.);
#22886=ORIENTED_EDGE('',*,*,#17306,.F.);
#22887=ORIENTED_EDGE('',*,*,#17307,.T.);
#22888=ORIENTED_EDGE('',*,*,#17308,.T.);
#22889=ORIENTED_EDGE('',*,*,#17303,.F.);
#22890=ORIENTED_EDGE('',*,*,#17309,.F.);
#22891=ORIENTED_EDGE('',*,*,#17305,.T.);
#22892=ORIENTED_EDGE('',*,*,#17310,.T.);
#22893=ORIENTED_EDGE('',*,*,#17307,.F.);
#22894=ORIENTED_EDGE('',*,*,#17311,.F.);
#22895=ORIENTED_EDGE('',*,*,#17312,.T.);
#22896=ORIENTED_EDGE('',*,*,#17313,.T.);
#22897=ORIENTED_EDGE('',*,*,#17314,.F.);
#22898=ORIENTED_EDGE('',*,*,#17315,.F.);
#22899=ORIENTED_EDGE('',*,*,#17316,.T.);
#22900=ORIENTED_EDGE('',*,*,#17317,.T.);
#22901=ORIENTED_EDGE('',*,*,#17312,.F.);
#22902=ORIENTED_EDGE('',*,*,#17318,.F.);
#22903=ORIENTED_EDGE('',*,*,#17319,.T.);
#22904=ORIENTED_EDGE('',*,*,#17320,.T.);
#22905=ORIENTED_EDGE('',*,*,#17316,.F.);
#22906=ORIENTED_EDGE('',*,*,#17321,.F.);
#22907=ORIENTED_EDGE('',*,*,#17322,.T.);
#22908=ORIENTED_EDGE('',*,*,#17323,.T.);
#22909=ORIENTED_EDGE('',*,*,#17319,.F.);
#22910=ORIENTED_EDGE('',*,*,#17324,.F.);
#22911=ORIENTED_EDGE('',*,*,#17325,.T.);
#22912=ORIENTED_EDGE('',*,*,#17326,.T.);
#22913=ORIENTED_EDGE('',*,*,#17322,.F.);
#22914=ORIENTED_EDGE('',*,*,#17327,.F.);
#22915=ORIENTED_EDGE('',*,*,#17328,.T.);
#22916=ORIENTED_EDGE('',*,*,#17329,.T.);
#22917=ORIENTED_EDGE('',*,*,#17325,.F.);
#22918=ORIENTED_EDGE('',*,*,#17330,.F.);
#22919=ORIENTED_EDGE('',*,*,#17331,.T.);
#22920=ORIENTED_EDGE('',*,*,#17332,.T.);
#22921=ORIENTED_EDGE('',*,*,#17328,.F.);
#22922=ORIENTED_EDGE('',*,*,#17333,.F.);
#22923=ORIENTED_EDGE('',*,*,#17334,.T.);
#22924=ORIENTED_EDGE('',*,*,#17335,.T.);
#22925=ORIENTED_EDGE('',*,*,#17331,.F.);
#22926=ORIENTED_EDGE('',*,*,#17336,.F.);
#22927=ORIENTED_EDGE('',*,*,#17337,.T.);
#22928=ORIENTED_EDGE('',*,*,#17338,.T.);
#22929=ORIENTED_EDGE('',*,*,#17334,.F.);
#22930=ORIENTED_EDGE('',*,*,#17339,.F.);
#22931=ORIENTED_EDGE('',*,*,#17340,.T.);
#22932=ORIENTED_EDGE('',*,*,#17341,.T.);
#22933=ORIENTED_EDGE('',*,*,#17337,.F.);
#22934=ORIENTED_EDGE('',*,*,#17342,.F.);
#22935=ORIENTED_EDGE('',*,*,#17314,.T.);
#22936=ORIENTED_EDGE('',*,*,#17343,.T.);
#22937=ORIENTED_EDGE('',*,*,#17340,.F.);
#22938=ORIENTED_EDGE('',*,*,#17343,.F.);
#22939=ORIENTED_EDGE('',*,*,#17313,.F.);
#22940=ORIENTED_EDGE('',*,*,#17317,.F.);
#22941=ORIENTED_EDGE('',*,*,#17320,.F.);
#22942=ORIENTED_EDGE('',*,*,#17323,.F.);
#22943=ORIENTED_EDGE('',*,*,#17326,.F.);
#22944=ORIENTED_EDGE('',*,*,#17329,.F.);
#22945=ORIENTED_EDGE('',*,*,#17332,.F.);
#22946=ORIENTED_EDGE('',*,*,#17335,.F.);
#22947=ORIENTED_EDGE('',*,*,#17338,.F.);
#22948=ORIENTED_EDGE('',*,*,#17341,.F.);
#22949=ORIENTED_EDGE('',*,*,#17310,.F.);
#22950=ORIENTED_EDGE('',*,*,#17304,.F.);
#22951=ORIENTED_EDGE('',*,*,#17308,.F.);
#22952=ORIENTED_EDGE('',*,*,#17302,.T.);
#22953=ORIENTED_EDGE('',*,*,#17309,.T.);
#22954=ORIENTED_EDGE('',*,*,#17306,.T.);
#22955=ORIENTED_EDGE('',*,*,#17242,.T.);
#22956=ORIENTED_EDGE('',*,*,#17264,.T.);
#22957=ORIENTED_EDGE('',*,*,#17261,.T.);
#22958=ORIENTED_EDGE('',*,*,#17258,.T.);
#22959=ORIENTED_EDGE('',*,*,#17255,.T.);
#22960=ORIENTED_EDGE('',*,*,#17252,.T.);
#22961=ORIENTED_EDGE('',*,*,#17249,.T.);
#22962=ORIENTED_EDGE('',*,*,#17246,.T.);
#22963=ORIENTED_EDGE('',*,*,#17344,.F.);
#22964=ORIENTED_EDGE('',*,*,#17345,.T.);
#22965=ORIENTED_EDGE('',*,*,#17346,.T.);
#22966=ORIENTED_EDGE('',*,*,#17347,.F.);
#22967=ORIENTED_EDGE('',*,*,#17348,.F.);
#22968=ORIENTED_EDGE('',*,*,#17349,.T.);
#22969=ORIENTED_EDGE('',*,*,#17350,.T.);
#22970=ORIENTED_EDGE('',*,*,#17345,.F.);
#22971=ORIENTED_EDGE('',*,*,#17351,.F.);
#22972=ORIENTED_EDGE('',*,*,#17352,.T.);
#22973=ORIENTED_EDGE('',*,*,#17353,.T.);
#22974=ORIENTED_EDGE('',*,*,#17349,.F.);
#22975=ORIENTED_EDGE('',*,*,#17354,.F.);
#22976=ORIENTED_EDGE('',*,*,#17355,.T.);
#22977=ORIENTED_EDGE('',*,*,#17356,.T.);
#22978=ORIENTED_EDGE('',*,*,#17352,.F.);
#22979=ORIENTED_EDGE('',*,*,#17357,.F.);
#22980=ORIENTED_EDGE('',*,*,#17358,.T.);
#22981=ORIENTED_EDGE('',*,*,#17359,.T.);
#22982=ORIENTED_EDGE('',*,*,#17355,.F.);
#22983=ORIENTED_EDGE('',*,*,#17360,.F.);
#22984=ORIENTED_EDGE('',*,*,#17361,.T.);
#22985=ORIENTED_EDGE('',*,*,#17362,.T.);
#22986=ORIENTED_EDGE('',*,*,#17358,.F.);
#22987=ORIENTED_EDGE('',*,*,#17363,.F.);
#22988=ORIENTED_EDGE('',*,*,#17364,.T.);
#22989=ORIENTED_EDGE('',*,*,#17365,.T.);
#22990=ORIENTED_EDGE('',*,*,#17361,.F.);
#22991=ORIENTED_EDGE('',*,*,#17366,.F.);
#22992=ORIENTED_EDGE('',*,*,#17347,.T.);
#22993=ORIENTED_EDGE('',*,*,#17367,.T.);
#22994=ORIENTED_EDGE('',*,*,#17364,.F.);
#22995=ORIENTED_EDGE('',*,*,#17368,.F.);
#22996=ORIENTED_EDGE('',*,*,#17369,.T.);
#22997=ORIENTED_EDGE('',*,*,#17370,.T.);
#22998=ORIENTED_EDGE('',*,*,#17371,.F.);
#22999=ORIENTED_EDGE('',*,*,#17372,.F.);
#23000=ORIENTED_EDGE('',*,*,#17373,.T.);
#23001=ORIENTED_EDGE('',*,*,#17374,.T.);
#23002=ORIENTED_EDGE('',*,*,#17369,.F.);
#23003=ORIENTED_EDGE('',*,*,#17375,.F.);
#23004=ORIENTED_EDGE('',*,*,#17376,.T.);
#23005=ORIENTED_EDGE('',*,*,#17377,.T.);
#23006=ORIENTED_EDGE('',*,*,#17373,.F.);
#23007=ORIENTED_EDGE('',*,*,#17378,.F.);
#23008=ORIENTED_EDGE('',*,*,#17379,.T.);
#23009=ORIENTED_EDGE('',*,*,#17380,.T.);
#23010=ORIENTED_EDGE('',*,*,#17376,.F.);
#23011=ORIENTED_EDGE('',*,*,#17381,.F.);
#23012=ORIENTED_EDGE('',*,*,#17382,.T.);
#23013=ORIENTED_EDGE('',*,*,#17383,.T.);
#23014=ORIENTED_EDGE('',*,*,#17379,.F.);
#23015=ORIENTED_EDGE('',*,*,#17384,.F.);
#23016=ORIENTED_EDGE('',*,*,#17385,.T.);
#23017=ORIENTED_EDGE('',*,*,#17386,.T.);
#23018=ORIENTED_EDGE('',*,*,#17382,.F.);
#23019=ORIENTED_EDGE('',*,*,#17387,.F.);
#23020=ORIENTED_EDGE('',*,*,#17388,.T.);
#23021=ORIENTED_EDGE('',*,*,#17389,.T.);
#23022=ORIENTED_EDGE('',*,*,#17385,.F.);
#23023=ORIENTED_EDGE('',*,*,#17390,.F.);
#23024=ORIENTED_EDGE('',*,*,#17391,.T.);
#23025=ORIENTED_EDGE('',*,*,#17392,.T.);
#23026=ORIENTED_EDGE('',*,*,#17388,.F.);
#23027=ORIENTED_EDGE('',*,*,#17393,.F.);
#23028=ORIENTED_EDGE('',*,*,#17394,.T.);
#23029=ORIENTED_EDGE('',*,*,#17395,.T.);
#23030=ORIENTED_EDGE('',*,*,#17391,.F.);
#23031=ORIENTED_EDGE('',*,*,#17396,.F.);
#23032=ORIENTED_EDGE('',*,*,#17397,.T.);
#23033=ORIENTED_EDGE('',*,*,#17398,.T.);
#23034=ORIENTED_EDGE('',*,*,#17394,.F.);
#23035=ORIENTED_EDGE('',*,*,#17399,.F.);
#23036=ORIENTED_EDGE('',*,*,#17400,.T.);
#23037=ORIENTED_EDGE('',*,*,#17401,.T.);
#23038=ORIENTED_EDGE('',*,*,#17397,.F.);
#23039=ORIENTED_EDGE('',*,*,#17402,.F.);
#23040=ORIENTED_EDGE('',*,*,#17371,.T.);
#23041=ORIENTED_EDGE('',*,*,#17403,.T.);
#23042=ORIENTED_EDGE('',*,*,#17400,.F.);
#23043=ORIENTED_EDGE('',*,*,#17403,.F.);
#23044=ORIENTED_EDGE('',*,*,#17370,.F.);
#23045=ORIENTED_EDGE('',*,*,#17374,.F.);
#23046=ORIENTED_EDGE('',*,*,#17377,.F.);
#23047=ORIENTED_EDGE('',*,*,#17380,.F.);
#23048=ORIENTED_EDGE('',*,*,#17383,.F.);
#23049=ORIENTED_EDGE('',*,*,#17386,.F.);
#23050=ORIENTED_EDGE('',*,*,#17389,.F.);
#23051=ORIENTED_EDGE('',*,*,#17392,.F.);
#23052=ORIENTED_EDGE('',*,*,#17395,.F.);
#23053=ORIENTED_EDGE('',*,*,#17398,.F.);
#23054=ORIENTED_EDGE('',*,*,#17401,.F.);
#23055=ORIENTED_EDGE('',*,*,#17367,.F.);
#23056=ORIENTED_EDGE('',*,*,#17346,.F.);
#23057=ORIENTED_EDGE('',*,*,#17350,.F.);
#23058=ORIENTED_EDGE('',*,*,#17353,.F.);
#23059=ORIENTED_EDGE('',*,*,#17356,.F.);
#23060=ORIENTED_EDGE('',*,*,#17359,.F.);
#23061=ORIENTED_EDGE('',*,*,#17362,.F.);
#23062=ORIENTED_EDGE('',*,*,#17365,.F.);
#23063=ORIENTED_EDGE('',*,*,#17404,.F.);
#23064=ORIENTED_EDGE('',*,*,#17405,.T.);
#23065=ORIENTED_EDGE('',*,*,#17406,.T.);
#23066=ORIENTED_EDGE('',*,*,#17407,.F.);
#23067=ORIENTED_EDGE('',*,*,#17408,.F.);
#23068=ORIENTED_EDGE('',*,*,#17409,.T.);
#23069=ORIENTED_EDGE('',*,*,#17410,.T.);
#23070=ORIENTED_EDGE('',*,*,#17405,.F.);
#23071=ORIENTED_EDGE('',*,*,#17411,.F.);
#23072=ORIENTED_EDGE('',*,*,#17412,.T.);
#23073=ORIENTED_EDGE('',*,*,#17413,.T.);
#23074=ORIENTED_EDGE('',*,*,#17409,.F.);
#23075=ORIENTED_EDGE('',*,*,#17414,.F.);
#23076=ORIENTED_EDGE('',*,*,#17415,.T.);
#23077=ORIENTED_EDGE('',*,*,#17416,.T.);
#23078=ORIENTED_EDGE('',*,*,#17412,.F.);
#23079=ORIENTED_EDGE('',*,*,#17417,.F.);
#23080=ORIENTED_EDGE('',*,*,#17418,.T.);
#23081=ORIENTED_EDGE('',*,*,#17419,.T.);
#23082=ORIENTED_EDGE('',*,*,#17415,.F.);
#23083=ORIENTED_EDGE('',*,*,#17420,.F.);
#23084=ORIENTED_EDGE('',*,*,#17421,.T.);
#23085=ORIENTED_EDGE('',*,*,#17422,.T.);
#23086=ORIENTED_EDGE('',*,*,#17418,.F.);
#23087=ORIENTED_EDGE('',*,*,#17423,.F.);
#23088=ORIENTED_EDGE('',*,*,#17424,.T.);
#23089=ORIENTED_EDGE('',*,*,#17425,.T.);
#23090=ORIENTED_EDGE('',*,*,#17421,.F.);
#23091=ORIENTED_EDGE('',*,*,#17426,.F.);
#23092=ORIENTED_EDGE('',*,*,#17427,.T.);
#23093=ORIENTED_EDGE('',*,*,#17428,.T.);
#23094=ORIENTED_EDGE('',*,*,#17424,.F.);
#23095=ORIENTED_EDGE('',*,*,#17429,.F.);
#23096=ORIENTED_EDGE('',*,*,#17430,.T.);
#23097=ORIENTED_EDGE('',*,*,#17431,.T.);
#23098=ORIENTED_EDGE('',*,*,#17427,.F.);
#23099=ORIENTED_EDGE('',*,*,#17432,.F.);
#23100=ORIENTED_EDGE('',*,*,#17433,.T.);
#23101=ORIENTED_EDGE('',*,*,#17434,.T.);
#23102=ORIENTED_EDGE('',*,*,#17430,.F.);
#23103=ORIENTED_EDGE('',*,*,#17435,.F.);
#23104=ORIENTED_EDGE('',*,*,#17436,.T.);
#23105=ORIENTED_EDGE('',*,*,#17437,.T.);
#23106=ORIENTED_EDGE('',*,*,#17433,.F.);
#23107=ORIENTED_EDGE('',*,*,#17438,.F.);
#23108=ORIENTED_EDGE('',*,*,#17439,.T.);
#23109=ORIENTED_EDGE('',*,*,#17440,.T.);
#23110=ORIENTED_EDGE('',*,*,#17436,.F.);
#23111=ORIENTED_EDGE('',*,*,#17441,.F.);
#23112=ORIENTED_EDGE('',*,*,#17442,.T.);
#23113=ORIENTED_EDGE('',*,*,#17443,.T.);
#23114=ORIENTED_EDGE('',*,*,#17439,.F.);
#23115=ORIENTED_EDGE('',*,*,#17444,.F.);
#23116=ORIENTED_EDGE('',*,*,#17445,.T.);
#23117=ORIENTED_EDGE('',*,*,#17446,.T.);
#23118=ORIENTED_EDGE('',*,*,#17442,.F.);
#23119=ORIENTED_EDGE('',*,*,#17447,.F.);
#23120=ORIENTED_EDGE('',*,*,#17448,.T.);
#23121=ORIENTED_EDGE('',*,*,#17449,.T.);
#23122=ORIENTED_EDGE('',*,*,#17445,.F.);
#23123=ORIENTED_EDGE('',*,*,#17450,.F.);
#23124=ORIENTED_EDGE('',*,*,#17451,.T.);
#23125=ORIENTED_EDGE('',*,*,#17452,.T.);
#23126=ORIENTED_EDGE('',*,*,#17448,.F.);
#23127=ORIENTED_EDGE('',*,*,#17453,.F.);
#23128=ORIENTED_EDGE('',*,*,#17454,.T.);
#23129=ORIENTED_EDGE('',*,*,#17455,.T.);
#23130=ORIENTED_EDGE('',*,*,#17451,.F.);
#23131=ORIENTED_EDGE('',*,*,#17456,.F.);
#23132=ORIENTED_EDGE('',*,*,#17457,.T.);
#23133=ORIENTED_EDGE('',*,*,#17458,.T.);
#23134=ORIENTED_EDGE('',*,*,#17454,.F.);
#23135=ORIENTED_EDGE('',*,*,#17459,.F.);
#23136=ORIENTED_EDGE('',*,*,#17460,.T.);
#23137=ORIENTED_EDGE('',*,*,#17461,.T.);
#23138=ORIENTED_EDGE('',*,*,#17457,.F.);
#23139=ORIENTED_EDGE('',*,*,#17462,.F.);
#23140=ORIENTED_EDGE('',*,*,#17463,.T.);
#23141=ORIENTED_EDGE('',*,*,#17464,.T.);
#23142=ORIENTED_EDGE('',*,*,#17460,.F.);
#23143=ORIENTED_EDGE('',*,*,#17465,.F.);
#23144=ORIENTED_EDGE('',*,*,#17466,.T.);
#23145=ORIENTED_EDGE('',*,*,#17467,.T.);
#23146=ORIENTED_EDGE('',*,*,#17463,.F.);
#23147=ORIENTED_EDGE('',*,*,#17468,.F.);
#23148=ORIENTED_EDGE('',*,*,#17469,.T.);
#23149=ORIENTED_EDGE('',*,*,#17470,.T.);
#23150=ORIENTED_EDGE('',*,*,#17466,.F.);
#23151=ORIENTED_EDGE('',*,*,#17471,.F.);
#23152=ORIENTED_EDGE('',*,*,#17472,.T.);
#23153=ORIENTED_EDGE('',*,*,#17473,.T.);
#23154=ORIENTED_EDGE('',*,*,#17469,.F.);
#23155=ORIENTED_EDGE('',*,*,#17474,.F.);
#23156=ORIENTED_EDGE('',*,*,#17475,.T.);
#23157=ORIENTED_EDGE('',*,*,#17476,.T.);
#23158=ORIENTED_EDGE('',*,*,#17472,.F.);
#23159=ORIENTED_EDGE('',*,*,#17477,.F.);
#23160=ORIENTED_EDGE('',*,*,#17478,.T.);
#23161=ORIENTED_EDGE('',*,*,#17479,.T.);
#23162=ORIENTED_EDGE('',*,*,#17475,.F.);
#23163=ORIENTED_EDGE('',*,*,#17480,.F.);
#23164=ORIENTED_EDGE('',*,*,#17481,.T.);
#23165=ORIENTED_EDGE('',*,*,#17482,.T.);
#23166=ORIENTED_EDGE('',*,*,#17478,.F.);
#23167=ORIENTED_EDGE('',*,*,#17483,.F.);
#23168=ORIENTED_EDGE('',*,*,#17484,.T.);
#23169=ORIENTED_EDGE('',*,*,#17485,.T.);
#23170=ORIENTED_EDGE('',*,*,#17481,.F.);
#23171=ORIENTED_EDGE('',*,*,#17486,.F.);
#23172=ORIENTED_EDGE('',*,*,#17487,.T.);
#23173=ORIENTED_EDGE('',*,*,#17488,.T.);
#23174=ORIENTED_EDGE('',*,*,#17484,.F.);
#23175=ORIENTED_EDGE('',*,*,#17489,.F.);
#23176=ORIENTED_EDGE('',*,*,#17490,.T.);
#23177=ORIENTED_EDGE('',*,*,#17491,.T.);
#23178=ORIENTED_EDGE('',*,*,#17487,.F.);
#23179=ORIENTED_EDGE('',*,*,#17492,.F.);
#23180=ORIENTED_EDGE('',*,*,#17407,.T.);
#23181=ORIENTED_EDGE('',*,*,#17493,.T.);
#23182=ORIENTED_EDGE('',*,*,#17490,.F.);
#23183=ORIENTED_EDGE('',*,*,#17493,.F.);
#23184=ORIENTED_EDGE('',*,*,#17406,.F.);
#23185=ORIENTED_EDGE('',*,*,#17410,.F.);
#23186=ORIENTED_EDGE('',*,*,#17413,.F.);
#23187=ORIENTED_EDGE('',*,*,#17416,.F.);
#23188=ORIENTED_EDGE('',*,*,#17419,.F.);
#23189=ORIENTED_EDGE('',*,*,#17422,.F.);
#23190=ORIENTED_EDGE('',*,*,#17425,.F.);
#23191=ORIENTED_EDGE('',*,*,#17428,.F.);
#23192=ORIENTED_EDGE('',*,*,#17431,.F.);
#23193=ORIENTED_EDGE('',*,*,#17434,.F.);
#23194=ORIENTED_EDGE('',*,*,#17437,.F.);
#23195=ORIENTED_EDGE('',*,*,#17440,.F.);
#23196=ORIENTED_EDGE('',*,*,#17443,.F.);
#23197=ORIENTED_EDGE('',*,*,#17446,.F.);
#23198=ORIENTED_EDGE('',*,*,#17449,.F.);
#23199=ORIENTED_EDGE('',*,*,#17452,.F.);
#23200=ORIENTED_EDGE('',*,*,#17455,.F.);
#23201=ORIENTED_EDGE('',*,*,#17458,.F.);
#23202=ORIENTED_EDGE('',*,*,#17461,.F.);
#23203=ORIENTED_EDGE('',*,*,#17464,.F.);
#23204=ORIENTED_EDGE('',*,*,#17467,.F.);
#23205=ORIENTED_EDGE('',*,*,#17470,.F.);
#23206=ORIENTED_EDGE('',*,*,#17473,.F.);
#23207=ORIENTED_EDGE('',*,*,#17476,.F.);
#23208=ORIENTED_EDGE('',*,*,#17479,.F.);
#23209=ORIENTED_EDGE('',*,*,#17482,.F.);
#23210=ORIENTED_EDGE('',*,*,#17485,.F.);
#23211=ORIENTED_EDGE('',*,*,#17488,.F.);
#23212=ORIENTED_EDGE('',*,*,#17491,.F.);
#23213=ORIENTED_EDGE('',*,*,#17344,.T.);
#23214=ORIENTED_EDGE('',*,*,#17366,.T.);
#23215=ORIENTED_EDGE('',*,*,#17363,.T.);
#23216=ORIENTED_EDGE('',*,*,#17360,.T.);
#23217=ORIENTED_EDGE('',*,*,#17357,.T.);
#23218=ORIENTED_EDGE('',*,*,#17354,.T.);
#23219=ORIENTED_EDGE('',*,*,#17351,.T.);
#23220=ORIENTED_EDGE('',*,*,#17348,.T.);
#23221=ORIENTED_EDGE('',*,*,#17494,.F.);
#23222=ORIENTED_EDGE('',*,*,#17495,.T.);
#23223=ORIENTED_EDGE('',*,*,#17496,.T.);
#23224=ORIENTED_EDGE('',*,*,#17497,.F.);
#23225=ORIENTED_EDGE('',*,*,#17498,.F.);
#23226=ORIENTED_EDGE('',*,*,#17499,.T.);
#23227=ORIENTED_EDGE('',*,*,#17500,.T.);
#23228=ORIENTED_EDGE('',*,*,#17495,.F.);
#23229=ORIENTED_EDGE('',*,*,#17501,.F.);
#23230=ORIENTED_EDGE('',*,*,#17502,.T.);
#23231=ORIENTED_EDGE('',*,*,#17503,.T.);
#23232=ORIENTED_EDGE('',*,*,#17499,.F.);
#23233=ORIENTED_EDGE('',*,*,#17504,.F.);
#23234=ORIENTED_EDGE('',*,*,#17505,.T.);
#23235=ORIENTED_EDGE('',*,*,#17506,.T.);
#23236=ORIENTED_EDGE('',*,*,#17502,.F.);
#23237=ORIENTED_EDGE('',*,*,#17507,.F.);
#23238=ORIENTED_EDGE('',*,*,#17508,.T.);
#23239=ORIENTED_EDGE('',*,*,#17509,.T.);
#23240=ORIENTED_EDGE('',*,*,#17505,.F.);
#23241=ORIENTED_EDGE('',*,*,#17510,.F.);
#23242=ORIENTED_EDGE('',*,*,#17511,.T.);
#23243=ORIENTED_EDGE('',*,*,#17512,.T.);
#23244=ORIENTED_EDGE('',*,*,#17508,.F.);
#23245=ORIENTED_EDGE('',*,*,#17513,.F.);
#23246=ORIENTED_EDGE('',*,*,#17514,.T.);
#23247=ORIENTED_EDGE('',*,*,#17515,.T.);
#23248=ORIENTED_EDGE('',*,*,#17511,.F.);
#23249=ORIENTED_EDGE('',*,*,#17516,.F.);
#23250=ORIENTED_EDGE('',*,*,#17497,.T.);
#23251=ORIENTED_EDGE('',*,*,#17517,.T.);
#23252=ORIENTED_EDGE('',*,*,#17514,.F.);
#23253=ORIENTED_EDGE('',*,*,#17518,.F.);
#23254=ORIENTED_EDGE('',*,*,#17519,.T.);
#23255=ORIENTED_EDGE('',*,*,#17520,.T.);
#23256=ORIENTED_EDGE('',*,*,#17521,.F.);
#23257=ORIENTED_EDGE('',*,*,#17522,.F.);
#23258=ORIENTED_EDGE('',*,*,#17523,.T.);
#23259=ORIENTED_EDGE('',*,*,#17524,.T.);
#23260=ORIENTED_EDGE('',*,*,#17519,.F.);
#23261=ORIENTED_EDGE('',*,*,#17525,.F.);
#23262=ORIENTED_EDGE('',*,*,#17526,.T.);
#23263=ORIENTED_EDGE('',*,*,#17527,.T.);
#23264=ORIENTED_EDGE('',*,*,#17523,.F.);
#23265=ORIENTED_EDGE('',*,*,#17528,.F.);
#23266=ORIENTED_EDGE('',*,*,#17529,.T.);
#23267=ORIENTED_EDGE('',*,*,#17530,.T.);
#23268=ORIENTED_EDGE('',*,*,#17526,.F.);
#23269=ORIENTED_EDGE('',*,*,#17531,.F.);
#23270=ORIENTED_EDGE('',*,*,#17532,.T.);
#23271=ORIENTED_EDGE('',*,*,#17533,.T.);
#23272=ORIENTED_EDGE('',*,*,#17529,.F.);
#23273=ORIENTED_EDGE('',*,*,#17534,.F.);
#23274=ORIENTED_EDGE('',*,*,#17535,.T.);
#23275=ORIENTED_EDGE('',*,*,#17536,.T.);
#23276=ORIENTED_EDGE('',*,*,#17532,.F.);
#23277=ORIENTED_EDGE('',*,*,#17537,.F.);
#23278=ORIENTED_EDGE('',*,*,#17538,.T.);
#23279=ORIENTED_EDGE('',*,*,#17539,.T.);
#23280=ORIENTED_EDGE('',*,*,#17535,.F.);
#23281=ORIENTED_EDGE('',*,*,#17540,.F.);
#23282=ORIENTED_EDGE('',*,*,#17541,.T.);
#23283=ORIENTED_EDGE('',*,*,#17542,.T.);
#23284=ORIENTED_EDGE('',*,*,#17538,.F.);
#23285=ORIENTED_EDGE('',*,*,#17543,.F.);
#23286=ORIENTED_EDGE('',*,*,#17544,.T.);
#23287=ORIENTED_EDGE('',*,*,#17545,.T.);
#23288=ORIENTED_EDGE('',*,*,#17541,.F.);
#23289=ORIENTED_EDGE('',*,*,#17546,.F.);
#23290=ORIENTED_EDGE('',*,*,#17547,.T.);
#23291=ORIENTED_EDGE('',*,*,#17548,.T.);
#23292=ORIENTED_EDGE('',*,*,#17544,.F.);
#23293=ORIENTED_EDGE('',*,*,#17549,.F.);
#23294=ORIENTED_EDGE('',*,*,#17550,.T.);
#23295=ORIENTED_EDGE('',*,*,#17551,.T.);
#23296=ORIENTED_EDGE('',*,*,#17547,.F.);
#23297=ORIENTED_EDGE('',*,*,#17552,.F.);
#23298=ORIENTED_EDGE('',*,*,#17521,.T.);
#23299=ORIENTED_EDGE('',*,*,#17553,.T.);
#23300=ORIENTED_EDGE('',*,*,#17550,.F.);
#23301=ORIENTED_EDGE('',*,*,#17553,.F.);
#23302=ORIENTED_EDGE('',*,*,#17520,.F.);
#23303=ORIENTED_EDGE('',*,*,#17524,.F.);
#23304=ORIENTED_EDGE('',*,*,#17527,.F.);
#23305=ORIENTED_EDGE('',*,*,#17530,.F.);
#23306=ORIENTED_EDGE('',*,*,#17533,.F.);
#23307=ORIENTED_EDGE('',*,*,#17536,.F.);
#23308=ORIENTED_EDGE('',*,*,#17539,.F.);
#23309=ORIENTED_EDGE('',*,*,#17542,.F.);
#23310=ORIENTED_EDGE('',*,*,#17545,.F.);
#23311=ORIENTED_EDGE('',*,*,#17548,.F.);
#23312=ORIENTED_EDGE('',*,*,#17551,.F.);
#23313=ORIENTED_EDGE('',*,*,#17517,.F.);
#23314=ORIENTED_EDGE('',*,*,#17496,.F.);
#23315=ORIENTED_EDGE('',*,*,#17500,.F.);
#23316=ORIENTED_EDGE('',*,*,#17503,.F.);
#23317=ORIENTED_EDGE('',*,*,#17506,.F.);
#23318=ORIENTED_EDGE('',*,*,#17509,.F.);
#23319=ORIENTED_EDGE('',*,*,#17512,.F.);
#23320=ORIENTED_EDGE('',*,*,#17515,.F.);
#23321=ORIENTED_EDGE('',*,*,#17554,.F.);
#23322=ORIENTED_EDGE('',*,*,#17555,.T.);
#23323=ORIENTED_EDGE('',*,*,#17556,.T.);
#23324=ORIENTED_EDGE('',*,*,#17557,.F.);
#23325=ORIENTED_EDGE('',*,*,#17558,.F.);
#23326=ORIENTED_EDGE('',*,*,#17559,.T.);
#23327=ORIENTED_EDGE('',*,*,#17560,.T.);
#23328=ORIENTED_EDGE('',*,*,#17555,.F.);
#23329=ORIENTED_EDGE('',*,*,#17561,.F.);
#23330=ORIENTED_EDGE('',*,*,#17562,.T.);
#23331=ORIENTED_EDGE('',*,*,#17563,.T.);
#23332=ORIENTED_EDGE('',*,*,#17559,.F.);
#23333=ORIENTED_EDGE('',*,*,#17564,.F.);
#23334=ORIENTED_EDGE('',*,*,#17565,.T.);
#23335=ORIENTED_EDGE('',*,*,#17566,.T.);
#23336=ORIENTED_EDGE('',*,*,#17562,.F.);
#23337=ORIENTED_EDGE('',*,*,#17567,.F.);
#23338=ORIENTED_EDGE('',*,*,#17568,.T.);
#23339=ORIENTED_EDGE('',*,*,#17569,.T.);
#23340=ORIENTED_EDGE('',*,*,#17565,.F.);
#23341=ORIENTED_EDGE('',*,*,#17570,.F.);
#23342=ORIENTED_EDGE('',*,*,#17571,.T.);
#23343=ORIENTED_EDGE('',*,*,#17572,.T.);
#23344=ORIENTED_EDGE('',*,*,#17568,.F.);
#23345=ORIENTED_EDGE('',*,*,#17573,.F.);
#23346=ORIENTED_EDGE('',*,*,#17574,.T.);
#23347=ORIENTED_EDGE('',*,*,#17575,.T.);
#23348=ORIENTED_EDGE('',*,*,#17571,.F.);
#23349=ORIENTED_EDGE('',*,*,#17576,.F.);
#23350=ORIENTED_EDGE('',*,*,#17577,.T.);
#23351=ORIENTED_EDGE('',*,*,#17578,.T.);
#23352=ORIENTED_EDGE('',*,*,#17574,.F.);
#23353=ORIENTED_EDGE('',*,*,#17579,.F.);
#23354=ORIENTED_EDGE('',*,*,#17580,.T.);
#23355=ORIENTED_EDGE('',*,*,#17581,.T.);
#23356=ORIENTED_EDGE('',*,*,#17577,.F.);
#23357=ORIENTED_EDGE('',*,*,#17582,.F.);
#23358=ORIENTED_EDGE('',*,*,#17583,.T.);
#23359=ORIENTED_EDGE('',*,*,#17584,.T.);
#23360=ORIENTED_EDGE('',*,*,#17580,.F.);
#23361=ORIENTED_EDGE('',*,*,#17585,.F.);
#23362=ORIENTED_EDGE('',*,*,#17586,.T.);
#23363=ORIENTED_EDGE('',*,*,#17587,.T.);
#23364=ORIENTED_EDGE('',*,*,#17583,.F.);
#23365=ORIENTED_EDGE('',*,*,#17588,.F.);
#23366=ORIENTED_EDGE('',*,*,#17589,.T.);
#23367=ORIENTED_EDGE('',*,*,#17590,.T.);
#23368=ORIENTED_EDGE('',*,*,#17586,.F.);
#23369=ORIENTED_EDGE('',*,*,#17591,.F.);
#23370=ORIENTED_EDGE('',*,*,#17592,.T.);
#23371=ORIENTED_EDGE('',*,*,#17593,.T.);
#23372=ORIENTED_EDGE('',*,*,#17589,.F.);
#23373=ORIENTED_EDGE('',*,*,#17594,.F.);
#23374=ORIENTED_EDGE('',*,*,#17595,.T.);
#23375=ORIENTED_EDGE('',*,*,#17596,.T.);
#23376=ORIENTED_EDGE('',*,*,#17592,.F.);
#23377=ORIENTED_EDGE('',*,*,#17597,.F.);
#23378=ORIENTED_EDGE('',*,*,#17598,.T.);
#23379=ORIENTED_EDGE('',*,*,#17599,.T.);
#23380=ORIENTED_EDGE('',*,*,#17595,.F.);
#23381=ORIENTED_EDGE('',*,*,#17600,.F.);
#23382=ORIENTED_EDGE('',*,*,#17601,.T.);
#23383=ORIENTED_EDGE('',*,*,#17602,.T.);
#23384=ORIENTED_EDGE('',*,*,#17598,.F.);
#23385=ORIENTED_EDGE('',*,*,#17603,.F.);
#23386=ORIENTED_EDGE('',*,*,#17604,.T.);
#23387=ORIENTED_EDGE('',*,*,#17605,.T.);
#23388=ORIENTED_EDGE('',*,*,#17601,.F.);
#23389=ORIENTED_EDGE('',*,*,#17606,.F.);
#23390=ORIENTED_EDGE('',*,*,#17607,.T.);
#23391=ORIENTED_EDGE('',*,*,#17608,.T.);
#23392=ORIENTED_EDGE('',*,*,#17604,.F.);
#23393=ORIENTED_EDGE('',*,*,#17609,.F.);
#23394=ORIENTED_EDGE('',*,*,#17610,.T.);
#23395=ORIENTED_EDGE('',*,*,#17611,.T.);
#23396=ORIENTED_EDGE('',*,*,#17607,.F.);
#23397=ORIENTED_EDGE('',*,*,#17612,.F.);
#23398=ORIENTED_EDGE('',*,*,#17613,.T.);
#23399=ORIENTED_EDGE('',*,*,#17614,.T.);
#23400=ORIENTED_EDGE('',*,*,#17610,.F.);
#23401=ORIENTED_EDGE('',*,*,#17615,.F.);
#23402=ORIENTED_EDGE('',*,*,#17616,.T.);
#23403=ORIENTED_EDGE('',*,*,#17617,.T.);
#23404=ORIENTED_EDGE('',*,*,#17613,.F.);
#23405=ORIENTED_EDGE('',*,*,#17618,.F.);
#23406=ORIENTED_EDGE('',*,*,#17557,.T.);
#23407=ORIENTED_EDGE('',*,*,#17619,.T.);
#23408=ORIENTED_EDGE('',*,*,#17616,.F.);
#23409=ORIENTED_EDGE('',*,*,#17619,.F.);
#23410=ORIENTED_EDGE('',*,*,#17556,.F.);
#23411=ORIENTED_EDGE('',*,*,#17560,.F.);
#23412=ORIENTED_EDGE('',*,*,#17563,.F.);
#23413=ORIENTED_EDGE('',*,*,#17566,.F.);
#23414=ORIENTED_EDGE('',*,*,#17569,.F.);
#23415=ORIENTED_EDGE('',*,*,#17572,.F.);
#23416=ORIENTED_EDGE('',*,*,#17575,.F.);
#23417=ORIENTED_EDGE('',*,*,#17578,.F.);
#23418=ORIENTED_EDGE('',*,*,#17581,.F.);
#23419=ORIENTED_EDGE('',*,*,#17584,.F.);
#23420=ORIENTED_EDGE('',*,*,#17587,.F.);
#23421=ORIENTED_EDGE('',*,*,#17590,.F.);
#23422=ORIENTED_EDGE('',*,*,#17593,.F.);
#23423=ORIENTED_EDGE('',*,*,#17596,.F.);
#23424=ORIENTED_EDGE('',*,*,#17599,.F.);
#23425=ORIENTED_EDGE('',*,*,#17602,.F.);
#23426=ORIENTED_EDGE('',*,*,#17605,.F.);
#23427=ORIENTED_EDGE('',*,*,#17608,.F.);
#23428=ORIENTED_EDGE('',*,*,#17611,.F.);
#23429=ORIENTED_EDGE('',*,*,#17614,.F.);
#23430=ORIENTED_EDGE('',*,*,#17617,.F.);
#23431=ORIENTED_EDGE('',*,*,#17494,.T.);
#23432=ORIENTED_EDGE('',*,*,#17516,.T.);
#23433=ORIENTED_EDGE('',*,*,#17513,.T.);
#23434=ORIENTED_EDGE('',*,*,#17510,.T.);
#23435=ORIENTED_EDGE('',*,*,#17507,.T.);
#23436=ORIENTED_EDGE('',*,*,#17504,.T.);
#23437=ORIENTED_EDGE('',*,*,#17501,.T.);
#23438=ORIENTED_EDGE('',*,*,#17498,.T.);
#23439=ORIENTED_EDGE('',*,*,#17620,.F.);
#23440=ORIENTED_EDGE('',*,*,#17621,.T.);
#23441=ORIENTED_EDGE('',*,*,#17622,.T.);
#23442=ORIENTED_EDGE('',*,*,#17623,.F.);
#23443=ORIENTED_EDGE('',*,*,#17624,.F.);
#23444=ORIENTED_EDGE('',*,*,#17625,.T.);
#23445=ORIENTED_EDGE('',*,*,#17626,.T.);
#23446=ORIENTED_EDGE('',*,*,#17621,.F.);
#23447=ORIENTED_EDGE('',*,*,#17627,.F.);
#23448=ORIENTED_EDGE('',*,*,#17628,.T.);
#23449=ORIENTED_EDGE('',*,*,#17629,.T.);
#23450=ORIENTED_EDGE('',*,*,#17625,.F.);
#23451=ORIENTED_EDGE('',*,*,#17630,.F.);
#23452=ORIENTED_EDGE('',*,*,#17631,.T.);
#23453=ORIENTED_EDGE('',*,*,#17632,.T.);
#23454=ORIENTED_EDGE('',*,*,#17628,.F.);
#23455=ORIENTED_EDGE('',*,*,#17633,.F.);
#23456=ORIENTED_EDGE('',*,*,#17634,.T.);
#23457=ORIENTED_EDGE('',*,*,#17635,.T.);
#23458=ORIENTED_EDGE('',*,*,#17631,.F.);
#23459=ORIENTED_EDGE('',*,*,#17636,.F.);
#23460=ORIENTED_EDGE('',*,*,#17637,.T.);
#23461=ORIENTED_EDGE('',*,*,#17638,.T.);
#23462=ORIENTED_EDGE('',*,*,#17634,.F.);
#23463=ORIENTED_EDGE('',*,*,#17639,.F.);
#23464=ORIENTED_EDGE('',*,*,#17640,.T.);
#23465=ORIENTED_EDGE('',*,*,#17641,.T.);
#23466=ORIENTED_EDGE('',*,*,#17637,.F.);
#23467=ORIENTED_EDGE('',*,*,#17642,.F.);
#23468=ORIENTED_EDGE('',*,*,#17623,.T.);
#23469=ORIENTED_EDGE('',*,*,#17643,.T.);
#23470=ORIENTED_EDGE('',*,*,#17640,.F.);
#23471=ORIENTED_EDGE('',*,*,#17644,.F.);
#23472=ORIENTED_EDGE('',*,*,#17645,.T.);
#23473=ORIENTED_EDGE('',*,*,#17646,.T.);
#23474=ORIENTED_EDGE('',*,*,#17647,.F.);
#23475=ORIENTED_EDGE('',*,*,#17648,.F.);
#23476=ORIENTED_EDGE('',*,*,#17649,.T.);
#23477=ORIENTED_EDGE('',*,*,#17650,.T.);
#23478=ORIENTED_EDGE('',*,*,#17645,.F.);
#23479=ORIENTED_EDGE('',*,*,#17651,.F.);
#23480=ORIENTED_EDGE('',*,*,#17652,.T.);
#23481=ORIENTED_EDGE('',*,*,#17653,.T.);
#23482=ORIENTED_EDGE('',*,*,#17649,.F.);
#23483=ORIENTED_EDGE('',*,*,#17654,.F.);
#23484=ORIENTED_EDGE('',*,*,#17655,.T.);
#23485=ORIENTED_EDGE('',*,*,#17656,.T.);
#23486=ORIENTED_EDGE('',*,*,#17652,.F.);
#23487=ORIENTED_EDGE('',*,*,#17657,.F.);
#23488=ORIENTED_EDGE('',*,*,#17658,.T.);
#23489=ORIENTED_EDGE('',*,*,#17659,.T.);
#23490=ORIENTED_EDGE('',*,*,#17655,.F.);
#23491=ORIENTED_EDGE('',*,*,#17660,.F.);
#23492=ORIENTED_EDGE('',*,*,#17661,.T.);
#23493=ORIENTED_EDGE('',*,*,#17662,.T.);
#23494=ORIENTED_EDGE('',*,*,#17658,.F.);
#23495=ORIENTED_EDGE('',*,*,#17663,.F.);
#23496=ORIENTED_EDGE('',*,*,#17664,.T.);
#23497=ORIENTED_EDGE('',*,*,#17665,.T.);
#23498=ORIENTED_EDGE('',*,*,#17661,.F.);
#23499=ORIENTED_EDGE('',*,*,#17666,.F.);
#23500=ORIENTED_EDGE('',*,*,#17667,.T.);
#23501=ORIENTED_EDGE('',*,*,#17668,.T.);
#23502=ORIENTED_EDGE('',*,*,#17664,.F.);
#23503=ORIENTED_EDGE('',*,*,#17669,.F.);
#23504=ORIENTED_EDGE('',*,*,#17670,.T.);
#23505=ORIENTED_EDGE('',*,*,#17671,.T.);
#23506=ORIENTED_EDGE('',*,*,#17667,.F.);
#23507=ORIENTED_EDGE('',*,*,#17672,.F.);
#23508=ORIENTED_EDGE('',*,*,#17673,.T.);
#23509=ORIENTED_EDGE('',*,*,#17674,.T.);
#23510=ORIENTED_EDGE('',*,*,#17670,.F.);
#23511=ORIENTED_EDGE('',*,*,#17675,.F.);
#23512=ORIENTED_EDGE('',*,*,#17676,.T.);
#23513=ORIENTED_EDGE('',*,*,#17677,.T.);
#23514=ORIENTED_EDGE('',*,*,#17673,.F.);
#23515=ORIENTED_EDGE('',*,*,#17678,.F.);
#23516=ORIENTED_EDGE('',*,*,#17647,.T.);
#23517=ORIENTED_EDGE('',*,*,#17679,.T.);
#23518=ORIENTED_EDGE('',*,*,#17676,.F.);
#23519=ORIENTED_EDGE('',*,*,#17679,.F.);
#23520=ORIENTED_EDGE('',*,*,#17646,.F.);
#23521=ORIENTED_EDGE('',*,*,#17650,.F.);
#23522=ORIENTED_EDGE('',*,*,#17653,.F.);
#23523=ORIENTED_EDGE('',*,*,#17656,.F.);
#23524=ORIENTED_EDGE('',*,*,#17659,.F.);
#23525=ORIENTED_EDGE('',*,*,#17662,.F.);
#23526=ORIENTED_EDGE('',*,*,#17665,.F.);
#23527=ORIENTED_EDGE('',*,*,#17668,.F.);
#23528=ORIENTED_EDGE('',*,*,#17671,.F.);
#23529=ORIENTED_EDGE('',*,*,#17674,.F.);
#23530=ORIENTED_EDGE('',*,*,#17677,.F.);
#23531=ORIENTED_EDGE('',*,*,#17643,.F.);
#23532=ORIENTED_EDGE('',*,*,#17622,.F.);
#23533=ORIENTED_EDGE('',*,*,#17626,.F.);
#23534=ORIENTED_EDGE('',*,*,#17629,.F.);
#23535=ORIENTED_EDGE('',*,*,#17632,.F.);
#23536=ORIENTED_EDGE('',*,*,#17635,.F.);
#23537=ORIENTED_EDGE('',*,*,#17638,.F.);
#23538=ORIENTED_EDGE('',*,*,#17641,.F.);
#23539=ORIENTED_EDGE('',*,*,#17680,.F.);
#23540=ORIENTED_EDGE('',*,*,#17681,.T.);
#23541=ORIENTED_EDGE('',*,*,#17682,.T.);
#23542=ORIENTED_EDGE('',*,*,#17683,.F.);
#23543=ORIENTED_EDGE('',*,*,#17684,.F.);
#23544=ORIENTED_EDGE('',*,*,#17685,.T.);
#23545=ORIENTED_EDGE('',*,*,#17686,.T.);
#23546=ORIENTED_EDGE('',*,*,#17681,.F.);
#23547=ORIENTED_EDGE('',*,*,#17687,.F.);
#23548=ORIENTED_EDGE('',*,*,#17688,.T.);
#23549=ORIENTED_EDGE('',*,*,#17689,.T.);
#23550=ORIENTED_EDGE('',*,*,#17685,.F.);
#23551=ORIENTED_EDGE('',*,*,#17690,.F.);
#23552=ORIENTED_EDGE('',*,*,#17691,.T.);
#23553=ORIENTED_EDGE('',*,*,#17692,.T.);
#23554=ORIENTED_EDGE('',*,*,#17688,.F.);
#23555=ORIENTED_EDGE('',*,*,#17693,.F.);
#23556=ORIENTED_EDGE('',*,*,#17694,.T.);
#23557=ORIENTED_EDGE('',*,*,#17695,.T.);
#23558=ORIENTED_EDGE('',*,*,#17691,.F.);
#23559=ORIENTED_EDGE('',*,*,#17696,.F.);
#23560=ORIENTED_EDGE('',*,*,#17697,.T.);
#23561=ORIENTED_EDGE('',*,*,#17698,.T.);
#23562=ORIENTED_EDGE('',*,*,#17694,.F.);
#23563=ORIENTED_EDGE('',*,*,#17699,.F.);
#23564=ORIENTED_EDGE('',*,*,#17700,.T.);
#23565=ORIENTED_EDGE('',*,*,#17701,.T.);
#23566=ORIENTED_EDGE('',*,*,#17697,.F.);
#23567=ORIENTED_EDGE('',*,*,#17702,.F.);
#23568=ORIENTED_EDGE('',*,*,#17703,.T.);
#23569=ORIENTED_EDGE('',*,*,#17704,.T.);
#23570=ORIENTED_EDGE('',*,*,#17700,.F.);
#23571=ORIENTED_EDGE('',*,*,#17705,.F.);
#23572=ORIENTED_EDGE('',*,*,#17683,.T.);
#23573=ORIENTED_EDGE('',*,*,#17706,.T.);
#23574=ORIENTED_EDGE('',*,*,#17703,.F.);
#23575=ORIENTED_EDGE('',*,*,#17706,.F.);
#23576=ORIENTED_EDGE('',*,*,#17682,.F.);
#23577=ORIENTED_EDGE('',*,*,#17686,.F.);
#23578=ORIENTED_EDGE('',*,*,#17689,.F.);
#23579=ORIENTED_EDGE('',*,*,#17692,.F.);
#23580=ORIENTED_EDGE('',*,*,#17695,.F.);
#23581=ORIENTED_EDGE('',*,*,#17698,.F.);
#23582=ORIENTED_EDGE('',*,*,#17701,.F.);
#23583=ORIENTED_EDGE('',*,*,#17704,.F.);
#23584=ORIENTED_EDGE('',*,*,#17620,.T.);
#23585=ORIENTED_EDGE('',*,*,#17642,.T.);
#23586=ORIENTED_EDGE('',*,*,#17639,.T.);
#23587=ORIENTED_EDGE('',*,*,#17636,.T.);
#23588=ORIENTED_EDGE('',*,*,#17633,.T.);
#23589=ORIENTED_EDGE('',*,*,#17630,.T.);
#23590=ORIENTED_EDGE('',*,*,#17627,.T.);
#23591=ORIENTED_EDGE('',*,*,#17624,.T.);
#23592=ORIENTED_EDGE('',*,*,#17707,.F.);
#23593=ORIENTED_EDGE('',*,*,#17708,.T.);
#23594=ORIENTED_EDGE('',*,*,#17709,.T.);
#23595=ORIENTED_EDGE('',*,*,#17710,.F.);
#23596=ORIENTED_EDGE('',*,*,#17711,.F.);
#23597=ORIENTED_EDGE('',*,*,#17712,.T.);
#23598=ORIENTED_EDGE('',*,*,#17713,.T.);
#23599=ORIENTED_EDGE('',*,*,#17708,.F.);
#23600=ORIENTED_EDGE('',*,*,#17714,.F.);
#23601=ORIENTED_EDGE('',*,*,#17715,.T.);
#23602=ORIENTED_EDGE('',*,*,#17716,.T.);
#23603=ORIENTED_EDGE('',*,*,#17712,.F.);
#23604=ORIENTED_EDGE('',*,*,#17717,.F.);
#23605=ORIENTED_EDGE('',*,*,#17718,.T.);
#23606=ORIENTED_EDGE('',*,*,#17719,.T.);
#23607=ORIENTED_EDGE('',*,*,#17715,.F.);
#23608=ORIENTED_EDGE('',*,*,#17720,.F.);
#23609=ORIENTED_EDGE('',*,*,#17721,.T.);
#23610=ORIENTED_EDGE('',*,*,#17722,.T.);
#23611=ORIENTED_EDGE('',*,*,#17718,.F.);
#23612=ORIENTED_EDGE('',*,*,#17723,.F.);
#23613=ORIENTED_EDGE('',*,*,#17724,.T.);
#23614=ORIENTED_EDGE('',*,*,#17725,.T.);
#23615=ORIENTED_EDGE('',*,*,#17721,.F.);
#23616=ORIENTED_EDGE('',*,*,#17726,.F.);
#23617=ORIENTED_EDGE('',*,*,#17727,.T.);
#23618=ORIENTED_EDGE('',*,*,#17728,.T.);
#23619=ORIENTED_EDGE('',*,*,#17724,.F.);
#23620=ORIENTED_EDGE('',*,*,#17729,.F.);
#23621=ORIENTED_EDGE('',*,*,#17710,.T.);
#23622=ORIENTED_EDGE('',*,*,#17730,.T.);
#23623=ORIENTED_EDGE('',*,*,#17727,.F.);
#23624=ORIENTED_EDGE('',*,*,#17731,.F.);
#23625=ORIENTED_EDGE('',*,*,#17732,.T.);
#23626=ORIENTED_EDGE('',*,*,#17733,.T.);
#23627=ORIENTED_EDGE('',*,*,#17734,.F.);
#23628=ORIENTED_EDGE('',*,*,#17735,.F.);
#23629=ORIENTED_EDGE('',*,*,#17736,.T.);
#23630=ORIENTED_EDGE('',*,*,#17737,.T.);
#23631=ORIENTED_EDGE('',*,*,#17732,.F.);
#23632=ORIENTED_EDGE('',*,*,#17738,.F.);
#23633=ORIENTED_EDGE('',*,*,#17739,.T.);
#23634=ORIENTED_EDGE('',*,*,#17740,.T.);
#23635=ORIENTED_EDGE('',*,*,#17736,.F.);
#23636=ORIENTED_EDGE('',*,*,#17741,.F.);
#23637=ORIENTED_EDGE('',*,*,#17742,.T.);
#23638=ORIENTED_EDGE('',*,*,#17743,.T.);
#23639=ORIENTED_EDGE('',*,*,#17739,.F.);
#23640=ORIENTED_EDGE('',*,*,#17744,.F.);
#23641=ORIENTED_EDGE('',*,*,#17745,.T.);
#23642=ORIENTED_EDGE('',*,*,#17746,.T.);
#23643=ORIENTED_EDGE('',*,*,#17742,.F.);
#23644=ORIENTED_EDGE('',*,*,#17747,.F.);
#23645=ORIENTED_EDGE('',*,*,#17748,.T.);
#23646=ORIENTED_EDGE('',*,*,#17749,.T.);
#23647=ORIENTED_EDGE('',*,*,#17745,.F.);
#23648=ORIENTED_EDGE('',*,*,#17750,.F.);
#23649=ORIENTED_EDGE('',*,*,#17751,.T.);
#23650=ORIENTED_EDGE('',*,*,#17752,.T.);
#23651=ORIENTED_EDGE('',*,*,#17748,.F.);
#23652=ORIENTED_EDGE('',*,*,#17753,.F.);
#23653=ORIENTED_EDGE('',*,*,#17754,.T.);
#23654=ORIENTED_EDGE('',*,*,#17755,.T.);
#23655=ORIENTED_EDGE('',*,*,#17751,.F.);
#23656=ORIENTED_EDGE('',*,*,#17756,.F.);
#23657=ORIENTED_EDGE('',*,*,#17757,.T.);
#23658=ORIENTED_EDGE('',*,*,#17758,.T.);
#23659=ORIENTED_EDGE('',*,*,#17754,.F.);
#23660=ORIENTED_EDGE('',*,*,#17759,.F.);
#23661=ORIENTED_EDGE('',*,*,#17760,.T.);
#23662=ORIENTED_EDGE('',*,*,#17761,.T.);
#23663=ORIENTED_EDGE('',*,*,#17757,.F.);
#23664=ORIENTED_EDGE('',*,*,#17762,.F.);
#23665=ORIENTED_EDGE('',*,*,#17763,.T.);
#23666=ORIENTED_EDGE('',*,*,#17764,.T.);
#23667=ORIENTED_EDGE('',*,*,#17760,.F.);
#23668=ORIENTED_EDGE('',*,*,#17765,.F.);
#23669=ORIENTED_EDGE('',*,*,#17734,.T.);
#23670=ORIENTED_EDGE('',*,*,#17766,.T.);
#23671=ORIENTED_EDGE('',*,*,#17763,.F.);
#23672=ORIENTED_EDGE('',*,*,#17766,.F.);
#23673=ORIENTED_EDGE('',*,*,#17733,.F.);
#23674=ORIENTED_EDGE('',*,*,#17737,.F.);
#23675=ORIENTED_EDGE('',*,*,#17740,.F.);
#23676=ORIENTED_EDGE('',*,*,#17743,.F.);
#23677=ORIENTED_EDGE('',*,*,#17746,.F.);
#23678=ORIENTED_EDGE('',*,*,#17749,.F.);
#23679=ORIENTED_EDGE('',*,*,#17752,.F.);
#23680=ORIENTED_EDGE('',*,*,#17755,.F.);
#23681=ORIENTED_EDGE('',*,*,#17758,.F.);
#23682=ORIENTED_EDGE('',*,*,#17761,.F.);
#23683=ORIENTED_EDGE('',*,*,#17764,.F.);
#23684=ORIENTED_EDGE('',*,*,#17730,.F.);
#23685=ORIENTED_EDGE('',*,*,#17709,.F.);
#23686=ORIENTED_EDGE('',*,*,#17713,.F.);
#23687=ORIENTED_EDGE('',*,*,#17716,.F.);
#23688=ORIENTED_EDGE('',*,*,#17719,.F.);
#23689=ORIENTED_EDGE('',*,*,#17722,.F.);
#23690=ORIENTED_EDGE('',*,*,#17725,.F.);
#23691=ORIENTED_EDGE('',*,*,#17728,.F.);
#23692=ORIENTED_EDGE('',*,*,#17707,.T.);
#23693=ORIENTED_EDGE('',*,*,#17729,.T.);
#23694=ORIENTED_EDGE('',*,*,#17726,.T.);
#23695=ORIENTED_EDGE('',*,*,#17723,.T.);
#23696=ORIENTED_EDGE('',*,*,#17720,.T.);
#23697=ORIENTED_EDGE('',*,*,#17717,.T.);
#23698=ORIENTED_EDGE('',*,*,#17714,.T.);
#23699=ORIENTED_EDGE('',*,*,#17711,.T.);
#23700=ORIENTED_EDGE('',*,*,#17767,.F.);
#23701=ORIENTED_EDGE('',*,*,#17768,.T.);
#23702=ORIENTED_EDGE('',*,*,#17769,.T.);
#23703=ORIENTED_EDGE('',*,*,#17770,.F.);
#23704=ORIENTED_EDGE('',*,*,#17771,.F.);
#23705=ORIENTED_EDGE('',*,*,#17772,.T.);
#23706=ORIENTED_EDGE('',*,*,#17773,.T.);
#23707=ORIENTED_EDGE('',*,*,#17768,.F.);
#23708=ORIENTED_EDGE('',*,*,#17774,.F.);
#23709=ORIENTED_EDGE('',*,*,#17775,.T.);
#23710=ORIENTED_EDGE('',*,*,#17776,.T.);
#23711=ORIENTED_EDGE('',*,*,#17772,.F.);
#23712=ORIENTED_EDGE('',*,*,#17777,.F.);
#23713=ORIENTED_EDGE('',*,*,#17778,.T.);
#23714=ORIENTED_EDGE('',*,*,#17779,.T.);
#23715=ORIENTED_EDGE('',*,*,#17775,.F.);
#23716=ORIENTED_EDGE('',*,*,#17780,.F.);
#23717=ORIENTED_EDGE('',*,*,#17781,.T.);
#23718=ORIENTED_EDGE('',*,*,#17782,.T.);
#23719=ORIENTED_EDGE('',*,*,#17778,.F.);
#23720=ORIENTED_EDGE('',*,*,#17783,.F.);
#23721=ORIENTED_EDGE('',*,*,#17784,.T.);
#23722=ORIENTED_EDGE('',*,*,#17785,.T.);
#23723=ORIENTED_EDGE('',*,*,#17781,.F.);
#23724=ORIENTED_EDGE('',*,*,#17786,.F.);
#23725=ORIENTED_EDGE('',*,*,#17787,.T.);
#23726=ORIENTED_EDGE('',*,*,#17788,.T.);
#23727=ORIENTED_EDGE('',*,*,#17784,.F.);
#23728=ORIENTED_EDGE('',*,*,#17789,.F.);
#23729=ORIENTED_EDGE('',*,*,#17770,.T.);
#23730=ORIENTED_EDGE('',*,*,#17790,.T.);
#23731=ORIENTED_EDGE('',*,*,#17787,.F.);
#23732=ORIENTED_EDGE('',*,*,#17791,.F.);
#23733=ORIENTED_EDGE('',*,*,#17792,.T.);
#23734=ORIENTED_EDGE('',*,*,#17793,.T.);
#23735=ORIENTED_EDGE('',*,*,#17794,.F.);
#23736=ORIENTED_EDGE('',*,*,#17795,.F.);
#23737=ORIENTED_EDGE('',*,*,#17796,.T.);
#23738=ORIENTED_EDGE('',*,*,#17797,.T.);
#23739=ORIENTED_EDGE('',*,*,#17792,.F.);
#23740=ORIENTED_EDGE('',*,*,#17798,.F.);
#23741=ORIENTED_EDGE('',*,*,#17799,.T.);
#23742=ORIENTED_EDGE('',*,*,#17800,.T.);
#23743=ORIENTED_EDGE('',*,*,#17796,.F.);
#23744=ORIENTED_EDGE('',*,*,#17801,.F.);
#23745=ORIENTED_EDGE('',*,*,#17802,.T.);
#23746=ORIENTED_EDGE('',*,*,#17803,.T.);
#23747=ORIENTED_EDGE('',*,*,#17799,.F.);
#23748=ORIENTED_EDGE('',*,*,#17804,.F.);
#23749=ORIENTED_EDGE('',*,*,#17805,.T.);
#23750=ORIENTED_EDGE('',*,*,#17806,.T.);
#23751=ORIENTED_EDGE('',*,*,#17802,.F.);
#23752=ORIENTED_EDGE('',*,*,#17807,.F.);
#23753=ORIENTED_EDGE('',*,*,#17808,.T.);
#23754=ORIENTED_EDGE('',*,*,#17809,.T.);
#23755=ORIENTED_EDGE('',*,*,#17805,.F.);
#23756=ORIENTED_EDGE('',*,*,#17810,.F.);
#23757=ORIENTED_EDGE('',*,*,#17811,.T.);
#23758=ORIENTED_EDGE('',*,*,#17812,.T.);
#23759=ORIENTED_EDGE('',*,*,#17808,.F.);
#23760=ORIENTED_EDGE('',*,*,#17813,.F.);
#23761=ORIENTED_EDGE('',*,*,#17814,.T.);
#23762=ORIENTED_EDGE('',*,*,#17815,.T.);
#23763=ORIENTED_EDGE('',*,*,#17811,.F.);
#23764=ORIENTED_EDGE('',*,*,#17816,.F.);
#23765=ORIENTED_EDGE('',*,*,#17817,.T.);
#23766=ORIENTED_EDGE('',*,*,#17818,.T.);
#23767=ORIENTED_EDGE('',*,*,#17814,.F.);
#23768=ORIENTED_EDGE('',*,*,#17819,.F.);
#23769=ORIENTED_EDGE('',*,*,#17820,.T.);
#23770=ORIENTED_EDGE('',*,*,#17821,.T.);
#23771=ORIENTED_EDGE('',*,*,#17817,.F.);
#23772=ORIENTED_EDGE('',*,*,#17822,.F.);
#23773=ORIENTED_EDGE('',*,*,#17823,.T.);
#23774=ORIENTED_EDGE('',*,*,#17824,.T.);
#23775=ORIENTED_EDGE('',*,*,#17820,.F.);
#23776=ORIENTED_EDGE('',*,*,#17825,.F.);
#23777=ORIENTED_EDGE('',*,*,#17794,.T.);
#23778=ORIENTED_EDGE('',*,*,#17826,.T.);
#23779=ORIENTED_EDGE('',*,*,#17823,.F.);
#23780=ORIENTED_EDGE('',*,*,#17826,.F.);
#23781=ORIENTED_EDGE('',*,*,#17793,.F.);
#23782=ORIENTED_EDGE('',*,*,#17797,.F.);
#23783=ORIENTED_EDGE('',*,*,#17800,.F.);
#23784=ORIENTED_EDGE('',*,*,#17803,.F.);
#23785=ORIENTED_EDGE('',*,*,#17806,.F.);
#23786=ORIENTED_EDGE('',*,*,#17809,.F.);
#23787=ORIENTED_EDGE('',*,*,#17812,.F.);
#23788=ORIENTED_EDGE('',*,*,#17815,.F.);
#23789=ORIENTED_EDGE('',*,*,#17818,.F.);
#23790=ORIENTED_EDGE('',*,*,#17821,.F.);
#23791=ORIENTED_EDGE('',*,*,#17824,.F.);
#23792=ORIENTED_EDGE('',*,*,#17790,.F.);
#23793=ORIENTED_EDGE('',*,*,#17769,.F.);
#23794=ORIENTED_EDGE('',*,*,#17773,.F.);
#23795=ORIENTED_EDGE('',*,*,#17776,.F.);
#23796=ORIENTED_EDGE('',*,*,#17779,.F.);
#23797=ORIENTED_EDGE('',*,*,#17782,.F.);
#23798=ORIENTED_EDGE('',*,*,#17785,.F.);
#23799=ORIENTED_EDGE('',*,*,#17788,.F.);
#23800=ORIENTED_EDGE('',*,*,#17827,.F.);
#23801=ORIENTED_EDGE('',*,*,#17828,.T.);
#23802=ORIENTED_EDGE('',*,*,#17829,.T.);
#23803=ORIENTED_EDGE('',*,*,#17830,.F.);
#23804=ORIENTED_EDGE('',*,*,#17831,.F.);
#23805=ORIENTED_EDGE('',*,*,#17832,.T.);
#23806=ORIENTED_EDGE('',*,*,#17833,.T.);
#23807=ORIENTED_EDGE('',*,*,#17828,.F.);
#23808=ORIENTED_EDGE('',*,*,#17834,.F.);
#23809=ORIENTED_EDGE('',*,*,#17835,.T.);
#23810=ORIENTED_EDGE('',*,*,#17836,.T.);
#23811=ORIENTED_EDGE('',*,*,#17832,.F.);
#23812=ORIENTED_EDGE('',*,*,#17837,.F.);
#23813=ORIENTED_EDGE('',*,*,#17838,.T.);
#23814=ORIENTED_EDGE('',*,*,#17839,.T.);
#23815=ORIENTED_EDGE('',*,*,#17835,.F.);
#23816=ORIENTED_EDGE('',*,*,#17840,.F.);
#23817=ORIENTED_EDGE('',*,*,#17841,.T.);
#23818=ORIENTED_EDGE('',*,*,#17842,.T.);
#23819=ORIENTED_EDGE('',*,*,#17838,.F.);
#23820=ORIENTED_EDGE('',*,*,#17843,.F.);
#23821=ORIENTED_EDGE('',*,*,#17844,.T.);
#23822=ORIENTED_EDGE('',*,*,#17845,.T.);
#23823=ORIENTED_EDGE('',*,*,#17841,.F.);
#23824=ORIENTED_EDGE('',*,*,#17846,.F.);
#23825=ORIENTED_EDGE('',*,*,#17847,.T.);
#23826=ORIENTED_EDGE('',*,*,#17848,.T.);
#23827=ORIENTED_EDGE('',*,*,#17844,.F.);
#23828=ORIENTED_EDGE('',*,*,#17849,.F.);
#23829=ORIENTED_EDGE('',*,*,#17850,.T.);
#23830=ORIENTED_EDGE('',*,*,#17851,.T.);
#23831=ORIENTED_EDGE('',*,*,#17847,.F.);
#23832=ORIENTED_EDGE('',*,*,#17852,.F.);
#23833=ORIENTED_EDGE('',*,*,#17830,.T.);
#23834=ORIENTED_EDGE('',*,*,#17853,.T.);
#23835=ORIENTED_EDGE('',*,*,#17850,.F.);
#23836=ORIENTED_EDGE('',*,*,#17853,.F.);
#23837=ORIENTED_EDGE('',*,*,#17829,.F.);
#23838=ORIENTED_EDGE('',*,*,#17833,.F.);
#23839=ORIENTED_EDGE('',*,*,#17836,.F.);
#23840=ORIENTED_EDGE('',*,*,#17839,.F.);
#23841=ORIENTED_EDGE('',*,*,#17842,.F.);
#23842=ORIENTED_EDGE('',*,*,#17845,.F.);
#23843=ORIENTED_EDGE('',*,*,#17848,.F.);
#23844=ORIENTED_EDGE('',*,*,#17851,.F.);
#23845=ORIENTED_EDGE('',*,*,#17767,.T.);
#23846=ORIENTED_EDGE('',*,*,#17789,.T.);
#23847=ORIENTED_EDGE('',*,*,#17786,.T.);
#23848=ORIENTED_EDGE('',*,*,#17783,.T.);
#23849=ORIENTED_EDGE('',*,*,#17780,.T.);
#23850=ORIENTED_EDGE('',*,*,#17777,.T.);
#23851=ORIENTED_EDGE('',*,*,#17774,.T.);
#23852=ORIENTED_EDGE('',*,*,#17771,.T.);
#23853=ORIENTED_EDGE('',*,*,#17854,.F.);
#23854=ORIENTED_EDGE('',*,*,#17855,.T.);
#23855=ORIENTED_EDGE('',*,*,#17856,.T.);
#23856=ORIENTED_EDGE('',*,*,#17857,.F.);
#23857=ORIENTED_EDGE('',*,*,#17858,.F.);
#23858=ORIENTED_EDGE('',*,*,#17859,.T.);
#23859=ORIENTED_EDGE('',*,*,#17860,.T.);
#23860=ORIENTED_EDGE('',*,*,#17855,.F.);
#23861=ORIENTED_EDGE('',*,*,#17861,.F.);
#23862=ORIENTED_EDGE('',*,*,#17862,.T.);
#23863=ORIENTED_EDGE('',*,*,#17863,.T.);
#23864=ORIENTED_EDGE('',*,*,#17859,.F.);
#23865=ORIENTED_EDGE('',*,*,#17864,.F.);
#23866=ORIENTED_EDGE('',*,*,#17865,.T.);
#23867=ORIENTED_EDGE('',*,*,#17866,.T.);
#23868=ORIENTED_EDGE('',*,*,#17862,.F.);
#23869=ORIENTED_EDGE('',*,*,#17867,.F.);
#23870=ORIENTED_EDGE('',*,*,#17868,.T.);
#23871=ORIENTED_EDGE('',*,*,#17869,.T.);
#23872=ORIENTED_EDGE('',*,*,#17865,.F.);
#23873=ORIENTED_EDGE('',*,*,#17870,.F.);
#23874=ORIENTED_EDGE('',*,*,#17871,.T.);
#23875=ORIENTED_EDGE('',*,*,#17872,.T.);
#23876=ORIENTED_EDGE('',*,*,#17868,.F.);
#23877=ORIENTED_EDGE('',*,*,#17873,.F.);
#23878=ORIENTED_EDGE('',*,*,#17874,.T.);
#23879=ORIENTED_EDGE('',*,*,#17875,.T.);
#23880=ORIENTED_EDGE('',*,*,#17871,.F.);
#23881=ORIENTED_EDGE('',*,*,#17876,.F.);
#23882=ORIENTED_EDGE('',*,*,#17857,.T.);
#23883=ORIENTED_EDGE('',*,*,#17877,.T.);
#23884=ORIENTED_EDGE('',*,*,#17874,.F.);
#23885=ORIENTED_EDGE('',*,*,#17878,.F.);
#23886=ORIENTED_EDGE('',*,*,#17879,.T.);
#23887=ORIENTED_EDGE('',*,*,#17880,.T.);
#23888=ORIENTED_EDGE('',*,*,#17881,.F.);
#23889=ORIENTED_EDGE('',*,*,#17882,.F.);
#23890=ORIENTED_EDGE('',*,*,#17883,.T.);
#23891=ORIENTED_EDGE('',*,*,#17884,.T.);
#23892=ORIENTED_EDGE('',*,*,#17879,.F.);
#23893=ORIENTED_EDGE('',*,*,#17885,.F.);
#23894=ORIENTED_EDGE('',*,*,#17886,.T.);
#23895=ORIENTED_EDGE('',*,*,#17887,.T.);
#23896=ORIENTED_EDGE('',*,*,#17883,.F.);
#23897=ORIENTED_EDGE('',*,*,#17888,.F.);
#23898=ORIENTED_EDGE('',*,*,#17889,.T.);
#23899=ORIENTED_EDGE('',*,*,#17890,.T.);
#23900=ORIENTED_EDGE('',*,*,#17886,.F.);
#23901=ORIENTED_EDGE('',*,*,#17891,.F.);
#23902=ORIENTED_EDGE('',*,*,#17892,.T.);
#23903=ORIENTED_EDGE('',*,*,#17893,.T.);
#23904=ORIENTED_EDGE('',*,*,#17889,.F.);
#23905=ORIENTED_EDGE('',*,*,#17894,.F.);
#23906=ORIENTED_EDGE('',*,*,#17895,.T.);
#23907=ORIENTED_EDGE('',*,*,#17896,.T.);
#23908=ORIENTED_EDGE('',*,*,#17892,.F.);
#23909=ORIENTED_EDGE('',*,*,#17897,.F.);
#23910=ORIENTED_EDGE('',*,*,#17898,.T.);
#23911=ORIENTED_EDGE('',*,*,#17899,.T.);
#23912=ORIENTED_EDGE('',*,*,#17895,.F.);
#23913=ORIENTED_EDGE('',*,*,#17900,.F.);
#23914=ORIENTED_EDGE('',*,*,#17901,.T.);
#23915=ORIENTED_EDGE('',*,*,#17902,.T.);
#23916=ORIENTED_EDGE('',*,*,#17898,.F.);
#23917=ORIENTED_EDGE('',*,*,#17903,.F.);
#23918=ORIENTED_EDGE('',*,*,#17904,.T.);
#23919=ORIENTED_EDGE('',*,*,#17905,.T.);
#23920=ORIENTED_EDGE('',*,*,#17901,.F.);
#23921=ORIENTED_EDGE('',*,*,#17906,.F.);
#23922=ORIENTED_EDGE('',*,*,#17907,.T.);
#23923=ORIENTED_EDGE('',*,*,#17908,.T.);
#23924=ORIENTED_EDGE('',*,*,#17904,.F.);
#23925=ORIENTED_EDGE('',*,*,#17909,.F.);
#23926=ORIENTED_EDGE('',*,*,#17910,.T.);
#23927=ORIENTED_EDGE('',*,*,#17911,.T.);
#23928=ORIENTED_EDGE('',*,*,#17907,.F.);
#23929=ORIENTED_EDGE('',*,*,#17912,.F.);
#23930=ORIENTED_EDGE('',*,*,#17881,.T.);
#23931=ORIENTED_EDGE('',*,*,#17913,.T.);
#23932=ORIENTED_EDGE('',*,*,#17910,.F.);
#23933=ORIENTED_EDGE('',*,*,#17913,.F.);
#23934=ORIENTED_EDGE('',*,*,#17880,.F.);
#23935=ORIENTED_EDGE('',*,*,#17884,.F.);
#23936=ORIENTED_EDGE('',*,*,#17887,.F.);
#23937=ORIENTED_EDGE('',*,*,#17890,.F.);
#23938=ORIENTED_EDGE('',*,*,#17893,.F.);
#23939=ORIENTED_EDGE('',*,*,#17896,.F.);
#23940=ORIENTED_EDGE('',*,*,#17899,.F.);
#23941=ORIENTED_EDGE('',*,*,#17902,.F.);
#23942=ORIENTED_EDGE('',*,*,#17905,.F.);
#23943=ORIENTED_EDGE('',*,*,#17908,.F.);
#23944=ORIENTED_EDGE('',*,*,#17911,.F.);
#23945=ORIENTED_EDGE('',*,*,#17877,.F.);
#23946=ORIENTED_EDGE('',*,*,#17856,.F.);
#23947=ORIENTED_EDGE('',*,*,#17860,.F.);
#23948=ORIENTED_EDGE('',*,*,#17863,.F.);
#23949=ORIENTED_EDGE('',*,*,#17866,.F.);
#23950=ORIENTED_EDGE('',*,*,#17869,.F.);
#23951=ORIENTED_EDGE('',*,*,#17872,.F.);
#23952=ORIENTED_EDGE('',*,*,#17875,.F.);
#23953=ORIENTED_EDGE('',*,*,#17914,.F.);
#23954=ORIENTED_EDGE('',*,*,#17915,.T.);
#23955=ORIENTED_EDGE('',*,*,#17916,.T.);
#23956=ORIENTED_EDGE('',*,*,#17917,.F.);
#23957=ORIENTED_EDGE('',*,*,#17918,.F.);
#23958=ORIENTED_EDGE('',*,*,#17919,.T.);
#23959=ORIENTED_EDGE('',*,*,#17920,.T.);
#23960=ORIENTED_EDGE('',*,*,#17915,.F.);
#23961=ORIENTED_EDGE('',*,*,#17921,.F.);
#23962=ORIENTED_EDGE('',*,*,#17922,.T.);
#23963=ORIENTED_EDGE('',*,*,#17923,.T.);
#23964=ORIENTED_EDGE('',*,*,#17919,.F.);
#23965=ORIENTED_EDGE('',*,*,#17924,.F.);
#23966=ORIENTED_EDGE('',*,*,#17925,.T.);
#23967=ORIENTED_EDGE('',*,*,#17926,.T.);
#23968=ORIENTED_EDGE('',*,*,#17922,.F.);
#23969=ORIENTED_EDGE('',*,*,#17927,.F.);
#23970=ORIENTED_EDGE('',*,*,#17928,.T.);
#23971=ORIENTED_EDGE('',*,*,#17929,.T.);
#23972=ORIENTED_EDGE('',*,*,#17925,.F.);
#23973=ORIENTED_EDGE('',*,*,#17930,.F.);
#23974=ORIENTED_EDGE('',*,*,#17931,.T.);
#23975=ORIENTED_EDGE('',*,*,#17932,.T.);
#23976=ORIENTED_EDGE('',*,*,#17928,.F.);
#23977=ORIENTED_EDGE('',*,*,#17933,.F.);
#23978=ORIENTED_EDGE('',*,*,#17934,.T.);
#23979=ORIENTED_EDGE('',*,*,#17935,.T.);
#23980=ORIENTED_EDGE('',*,*,#17931,.F.);
#23981=ORIENTED_EDGE('',*,*,#17936,.F.);
#23982=ORIENTED_EDGE('',*,*,#17937,.T.);
#23983=ORIENTED_EDGE('',*,*,#17938,.T.);
#23984=ORIENTED_EDGE('',*,*,#17934,.F.);
#23985=ORIENTED_EDGE('',*,*,#17939,.F.);
#23986=ORIENTED_EDGE('',*,*,#17940,.T.);
#23987=ORIENTED_EDGE('',*,*,#17941,.T.);
#23988=ORIENTED_EDGE('',*,*,#17937,.F.);
#23989=ORIENTED_EDGE('',*,*,#17942,.F.);
#23990=ORIENTED_EDGE('',*,*,#17943,.T.);
#23991=ORIENTED_EDGE('',*,*,#17944,.T.);
#23992=ORIENTED_EDGE('',*,*,#17940,.F.);
#23993=ORIENTED_EDGE('',*,*,#17945,.F.);
#23994=ORIENTED_EDGE('',*,*,#17946,.T.);
#23995=ORIENTED_EDGE('',*,*,#17947,.T.);
#23996=ORIENTED_EDGE('',*,*,#17943,.F.);
#23997=ORIENTED_EDGE('',*,*,#17948,.F.);
#23998=ORIENTED_EDGE('',*,*,#17949,.T.);
#23999=ORIENTED_EDGE('',*,*,#17950,.T.);
#24000=ORIENTED_EDGE('',*,*,#17946,.F.);
#24001=ORIENTED_EDGE('',*,*,#17951,.F.);
#24002=ORIENTED_EDGE('',*,*,#17952,.T.);
#24003=ORIENTED_EDGE('',*,*,#17953,.T.);
#24004=ORIENTED_EDGE('',*,*,#17949,.F.);
#24005=ORIENTED_EDGE('',*,*,#17954,.F.);
#24006=ORIENTED_EDGE('',*,*,#17955,.T.);
#24007=ORIENTED_EDGE('',*,*,#17956,.T.);
#24008=ORIENTED_EDGE('',*,*,#17952,.F.);
#24009=ORIENTED_EDGE('',*,*,#17957,.F.);
#24010=ORIENTED_EDGE('',*,*,#17958,.T.);
#24011=ORIENTED_EDGE('',*,*,#17959,.T.);
#24012=ORIENTED_EDGE('',*,*,#17955,.F.);
#24013=ORIENTED_EDGE('',*,*,#17960,.F.);
#24014=ORIENTED_EDGE('',*,*,#17961,.T.);
#24015=ORIENTED_EDGE('',*,*,#17962,.T.);
#24016=ORIENTED_EDGE('',*,*,#17958,.F.);
#24017=ORIENTED_EDGE('',*,*,#17963,.F.);
#24018=ORIENTED_EDGE('',*,*,#17964,.T.);
#24019=ORIENTED_EDGE('',*,*,#17965,.T.);
#24020=ORIENTED_EDGE('',*,*,#17961,.F.);
#24021=ORIENTED_EDGE('',*,*,#17966,.F.);
#24022=ORIENTED_EDGE('',*,*,#17967,.T.);
#24023=ORIENTED_EDGE('',*,*,#17968,.T.);
#24024=ORIENTED_EDGE('',*,*,#17964,.F.);
#24025=ORIENTED_EDGE('',*,*,#17969,.F.);
#24026=ORIENTED_EDGE('',*,*,#17970,.T.);
#24027=ORIENTED_EDGE('',*,*,#17971,.T.);
#24028=ORIENTED_EDGE('',*,*,#17967,.F.);
#24029=ORIENTED_EDGE('',*,*,#17972,.F.);
#24030=ORIENTED_EDGE('',*,*,#17973,.T.);
#24031=ORIENTED_EDGE('',*,*,#17974,.T.);
#24032=ORIENTED_EDGE('',*,*,#17970,.F.);
#24033=ORIENTED_EDGE('',*,*,#17975,.F.);
#24034=ORIENTED_EDGE('',*,*,#17976,.T.);
#24035=ORIENTED_EDGE('',*,*,#17977,.T.);
#24036=ORIENTED_EDGE('',*,*,#17973,.F.);
#24037=ORIENTED_EDGE('',*,*,#17978,.F.);
#24038=ORIENTED_EDGE('',*,*,#17917,.T.);
#24039=ORIENTED_EDGE('',*,*,#17979,.T.);
#24040=ORIENTED_EDGE('',*,*,#17976,.F.);
#24041=ORIENTED_EDGE('',*,*,#17979,.F.);
#24042=ORIENTED_EDGE('',*,*,#17916,.F.);
#24043=ORIENTED_EDGE('',*,*,#17920,.F.);
#24044=ORIENTED_EDGE('',*,*,#17923,.F.);
#24045=ORIENTED_EDGE('',*,*,#17926,.F.);
#24046=ORIENTED_EDGE('',*,*,#17929,.F.);
#24047=ORIENTED_EDGE('',*,*,#17932,.F.);
#24048=ORIENTED_EDGE('',*,*,#17935,.F.);
#24049=ORIENTED_EDGE('',*,*,#17938,.F.);
#24050=ORIENTED_EDGE('',*,*,#17941,.F.);
#24051=ORIENTED_EDGE('',*,*,#17944,.F.);
#24052=ORIENTED_EDGE('',*,*,#17947,.F.);
#24053=ORIENTED_EDGE('',*,*,#17950,.F.);
#24054=ORIENTED_EDGE('',*,*,#17953,.F.);
#24055=ORIENTED_EDGE('',*,*,#17956,.F.);
#24056=ORIENTED_EDGE('',*,*,#17959,.F.);
#24057=ORIENTED_EDGE('',*,*,#17962,.F.);
#24058=ORIENTED_EDGE('',*,*,#17965,.F.);
#24059=ORIENTED_EDGE('',*,*,#17968,.F.);
#24060=ORIENTED_EDGE('',*,*,#17971,.F.);
#24061=ORIENTED_EDGE('',*,*,#17974,.F.);
#24062=ORIENTED_EDGE('',*,*,#17977,.F.);
#24063=ORIENTED_EDGE('',*,*,#17854,.T.);
#24064=ORIENTED_EDGE('',*,*,#17876,.T.);
#24065=ORIENTED_EDGE('',*,*,#17873,.T.);
#24066=ORIENTED_EDGE('',*,*,#17870,.T.);
#24067=ORIENTED_EDGE('',*,*,#17867,.T.);
#24068=ORIENTED_EDGE('',*,*,#17864,.T.);
#24069=ORIENTED_EDGE('',*,*,#17861,.T.);
#24070=ORIENTED_EDGE('',*,*,#17858,.T.);
#24071=ORIENTED_EDGE('',*,*,#17980,.F.);
#24072=ORIENTED_EDGE('',*,*,#17981,.T.);
#24073=ORIENTED_EDGE('',*,*,#17982,.T.);
#24074=ORIENTED_EDGE('',*,*,#17983,.F.);
#24075=ORIENTED_EDGE('',*,*,#17984,.F.);
#24076=ORIENTED_EDGE('',*,*,#17985,.T.);
#24077=ORIENTED_EDGE('',*,*,#17986,.T.);
#24078=ORIENTED_EDGE('',*,*,#17981,.F.);
#24079=ORIENTED_EDGE('',*,*,#17987,.F.);
#24080=ORIENTED_EDGE('',*,*,#17988,.T.);
#24081=ORIENTED_EDGE('',*,*,#17989,.T.);
#24082=ORIENTED_EDGE('',*,*,#17985,.F.);
#24083=ORIENTED_EDGE('',*,*,#17990,.F.);
#24084=ORIENTED_EDGE('',*,*,#17991,.T.);
#24085=ORIENTED_EDGE('',*,*,#17992,.T.);
#24086=ORIENTED_EDGE('',*,*,#17988,.F.);
#24087=ORIENTED_EDGE('',*,*,#17993,.F.);
#24088=ORIENTED_EDGE('',*,*,#17994,.T.);
#24089=ORIENTED_EDGE('',*,*,#17995,.T.);
#24090=ORIENTED_EDGE('',*,*,#17991,.F.);
#24091=ORIENTED_EDGE('',*,*,#17996,.F.);
#24092=ORIENTED_EDGE('',*,*,#17997,.T.);
#24093=ORIENTED_EDGE('',*,*,#17998,.T.);
#24094=ORIENTED_EDGE('',*,*,#17994,.F.);
#24095=ORIENTED_EDGE('',*,*,#17999,.F.);
#24096=ORIENTED_EDGE('',*,*,#18000,.T.);
#24097=ORIENTED_EDGE('',*,*,#18001,.T.);
#24098=ORIENTED_EDGE('',*,*,#17997,.F.);
#24099=ORIENTED_EDGE('',*,*,#18002,.F.);
#24100=ORIENTED_EDGE('',*,*,#17983,.T.);
#24101=ORIENTED_EDGE('',*,*,#18003,.T.);
#24102=ORIENTED_EDGE('',*,*,#18000,.F.);
#24103=ORIENTED_EDGE('',*,*,#18004,.F.);
#24104=ORIENTED_EDGE('',*,*,#18005,.T.);
#24105=ORIENTED_EDGE('',*,*,#18006,.T.);
#24106=ORIENTED_EDGE('',*,*,#18007,.F.);
#24107=ORIENTED_EDGE('',*,*,#18008,.F.);
#24108=ORIENTED_EDGE('',*,*,#18009,.T.);
#24109=ORIENTED_EDGE('',*,*,#18010,.T.);
#24110=ORIENTED_EDGE('',*,*,#18005,.F.);
#24111=ORIENTED_EDGE('',*,*,#18011,.F.);
#24112=ORIENTED_EDGE('',*,*,#18012,.T.);
#24113=ORIENTED_EDGE('',*,*,#18013,.T.);
#24114=ORIENTED_EDGE('',*,*,#18009,.F.);
#24115=ORIENTED_EDGE('',*,*,#18014,.F.);
#24116=ORIENTED_EDGE('',*,*,#18015,.T.);
#24117=ORIENTED_EDGE('',*,*,#18016,.T.);
#24118=ORIENTED_EDGE('',*,*,#18012,.F.);
#24119=ORIENTED_EDGE('',*,*,#18017,.F.);
#24120=ORIENTED_EDGE('',*,*,#18018,.T.);
#24121=ORIENTED_EDGE('',*,*,#18019,.T.);
#24122=ORIENTED_EDGE('',*,*,#18015,.F.);
#24123=ORIENTED_EDGE('',*,*,#18020,.F.);
#24124=ORIENTED_EDGE('',*,*,#18021,.T.);
#24125=ORIENTED_EDGE('',*,*,#18022,.T.);
#24126=ORIENTED_EDGE('',*,*,#18018,.F.);
#24127=ORIENTED_EDGE('',*,*,#18023,.F.);
#24128=ORIENTED_EDGE('',*,*,#18024,.T.);
#24129=ORIENTED_EDGE('',*,*,#18025,.T.);
#24130=ORIENTED_EDGE('',*,*,#18021,.F.);
#24131=ORIENTED_EDGE('',*,*,#18026,.F.);
#24132=ORIENTED_EDGE('',*,*,#18027,.T.);
#24133=ORIENTED_EDGE('',*,*,#18028,.T.);
#24134=ORIENTED_EDGE('',*,*,#18024,.F.);
#24135=ORIENTED_EDGE('',*,*,#18029,.F.);
#24136=ORIENTED_EDGE('',*,*,#18030,.T.);
#24137=ORIENTED_EDGE('',*,*,#18031,.T.);
#24138=ORIENTED_EDGE('',*,*,#18027,.F.);
#24139=ORIENTED_EDGE('',*,*,#18032,.F.);
#24140=ORIENTED_EDGE('',*,*,#18033,.T.);
#24141=ORIENTED_EDGE('',*,*,#18034,.T.);
#24142=ORIENTED_EDGE('',*,*,#18030,.F.);
#24143=ORIENTED_EDGE('',*,*,#18035,.F.);
#24144=ORIENTED_EDGE('',*,*,#18036,.T.);
#24145=ORIENTED_EDGE('',*,*,#18037,.T.);
#24146=ORIENTED_EDGE('',*,*,#18033,.F.);
#24147=ORIENTED_EDGE('',*,*,#18038,.F.);
#24148=ORIENTED_EDGE('',*,*,#18007,.T.);
#24149=ORIENTED_EDGE('',*,*,#18039,.T.);
#24150=ORIENTED_EDGE('',*,*,#18036,.F.);
#24151=ORIENTED_EDGE('',*,*,#18039,.F.);
#24152=ORIENTED_EDGE('',*,*,#18006,.F.);
#24153=ORIENTED_EDGE('',*,*,#18010,.F.);
#24154=ORIENTED_EDGE('',*,*,#18013,.F.);
#24155=ORIENTED_EDGE('',*,*,#18016,.F.);
#24156=ORIENTED_EDGE('',*,*,#18019,.F.);
#24157=ORIENTED_EDGE('',*,*,#18022,.F.);
#24158=ORIENTED_EDGE('',*,*,#18025,.F.);
#24159=ORIENTED_EDGE('',*,*,#18028,.F.);
#24160=ORIENTED_EDGE('',*,*,#18031,.F.);
#24161=ORIENTED_EDGE('',*,*,#18034,.F.);
#24162=ORIENTED_EDGE('',*,*,#18037,.F.);
#24163=ORIENTED_EDGE('',*,*,#18003,.F.);
#24164=ORIENTED_EDGE('',*,*,#17982,.F.);
#24165=ORIENTED_EDGE('',*,*,#17986,.F.);
#24166=ORIENTED_EDGE('',*,*,#17989,.F.);
#24167=ORIENTED_EDGE('',*,*,#17992,.F.);
#24168=ORIENTED_EDGE('',*,*,#17995,.F.);
#24169=ORIENTED_EDGE('',*,*,#17998,.F.);
#24170=ORIENTED_EDGE('',*,*,#18001,.F.);
#24171=ORIENTED_EDGE('',*,*,#18040,.F.);
#24172=ORIENTED_EDGE('',*,*,#18041,.T.);
#24173=ORIENTED_EDGE('',*,*,#18042,.T.);
#24174=ORIENTED_EDGE('',*,*,#18043,.F.);
#24175=ORIENTED_EDGE('',*,*,#18044,.F.);
#24176=ORIENTED_EDGE('',*,*,#18045,.T.);
#24177=ORIENTED_EDGE('',*,*,#18046,.T.);
#24178=ORIENTED_EDGE('',*,*,#18041,.F.);
#24179=ORIENTED_EDGE('',*,*,#18047,.F.);
#24180=ORIENTED_EDGE('',*,*,#18048,.T.);
#24181=ORIENTED_EDGE('',*,*,#18049,.T.);
#24182=ORIENTED_EDGE('',*,*,#18045,.F.);
#24183=ORIENTED_EDGE('',*,*,#18050,.F.);
#24184=ORIENTED_EDGE('',*,*,#18051,.T.);
#24185=ORIENTED_EDGE('',*,*,#18052,.T.);
#24186=ORIENTED_EDGE('',*,*,#18048,.F.);
#24187=ORIENTED_EDGE('',*,*,#18053,.F.);
#24188=ORIENTED_EDGE('',*,*,#18054,.T.);
#24189=ORIENTED_EDGE('',*,*,#18055,.T.);
#24190=ORIENTED_EDGE('',*,*,#18051,.F.);
#24191=ORIENTED_EDGE('',*,*,#18056,.F.);
#24192=ORIENTED_EDGE('',*,*,#18057,.T.);
#24193=ORIENTED_EDGE('',*,*,#18058,.T.);
#24194=ORIENTED_EDGE('',*,*,#18054,.F.);
#24195=ORIENTED_EDGE('',*,*,#18059,.F.);
#24196=ORIENTED_EDGE('',*,*,#18060,.T.);
#24197=ORIENTED_EDGE('',*,*,#18061,.T.);
#24198=ORIENTED_EDGE('',*,*,#18057,.F.);
#24199=ORIENTED_EDGE('',*,*,#18062,.F.);
#24200=ORIENTED_EDGE('',*,*,#18063,.T.);
#24201=ORIENTED_EDGE('',*,*,#18064,.T.);
#24202=ORIENTED_EDGE('',*,*,#18060,.F.);
#24203=ORIENTED_EDGE('',*,*,#18065,.F.);
#24204=ORIENTED_EDGE('',*,*,#18066,.T.);
#24205=ORIENTED_EDGE('',*,*,#18067,.T.);
#24206=ORIENTED_EDGE('',*,*,#18063,.F.);
#24207=ORIENTED_EDGE('',*,*,#18068,.F.);
#24208=ORIENTED_EDGE('',*,*,#18069,.T.);
#24209=ORIENTED_EDGE('',*,*,#18070,.T.);
#24210=ORIENTED_EDGE('',*,*,#18066,.F.);
#24211=ORIENTED_EDGE('',*,*,#18071,.F.);
#24212=ORIENTED_EDGE('',*,*,#18072,.T.);
#24213=ORIENTED_EDGE('',*,*,#18073,.T.);
#24214=ORIENTED_EDGE('',*,*,#18069,.F.);
#24215=ORIENTED_EDGE('',*,*,#18074,.F.);
#24216=ORIENTED_EDGE('',*,*,#18075,.T.);
#24217=ORIENTED_EDGE('',*,*,#18076,.T.);
#24218=ORIENTED_EDGE('',*,*,#18072,.F.);
#24219=ORIENTED_EDGE('',*,*,#18077,.F.);
#24220=ORIENTED_EDGE('',*,*,#18078,.T.);
#24221=ORIENTED_EDGE('',*,*,#18079,.T.);
#24222=ORIENTED_EDGE('',*,*,#18075,.F.);
#24223=ORIENTED_EDGE('',*,*,#18080,.F.);
#24224=ORIENTED_EDGE('',*,*,#18081,.T.);
#24225=ORIENTED_EDGE('',*,*,#18082,.T.);
#24226=ORIENTED_EDGE('',*,*,#18078,.F.);
#24227=ORIENTED_EDGE('',*,*,#18083,.F.);
#24228=ORIENTED_EDGE('',*,*,#18084,.T.);
#24229=ORIENTED_EDGE('',*,*,#18085,.T.);
#24230=ORIENTED_EDGE('',*,*,#18081,.F.);
#24231=ORIENTED_EDGE('',*,*,#18086,.F.);
#24232=ORIENTED_EDGE('',*,*,#18087,.T.);
#24233=ORIENTED_EDGE('',*,*,#18088,.T.);
#24234=ORIENTED_EDGE('',*,*,#18084,.F.);
#24235=ORIENTED_EDGE('',*,*,#18089,.F.);
#24236=ORIENTED_EDGE('',*,*,#18090,.T.);
#24237=ORIENTED_EDGE('',*,*,#18091,.T.);
#24238=ORIENTED_EDGE('',*,*,#18087,.F.);
#24239=ORIENTED_EDGE('',*,*,#18092,.F.);
#24240=ORIENTED_EDGE('',*,*,#18093,.T.);
#24241=ORIENTED_EDGE('',*,*,#18094,.T.);
#24242=ORIENTED_EDGE('',*,*,#18090,.F.);
#24243=ORIENTED_EDGE('',*,*,#18095,.F.);
#24244=ORIENTED_EDGE('',*,*,#18096,.T.);
#24245=ORIENTED_EDGE('',*,*,#18097,.T.);
#24246=ORIENTED_EDGE('',*,*,#18093,.F.);
#24247=ORIENTED_EDGE('',*,*,#18098,.F.);
#24248=ORIENTED_EDGE('',*,*,#18099,.T.);
#24249=ORIENTED_EDGE('',*,*,#18100,.T.);
#24250=ORIENTED_EDGE('',*,*,#18096,.F.);
#24251=ORIENTED_EDGE('',*,*,#18101,.F.);
#24252=ORIENTED_EDGE('',*,*,#18102,.T.);
#24253=ORIENTED_EDGE('',*,*,#18103,.T.);
#24254=ORIENTED_EDGE('',*,*,#18099,.F.);
#24255=ORIENTED_EDGE('',*,*,#18104,.F.);
#24256=ORIENTED_EDGE('',*,*,#18105,.T.);
#24257=ORIENTED_EDGE('',*,*,#18106,.T.);
#24258=ORIENTED_EDGE('',*,*,#18102,.F.);
#24259=ORIENTED_EDGE('',*,*,#18107,.F.);
#24260=ORIENTED_EDGE('',*,*,#18108,.T.);
#24261=ORIENTED_EDGE('',*,*,#18109,.T.);
#24262=ORIENTED_EDGE('',*,*,#18105,.F.);
#24263=ORIENTED_EDGE('',*,*,#18110,.F.);
#24264=ORIENTED_EDGE('',*,*,#18111,.T.);
#24265=ORIENTED_EDGE('',*,*,#18112,.T.);
#24266=ORIENTED_EDGE('',*,*,#18108,.F.);
#24267=ORIENTED_EDGE('',*,*,#18113,.F.);
#24268=ORIENTED_EDGE('',*,*,#18114,.T.);
#24269=ORIENTED_EDGE('',*,*,#18115,.T.);
#24270=ORIENTED_EDGE('',*,*,#18111,.F.);
#24271=ORIENTED_EDGE('',*,*,#18116,.F.);
#24272=ORIENTED_EDGE('',*,*,#18117,.T.);
#24273=ORIENTED_EDGE('',*,*,#18118,.T.);
#24274=ORIENTED_EDGE('',*,*,#18114,.F.);
#24275=ORIENTED_EDGE('',*,*,#18119,.F.);
#24276=ORIENTED_EDGE('',*,*,#18120,.T.);
#24277=ORIENTED_EDGE('',*,*,#18121,.T.);
#24278=ORIENTED_EDGE('',*,*,#18117,.F.);
#24279=ORIENTED_EDGE('',*,*,#18122,.F.);
#24280=ORIENTED_EDGE('',*,*,#18123,.T.);
#24281=ORIENTED_EDGE('',*,*,#18124,.T.);
#24282=ORIENTED_EDGE('',*,*,#18120,.F.);
#24283=ORIENTED_EDGE('',*,*,#18125,.F.);
#24284=ORIENTED_EDGE('',*,*,#18126,.T.);
#24285=ORIENTED_EDGE('',*,*,#18127,.T.);
#24286=ORIENTED_EDGE('',*,*,#18123,.F.);
#24287=ORIENTED_EDGE('',*,*,#18128,.F.);
#24288=ORIENTED_EDGE('',*,*,#18043,.T.);
#24289=ORIENTED_EDGE('',*,*,#18129,.T.);
#24290=ORIENTED_EDGE('',*,*,#18126,.F.);
#24291=ORIENTED_EDGE('',*,*,#18129,.F.);
#24292=ORIENTED_EDGE('',*,*,#18042,.F.);
#24293=ORIENTED_EDGE('',*,*,#18046,.F.);
#24294=ORIENTED_EDGE('',*,*,#18049,.F.);
#24295=ORIENTED_EDGE('',*,*,#18052,.F.);
#24296=ORIENTED_EDGE('',*,*,#18055,.F.);
#24297=ORIENTED_EDGE('',*,*,#18058,.F.);
#24298=ORIENTED_EDGE('',*,*,#18061,.F.);
#24299=ORIENTED_EDGE('',*,*,#18064,.F.);
#24300=ORIENTED_EDGE('',*,*,#18067,.F.);
#24301=ORIENTED_EDGE('',*,*,#18070,.F.);
#24302=ORIENTED_EDGE('',*,*,#18073,.F.);
#24303=ORIENTED_EDGE('',*,*,#18076,.F.);
#24304=ORIENTED_EDGE('',*,*,#18079,.F.);
#24305=ORIENTED_EDGE('',*,*,#18082,.F.);
#24306=ORIENTED_EDGE('',*,*,#18085,.F.);
#24307=ORIENTED_EDGE('',*,*,#18088,.F.);
#24308=ORIENTED_EDGE('',*,*,#18091,.F.);
#24309=ORIENTED_EDGE('',*,*,#18094,.F.);
#24310=ORIENTED_EDGE('',*,*,#18097,.F.);
#24311=ORIENTED_EDGE('',*,*,#18100,.F.);
#24312=ORIENTED_EDGE('',*,*,#18103,.F.);
#24313=ORIENTED_EDGE('',*,*,#18106,.F.);
#24314=ORIENTED_EDGE('',*,*,#18109,.F.);
#24315=ORIENTED_EDGE('',*,*,#18112,.F.);
#24316=ORIENTED_EDGE('',*,*,#18115,.F.);
#24317=ORIENTED_EDGE('',*,*,#18118,.F.);
#24318=ORIENTED_EDGE('',*,*,#18121,.F.);
#24319=ORIENTED_EDGE('',*,*,#18124,.F.);
#24320=ORIENTED_EDGE('',*,*,#18127,.F.);
#24321=ORIENTED_EDGE('',*,*,#17980,.T.);
#24322=ORIENTED_EDGE('',*,*,#18002,.T.);
#24323=ORIENTED_EDGE('',*,*,#17999,.T.);
#24324=ORIENTED_EDGE('',*,*,#17996,.T.);
#24325=ORIENTED_EDGE('',*,*,#17993,.T.);
#24326=ORIENTED_EDGE('',*,*,#17990,.T.);
#24327=ORIENTED_EDGE('',*,*,#17987,.T.);
#24328=ORIENTED_EDGE('',*,*,#17984,.T.);
#24329=ORIENTED_EDGE('',*,*,#18130,.F.);
#24330=ORIENTED_EDGE('',*,*,#18131,.T.);
#24331=ORIENTED_EDGE('',*,*,#18132,.T.);
#24332=ORIENTED_EDGE('',*,*,#18133,.F.);
#24333=ORIENTED_EDGE('',*,*,#18134,.F.);
#24334=ORIENTED_EDGE('',*,*,#18135,.T.);
#24335=ORIENTED_EDGE('',*,*,#18136,.T.);
#24336=ORIENTED_EDGE('',*,*,#18131,.F.);
#24337=ORIENTED_EDGE('',*,*,#18137,.F.);
#24338=ORIENTED_EDGE('',*,*,#18138,.T.);
#24339=ORIENTED_EDGE('',*,*,#18139,.T.);
#24340=ORIENTED_EDGE('',*,*,#18135,.F.);
#24341=ORIENTED_EDGE('',*,*,#18140,.F.);
#24342=ORIENTED_EDGE('',*,*,#18141,.T.);
#24343=ORIENTED_EDGE('',*,*,#18142,.T.);
#24344=ORIENTED_EDGE('',*,*,#18138,.F.);
#24345=ORIENTED_EDGE('',*,*,#18143,.F.);
#24346=ORIENTED_EDGE('',*,*,#18144,.T.);
#24347=ORIENTED_EDGE('',*,*,#18145,.T.);
#24348=ORIENTED_EDGE('',*,*,#18141,.F.);
#24349=ORIENTED_EDGE('',*,*,#18146,.F.);
#24350=ORIENTED_EDGE('',*,*,#18147,.T.);
#24351=ORIENTED_EDGE('',*,*,#18148,.T.);
#24352=ORIENTED_EDGE('',*,*,#18144,.F.);
#24353=ORIENTED_EDGE('',*,*,#18149,.F.);
#24354=ORIENTED_EDGE('',*,*,#18150,.T.);
#24355=ORIENTED_EDGE('',*,*,#18151,.T.);
#24356=ORIENTED_EDGE('',*,*,#18147,.F.);
#24357=ORIENTED_EDGE('',*,*,#18152,.F.);
#24358=ORIENTED_EDGE('',*,*,#18133,.T.);
#24359=ORIENTED_EDGE('',*,*,#18153,.T.);
#24360=ORIENTED_EDGE('',*,*,#18150,.F.);
#24361=ORIENTED_EDGE('',*,*,#18154,.F.);
#24362=ORIENTED_EDGE('',*,*,#18155,.T.);
#24363=ORIENTED_EDGE('',*,*,#18156,.T.);
#24364=ORIENTED_EDGE('',*,*,#18157,.F.);
#24365=ORIENTED_EDGE('',*,*,#18158,.F.);
#24366=ORIENTED_EDGE('',*,*,#18159,.T.);
#24367=ORIENTED_EDGE('',*,*,#18160,.T.);
#24368=ORIENTED_EDGE('',*,*,#18155,.F.);
#24369=ORIENTED_EDGE('',*,*,#18161,.F.);
#24370=ORIENTED_EDGE('',*,*,#18162,.T.);
#24371=ORIENTED_EDGE('',*,*,#18163,.T.);
#24372=ORIENTED_EDGE('',*,*,#18159,.F.);
#24373=ORIENTED_EDGE('',*,*,#18164,.F.);
#24374=ORIENTED_EDGE('',*,*,#18165,.T.);
#24375=ORIENTED_EDGE('',*,*,#18166,.T.);
#24376=ORIENTED_EDGE('',*,*,#18162,.F.);
#24377=ORIENTED_EDGE('',*,*,#18167,.F.);
#24378=ORIENTED_EDGE('',*,*,#18168,.T.);
#24379=ORIENTED_EDGE('',*,*,#18169,.T.);
#24380=ORIENTED_EDGE('',*,*,#18165,.F.);
#24381=ORIENTED_EDGE('',*,*,#18170,.F.);
#24382=ORIENTED_EDGE('',*,*,#18171,.T.);
#24383=ORIENTED_EDGE('',*,*,#18172,.T.);
#24384=ORIENTED_EDGE('',*,*,#18168,.F.);
#24385=ORIENTED_EDGE('',*,*,#18173,.F.);
#24386=ORIENTED_EDGE('',*,*,#18174,.T.);
#24387=ORIENTED_EDGE('',*,*,#18175,.T.);
#24388=ORIENTED_EDGE('',*,*,#18171,.F.);
#24389=ORIENTED_EDGE('',*,*,#18176,.F.);
#24390=ORIENTED_EDGE('',*,*,#18177,.T.);
#24391=ORIENTED_EDGE('',*,*,#18178,.T.);
#24392=ORIENTED_EDGE('',*,*,#18174,.F.);
#24393=ORIENTED_EDGE('',*,*,#18179,.F.);
#24394=ORIENTED_EDGE('',*,*,#18180,.T.);
#24395=ORIENTED_EDGE('',*,*,#18181,.T.);
#24396=ORIENTED_EDGE('',*,*,#18177,.F.);
#24397=ORIENTED_EDGE('',*,*,#18182,.F.);
#24398=ORIENTED_EDGE('',*,*,#18183,.T.);
#24399=ORIENTED_EDGE('',*,*,#18184,.T.);
#24400=ORIENTED_EDGE('',*,*,#18180,.F.);
#24401=ORIENTED_EDGE('',*,*,#18185,.F.);
#24402=ORIENTED_EDGE('',*,*,#18186,.T.);
#24403=ORIENTED_EDGE('',*,*,#18187,.T.);
#24404=ORIENTED_EDGE('',*,*,#18183,.F.);
#24405=ORIENTED_EDGE('',*,*,#18188,.F.);
#24406=ORIENTED_EDGE('',*,*,#18157,.T.);
#24407=ORIENTED_EDGE('',*,*,#18189,.T.);
#24408=ORIENTED_EDGE('',*,*,#18186,.F.);
#24409=ORIENTED_EDGE('',*,*,#18189,.F.);
#24410=ORIENTED_EDGE('',*,*,#18156,.F.);
#24411=ORIENTED_EDGE('',*,*,#18160,.F.);
#24412=ORIENTED_EDGE('',*,*,#18163,.F.);
#24413=ORIENTED_EDGE('',*,*,#18166,.F.);
#24414=ORIENTED_EDGE('',*,*,#18169,.F.);
#24415=ORIENTED_EDGE('',*,*,#18172,.F.);
#24416=ORIENTED_EDGE('',*,*,#18175,.F.);
#24417=ORIENTED_EDGE('',*,*,#18178,.F.);
#24418=ORIENTED_EDGE('',*,*,#18181,.F.);
#24419=ORIENTED_EDGE('',*,*,#18184,.F.);
#24420=ORIENTED_EDGE('',*,*,#18187,.F.);
#24421=ORIENTED_EDGE('',*,*,#18153,.F.);
#24422=ORIENTED_EDGE('',*,*,#18132,.F.);
#24423=ORIENTED_EDGE('',*,*,#18136,.F.);
#24424=ORIENTED_EDGE('',*,*,#18139,.F.);
#24425=ORIENTED_EDGE('',*,*,#18142,.F.);
#24426=ORIENTED_EDGE('',*,*,#18145,.F.);
#24427=ORIENTED_EDGE('',*,*,#18148,.F.);
#24428=ORIENTED_EDGE('',*,*,#18151,.F.);
#24429=ORIENTED_EDGE('',*,*,#18190,.F.);
#24430=ORIENTED_EDGE('',*,*,#18191,.T.);
#24431=ORIENTED_EDGE('',*,*,#18192,.T.);
#24432=ORIENTED_EDGE('',*,*,#18193,.F.);
#24433=ORIENTED_EDGE('',*,*,#18194,.F.);
#24434=ORIENTED_EDGE('',*,*,#18195,.T.);
#24435=ORIENTED_EDGE('',*,*,#18196,.T.);
#24436=ORIENTED_EDGE('',*,*,#18191,.F.);
#24437=ORIENTED_EDGE('',*,*,#18197,.F.);
#24438=ORIENTED_EDGE('',*,*,#18193,.T.);
#24439=ORIENTED_EDGE('',*,*,#18198,.T.);
#24440=ORIENTED_EDGE('',*,*,#18195,.F.);
#24441=ORIENTED_EDGE('',*,*,#18199,.F.);
#24442=ORIENTED_EDGE('',*,*,#18200,.T.);
#24443=ORIENTED_EDGE('',*,*,#18201,.T.);
#24444=ORIENTED_EDGE('',*,*,#18202,.F.);
#24445=ORIENTED_EDGE('',*,*,#18203,.F.);
#24446=ORIENTED_EDGE('',*,*,#18204,.T.);
#24447=ORIENTED_EDGE('',*,*,#18205,.T.);
#24448=ORIENTED_EDGE('',*,*,#18200,.F.);
#24449=ORIENTED_EDGE('',*,*,#18206,.F.);
#24450=ORIENTED_EDGE('',*,*,#18207,.T.);
#24451=ORIENTED_EDGE('',*,*,#18208,.T.);
#24452=ORIENTED_EDGE('',*,*,#18204,.F.);
#24453=ORIENTED_EDGE('',*,*,#18209,.F.);
#24454=ORIENTED_EDGE('',*,*,#18210,.T.);
#24455=ORIENTED_EDGE('',*,*,#18211,.T.);
#24456=ORIENTED_EDGE('',*,*,#18207,.F.);
#24457=ORIENTED_EDGE('',*,*,#18212,.F.);
#24458=ORIENTED_EDGE('',*,*,#18213,.T.);
#24459=ORIENTED_EDGE('',*,*,#18214,.T.);
#24460=ORIENTED_EDGE('',*,*,#18210,.F.);
#24461=ORIENTED_EDGE('',*,*,#18215,.F.);
#24462=ORIENTED_EDGE('',*,*,#18216,.T.);
#24463=ORIENTED_EDGE('',*,*,#18217,.T.);
#24464=ORIENTED_EDGE('',*,*,#18213,.F.);
#24465=ORIENTED_EDGE('',*,*,#18218,.F.);
#24466=ORIENTED_EDGE('',*,*,#18219,.T.);
#24467=ORIENTED_EDGE('',*,*,#18220,.T.);
#24468=ORIENTED_EDGE('',*,*,#18216,.F.);
#24469=ORIENTED_EDGE('',*,*,#18221,.F.);
#24470=ORIENTED_EDGE('',*,*,#18222,.T.);
#24471=ORIENTED_EDGE('',*,*,#18223,.T.);
#24472=ORIENTED_EDGE('',*,*,#18219,.F.);
#24473=ORIENTED_EDGE('',*,*,#18224,.F.);
#24474=ORIENTED_EDGE('',*,*,#18225,.T.);
#24475=ORIENTED_EDGE('',*,*,#18226,.T.);
#24476=ORIENTED_EDGE('',*,*,#18222,.F.);
#24477=ORIENTED_EDGE('',*,*,#18227,.F.);
#24478=ORIENTED_EDGE('',*,*,#18228,.T.);
#24479=ORIENTED_EDGE('',*,*,#18229,.T.);
#24480=ORIENTED_EDGE('',*,*,#18225,.F.);
#24481=ORIENTED_EDGE('',*,*,#18230,.F.);
#24482=ORIENTED_EDGE('',*,*,#18202,.T.);
#24483=ORIENTED_EDGE('',*,*,#18231,.T.);
#24484=ORIENTED_EDGE('',*,*,#18228,.F.);
#24485=ORIENTED_EDGE('',*,*,#18231,.F.);
#24486=ORIENTED_EDGE('',*,*,#18201,.F.);
#24487=ORIENTED_EDGE('',*,*,#18205,.F.);
#24488=ORIENTED_EDGE('',*,*,#18208,.F.);
#24489=ORIENTED_EDGE('',*,*,#18211,.F.);
#24490=ORIENTED_EDGE('',*,*,#18214,.F.);
#24491=ORIENTED_EDGE('',*,*,#18217,.F.);
#24492=ORIENTED_EDGE('',*,*,#18220,.F.);
#24493=ORIENTED_EDGE('',*,*,#18223,.F.);
#24494=ORIENTED_EDGE('',*,*,#18226,.F.);
#24495=ORIENTED_EDGE('',*,*,#18229,.F.);
#24496=ORIENTED_EDGE('',*,*,#18198,.F.);
#24497=ORIENTED_EDGE('',*,*,#18192,.F.);
#24498=ORIENTED_EDGE('',*,*,#18196,.F.);
#24499=ORIENTED_EDGE('',*,*,#18190,.T.);
#24500=ORIENTED_EDGE('',*,*,#18197,.T.);
#24501=ORIENTED_EDGE('',*,*,#18194,.T.);
#24502=ORIENTED_EDGE('',*,*,#18130,.T.);
#24503=ORIENTED_EDGE('',*,*,#18152,.T.);
#24504=ORIENTED_EDGE('',*,*,#18149,.T.);
#24505=ORIENTED_EDGE('',*,*,#18146,.T.);
#24506=ORIENTED_EDGE('',*,*,#18143,.T.);
#24507=ORIENTED_EDGE('',*,*,#18140,.T.);
#24508=ORIENTED_EDGE('',*,*,#18137,.T.);
#24509=ORIENTED_EDGE('',*,*,#18134,.T.);
#24510=ORIENTED_EDGE('',*,*,#18232,.F.);
#24511=ORIENTED_EDGE('',*,*,#18233,.T.);
#24512=ORIENTED_EDGE('',*,*,#18234,.T.);
#24513=ORIENTED_EDGE('',*,*,#18235,.F.);
#24514=ORIENTED_EDGE('',*,*,#18236,.F.);
#24515=ORIENTED_EDGE('',*,*,#18237,.T.);
#24516=ORIENTED_EDGE('',*,*,#18238,.T.);
#24517=ORIENTED_EDGE('',*,*,#18233,.F.);
#24518=ORIENTED_EDGE('',*,*,#18239,.F.);
#24519=ORIENTED_EDGE('',*,*,#18240,.T.);
#24520=ORIENTED_EDGE('',*,*,#18241,.T.);
#24521=ORIENTED_EDGE('',*,*,#18237,.F.);
#24522=ORIENTED_EDGE('',*,*,#18242,.F.);
#24523=ORIENTED_EDGE('',*,*,#18235,.T.);
#24524=ORIENTED_EDGE('',*,*,#18243,.T.);
#24525=ORIENTED_EDGE('',*,*,#18240,.F.);
#24526=ORIENTED_EDGE('',*,*,#18243,.F.);
#24527=ORIENTED_EDGE('',*,*,#18234,.F.);
#24528=ORIENTED_EDGE('',*,*,#18238,.F.);
#24529=ORIENTED_EDGE('',*,*,#18241,.F.);
#24530=ORIENTED_EDGE('',*,*,#18244,.F.);
#24531=ORIENTED_EDGE('',*,*,#18245,.T.);
#24532=ORIENTED_EDGE('',*,*,#18246,.T.);
#24533=ORIENTED_EDGE('',*,*,#18247,.F.);
#24534=ORIENTED_EDGE('',*,*,#18248,.F.);
#24535=ORIENTED_EDGE('',*,*,#18249,.T.);
#24536=ORIENTED_EDGE('',*,*,#18250,.T.);
#24537=ORIENTED_EDGE('',*,*,#18245,.F.);
#24538=ORIENTED_EDGE('',*,*,#18251,.F.);
#24539=ORIENTED_EDGE('',*,*,#18252,.T.);
#24540=ORIENTED_EDGE('',*,*,#18253,.T.);
#24541=ORIENTED_EDGE('',*,*,#18249,.F.);
#24542=ORIENTED_EDGE('',*,*,#18254,.F.);
#24543=ORIENTED_EDGE('',*,*,#18247,.T.);
#24544=ORIENTED_EDGE('',*,*,#18255,.T.);
#24545=ORIENTED_EDGE('',*,*,#18252,.F.);
#24546=ORIENTED_EDGE('',*,*,#18255,.F.);
#24547=ORIENTED_EDGE('',*,*,#18246,.F.);
#24548=ORIENTED_EDGE('',*,*,#18250,.F.);
#24549=ORIENTED_EDGE('',*,*,#18253,.F.);
#24550=ORIENTED_EDGE('',*,*,#18256,.F.);
#24551=ORIENTED_EDGE('',*,*,#18257,.T.);
#24552=ORIENTED_EDGE('',*,*,#18258,.T.);
#24553=ORIENTED_EDGE('',*,*,#18259,.F.);
#24554=ORIENTED_EDGE('',*,*,#18260,.F.);
#24555=ORIENTED_EDGE('',*,*,#18261,.T.);
#24556=ORIENTED_EDGE('',*,*,#18262,.T.);
#24557=ORIENTED_EDGE('',*,*,#18257,.F.);
#24558=ORIENTED_EDGE('',*,*,#18263,.F.);
#24559=ORIENTED_EDGE('',*,*,#18264,.T.);
#24560=ORIENTED_EDGE('',*,*,#18265,.T.);
#24561=ORIENTED_EDGE('',*,*,#18261,.F.);
#24562=ORIENTED_EDGE('',*,*,#18266,.F.);
#24563=ORIENTED_EDGE('',*,*,#18259,.T.);
#24564=ORIENTED_EDGE('',*,*,#18267,.T.);
#24565=ORIENTED_EDGE('',*,*,#18264,.F.);
#24566=ORIENTED_EDGE('',*,*,#18267,.F.);
#24567=ORIENTED_EDGE('',*,*,#18258,.F.);
#24568=ORIENTED_EDGE('',*,*,#18262,.F.);
#24569=ORIENTED_EDGE('',*,*,#18265,.F.);
#24570=ORIENTED_EDGE('',*,*,#18268,.F.);
#24571=ORIENTED_EDGE('',*,*,#18269,.T.);
#24572=ORIENTED_EDGE('',*,*,#18270,.T.);
#24573=ORIENTED_EDGE('',*,*,#18271,.F.);
#24574=ORIENTED_EDGE('',*,*,#18272,.F.);
#24575=ORIENTED_EDGE('',*,*,#18273,.T.);
#24576=ORIENTED_EDGE('',*,*,#18274,.T.);
#24577=ORIENTED_EDGE('',*,*,#18269,.F.);
#24578=ORIENTED_EDGE('',*,*,#18275,.F.);
#24579=ORIENTED_EDGE('',*,*,#18276,.T.);
#24580=ORIENTED_EDGE('',*,*,#18277,.T.);
#24581=ORIENTED_EDGE('',*,*,#18273,.F.);
#24582=ORIENTED_EDGE('',*,*,#18278,.F.);
#24583=ORIENTED_EDGE('',*,*,#18271,.T.);
#24584=ORIENTED_EDGE('',*,*,#18279,.T.);
#24585=ORIENTED_EDGE('',*,*,#18276,.F.);
#24586=ORIENTED_EDGE('',*,*,#18279,.F.);
#24587=ORIENTED_EDGE('',*,*,#18270,.F.);
#24588=ORIENTED_EDGE('',*,*,#18274,.F.);
#24589=ORIENTED_EDGE('',*,*,#18277,.F.);
#24590=ORIENTED_EDGE('',*,*,#18280,.F.);
#24591=ORIENTED_EDGE('',*,*,#18281,.T.);
#24592=ORIENTED_EDGE('',*,*,#18282,.T.);
#24593=ORIENTED_EDGE('',*,*,#18283,.F.);
#24594=ORIENTED_EDGE('',*,*,#18284,.F.);
#24595=ORIENTED_EDGE('',*,*,#18285,.T.);
#24596=ORIENTED_EDGE('',*,*,#18286,.T.);
#24597=ORIENTED_EDGE('',*,*,#18281,.F.);
#24598=ORIENTED_EDGE('',*,*,#18287,.F.);
#24599=ORIENTED_EDGE('',*,*,#18288,.T.);
#24600=ORIENTED_EDGE('',*,*,#18289,.T.);
#24601=ORIENTED_EDGE('',*,*,#18285,.F.);
#24602=ORIENTED_EDGE('',*,*,#18290,.F.);
#24603=ORIENTED_EDGE('',*,*,#18283,.T.);
#24604=ORIENTED_EDGE('',*,*,#18291,.T.);
#24605=ORIENTED_EDGE('',*,*,#18288,.F.);
#24606=ORIENTED_EDGE('',*,*,#18291,.F.);
#24607=ORIENTED_EDGE('',*,*,#18282,.F.);
#24608=ORIENTED_EDGE('',*,*,#18286,.F.);
#24609=ORIENTED_EDGE('',*,*,#18289,.F.);
#24610=ORIENTED_EDGE('',*,*,#18292,.F.);
#24611=ORIENTED_EDGE('',*,*,#18293,.T.);
#24612=ORIENTED_EDGE('',*,*,#18294,.T.);
#24613=ORIENTED_EDGE('',*,*,#18295,.F.);
#24614=ORIENTED_EDGE('',*,*,#18296,.F.);
#24615=ORIENTED_EDGE('',*,*,#18297,.T.);
#24616=ORIENTED_EDGE('',*,*,#18298,.T.);
#24617=ORIENTED_EDGE('',*,*,#18293,.F.);
#24618=ORIENTED_EDGE('',*,*,#18299,.F.);
#24619=ORIENTED_EDGE('',*,*,#18300,.T.);
#24620=ORIENTED_EDGE('',*,*,#18301,.T.);
#24621=ORIENTED_EDGE('',*,*,#18297,.F.);
#24622=ORIENTED_EDGE('',*,*,#18302,.F.);
#24623=ORIENTED_EDGE('',*,*,#18295,.T.);
#24624=ORIENTED_EDGE('',*,*,#18303,.T.);
#24625=ORIENTED_EDGE('',*,*,#18300,.F.);
#24626=ORIENTED_EDGE('',*,*,#18303,.F.);
#24627=ORIENTED_EDGE('',*,*,#18294,.F.);
#24628=ORIENTED_EDGE('',*,*,#18298,.F.);
#24629=ORIENTED_EDGE('',*,*,#18301,.F.);
#24630=ORIENTED_EDGE('',*,*,#18304,.F.);
#24631=ORIENTED_EDGE('',*,*,#18305,.T.);
#24632=ORIENTED_EDGE('',*,*,#18306,.T.);
#24633=ORIENTED_EDGE('',*,*,#18307,.F.);
#24634=ORIENTED_EDGE('',*,*,#18308,.F.);
#24635=ORIENTED_EDGE('',*,*,#18309,.T.);
#24636=ORIENTED_EDGE('',*,*,#18310,.T.);
#24637=ORIENTED_EDGE('',*,*,#18305,.F.);
#24638=ORIENTED_EDGE('',*,*,#18311,.F.);
#24639=ORIENTED_EDGE('',*,*,#18312,.T.);
#24640=ORIENTED_EDGE('',*,*,#18313,.T.);
#24641=ORIENTED_EDGE('',*,*,#18309,.F.);
#24642=ORIENTED_EDGE('',*,*,#18314,.F.);
#24643=ORIENTED_EDGE('',*,*,#18307,.T.);
#24644=ORIENTED_EDGE('',*,*,#18315,.T.);
#24645=ORIENTED_EDGE('',*,*,#18312,.F.);
#24646=ORIENTED_EDGE('',*,*,#18315,.F.);
#24647=ORIENTED_EDGE('',*,*,#18306,.F.);
#24648=ORIENTED_EDGE('',*,*,#18310,.F.);
#24649=ORIENTED_EDGE('',*,*,#18313,.F.);
#24650=ORIENTED_EDGE('',*,*,#18316,.F.);
#24651=ORIENTED_EDGE('',*,*,#18317,.T.);
#24652=ORIENTED_EDGE('',*,*,#18318,.T.);
#24653=ORIENTED_EDGE('',*,*,#18319,.F.);
#24654=ORIENTED_EDGE('',*,*,#18320,.F.);
#24655=ORIENTED_EDGE('',*,*,#18321,.T.);
#24656=ORIENTED_EDGE('',*,*,#18322,.T.);
#24657=ORIENTED_EDGE('',*,*,#18317,.F.);
#24658=ORIENTED_EDGE('',*,*,#18323,.F.);
#24659=ORIENTED_EDGE('',*,*,#18324,.T.);
#24660=ORIENTED_EDGE('',*,*,#18325,.T.);
#24661=ORIENTED_EDGE('',*,*,#18321,.F.);
#24662=ORIENTED_EDGE('',*,*,#18326,.F.);
#24663=ORIENTED_EDGE('',*,*,#18319,.T.);
#24664=ORIENTED_EDGE('',*,*,#18327,.T.);
#24665=ORIENTED_EDGE('',*,*,#18324,.F.);
#24666=ORIENTED_EDGE('',*,*,#18327,.F.);
#24667=ORIENTED_EDGE('',*,*,#18318,.F.);
#24668=ORIENTED_EDGE('',*,*,#18322,.F.);
#24669=ORIENTED_EDGE('',*,*,#18325,.F.);
#24670=ORIENTED_EDGE('',*,*,#18328,.F.);
#24671=ORIENTED_EDGE('',*,*,#18329,.T.);
#24672=ORIENTED_EDGE('',*,*,#18330,.T.);
#24673=ORIENTED_EDGE('',*,*,#18331,.F.);
#24674=ORIENTED_EDGE('',*,*,#18332,.F.);
#24675=ORIENTED_EDGE('',*,*,#18333,.T.);
#24676=ORIENTED_EDGE('',*,*,#18334,.T.);
#24677=ORIENTED_EDGE('',*,*,#18329,.F.);
#24678=ORIENTED_EDGE('',*,*,#18335,.F.);
#24679=ORIENTED_EDGE('',*,*,#18336,.T.);
#24680=ORIENTED_EDGE('',*,*,#18337,.T.);
#24681=ORIENTED_EDGE('',*,*,#18333,.F.);
#24682=ORIENTED_EDGE('',*,*,#18338,.F.);
#24683=ORIENTED_EDGE('',*,*,#18331,.T.);
#24684=ORIENTED_EDGE('',*,*,#18339,.T.);
#24685=ORIENTED_EDGE('',*,*,#18336,.F.);
#24686=ORIENTED_EDGE('',*,*,#18339,.F.);
#24687=ORIENTED_EDGE('',*,*,#18330,.F.);
#24688=ORIENTED_EDGE('',*,*,#18334,.F.);
#24689=ORIENTED_EDGE('',*,*,#18337,.F.);
#24690=ORIENTED_EDGE('',*,*,#18340,.F.);
#24691=ORIENTED_EDGE('',*,*,#18341,.T.);
#24692=ORIENTED_EDGE('',*,*,#18342,.T.);
#24693=ORIENTED_EDGE('',*,*,#18343,.F.);
#24694=ORIENTED_EDGE('',*,*,#18344,.F.);
#24695=ORIENTED_EDGE('',*,*,#18345,.T.);
#24696=ORIENTED_EDGE('',*,*,#18346,.T.);
#24697=ORIENTED_EDGE('',*,*,#18341,.F.);
#24698=ORIENTED_EDGE('',*,*,#18347,.F.);
#24699=ORIENTED_EDGE('',*,*,#18348,.T.);
#24700=ORIENTED_EDGE('',*,*,#18349,.T.);
#24701=ORIENTED_EDGE('',*,*,#18345,.F.);
#24702=ORIENTED_EDGE('',*,*,#18350,.F.);
#24703=ORIENTED_EDGE('',*,*,#18343,.T.);
#24704=ORIENTED_EDGE('',*,*,#18351,.T.);
#24705=ORIENTED_EDGE('',*,*,#18348,.F.);
#24706=ORIENTED_EDGE('',*,*,#18351,.F.);
#24707=ORIENTED_EDGE('',*,*,#18342,.F.);
#24708=ORIENTED_EDGE('',*,*,#18346,.F.);
#24709=ORIENTED_EDGE('',*,*,#18349,.F.);
#24710=ORIENTED_EDGE('',*,*,#18352,.F.);
#24711=ORIENTED_EDGE('',*,*,#18353,.T.);
#24712=ORIENTED_EDGE('',*,*,#18354,.T.);
#24713=ORIENTED_EDGE('',*,*,#18355,.F.);
#24714=ORIENTED_EDGE('',*,*,#18356,.F.);
#24715=ORIENTED_EDGE('',*,*,#18357,.T.);
#24716=ORIENTED_EDGE('',*,*,#18358,.T.);
#24717=ORIENTED_EDGE('',*,*,#18353,.F.);
#24718=ORIENTED_EDGE('',*,*,#18359,.F.);
#24719=ORIENTED_EDGE('',*,*,#18360,.T.);
#24720=ORIENTED_EDGE('',*,*,#18361,.T.);
#24721=ORIENTED_EDGE('',*,*,#18357,.F.);
#24722=ORIENTED_EDGE('',*,*,#18362,.F.);
#24723=ORIENTED_EDGE('',*,*,#18355,.T.);
#24724=ORIENTED_EDGE('',*,*,#18363,.T.);
#24725=ORIENTED_EDGE('',*,*,#18360,.F.);
#24726=ORIENTED_EDGE('',*,*,#18363,.F.);
#24727=ORIENTED_EDGE('',*,*,#18354,.F.);
#24728=ORIENTED_EDGE('',*,*,#18358,.F.);
#24729=ORIENTED_EDGE('',*,*,#18361,.F.);
#24730=ORIENTED_EDGE('',*,*,#18364,.F.);
#24731=ORIENTED_EDGE('',*,*,#18365,.T.);
#24732=ORIENTED_EDGE('',*,*,#18366,.T.);
#24733=ORIENTED_EDGE('',*,*,#18367,.F.);
#24734=ORIENTED_EDGE('',*,*,#18368,.F.);
#24735=ORIENTED_EDGE('',*,*,#18369,.T.);
#24736=ORIENTED_EDGE('',*,*,#18370,.T.);
#24737=ORIENTED_EDGE('',*,*,#18365,.F.);
#24738=ORIENTED_EDGE('',*,*,#18371,.F.);
#24739=ORIENTED_EDGE('',*,*,#18372,.T.);
#24740=ORIENTED_EDGE('',*,*,#18373,.T.);
#24741=ORIENTED_EDGE('',*,*,#18369,.F.);
#24742=ORIENTED_EDGE('',*,*,#18374,.F.);
#24743=ORIENTED_EDGE('',*,*,#18367,.T.);
#24744=ORIENTED_EDGE('',*,*,#18375,.T.);
#24745=ORIENTED_EDGE('',*,*,#18372,.F.);
#24746=ORIENTED_EDGE('',*,*,#18375,.F.);
#24747=ORIENTED_EDGE('',*,*,#18366,.F.);
#24748=ORIENTED_EDGE('',*,*,#18370,.F.);
#24749=ORIENTED_EDGE('',*,*,#18373,.F.);
#24750=ORIENTED_EDGE('',*,*,#18376,.F.);
#24751=ORIENTED_EDGE('',*,*,#18377,.T.);
#24752=ORIENTED_EDGE('',*,*,#18378,.T.);
#24753=ORIENTED_EDGE('',*,*,#18379,.F.);
#24754=ORIENTED_EDGE('',*,*,#18380,.F.);
#24755=ORIENTED_EDGE('',*,*,#18381,.T.);
#24756=ORIENTED_EDGE('',*,*,#18382,.T.);
#24757=ORIENTED_EDGE('',*,*,#18377,.F.);
#24758=ORIENTED_EDGE('',*,*,#18383,.F.);
#24759=ORIENTED_EDGE('',*,*,#18384,.T.);
#24760=ORIENTED_EDGE('',*,*,#18385,.T.);
#24761=ORIENTED_EDGE('',*,*,#18381,.F.);
#24762=ORIENTED_EDGE('',*,*,#18386,.F.);
#24763=ORIENTED_EDGE('',*,*,#18379,.T.);
#24764=ORIENTED_EDGE('',*,*,#18387,.T.);
#24765=ORIENTED_EDGE('',*,*,#18384,.F.);
#24766=ORIENTED_EDGE('',*,*,#18387,.F.);
#24767=ORIENTED_EDGE('',*,*,#18378,.F.);
#24768=ORIENTED_EDGE('',*,*,#18382,.F.);
#24769=ORIENTED_EDGE('',*,*,#18385,.F.);
#24770=ORIENTED_EDGE('',*,*,#18388,.F.);
#24771=ORIENTED_EDGE('',*,*,#18389,.T.);
#24772=ORIENTED_EDGE('',*,*,#18390,.T.);
#24773=ORIENTED_EDGE('',*,*,#18391,.F.);
#24774=ORIENTED_EDGE('',*,*,#18392,.F.);
#24775=ORIENTED_EDGE('',*,*,#18393,.T.);
#24776=ORIENTED_EDGE('',*,*,#18394,.T.);
#24777=ORIENTED_EDGE('',*,*,#18389,.F.);
#24778=ORIENTED_EDGE('',*,*,#18395,.F.);
#24779=ORIENTED_EDGE('',*,*,#18396,.T.);
#24780=ORIENTED_EDGE('',*,*,#18397,.T.);
#24781=ORIENTED_EDGE('',*,*,#18393,.F.);
#24782=ORIENTED_EDGE('',*,*,#18398,.F.);
#24783=ORIENTED_EDGE('',*,*,#18391,.T.);
#24784=ORIENTED_EDGE('',*,*,#18399,.T.);
#24785=ORIENTED_EDGE('',*,*,#18396,.F.);
#24786=ORIENTED_EDGE('',*,*,#18399,.F.);
#24787=ORIENTED_EDGE('',*,*,#18390,.F.);
#24788=ORIENTED_EDGE('',*,*,#18394,.F.);
#24789=ORIENTED_EDGE('',*,*,#18397,.F.);
#24790=ORIENTED_EDGE('',*,*,#18400,.F.);
#24791=ORIENTED_EDGE('',*,*,#18401,.T.);
#24792=ORIENTED_EDGE('',*,*,#18402,.T.);
#24793=ORIENTED_EDGE('',*,*,#18403,.F.);
#24794=ORIENTED_EDGE('',*,*,#18404,.F.);
#24795=ORIENTED_EDGE('',*,*,#18405,.T.);
#24796=ORIENTED_EDGE('',*,*,#18406,.T.);
#24797=ORIENTED_EDGE('',*,*,#18401,.F.);
#24798=ORIENTED_EDGE('',*,*,#18407,.F.);
#24799=ORIENTED_EDGE('',*,*,#18408,.T.);
#24800=ORIENTED_EDGE('',*,*,#18409,.T.);
#24801=ORIENTED_EDGE('',*,*,#18405,.F.);
#24802=ORIENTED_EDGE('',*,*,#18410,.F.);
#24803=ORIENTED_EDGE('',*,*,#18403,.T.);
#24804=ORIENTED_EDGE('',*,*,#18411,.T.);
#24805=ORIENTED_EDGE('',*,*,#18408,.F.);
#24806=ORIENTED_EDGE('',*,*,#18411,.F.);
#24807=ORIENTED_EDGE('',*,*,#18402,.F.);
#24808=ORIENTED_EDGE('',*,*,#18406,.F.);
#24809=ORIENTED_EDGE('',*,*,#18409,.F.);
#24810=ORIENTED_EDGE('',*,*,#18412,.F.);
#24811=ORIENTED_EDGE('',*,*,#18413,.T.);
#24812=ORIENTED_EDGE('',*,*,#18414,.T.);
#24813=ORIENTED_EDGE('',*,*,#18415,.F.);
#24814=ORIENTED_EDGE('',*,*,#18416,.F.);
#24815=ORIENTED_EDGE('',*,*,#18417,.T.);
#24816=ORIENTED_EDGE('',*,*,#18418,.T.);
#24817=ORIENTED_EDGE('',*,*,#18413,.F.);
#24818=ORIENTED_EDGE('',*,*,#18419,.F.);
#24819=ORIENTED_EDGE('',*,*,#18420,.T.);
#24820=ORIENTED_EDGE('',*,*,#18421,.T.);
#24821=ORIENTED_EDGE('',*,*,#18417,.F.);
#24822=ORIENTED_EDGE('',*,*,#18422,.F.);
#24823=ORIENTED_EDGE('',*,*,#18415,.T.);
#24824=ORIENTED_EDGE('',*,*,#18423,.T.);
#24825=ORIENTED_EDGE('',*,*,#18420,.F.);
#24826=ORIENTED_EDGE('',*,*,#18423,.F.);
#24827=ORIENTED_EDGE('',*,*,#18414,.F.);
#24828=ORIENTED_EDGE('',*,*,#18418,.F.);
#24829=ORIENTED_EDGE('',*,*,#18421,.F.);
#24830=ORIENTED_EDGE('',*,*,#18424,.F.);
#24831=ORIENTED_EDGE('',*,*,#18425,.T.);
#24832=ORIENTED_EDGE('',*,*,#18426,.T.);
#24833=ORIENTED_EDGE('',*,*,#18427,.F.);
#24834=ORIENTED_EDGE('',*,*,#18428,.F.);
#24835=ORIENTED_EDGE('',*,*,#18429,.T.);
#24836=ORIENTED_EDGE('',*,*,#18430,.T.);
#24837=ORIENTED_EDGE('',*,*,#18425,.F.);
#24838=ORIENTED_EDGE('',*,*,#18431,.F.);
#24839=ORIENTED_EDGE('',*,*,#18432,.T.);
#24840=ORIENTED_EDGE('',*,*,#18433,.T.);
#24841=ORIENTED_EDGE('',*,*,#18429,.F.);
#24842=ORIENTED_EDGE('',*,*,#18434,.F.);
#24843=ORIENTED_EDGE('',*,*,#18427,.T.);
#24844=ORIENTED_EDGE('',*,*,#18435,.T.);
#24845=ORIENTED_EDGE('',*,*,#18432,.F.);
#24846=ORIENTED_EDGE('',*,*,#18435,.F.);
#24847=ORIENTED_EDGE('',*,*,#18426,.F.);
#24848=ORIENTED_EDGE('',*,*,#18430,.F.);
#24849=ORIENTED_EDGE('',*,*,#18433,.F.);
#24850=ORIENTED_EDGE('',*,*,#18436,.F.);
#24851=ORIENTED_EDGE('',*,*,#18437,.T.);
#24852=ORIENTED_EDGE('',*,*,#18438,.T.);
#24853=ORIENTED_EDGE('',*,*,#18439,.F.);
#24854=ORIENTED_EDGE('',*,*,#18440,.F.);
#24855=ORIENTED_EDGE('',*,*,#18441,.T.);
#24856=ORIENTED_EDGE('',*,*,#18442,.T.);
#24857=ORIENTED_EDGE('',*,*,#18437,.F.);
#24858=ORIENTED_EDGE('',*,*,#18443,.F.);
#24859=ORIENTED_EDGE('',*,*,#18444,.T.);
#24860=ORIENTED_EDGE('',*,*,#18445,.T.);
#24861=ORIENTED_EDGE('',*,*,#18441,.F.);
#24862=ORIENTED_EDGE('',*,*,#18446,.F.);
#24863=ORIENTED_EDGE('',*,*,#18439,.T.);
#24864=ORIENTED_EDGE('',*,*,#18447,.T.);
#24865=ORIENTED_EDGE('',*,*,#18444,.F.);
#24866=ORIENTED_EDGE('',*,*,#18447,.F.);
#24867=ORIENTED_EDGE('',*,*,#18438,.F.);
#24868=ORIENTED_EDGE('',*,*,#18442,.F.);
#24869=ORIENTED_EDGE('',*,*,#18445,.F.);
#24870=ORIENTED_EDGE('',*,*,#18448,.F.);
#24871=ORIENTED_EDGE('',*,*,#18449,.T.);
#24872=ORIENTED_EDGE('',*,*,#18450,.T.);
#24873=ORIENTED_EDGE('',*,*,#18451,.F.);
#24874=ORIENTED_EDGE('',*,*,#18452,.F.);
#24875=ORIENTED_EDGE('',*,*,#18453,.T.);
#24876=ORIENTED_EDGE('',*,*,#18454,.T.);
#24877=ORIENTED_EDGE('',*,*,#18449,.F.);
#24878=ORIENTED_EDGE('',*,*,#18455,.F.);
#24879=ORIENTED_EDGE('',*,*,#18456,.T.);
#24880=ORIENTED_EDGE('',*,*,#18457,.T.);
#24881=ORIENTED_EDGE('',*,*,#18453,.F.);
#24882=ORIENTED_EDGE('',*,*,#18458,.F.);
#24883=ORIENTED_EDGE('',*,*,#18451,.T.);
#24884=ORIENTED_EDGE('',*,*,#18459,.T.);
#24885=ORIENTED_EDGE('',*,*,#18456,.F.);
#24886=ORIENTED_EDGE('',*,*,#18459,.F.);
#24887=ORIENTED_EDGE('',*,*,#18450,.F.);
#24888=ORIENTED_EDGE('',*,*,#18454,.F.);
#24889=ORIENTED_EDGE('',*,*,#18457,.F.);
#24890=ORIENTED_EDGE('',*,*,#18460,.F.);
#24891=ORIENTED_EDGE('',*,*,#18461,.T.);
#24892=ORIENTED_EDGE('',*,*,#18462,.T.);
#24893=ORIENTED_EDGE('',*,*,#18463,.F.);
#24894=ORIENTED_EDGE('',*,*,#18464,.F.);
#24895=ORIENTED_EDGE('',*,*,#18465,.T.);
#24896=ORIENTED_EDGE('',*,*,#18466,.T.);
#24897=ORIENTED_EDGE('',*,*,#18461,.F.);
#24898=ORIENTED_EDGE('',*,*,#18467,.F.);
#24899=ORIENTED_EDGE('',*,*,#18468,.T.);
#24900=ORIENTED_EDGE('',*,*,#18469,.T.);
#24901=ORIENTED_EDGE('',*,*,#18465,.F.);
#24902=ORIENTED_EDGE('',*,*,#18470,.F.);
#24903=ORIENTED_EDGE('',*,*,#18463,.T.);
#24904=ORIENTED_EDGE('',*,*,#18471,.T.);
#24905=ORIENTED_EDGE('',*,*,#18468,.F.);
#24906=ORIENTED_EDGE('',*,*,#18471,.F.);
#24907=ORIENTED_EDGE('',*,*,#18462,.F.);
#24908=ORIENTED_EDGE('',*,*,#18466,.F.);
#24909=ORIENTED_EDGE('',*,*,#18469,.F.);
#24910=ORIENTED_EDGE('',*,*,#18472,.F.);
#24911=ORIENTED_EDGE('',*,*,#18473,.T.);
#24912=ORIENTED_EDGE('',*,*,#18474,.T.);
#24913=ORIENTED_EDGE('',*,*,#18475,.F.);
#24914=ORIENTED_EDGE('',*,*,#18476,.F.);
#24915=ORIENTED_EDGE('',*,*,#18477,.T.);
#24916=ORIENTED_EDGE('',*,*,#18478,.T.);
#24917=ORIENTED_EDGE('',*,*,#18473,.F.);
#24918=ORIENTED_EDGE('',*,*,#18479,.F.);
#24919=ORIENTED_EDGE('',*,*,#18480,.T.);
#24920=ORIENTED_EDGE('',*,*,#18481,.T.);
#24921=ORIENTED_EDGE('',*,*,#18477,.F.);
#24922=ORIENTED_EDGE('',*,*,#18482,.F.);
#24923=ORIENTED_EDGE('',*,*,#18475,.T.);
#24924=ORIENTED_EDGE('',*,*,#18483,.T.);
#24925=ORIENTED_EDGE('',*,*,#18480,.F.);
#24926=ORIENTED_EDGE('',*,*,#18483,.F.);
#24927=ORIENTED_EDGE('',*,*,#18474,.F.);
#24928=ORIENTED_EDGE('',*,*,#18478,.F.);
#24929=ORIENTED_EDGE('',*,*,#18481,.F.);
#24930=ORIENTED_EDGE('',*,*,#18484,.F.);
#24931=ORIENTED_EDGE('',*,*,#18485,.T.);
#24932=ORIENTED_EDGE('',*,*,#18486,.T.);
#24933=ORIENTED_EDGE('',*,*,#18487,.F.);
#24934=ORIENTED_EDGE('',*,*,#18488,.F.);
#24935=ORIENTED_EDGE('',*,*,#18489,.T.);
#24936=ORIENTED_EDGE('',*,*,#18490,.T.);
#24937=ORIENTED_EDGE('',*,*,#18485,.F.);
#24938=ORIENTED_EDGE('',*,*,#18491,.F.);
#24939=ORIENTED_EDGE('',*,*,#18492,.T.);
#24940=ORIENTED_EDGE('',*,*,#18493,.T.);
#24941=ORIENTED_EDGE('',*,*,#18489,.F.);
#24942=ORIENTED_EDGE('',*,*,#18494,.F.);
#24943=ORIENTED_EDGE('',*,*,#18487,.T.);
#24944=ORIENTED_EDGE('',*,*,#18495,.T.);
#24945=ORIENTED_EDGE('',*,*,#18492,.F.);
#24946=ORIENTED_EDGE('',*,*,#18495,.F.);
#24947=ORIENTED_EDGE('',*,*,#18486,.F.);
#24948=ORIENTED_EDGE('',*,*,#18490,.F.);
#24949=ORIENTED_EDGE('',*,*,#18493,.F.);
#24950=ORIENTED_EDGE('',*,*,#18496,.F.);
#24951=ORIENTED_EDGE('',*,*,#18497,.T.);
#24952=ORIENTED_EDGE('',*,*,#18498,.T.);
#24953=ORIENTED_EDGE('',*,*,#18499,.F.);
#24954=ORIENTED_EDGE('',*,*,#18500,.F.);
#24955=ORIENTED_EDGE('',*,*,#18501,.T.);
#24956=ORIENTED_EDGE('',*,*,#18502,.T.);
#24957=ORIENTED_EDGE('',*,*,#18497,.F.);
#24958=ORIENTED_EDGE('',*,*,#18503,.F.);
#24959=ORIENTED_EDGE('',*,*,#18504,.T.);
#24960=ORIENTED_EDGE('',*,*,#18505,.T.);
#24961=ORIENTED_EDGE('',*,*,#18501,.F.);
#24962=ORIENTED_EDGE('',*,*,#18506,.F.);
#24963=ORIENTED_EDGE('',*,*,#18499,.T.);
#24964=ORIENTED_EDGE('',*,*,#18507,.T.);
#24965=ORIENTED_EDGE('',*,*,#18504,.F.);
#24966=ORIENTED_EDGE('',*,*,#18507,.F.);
#24967=ORIENTED_EDGE('',*,*,#18498,.F.);
#24968=ORIENTED_EDGE('',*,*,#18502,.F.);
#24969=ORIENTED_EDGE('',*,*,#18505,.F.);
#24970=ORIENTED_EDGE('',*,*,#18508,.F.);
#24971=ORIENTED_EDGE('',*,*,#18509,.T.);
#24972=ORIENTED_EDGE('',*,*,#18510,.T.);
#24973=ORIENTED_EDGE('',*,*,#18511,.F.);
#24974=ORIENTED_EDGE('',*,*,#18512,.F.);
#24975=ORIENTED_EDGE('',*,*,#18513,.T.);
#24976=ORIENTED_EDGE('',*,*,#18514,.T.);
#24977=ORIENTED_EDGE('',*,*,#18509,.F.);
#24978=ORIENTED_EDGE('',*,*,#18515,.F.);
#24979=ORIENTED_EDGE('',*,*,#18516,.T.);
#24980=ORIENTED_EDGE('',*,*,#18517,.T.);
#24981=ORIENTED_EDGE('',*,*,#18513,.F.);
#24982=ORIENTED_EDGE('',*,*,#18518,.F.);
#24983=ORIENTED_EDGE('',*,*,#18511,.T.);
#24984=ORIENTED_EDGE('',*,*,#18519,.T.);
#24985=ORIENTED_EDGE('',*,*,#18516,.F.);
#24986=ORIENTED_EDGE('',*,*,#18519,.F.);
#24987=ORIENTED_EDGE('',*,*,#18510,.F.);
#24988=ORIENTED_EDGE('',*,*,#18514,.F.);
#24989=ORIENTED_EDGE('',*,*,#18517,.F.);
#24990=ORIENTED_EDGE('',*,*,#18520,.F.);
#24991=ORIENTED_EDGE('',*,*,#18521,.T.);
#24992=ORIENTED_EDGE('',*,*,#18522,.T.);
#24993=ORIENTED_EDGE('',*,*,#18523,.F.);
#24994=ORIENTED_EDGE('',*,*,#18524,.F.);
#24995=ORIENTED_EDGE('',*,*,#18525,.T.);
#24996=ORIENTED_EDGE('',*,*,#18526,.T.);
#24997=ORIENTED_EDGE('',*,*,#18521,.F.);
#24998=ORIENTED_EDGE('',*,*,#18527,.F.);
#24999=ORIENTED_EDGE('',*,*,#18528,.T.);
#25000=ORIENTED_EDGE('',*,*,#18529,.T.);
#25001=ORIENTED_EDGE('',*,*,#18525,.F.);
#25002=ORIENTED_EDGE('',*,*,#18530,.F.);
#25003=ORIENTED_EDGE('',*,*,#18523,.T.);
#25004=ORIENTED_EDGE('',*,*,#18531,.T.);
#25005=ORIENTED_EDGE('',*,*,#18528,.F.);
#25006=ORIENTED_EDGE('',*,*,#18531,.F.);
#25007=ORIENTED_EDGE('',*,*,#18522,.F.);
#25008=ORIENTED_EDGE('',*,*,#18526,.F.);
#25009=ORIENTED_EDGE('',*,*,#18529,.F.);
#25010=ORIENTED_EDGE('',*,*,#18532,.F.);
#25011=ORIENTED_EDGE('',*,*,#18533,.T.);
#25012=ORIENTED_EDGE('',*,*,#18534,.T.);
#25013=ORIENTED_EDGE('',*,*,#18535,.F.);
#25014=ORIENTED_EDGE('',*,*,#18536,.F.);
#25015=ORIENTED_EDGE('',*,*,#18537,.T.);
#25016=ORIENTED_EDGE('',*,*,#18538,.T.);
#25017=ORIENTED_EDGE('',*,*,#18533,.F.);
#25018=ORIENTED_EDGE('',*,*,#18539,.F.);
#25019=ORIENTED_EDGE('',*,*,#18540,.T.);
#25020=ORIENTED_EDGE('',*,*,#18541,.T.);
#25021=ORIENTED_EDGE('',*,*,#18537,.F.);
#25022=ORIENTED_EDGE('',*,*,#18542,.F.);
#25023=ORIENTED_EDGE('',*,*,#18535,.T.);
#25024=ORIENTED_EDGE('',*,*,#18543,.T.);
#25025=ORIENTED_EDGE('',*,*,#18540,.F.);
#25026=ORIENTED_EDGE('',*,*,#18543,.F.);
#25027=ORIENTED_EDGE('',*,*,#18534,.F.);
#25028=ORIENTED_EDGE('',*,*,#18538,.F.);
#25029=ORIENTED_EDGE('',*,*,#18541,.F.);
#25030=ORIENTED_EDGE('',*,*,#18544,.F.);
#25031=ORIENTED_EDGE('',*,*,#18545,.T.);
#25032=ORIENTED_EDGE('',*,*,#18546,.T.);
#25033=ORIENTED_EDGE('',*,*,#18547,.F.);
#25034=ORIENTED_EDGE('',*,*,#18548,.F.);
#25035=ORIENTED_EDGE('',*,*,#18549,.T.);
#25036=ORIENTED_EDGE('',*,*,#18550,.T.);
#25037=ORIENTED_EDGE('',*,*,#18545,.F.);
#25038=ORIENTED_EDGE('',*,*,#18551,.F.);
#25039=ORIENTED_EDGE('',*,*,#18552,.T.);
#25040=ORIENTED_EDGE('',*,*,#18553,.T.);
#25041=ORIENTED_EDGE('',*,*,#18549,.F.);
#25042=ORIENTED_EDGE('',*,*,#18554,.F.);
#25043=ORIENTED_EDGE('',*,*,#18547,.T.);
#25044=ORIENTED_EDGE('',*,*,#18555,.T.);
#25045=ORIENTED_EDGE('',*,*,#18552,.F.);
#25046=ORIENTED_EDGE('',*,*,#18555,.F.);
#25047=ORIENTED_EDGE('',*,*,#18546,.F.);
#25048=ORIENTED_EDGE('',*,*,#18550,.F.);
#25049=ORIENTED_EDGE('',*,*,#18553,.F.);
#25050=ORIENTED_EDGE('',*,*,#18556,.F.);
#25051=ORIENTED_EDGE('',*,*,#18557,.T.);
#25052=ORIENTED_EDGE('',*,*,#18558,.T.);
#25053=ORIENTED_EDGE('',*,*,#18559,.F.);
#25054=ORIENTED_EDGE('',*,*,#18560,.F.);
#25055=ORIENTED_EDGE('',*,*,#18561,.T.);
#25056=ORIENTED_EDGE('',*,*,#18562,.T.);
#25057=ORIENTED_EDGE('',*,*,#18557,.F.);
#25058=ORIENTED_EDGE('',*,*,#18563,.F.);
#25059=ORIENTED_EDGE('',*,*,#18564,.T.);
#25060=ORIENTED_EDGE('',*,*,#18565,.T.);
#25061=ORIENTED_EDGE('',*,*,#18561,.F.);
#25062=ORIENTED_EDGE('',*,*,#18566,.F.);
#25063=ORIENTED_EDGE('',*,*,#18559,.T.);
#25064=ORIENTED_EDGE('',*,*,#18567,.T.);
#25065=ORIENTED_EDGE('',*,*,#18564,.F.);
#25066=ORIENTED_EDGE('',*,*,#18567,.F.);
#25067=ORIENTED_EDGE('',*,*,#18558,.F.);
#25068=ORIENTED_EDGE('',*,*,#18562,.F.);
#25069=ORIENTED_EDGE('',*,*,#18565,.F.);
#25070=ORIENTED_EDGE('',*,*,#18568,.F.);
#25071=ORIENTED_EDGE('',*,*,#18569,.T.);
#25072=ORIENTED_EDGE('',*,*,#18570,.T.);
#25073=ORIENTED_EDGE('',*,*,#18571,.F.);
#25074=ORIENTED_EDGE('',*,*,#18572,.F.);
#25075=ORIENTED_EDGE('',*,*,#18573,.T.);
#25076=ORIENTED_EDGE('',*,*,#18574,.T.);
#25077=ORIENTED_EDGE('',*,*,#18569,.F.);
#25078=ORIENTED_EDGE('',*,*,#18575,.F.);
#25079=ORIENTED_EDGE('',*,*,#18576,.T.);
#25080=ORIENTED_EDGE('',*,*,#18577,.T.);
#25081=ORIENTED_EDGE('',*,*,#18573,.F.);
#25082=ORIENTED_EDGE('',*,*,#18578,.F.);
#25083=ORIENTED_EDGE('',*,*,#18571,.T.);
#25084=ORIENTED_EDGE('',*,*,#18579,.T.);
#25085=ORIENTED_EDGE('',*,*,#18576,.F.);
#25086=ORIENTED_EDGE('',*,*,#18579,.F.);
#25087=ORIENTED_EDGE('',*,*,#18570,.F.);
#25088=ORIENTED_EDGE('',*,*,#18574,.F.);
#25089=ORIENTED_EDGE('',*,*,#18577,.F.);
#25090=ORIENTED_EDGE('',*,*,#18580,.F.);
#25091=ORIENTED_EDGE('',*,*,#18581,.T.);
#25092=ORIENTED_EDGE('',*,*,#18582,.T.);
#25093=ORIENTED_EDGE('',*,*,#18583,.F.);
#25094=ORIENTED_EDGE('',*,*,#18584,.F.);
#25095=ORIENTED_EDGE('',*,*,#18585,.T.);
#25096=ORIENTED_EDGE('',*,*,#18586,.T.);
#25097=ORIENTED_EDGE('',*,*,#18581,.F.);
#25098=ORIENTED_EDGE('',*,*,#18587,.F.);
#25099=ORIENTED_EDGE('',*,*,#18588,.T.);
#25100=ORIENTED_EDGE('',*,*,#18589,.T.);
#25101=ORIENTED_EDGE('',*,*,#18585,.F.);
#25102=ORIENTED_EDGE('',*,*,#18590,.F.);
#25103=ORIENTED_EDGE('',*,*,#18583,.T.);
#25104=ORIENTED_EDGE('',*,*,#18591,.T.);
#25105=ORIENTED_EDGE('',*,*,#18588,.F.);
#25106=ORIENTED_EDGE('',*,*,#18591,.F.);
#25107=ORIENTED_EDGE('',*,*,#18582,.F.);
#25108=ORIENTED_EDGE('',*,*,#18586,.F.);
#25109=ORIENTED_EDGE('',*,*,#18589,.F.);
#25110=ORIENTED_EDGE('',*,*,#18592,.F.);
#25111=ORIENTED_EDGE('',*,*,#18593,.T.);
#25112=ORIENTED_EDGE('',*,*,#18594,.T.);
#25113=ORIENTED_EDGE('',*,*,#18595,.F.);
#25114=ORIENTED_EDGE('',*,*,#18596,.F.);
#25115=ORIENTED_EDGE('',*,*,#18597,.T.);
#25116=ORIENTED_EDGE('',*,*,#18598,.T.);
#25117=ORIENTED_EDGE('',*,*,#18593,.F.);
#25118=ORIENTED_EDGE('',*,*,#18599,.F.);
#25119=ORIENTED_EDGE('',*,*,#18600,.T.);
#25120=ORIENTED_EDGE('',*,*,#18601,.T.);
#25121=ORIENTED_EDGE('',*,*,#18597,.F.);
#25122=ORIENTED_EDGE('',*,*,#18602,.F.);
#25123=ORIENTED_EDGE('',*,*,#18595,.T.);
#25124=ORIENTED_EDGE('',*,*,#18603,.T.);
#25125=ORIENTED_EDGE('',*,*,#18600,.F.);
#25126=ORIENTED_EDGE('',*,*,#18603,.F.);
#25127=ORIENTED_EDGE('',*,*,#18594,.F.);
#25128=ORIENTED_EDGE('',*,*,#18598,.F.);
#25129=ORIENTED_EDGE('',*,*,#18601,.F.);
#25130=ORIENTED_EDGE('',*,*,#18604,.F.);
#25131=ORIENTED_EDGE('',*,*,#18605,.T.);
#25132=ORIENTED_EDGE('',*,*,#18606,.T.);
#25133=ORIENTED_EDGE('',*,*,#18607,.F.);
#25134=ORIENTED_EDGE('',*,*,#18608,.F.);
#25135=ORIENTED_EDGE('',*,*,#18609,.T.);
#25136=ORIENTED_EDGE('',*,*,#18610,.T.);
#25137=ORIENTED_EDGE('',*,*,#18605,.F.);
#25138=ORIENTED_EDGE('',*,*,#18611,.F.);
#25139=ORIENTED_EDGE('',*,*,#18612,.T.);
#25140=ORIENTED_EDGE('',*,*,#18613,.T.);
#25141=ORIENTED_EDGE('',*,*,#18609,.F.);
#25142=ORIENTED_EDGE('',*,*,#18614,.F.);
#25143=ORIENTED_EDGE('',*,*,#18607,.T.);
#25144=ORIENTED_EDGE('',*,*,#18615,.T.);
#25145=ORIENTED_EDGE('',*,*,#18612,.F.);
#25146=ORIENTED_EDGE('',*,*,#18615,.F.);
#25147=ORIENTED_EDGE('',*,*,#18606,.F.);
#25148=ORIENTED_EDGE('',*,*,#18610,.F.);
#25149=ORIENTED_EDGE('',*,*,#18613,.F.);
#25150=ORIENTED_EDGE('',*,*,#18616,.F.);
#25151=ORIENTED_EDGE('',*,*,#18617,.T.);
#25152=ORIENTED_EDGE('',*,*,#18618,.T.);
#25153=ORIENTED_EDGE('',*,*,#18619,.F.);
#25154=ORIENTED_EDGE('',*,*,#18620,.F.);
#25155=ORIENTED_EDGE('',*,*,#18621,.T.);
#25156=ORIENTED_EDGE('',*,*,#18622,.T.);
#25157=ORIENTED_EDGE('',*,*,#18617,.F.);
#25158=ORIENTED_EDGE('',*,*,#18623,.F.);
#25159=ORIENTED_EDGE('',*,*,#18624,.T.);
#25160=ORIENTED_EDGE('',*,*,#18625,.T.);
#25161=ORIENTED_EDGE('',*,*,#18621,.F.);
#25162=ORIENTED_EDGE('',*,*,#18626,.F.);
#25163=ORIENTED_EDGE('',*,*,#18619,.T.);
#25164=ORIENTED_EDGE('',*,*,#18627,.T.);
#25165=ORIENTED_EDGE('',*,*,#18624,.F.);
#25166=ORIENTED_EDGE('',*,*,#18627,.F.);
#25167=ORIENTED_EDGE('',*,*,#18618,.F.);
#25168=ORIENTED_EDGE('',*,*,#18622,.F.);
#25169=ORIENTED_EDGE('',*,*,#18625,.F.);
#25170=ORIENTED_EDGE('',*,*,#18628,.F.);
#25171=ORIENTED_EDGE('',*,*,#18629,.T.);
#25172=ORIENTED_EDGE('',*,*,#18630,.T.);
#25173=ORIENTED_EDGE('',*,*,#18631,.F.);
#25174=ORIENTED_EDGE('',*,*,#18632,.F.);
#25175=ORIENTED_EDGE('',*,*,#18633,.T.);
#25176=ORIENTED_EDGE('',*,*,#18634,.T.);
#25177=ORIENTED_EDGE('',*,*,#18629,.F.);
#25178=ORIENTED_EDGE('',*,*,#18635,.F.);
#25179=ORIENTED_EDGE('',*,*,#18636,.T.);
#25180=ORIENTED_EDGE('',*,*,#18637,.T.);
#25181=ORIENTED_EDGE('',*,*,#18633,.F.);
#25182=ORIENTED_EDGE('',*,*,#18638,.F.);
#25183=ORIENTED_EDGE('',*,*,#18631,.T.);
#25184=ORIENTED_EDGE('',*,*,#18639,.T.);
#25185=ORIENTED_EDGE('',*,*,#18636,.F.);
#25186=ORIENTED_EDGE('',*,*,#18639,.F.);
#25187=ORIENTED_EDGE('',*,*,#18630,.F.);
#25188=ORIENTED_EDGE('',*,*,#18634,.F.);
#25189=ORIENTED_EDGE('',*,*,#18637,.F.);
#25190=ORIENTED_EDGE('',*,*,#18640,.F.);
#25191=ORIENTED_EDGE('',*,*,#18641,.T.);
#25192=ORIENTED_EDGE('',*,*,#18642,.T.);
#25193=ORIENTED_EDGE('',*,*,#18643,.F.);
#25194=ORIENTED_EDGE('',*,*,#18644,.F.);
#25195=ORIENTED_EDGE('',*,*,#18645,.T.);
#25196=ORIENTED_EDGE('',*,*,#18646,.T.);
#25197=ORIENTED_EDGE('',*,*,#18641,.F.);
#25198=ORIENTED_EDGE('',*,*,#18647,.F.);
#25199=ORIENTED_EDGE('',*,*,#18648,.T.);
#25200=ORIENTED_EDGE('',*,*,#18649,.T.);
#25201=ORIENTED_EDGE('',*,*,#18645,.F.);
#25202=ORIENTED_EDGE('',*,*,#18650,.F.);
#25203=ORIENTED_EDGE('',*,*,#18643,.T.);
#25204=ORIENTED_EDGE('',*,*,#18651,.T.);
#25205=ORIENTED_EDGE('',*,*,#18648,.F.);
#25206=ORIENTED_EDGE('',*,*,#18651,.F.);
#25207=ORIENTED_EDGE('',*,*,#18642,.F.);
#25208=ORIENTED_EDGE('',*,*,#18646,.F.);
#25209=ORIENTED_EDGE('',*,*,#18649,.F.);
#25210=ORIENTED_EDGE('',*,*,#18652,.F.);
#25211=ORIENTED_EDGE('',*,*,#18653,.T.);
#25212=ORIENTED_EDGE('',*,*,#18654,.T.);
#25213=ORIENTED_EDGE('',*,*,#18655,.F.);
#25214=ORIENTED_EDGE('',*,*,#18656,.F.);
#25215=ORIENTED_EDGE('',*,*,#18657,.T.);
#25216=ORIENTED_EDGE('',*,*,#18658,.T.);
#25217=ORIENTED_EDGE('',*,*,#18653,.F.);
#25218=ORIENTED_EDGE('',*,*,#18659,.F.);
#25219=ORIENTED_EDGE('',*,*,#18660,.T.);
#25220=ORIENTED_EDGE('',*,*,#18661,.T.);
#25221=ORIENTED_EDGE('',*,*,#18657,.F.);
#25222=ORIENTED_EDGE('',*,*,#18662,.F.);
#25223=ORIENTED_EDGE('',*,*,#18655,.T.);
#25224=ORIENTED_EDGE('',*,*,#18663,.T.);
#25225=ORIENTED_EDGE('',*,*,#18660,.F.);
#25226=ORIENTED_EDGE('',*,*,#18663,.F.);
#25227=ORIENTED_EDGE('',*,*,#18654,.F.);
#25228=ORIENTED_EDGE('',*,*,#18658,.F.);
#25229=ORIENTED_EDGE('',*,*,#18661,.F.);
#25230=ORIENTED_EDGE('',*,*,#18664,.F.);
#25231=ORIENTED_EDGE('',*,*,#18665,.T.);
#25232=ORIENTED_EDGE('',*,*,#18666,.T.);
#25233=ORIENTED_EDGE('',*,*,#18667,.F.);
#25234=ORIENTED_EDGE('',*,*,#18668,.F.);
#25235=ORIENTED_EDGE('',*,*,#18669,.T.);
#25236=ORIENTED_EDGE('',*,*,#18670,.T.);
#25237=ORIENTED_EDGE('',*,*,#18665,.F.);
#25238=ORIENTED_EDGE('',*,*,#18671,.F.);
#25239=ORIENTED_EDGE('',*,*,#18672,.T.);
#25240=ORIENTED_EDGE('',*,*,#18673,.T.);
#25241=ORIENTED_EDGE('',*,*,#18669,.F.);
#25242=ORIENTED_EDGE('',*,*,#18674,.F.);
#25243=ORIENTED_EDGE('',*,*,#18667,.T.);
#25244=ORIENTED_EDGE('',*,*,#18675,.T.);
#25245=ORIENTED_EDGE('',*,*,#18672,.F.);
#25246=ORIENTED_EDGE('',*,*,#18675,.F.);
#25247=ORIENTED_EDGE('',*,*,#18666,.F.);
#25248=ORIENTED_EDGE('',*,*,#18670,.F.);
#25249=ORIENTED_EDGE('',*,*,#18673,.F.);
#25250=ORIENTED_EDGE('',*,*,#18676,.F.);
#25251=ORIENTED_EDGE('',*,*,#18677,.T.);
#25252=ORIENTED_EDGE('',*,*,#18678,.T.);
#25253=ORIENTED_EDGE('',*,*,#18679,.F.);
#25254=ORIENTED_EDGE('',*,*,#18680,.F.);
#25255=ORIENTED_EDGE('',*,*,#18681,.T.);
#25256=ORIENTED_EDGE('',*,*,#18682,.T.);
#25257=ORIENTED_EDGE('',*,*,#18677,.F.);
#25258=ORIENTED_EDGE('',*,*,#18683,.F.);
#25259=ORIENTED_EDGE('',*,*,#18684,.T.);
#25260=ORIENTED_EDGE('',*,*,#18685,.T.);
#25261=ORIENTED_EDGE('',*,*,#18681,.F.);
#25262=ORIENTED_EDGE('',*,*,#18686,.F.);
#25263=ORIENTED_EDGE('',*,*,#18679,.T.);
#25264=ORIENTED_EDGE('',*,*,#18687,.T.);
#25265=ORIENTED_EDGE('',*,*,#18684,.F.);
#25266=ORIENTED_EDGE('',*,*,#18687,.F.);
#25267=ORIENTED_EDGE('',*,*,#18678,.F.);
#25268=ORIENTED_EDGE('',*,*,#18682,.F.);
#25269=ORIENTED_EDGE('',*,*,#18685,.F.);
#25270=ORIENTED_EDGE('',*,*,#18688,.F.);
#25271=ORIENTED_EDGE('',*,*,#18689,.T.);
#25272=ORIENTED_EDGE('',*,*,#18690,.T.);
#25273=ORIENTED_EDGE('',*,*,#18691,.F.);
#25274=ORIENTED_EDGE('',*,*,#18692,.F.);
#25275=ORIENTED_EDGE('',*,*,#18693,.T.);
#25276=ORIENTED_EDGE('',*,*,#18694,.T.);
#25277=ORIENTED_EDGE('',*,*,#18689,.F.);
#25278=ORIENTED_EDGE('',*,*,#18695,.F.);
#25279=ORIENTED_EDGE('',*,*,#18696,.T.);
#25280=ORIENTED_EDGE('',*,*,#18697,.T.);
#25281=ORIENTED_EDGE('',*,*,#18693,.F.);
#25282=ORIENTED_EDGE('',*,*,#18698,.F.);
#25283=ORIENTED_EDGE('',*,*,#18691,.T.);
#25284=ORIENTED_EDGE('',*,*,#18699,.T.);
#25285=ORIENTED_EDGE('',*,*,#18696,.F.);
#25286=ORIENTED_EDGE('',*,*,#18699,.F.);
#25287=ORIENTED_EDGE('',*,*,#18690,.F.);
#25288=ORIENTED_EDGE('',*,*,#18694,.F.);
#25289=ORIENTED_EDGE('',*,*,#18697,.F.);
#25290=ORIENTED_EDGE('',*,*,#18700,.F.);
#25291=ORIENTED_EDGE('',*,*,#18701,.T.);
#25292=ORIENTED_EDGE('',*,*,#18702,.T.);
#25293=ORIENTED_EDGE('',*,*,#18703,.F.);
#25294=ORIENTED_EDGE('',*,*,#18704,.F.);
#25295=ORIENTED_EDGE('',*,*,#18705,.T.);
#25296=ORIENTED_EDGE('',*,*,#18706,.T.);
#25297=ORIENTED_EDGE('',*,*,#18701,.F.);
#25298=ORIENTED_EDGE('',*,*,#18707,.F.);
#25299=ORIENTED_EDGE('',*,*,#18708,.T.);
#25300=ORIENTED_EDGE('',*,*,#18709,.T.);
#25301=ORIENTED_EDGE('',*,*,#18705,.F.);
#25302=ORIENTED_EDGE('',*,*,#18710,.F.);
#25303=ORIENTED_EDGE('',*,*,#18703,.T.);
#25304=ORIENTED_EDGE('',*,*,#18711,.T.);
#25305=ORIENTED_EDGE('',*,*,#18708,.F.);
#25306=ORIENTED_EDGE('',*,*,#18711,.F.);
#25307=ORIENTED_EDGE('',*,*,#18702,.F.);
#25308=ORIENTED_EDGE('',*,*,#18706,.F.);
#25309=ORIENTED_EDGE('',*,*,#18709,.F.);
#25310=ORIENTED_EDGE('',*,*,#18712,.F.);
#25311=ORIENTED_EDGE('',*,*,#18713,.T.);
#25312=ORIENTED_EDGE('',*,*,#18714,.T.);
#25313=ORIENTED_EDGE('',*,*,#18715,.F.);
#25314=ORIENTED_EDGE('',*,*,#18716,.F.);
#25315=ORIENTED_EDGE('',*,*,#18717,.T.);
#25316=ORIENTED_EDGE('',*,*,#18718,.T.);
#25317=ORIENTED_EDGE('',*,*,#18713,.F.);
#25318=ORIENTED_EDGE('',*,*,#18719,.F.);
#25319=ORIENTED_EDGE('',*,*,#18720,.T.);
#25320=ORIENTED_EDGE('',*,*,#18721,.T.);
#25321=ORIENTED_EDGE('',*,*,#18717,.F.);
#25322=ORIENTED_EDGE('',*,*,#18722,.F.);
#25323=ORIENTED_EDGE('',*,*,#18715,.T.);
#25324=ORIENTED_EDGE('',*,*,#18723,.T.);
#25325=ORIENTED_EDGE('',*,*,#18720,.F.);
#25326=ORIENTED_EDGE('',*,*,#18723,.F.);
#25327=ORIENTED_EDGE('',*,*,#18714,.F.);
#25328=ORIENTED_EDGE('',*,*,#18718,.F.);
#25329=ORIENTED_EDGE('',*,*,#18721,.F.);
#25330=ORIENTED_EDGE('',*,*,#18724,.F.);
#25331=ORIENTED_EDGE('',*,*,#18725,.T.);
#25332=ORIENTED_EDGE('',*,*,#18726,.T.);
#25333=ORIENTED_EDGE('',*,*,#18727,.F.);
#25334=ORIENTED_EDGE('',*,*,#18728,.F.);
#25335=ORIENTED_EDGE('',*,*,#18729,.T.);
#25336=ORIENTED_EDGE('',*,*,#18730,.T.);
#25337=ORIENTED_EDGE('',*,*,#18725,.F.);
#25338=ORIENTED_EDGE('',*,*,#18731,.F.);
#25339=ORIENTED_EDGE('',*,*,#18732,.T.);
#25340=ORIENTED_EDGE('',*,*,#18733,.T.);
#25341=ORIENTED_EDGE('',*,*,#18729,.F.);
#25342=ORIENTED_EDGE('',*,*,#18734,.F.);
#25343=ORIENTED_EDGE('',*,*,#18727,.T.);
#25344=ORIENTED_EDGE('',*,*,#18735,.T.);
#25345=ORIENTED_EDGE('',*,*,#18732,.F.);
#25346=ORIENTED_EDGE('',*,*,#18735,.F.);
#25347=ORIENTED_EDGE('',*,*,#18726,.F.);
#25348=ORIENTED_EDGE('',*,*,#18730,.F.);
#25349=ORIENTED_EDGE('',*,*,#18733,.F.);
#25350=ORIENTED_EDGE('',*,*,#18736,.F.);
#25351=ORIENTED_EDGE('',*,*,#18737,.T.);
#25352=ORIENTED_EDGE('',*,*,#18738,.T.);
#25353=ORIENTED_EDGE('',*,*,#18739,.F.);
#25354=ORIENTED_EDGE('',*,*,#18740,.F.);
#25355=ORIENTED_EDGE('',*,*,#18741,.T.);
#25356=ORIENTED_EDGE('',*,*,#18742,.T.);
#25357=ORIENTED_EDGE('',*,*,#18737,.F.);
#25358=ORIENTED_EDGE('',*,*,#18743,.F.);
#25359=ORIENTED_EDGE('',*,*,#18744,.T.);
#25360=ORIENTED_EDGE('',*,*,#18745,.T.);
#25361=ORIENTED_EDGE('',*,*,#18741,.F.);
#25362=ORIENTED_EDGE('',*,*,#18746,.F.);
#25363=ORIENTED_EDGE('',*,*,#18739,.T.);
#25364=ORIENTED_EDGE('',*,*,#18747,.T.);
#25365=ORIENTED_EDGE('',*,*,#18744,.F.);
#25366=ORIENTED_EDGE('',*,*,#18747,.F.);
#25367=ORIENTED_EDGE('',*,*,#18738,.F.);
#25368=ORIENTED_EDGE('',*,*,#18742,.F.);
#25369=ORIENTED_EDGE('',*,*,#18745,.F.);
#25370=ORIENTED_EDGE('',*,*,#18748,.F.);
#25371=ORIENTED_EDGE('',*,*,#18749,.T.);
#25372=ORIENTED_EDGE('',*,*,#18750,.T.);
#25373=ORIENTED_EDGE('',*,*,#18751,.F.);
#25374=ORIENTED_EDGE('',*,*,#18752,.F.);
#25375=ORIENTED_EDGE('',*,*,#18753,.T.);
#25376=ORIENTED_EDGE('',*,*,#18754,.T.);
#25377=ORIENTED_EDGE('',*,*,#18749,.F.);
#25378=ORIENTED_EDGE('',*,*,#18755,.F.);
#25379=ORIENTED_EDGE('',*,*,#18756,.T.);
#25380=ORIENTED_EDGE('',*,*,#18757,.T.);
#25381=ORIENTED_EDGE('',*,*,#18753,.F.);
#25382=ORIENTED_EDGE('',*,*,#18758,.F.);
#25383=ORIENTED_EDGE('',*,*,#18751,.T.);
#25384=ORIENTED_EDGE('',*,*,#18759,.T.);
#25385=ORIENTED_EDGE('',*,*,#18756,.F.);
#25386=ORIENTED_EDGE('',*,*,#18759,.F.);
#25387=ORIENTED_EDGE('',*,*,#18750,.F.);
#25388=ORIENTED_EDGE('',*,*,#18754,.F.);
#25389=ORIENTED_EDGE('',*,*,#18757,.F.);
#25390=ORIENTED_EDGE('',*,*,#18760,.F.);
#25391=ORIENTED_EDGE('',*,*,#18761,.T.);
#25392=ORIENTED_EDGE('',*,*,#18762,.T.);
#25393=ORIENTED_EDGE('',*,*,#18763,.F.);
#25394=ORIENTED_EDGE('',*,*,#18764,.F.);
#25395=ORIENTED_EDGE('',*,*,#18765,.T.);
#25396=ORIENTED_EDGE('',*,*,#18766,.T.);
#25397=ORIENTED_EDGE('',*,*,#18761,.F.);
#25398=ORIENTED_EDGE('',*,*,#18767,.F.);
#25399=ORIENTED_EDGE('',*,*,#18768,.T.);
#25400=ORIENTED_EDGE('',*,*,#18769,.T.);
#25401=ORIENTED_EDGE('',*,*,#18765,.F.);
#25402=ORIENTED_EDGE('',*,*,#18770,.F.);
#25403=ORIENTED_EDGE('',*,*,#18763,.T.);
#25404=ORIENTED_EDGE('',*,*,#18771,.T.);
#25405=ORIENTED_EDGE('',*,*,#18768,.F.);
#25406=ORIENTED_EDGE('',*,*,#18771,.F.);
#25407=ORIENTED_EDGE('',*,*,#18762,.F.);
#25408=ORIENTED_EDGE('',*,*,#18766,.F.);
#25409=ORIENTED_EDGE('',*,*,#18769,.F.);
#25410=ORIENTED_EDGE('',*,*,#18772,.F.);
#25411=ORIENTED_EDGE('',*,*,#18773,.T.);
#25412=ORIENTED_EDGE('',*,*,#18774,.T.);
#25413=ORIENTED_EDGE('',*,*,#18775,.F.);
#25414=ORIENTED_EDGE('',*,*,#18776,.F.);
#25415=ORIENTED_EDGE('',*,*,#18777,.T.);
#25416=ORIENTED_EDGE('',*,*,#18778,.T.);
#25417=ORIENTED_EDGE('',*,*,#18773,.F.);
#25418=ORIENTED_EDGE('',*,*,#18779,.F.);
#25419=ORIENTED_EDGE('',*,*,#18780,.T.);
#25420=ORIENTED_EDGE('',*,*,#18781,.T.);
#25421=ORIENTED_EDGE('',*,*,#18777,.F.);
#25422=ORIENTED_EDGE('',*,*,#18782,.F.);
#25423=ORIENTED_EDGE('',*,*,#18775,.T.);
#25424=ORIENTED_EDGE('',*,*,#18783,.T.);
#25425=ORIENTED_EDGE('',*,*,#18780,.F.);
#25426=ORIENTED_EDGE('',*,*,#18783,.F.);
#25427=ORIENTED_EDGE('',*,*,#18774,.F.);
#25428=ORIENTED_EDGE('',*,*,#18778,.F.);
#25429=ORIENTED_EDGE('',*,*,#18781,.F.);
#25430=ORIENTED_EDGE('',*,*,#18784,.F.);
#25431=ORIENTED_EDGE('',*,*,#18785,.T.);
#25432=ORIENTED_EDGE('',*,*,#18786,.T.);
#25433=ORIENTED_EDGE('',*,*,#18787,.F.);
#25434=ORIENTED_EDGE('',*,*,#18788,.F.);
#25435=ORIENTED_EDGE('',*,*,#18789,.T.);
#25436=ORIENTED_EDGE('',*,*,#18790,.T.);
#25437=ORIENTED_EDGE('',*,*,#18785,.F.);
#25438=ORIENTED_EDGE('',*,*,#18791,.F.);
#25439=ORIENTED_EDGE('',*,*,#18792,.T.);
#25440=ORIENTED_EDGE('',*,*,#18793,.T.);
#25441=ORIENTED_EDGE('',*,*,#18789,.F.);
#25442=ORIENTED_EDGE('',*,*,#18794,.F.);
#25443=ORIENTED_EDGE('',*,*,#18787,.T.);
#25444=ORIENTED_EDGE('',*,*,#18795,.T.);
#25445=ORIENTED_EDGE('',*,*,#18792,.F.);
#25446=ORIENTED_EDGE('',*,*,#18795,.F.);
#25447=ORIENTED_EDGE('',*,*,#18786,.F.);
#25448=ORIENTED_EDGE('',*,*,#18790,.F.);
#25449=ORIENTED_EDGE('',*,*,#18793,.F.);
#25450=ORIENTED_EDGE('',*,*,#18796,.F.);
#25451=ORIENTED_EDGE('',*,*,#18797,.T.);
#25452=ORIENTED_EDGE('',*,*,#18798,.T.);
#25453=ORIENTED_EDGE('',*,*,#18799,.F.);
#25454=ORIENTED_EDGE('',*,*,#18800,.F.);
#25455=ORIENTED_EDGE('',*,*,#18801,.T.);
#25456=ORIENTED_EDGE('',*,*,#18802,.T.);
#25457=ORIENTED_EDGE('',*,*,#18797,.F.);
#25458=ORIENTED_EDGE('',*,*,#18803,.F.);
#25459=ORIENTED_EDGE('',*,*,#18804,.T.);
#25460=ORIENTED_EDGE('',*,*,#18805,.T.);
#25461=ORIENTED_EDGE('',*,*,#18801,.F.);
#25462=ORIENTED_EDGE('',*,*,#18806,.F.);
#25463=ORIENTED_EDGE('',*,*,#18799,.T.);
#25464=ORIENTED_EDGE('',*,*,#18807,.T.);
#25465=ORIENTED_EDGE('',*,*,#18804,.F.);
#25466=ORIENTED_EDGE('',*,*,#18807,.F.);
#25467=ORIENTED_EDGE('',*,*,#18798,.F.);
#25468=ORIENTED_EDGE('',*,*,#18802,.F.);
#25469=ORIENTED_EDGE('',*,*,#18805,.F.);
#25470=ORIENTED_EDGE('',*,*,#18808,.F.);
#25471=ORIENTED_EDGE('',*,*,#18809,.T.);
#25472=ORIENTED_EDGE('',*,*,#18810,.T.);
#25473=ORIENTED_EDGE('',*,*,#18811,.F.);
#25474=ORIENTED_EDGE('',*,*,#18812,.F.);
#25475=ORIENTED_EDGE('',*,*,#18813,.T.);
#25476=ORIENTED_EDGE('',*,*,#18814,.T.);
#25477=ORIENTED_EDGE('',*,*,#18809,.F.);
#25478=ORIENTED_EDGE('',*,*,#18815,.F.);
#25479=ORIENTED_EDGE('',*,*,#18816,.T.);
#25480=ORIENTED_EDGE('',*,*,#18817,.T.);
#25481=ORIENTED_EDGE('',*,*,#18813,.F.);
#25482=ORIENTED_EDGE('',*,*,#18818,.F.);
#25483=ORIENTED_EDGE('',*,*,#18811,.T.);
#25484=ORIENTED_EDGE('',*,*,#18819,.T.);
#25485=ORIENTED_EDGE('',*,*,#18816,.F.);
#25486=ORIENTED_EDGE('',*,*,#18819,.F.);
#25487=ORIENTED_EDGE('',*,*,#18810,.F.);
#25488=ORIENTED_EDGE('',*,*,#18814,.F.);
#25489=ORIENTED_EDGE('',*,*,#18817,.F.);
#25490=ORIENTED_EDGE('',*,*,#18820,.F.);
#25491=ORIENTED_EDGE('',*,*,#18821,.T.);
#25492=ORIENTED_EDGE('',*,*,#18822,.T.);
#25493=ORIENTED_EDGE('',*,*,#18823,.F.);
#25494=ORIENTED_EDGE('',*,*,#18824,.F.);
#25495=ORIENTED_EDGE('',*,*,#18825,.T.);
#25496=ORIENTED_EDGE('',*,*,#18826,.T.);
#25497=ORIENTED_EDGE('',*,*,#18821,.F.);
#25498=ORIENTED_EDGE('',*,*,#18827,.F.);
#25499=ORIENTED_EDGE('',*,*,#18828,.T.);
#25500=ORIENTED_EDGE('',*,*,#18829,.T.);
#25501=ORIENTED_EDGE('',*,*,#18825,.F.);
#25502=ORIENTED_EDGE('',*,*,#18830,.F.);
#25503=ORIENTED_EDGE('',*,*,#18823,.T.);
#25504=ORIENTED_EDGE('',*,*,#18831,.T.);
#25505=ORIENTED_EDGE('',*,*,#18828,.F.);
#25506=ORIENTED_EDGE('',*,*,#18831,.F.);
#25507=ORIENTED_EDGE('',*,*,#18822,.F.);
#25508=ORIENTED_EDGE('',*,*,#18826,.F.);
#25509=ORIENTED_EDGE('',*,*,#18829,.F.);
#25510=ORIENTED_EDGE('',*,*,#18832,.F.);
#25511=ORIENTED_EDGE('',*,*,#18833,.T.);
#25512=ORIENTED_EDGE('',*,*,#18834,.T.);
#25513=ORIENTED_EDGE('',*,*,#18835,.F.);
#25514=ORIENTED_EDGE('',*,*,#18836,.F.);
#25515=ORIENTED_EDGE('',*,*,#18837,.T.);
#25516=ORIENTED_EDGE('',*,*,#18838,.T.);
#25517=ORIENTED_EDGE('',*,*,#18833,.F.);
#25518=ORIENTED_EDGE('',*,*,#18839,.F.);
#25519=ORIENTED_EDGE('',*,*,#18840,.T.);
#25520=ORIENTED_EDGE('',*,*,#18841,.T.);
#25521=ORIENTED_EDGE('',*,*,#18837,.F.);
#25522=ORIENTED_EDGE('',*,*,#18842,.F.);
#25523=ORIENTED_EDGE('',*,*,#18835,.T.);
#25524=ORIENTED_EDGE('',*,*,#18843,.T.);
#25525=ORIENTED_EDGE('',*,*,#18840,.F.);
#25526=ORIENTED_EDGE('',*,*,#18843,.F.);
#25527=ORIENTED_EDGE('',*,*,#18834,.F.);
#25528=ORIENTED_EDGE('',*,*,#18838,.F.);
#25529=ORIENTED_EDGE('',*,*,#18841,.F.);
#25530=ORIENTED_EDGE('',*,*,#18844,.F.);
#25531=ORIENTED_EDGE('',*,*,#18845,.T.);
#25532=ORIENTED_EDGE('',*,*,#18846,.T.);
#25533=ORIENTED_EDGE('',*,*,#18847,.F.);
#25534=ORIENTED_EDGE('',*,*,#18848,.F.);
#25535=ORIENTED_EDGE('',*,*,#18849,.T.);
#25536=ORIENTED_EDGE('',*,*,#18850,.T.);
#25537=ORIENTED_EDGE('',*,*,#18845,.F.);
#25538=ORIENTED_EDGE('',*,*,#18851,.F.);
#25539=ORIENTED_EDGE('',*,*,#18852,.T.);
#25540=ORIENTED_EDGE('',*,*,#18853,.T.);
#25541=ORIENTED_EDGE('',*,*,#18849,.F.);
#25542=ORIENTED_EDGE('',*,*,#18854,.F.);
#25543=ORIENTED_EDGE('',*,*,#18847,.T.);
#25544=ORIENTED_EDGE('',*,*,#18855,.T.);
#25545=ORIENTED_EDGE('',*,*,#18852,.F.);
#25546=ORIENTED_EDGE('',*,*,#18855,.F.);
#25547=ORIENTED_EDGE('',*,*,#18846,.F.);
#25548=ORIENTED_EDGE('',*,*,#18850,.F.);
#25549=ORIENTED_EDGE('',*,*,#18853,.F.);
#25550=ORIENTED_EDGE('',*,*,#18856,.F.);
#25551=ORIENTED_EDGE('',*,*,#18857,.T.);
#25552=ORIENTED_EDGE('',*,*,#18858,.T.);
#25553=ORIENTED_EDGE('',*,*,#18859,.F.);
#25554=ORIENTED_EDGE('',*,*,#18860,.F.);
#25555=ORIENTED_EDGE('',*,*,#18861,.T.);
#25556=ORIENTED_EDGE('',*,*,#18862,.T.);
#25557=ORIENTED_EDGE('',*,*,#18857,.F.);
#25558=ORIENTED_EDGE('',*,*,#18863,.F.);
#25559=ORIENTED_EDGE('',*,*,#18864,.T.);
#25560=ORIENTED_EDGE('',*,*,#18865,.T.);
#25561=ORIENTED_EDGE('',*,*,#18861,.F.);
#25562=ORIENTED_EDGE('',*,*,#18866,.F.);
#25563=ORIENTED_EDGE('',*,*,#18859,.T.);
#25564=ORIENTED_EDGE('',*,*,#18867,.T.);
#25565=ORIENTED_EDGE('',*,*,#18864,.F.);
#25566=ORIENTED_EDGE('',*,*,#18867,.F.);
#25567=ORIENTED_EDGE('',*,*,#18858,.F.);
#25568=ORIENTED_EDGE('',*,*,#18862,.F.);
#25569=ORIENTED_EDGE('',*,*,#18865,.F.);
#25570=ORIENTED_EDGE('',*,*,#18868,.F.);
#25571=ORIENTED_EDGE('',*,*,#18869,.T.);
#25572=ORIENTED_EDGE('',*,*,#18870,.T.);
#25573=ORIENTED_EDGE('',*,*,#18871,.F.);
#25574=ORIENTED_EDGE('',*,*,#18872,.F.);
#25575=ORIENTED_EDGE('',*,*,#18873,.T.);
#25576=ORIENTED_EDGE('',*,*,#18874,.T.);
#25577=ORIENTED_EDGE('',*,*,#18869,.F.);
#25578=ORIENTED_EDGE('',*,*,#18875,.F.);
#25579=ORIENTED_EDGE('',*,*,#18876,.T.);
#25580=ORIENTED_EDGE('',*,*,#18877,.T.);
#25581=ORIENTED_EDGE('',*,*,#18873,.F.);
#25582=ORIENTED_EDGE('',*,*,#18878,.F.);
#25583=ORIENTED_EDGE('',*,*,#18871,.T.);
#25584=ORIENTED_EDGE('',*,*,#18879,.T.);
#25585=ORIENTED_EDGE('',*,*,#18876,.F.);
#25586=ORIENTED_EDGE('',*,*,#18879,.F.);
#25587=ORIENTED_EDGE('',*,*,#18870,.F.);
#25588=ORIENTED_EDGE('',*,*,#18874,.F.);
#25589=ORIENTED_EDGE('',*,*,#18877,.F.);
#25590=ORIENTED_EDGE('',*,*,#18880,.F.);
#25591=ORIENTED_EDGE('',*,*,#18881,.T.);
#25592=ORIENTED_EDGE('',*,*,#18882,.T.);
#25593=ORIENTED_EDGE('',*,*,#18883,.F.);
#25594=ORIENTED_EDGE('',*,*,#18884,.F.);
#25595=ORIENTED_EDGE('',*,*,#18885,.T.);
#25596=ORIENTED_EDGE('',*,*,#18886,.T.);
#25597=ORIENTED_EDGE('',*,*,#18881,.F.);
#25598=ORIENTED_EDGE('',*,*,#18887,.F.);
#25599=ORIENTED_EDGE('',*,*,#18888,.T.);
#25600=ORIENTED_EDGE('',*,*,#18889,.T.);
#25601=ORIENTED_EDGE('',*,*,#18885,.F.);
#25602=ORIENTED_EDGE('',*,*,#18890,.F.);
#25603=ORIENTED_EDGE('',*,*,#18883,.T.);
#25604=ORIENTED_EDGE('',*,*,#18891,.T.);
#25605=ORIENTED_EDGE('',*,*,#18888,.F.);
#25606=ORIENTED_EDGE('',*,*,#18891,.F.);
#25607=ORIENTED_EDGE('',*,*,#18882,.F.);
#25608=ORIENTED_EDGE('',*,*,#18886,.F.);
#25609=ORIENTED_EDGE('',*,*,#18889,.F.);
#25610=ORIENTED_EDGE('',*,*,#18892,.F.);
#25611=ORIENTED_EDGE('',*,*,#18893,.T.);
#25612=ORIENTED_EDGE('',*,*,#18894,.T.);
#25613=ORIENTED_EDGE('',*,*,#18895,.F.);
#25614=ORIENTED_EDGE('',*,*,#18896,.F.);
#25615=ORIENTED_EDGE('',*,*,#18897,.T.);
#25616=ORIENTED_EDGE('',*,*,#18898,.T.);
#25617=ORIENTED_EDGE('',*,*,#18893,.F.);
#25618=ORIENTED_EDGE('',*,*,#18899,.F.);
#25619=ORIENTED_EDGE('',*,*,#18900,.T.);
#25620=ORIENTED_EDGE('',*,*,#18901,.T.);
#25621=ORIENTED_EDGE('',*,*,#18897,.F.);
#25622=ORIENTED_EDGE('',*,*,#18902,.F.);
#25623=ORIENTED_EDGE('',*,*,#18895,.T.);
#25624=ORIENTED_EDGE('',*,*,#18903,.T.);
#25625=ORIENTED_EDGE('',*,*,#18900,.F.);
#25626=ORIENTED_EDGE('',*,*,#18903,.F.);
#25627=ORIENTED_EDGE('',*,*,#18894,.F.);
#25628=ORIENTED_EDGE('',*,*,#18898,.F.);
#25629=ORIENTED_EDGE('',*,*,#18901,.F.);
#25630=ORIENTED_EDGE('',*,*,#18904,.F.);
#25631=ORIENTED_EDGE('',*,*,#18905,.T.);
#25632=ORIENTED_EDGE('',*,*,#18906,.T.);
#25633=ORIENTED_EDGE('',*,*,#18907,.F.);
#25634=ORIENTED_EDGE('',*,*,#18908,.F.);
#25635=ORIENTED_EDGE('',*,*,#18909,.T.);
#25636=ORIENTED_EDGE('',*,*,#18910,.T.);
#25637=ORIENTED_EDGE('',*,*,#18905,.F.);
#25638=ORIENTED_EDGE('',*,*,#18911,.F.);
#25639=ORIENTED_EDGE('',*,*,#18912,.T.);
#25640=ORIENTED_EDGE('',*,*,#18913,.T.);
#25641=ORIENTED_EDGE('',*,*,#18909,.F.);
#25642=ORIENTED_EDGE('',*,*,#18914,.F.);
#25643=ORIENTED_EDGE('',*,*,#18907,.T.);
#25644=ORIENTED_EDGE('',*,*,#18915,.T.);
#25645=ORIENTED_EDGE('',*,*,#18912,.F.);
#25646=ORIENTED_EDGE('',*,*,#18915,.F.);
#25647=ORIENTED_EDGE('',*,*,#18906,.F.);
#25648=ORIENTED_EDGE('',*,*,#18910,.F.);
#25649=ORIENTED_EDGE('',*,*,#18913,.F.);
#25650=ORIENTED_EDGE('',*,*,#18916,.F.);
#25651=ORIENTED_EDGE('',*,*,#18917,.T.);
#25652=ORIENTED_EDGE('',*,*,#18918,.T.);
#25653=ORIENTED_EDGE('',*,*,#18919,.F.);
#25654=ORIENTED_EDGE('',*,*,#18920,.F.);
#25655=ORIENTED_EDGE('',*,*,#18921,.T.);
#25656=ORIENTED_EDGE('',*,*,#18922,.T.);
#25657=ORIENTED_EDGE('',*,*,#18917,.F.);
#25658=ORIENTED_EDGE('',*,*,#18923,.F.);
#25659=ORIENTED_EDGE('',*,*,#18924,.T.);
#25660=ORIENTED_EDGE('',*,*,#18925,.T.);
#25661=ORIENTED_EDGE('',*,*,#18921,.F.);
#25662=ORIENTED_EDGE('',*,*,#18926,.F.);
#25663=ORIENTED_EDGE('',*,*,#18919,.T.);
#25664=ORIENTED_EDGE('',*,*,#18927,.T.);
#25665=ORIENTED_EDGE('',*,*,#18924,.F.);
#25666=ORIENTED_EDGE('',*,*,#18927,.F.);
#25667=ORIENTED_EDGE('',*,*,#18918,.F.);
#25668=ORIENTED_EDGE('',*,*,#18922,.F.);
#25669=ORIENTED_EDGE('',*,*,#18925,.F.);
#25670=ORIENTED_EDGE('',*,*,#18928,.F.);
#25671=ORIENTED_EDGE('',*,*,#18929,.T.);
#25672=ORIENTED_EDGE('',*,*,#18930,.T.);
#25673=ORIENTED_EDGE('',*,*,#18931,.F.);
#25674=ORIENTED_EDGE('',*,*,#18932,.F.);
#25675=ORIENTED_EDGE('',*,*,#18933,.T.);
#25676=ORIENTED_EDGE('',*,*,#18934,.T.);
#25677=ORIENTED_EDGE('',*,*,#18929,.F.);
#25678=ORIENTED_EDGE('',*,*,#18935,.F.);
#25679=ORIENTED_EDGE('',*,*,#18936,.T.);
#25680=ORIENTED_EDGE('',*,*,#18937,.T.);
#25681=ORIENTED_EDGE('',*,*,#18933,.F.);
#25682=ORIENTED_EDGE('',*,*,#18938,.F.);
#25683=ORIENTED_EDGE('',*,*,#18931,.T.);
#25684=ORIENTED_EDGE('',*,*,#18939,.T.);
#25685=ORIENTED_EDGE('',*,*,#18936,.F.);
#25686=ORIENTED_EDGE('',*,*,#18939,.F.);
#25687=ORIENTED_EDGE('',*,*,#18930,.F.);
#25688=ORIENTED_EDGE('',*,*,#18934,.F.);
#25689=ORIENTED_EDGE('',*,*,#18937,.F.);
#25690=ORIENTED_EDGE('',*,*,#18940,.F.);
#25691=ORIENTED_EDGE('',*,*,#18941,.T.);
#25692=ORIENTED_EDGE('',*,*,#18942,.T.);
#25693=ORIENTED_EDGE('',*,*,#18943,.F.);
#25694=ORIENTED_EDGE('',*,*,#18944,.F.);
#25695=ORIENTED_EDGE('',*,*,#18945,.T.);
#25696=ORIENTED_EDGE('',*,*,#18946,.T.);
#25697=ORIENTED_EDGE('',*,*,#18941,.F.);
#25698=ORIENTED_EDGE('',*,*,#18947,.F.);
#25699=ORIENTED_EDGE('',*,*,#18948,.T.);
#25700=ORIENTED_EDGE('',*,*,#18949,.T.);
#25701=ORIENTED_EDGE('',*,*,#18945,.F.);
#25702=ORIENTED_EDGE('',*,*,#18950,.F.);
#25703=ORIENTED_EDGE('',*,*,#18943,.T.);
#25704=ORIENTED_EDGE('',*,*,#18951,.T.);
#25705=ORIENTED_EDGE('',*,*,#18948,.F.);
#25706=ORIENTED_EDGE('',*,*,#18951,.F.);
#25707=ORIENTED_EDGE('',*,*,#18942,.F.);
#25708=ORIENTED_EDGE('',*,*,#18946,.F.);
#25709=ORIENTED_EDGE('',*,*,#18949,.F.);
#25710=ORIENTED_EDGE('',*,*,#18952,.F.);
#25711=ORIENTED_EDGE('',*,*,#18953,.T.);
#25712=ORIENTED_EDGE('',*,*,#18954,.T.);
#25713=ORIENTED_EDGE('',*,*,#18955,.F.);
#25714=ORIENTED_EDGE('',*,*,#18956,.F.);
#25715=ORIENTED_EDGE('',*,*,#18957,.T.);
#25716=ORIENTED_EDGE('',*,*,#18958,.T.);
#25717=ORIENTED_EDGE('',*,*,#18953,.F.);
#25718=ORIENTED_EDGE('',*,*,#18959,.F.);
#25719=ORIENTED_EDGE('',*,*,#18960,.T.);
#25720=ORIENTED_EDGE('',*,*,#18961,.T.);
#25721=ORIENTED_EDGE('',*,*,#18957,.F.);
#25722=ORIENTED_EDGE('',*,*,#18962,.F.);
#25723=ORIENTED_EDGE('',*,*,#18955,.T.);
#25724=ORIENTED_EDGE('',*,*,#18963,.T.);
#25725=ORIENTED_EDGE('',*,*,#18960,.F.);
#25726=ORIENTED_EDGE('',*,*,#18963,.F.);
#25727=ORIENTED_EDGE('',*,*,#18954,.F.);
#25728=ORIENTED_EDGE('',*,*,#18958,.F.);
#25729=ORIENTED_EDGE('',*,*,#18961,.F.);
#25730=ORIENTED_EDGE('',*,*,#18964,.F.);
#25731=ORIENTED_EDGE('',*,*,#18965,.T.);
#25732=ORIENTED_EDGE('',*,*,#18966,.T.);
#25733=ORIENTED_EDGE('',*,*,#18967,.F.);
#25734=ORIENTED_EDGE('',*,*,#18968,.F.);
#25735=ORIENTED_EDGE('',*,*,#18969,.T.);
#25736=ORIENTED_EDGE('',*,*,#18970,.T.);
#25737=ORIENTED_EDGE('',*,*,#18965,.F.);
#25738=ORIENTED_EDGE('',*,*,#18971,.F.);
#25739=ORIENTED_EDGE('',*,*,#18972,.T.);
#25740=ORIENTED_EDGE('',*,*,#18973,.T.);
#25741=ORIENTED_EDGE('',*,*,#18969,.F.);
#25742=ORIENTED_EDGE('',*,*,#18974,.F.);
#25743=ORIENTED_EDGE('',*,*,#18967,.T.);
#25744=ORIENTED_EDGE('',*,*,#18975,.T.);
#25745=ORIENTED_EDGE('',*,*,#18972,.F.);
#25746=ORIENTED_EDGE('',*,*,#18975,.F.);
#25747=ORIENTED_EDGE('',*,*,#18966,.F.);
#25748=ORIENTED_EDGE('',*,*,#18970,.F.);
#25749=ORIENTED_EDGE('',*,*,#18973,.F.);
#25750=ORIENTED_EDGE('',*,*,#18976,.F.);
#25751=ORIENTED_EDGE('',*,*,#18977,.T.);
#25752=ORIENTED_EDGE('',*,*,#18978,.T.);
#25753=ORIENTED_EDGE('',*,*,#18979,.F.);
#25754=ORIENTED_EDGE('',*,*,#18980,.F.);
#25755=ORIENTED_EDGE('',*,*,#18981,.T.);
#25756=ORIENTED_EDGE('',*,*,#18982,.T.);
#25757=ORIENTED_EDGE('',*,*,#18977,.F.);
#25758=ORIENTED_EDGE('',*,*,#18983,.F.);
#25759=ORIENTED_EDGE('',*,*,#18984,.T.);
#25760=ORIENTED_EDGE('',*,*,#18985,.T.);
#25761=ORIENTED_EDGE('',*,*,#18981,.F.);
#25762=ORIENTED_EDGE('',*,*,#18986,.F.);
#25763=ORIENTED_EDGE('',*,*,#18979,.T.);
#25764=ORIENTED_EDGE('',*,*,#18987,.T.);
#25765=ORIENTED_EDGE('',*,*,#18984,.F.);
#25766=ORIENTED_EDGE('',*,*,#18987,.F.);
#25767=ORIENTED_EDGE('',*,*,#18978,.F.);
#25768=ORIENTED_EDGE('',*,*,#18982,.F.);
#25769=ORIENTED_EDGE('',*,*,#18985,.F.);
#25770=ORIENTED_EDGE('',*,*,#18988,.F.);
#25771=ORIENTED_EDGE('',*,*,#18989,.T.);
#25772=ORIENTED_EDGE('',*,*,#18990,.T.);
#25773=ORIENTED_EDGE('',*,*,#18991,.F.);
#25774=ORIENTED_EDGE('',*,*,#18992,.F.);
#25775=ORIENTED_EDGE('',*,*,#18993,.T.);
#25776=ORIENTED_EDGE('',*,*,#18994,.T.);
#25777=ORIENTED_EDGE('',*,*,#18989,.F.);
#25778=ORIENTED_EDGE('',*,*,#18995,.F.);
#25779=ORIENTED_EDGE('',*,*,#18996,.T.);
#25780=ORIENTED_EDGE('',*,*,#18997,.T.);
#25781=ORIENTED_EDGE('',*,*,#18993,.F.);
#25782=ORIENTED_EDGE('',*,*,#18998,.F.);
#25783=ORIENTED_EDGE('',*,*,#18991,.T.);
#25784=ORIENTED_EDGE('',*,*,#18999,.T.);
#25785=ORIENTED_EDGE('',*,*,#18996,.F.);
#25786=ORIENTED_EDGE('',*,*,#18999,.F.);
#25787=ORIENTED_EDGE('',*,*,#18990,.F.);
#25788=ORIENTED_EDGE('',*,*,#18994,.F.);
#25789=ORIENTED_EDGE('',*,*,#18997,.F.);
#25790=ORIENTED_EDGE('',*,*,#19000,.F.);
#25791=ORIENTED_EDGE('',*,*,#19001,.T.);
#25792=ORIENTED_EDGE('',*,*,#19002,.T.);
#25793=ORIENTED_EDGE('',*,*,#19003,.F.);
#25794=ORIENTED_EDGE('',*,*,#19004,.F.);
#25795=ORIENTED_EDGE('',*,*,#19005,.T.);
#25796=ORIENTED_EDGE('',*,*,#19006,.T.);
#25797=ORIENTED_EDGE('',*,*,#19001,.F.);
#25798=ORIENTED_EDGE('',*,*,#19007,.F.);
#25799=ORIENTED_EDGE('',*,*,#19008,.T.);
#25800=ORIENTED_EDGE('',*,*,#19009,.T.);
#25801=ORIENTED_EDGE('',*,*,#19005,.F.);
#25802=ORIENTED_EDGE('',*,*,#19010,.F.);
#25803=ORIENTED_EDGE('',*,*,#19003,.T.);
#25804=ORIENTED_EDGE('',*,*,#19011,.T.);
#25805=ORIENTED_EDGE('',*,*,#19008,.F.);
#25806=ORIENTED_EDGE('',*,*,#19011,.F.);
#25807=ORIENTED_EDGE('',*,*,#19002,.F.);
#25808=ORIENTED_EDGE('',*,*,#19006,.F.);
#25809=ORIENTED_EDGE('',*,*,#19009,.F.);
#25810=ORIENTED_EDGE('',*,*,#19012,.F.);
#25811=ORIENTED_EDGE('',*,*,#19013,.T.);
#25812=ORIENTED_EDGE('',*,*,#19014,.T.);
#25813=ORIENTED_EDGE('',*,*,#19015,.F.);
#25814=ORIENTED_EDGE('',*,*,#19016,.F.);
#25815=ORIENTED_EDGE('',*,*,#19017,.T.);
#25816=ORIENTED_EDGE('',*,*,#19018,.T.);
#25817=ORIENTED_EDGE('',*,*,#19013,.F.);
#25818=ORIENTED_EDGE('',*,*,#19019,.F.);
#25819=ORIENTED_EDGE('',*,*,#19020,.T.);
#25820=ORIENTED_EDGE('',*,*,#19021,.T.);
#25821=ORIENTED_EDGE('',*,*,#19017,.F.);
#25822=ORIENTED_EDGE('',*,*,#19022,.F.);
#25823=ORIENTED_EDGE('',*,*,#19015,.T.);
#25824=ORIENTED_EDGE('',*,*,#19023,.T.);
#25825=ORIENTED_EDGE('',*,*,#19020,.F.);
#25826=ORIENTED_EDGE('',*,*,#19023,.F.);
#25827=ORIENTED_EDGE('',*,*,#19014,.F.);
#25828=ORIENTED_EDGE('',*,*,#19018,.F.);
#25829=ORIENTED_EDGE('',*,*,#19021,.F.);
#25830=ORIENTED_EDGE('',*,*,#19024,.F.);
#25831=ORIENTED_EDGE('',*,*,#19025,.T.);
#25832=ORIENTED_EDGE('',*,*,#19026,.T.);
#25833=ORIENTED_EDGE('',*,*,#19027,.F.);
#25834=ORIENTED_EDGE('',*,*,#19028,.F.);
#25835=ORIENTED_EDGE('',*,*,#19029,.T.);
#25836=ORIENTED_EDGE('',*,*,#19030,.T.);
#25837=ORIENTED_EDGE('',*,*,#19025,.F.);
#25838=ORIENTED_EDGE('',*,*,#19031,.F.);
#25839=ORIENTED_EDGE('',*,*,#19032,.T.);
#25840=ORIENTED_EDGE('',*,*,#19033,.T.);
#25841=ORIENTED_EDGE('',*,*,#19029,.F.);
#25842=ORIENTED_EDGE('',*,*,#19034,.F.);
#25843=ORIENTED_EDGE('',*,*,#19027,.T.);
#25844=ORIENTED_EDGE('',*,*,#19035,.T.);
#25845=ORIENTED_EDGE('',*,*,#19032,.F.);
#25846=ORIENTED_EDGE('',*,*,#19035,.F.);
#25847=ORIENTED_EDGE('',*,*,#19026,.F.);
#25848=ORIENTED_EDGE('',*,*,#19030,.F.);
#25849=ORIENTED_EDGE('',*,*,#19033,.F.);
#25850=ORIENTED_EDGE('',*,*,#19036,.F.);
#25851=ORIENTED_EDGE('',*,*,#19037,.T.);
#25852=ORIENTED_EDGE('',*,*,#19038,.T.);
#25853=ORIENTED_EDGE('',*,*,#19039,.F.);
#25854=ORIENTED_EDGE('',*,*,#19040,.F.);
#25855=ORIENTED_EDGE('',*,*,#19041,.T.);
#25856=ORIENTED_EDGE('',*,*,#19042,.T.);
#25857=ORIENTED_EDGE('',*,*,#19037,.F.);
#25858=ORIENTED_EDGE('',*,*,#19043,.F.);
#25859=ORIENTED_EDGE('',*,*,#19044,.T.);
#25860=ORIENTED_EDGE('',*,*,#19045,.T.);
#25861=ORIENTED_EDGE('',*,*,#19041,.F.);
#25862=ORIENTED_EDGE('',*,*,#19046,.F.);
#25863=ORIENTED_EDGE('',*,*,#19039,.T.);
#25864=ORIENTED_EDGE('',*,*,#19047,.T.);
#25865=ORIENTED_EDGE('',*,*,#19044,.F.);
#25866=ORIENTED_EDGE('',*,*,#19047,.F.);
#25867=ORIENTED_EDGE('',*,*,#19038,.F.);
#25868=ORIENTED_EDGE('',*,*,#19042,.F.);
#25869=ORIENTED_EDGE('',*,*,#19045,.F.);
#25870=ORIENTED_EDGE('',*,*,#19048,.F.);
#25871=ORIENTED_EDGE('',*,*,#19049,.T.);
#25872=ORIENTED_EDGE('',*,*,#19050,.T.);
#25873=ORIENTED_EDGE('',*,*,#19051,.F.);
#25874=ORIENTED_EDGE('',*,*,#19052,.F.);
#25875=ORIENTED_EDGE('',*,*,#19053,.T.);
#25876=ORIENTED_EDGE('',*,*,#19054,.T.);
#25877=ORIENTED_EDGE('',*,*,#19049,.F.);
#25878=ORIENTED_EDGE('',*,*,#19055,.F.);
#25879=ORIENTED_EDGE('',*,*,#19056,.T.);
#25880=ORIENTED_EDGE('',*,*,#19057,.T.);
#25881=ORIENTED_EDGE('',*,*,#19053,.F.);
#25882=ORIENTED_EDGE('',*,*,#19058,.F.);
#25883=ORIENTED_EDGE('',*,*,#19051,.T.);
#25884=ORIENTED_EDGE('',*,*,#19059,.T.);
#25885=ORIENTED_EDGE('',*,*,#19056,.F.);
#25886=ORIENTED_EDGE('',*,*,#19059,.F.);
#25887=ORIENTED_EDGE('',*,*,#19050,.F.);
#25888=ORIENTED_EDGE('',*,*,#19054,.F.);
#25889=ORIENTED_EDGE('',*,*,#19057,.F.);
#25890=ORIENTED_EDGE('',*,*,#19060,.F.);
#25891=ORIENTED_EDGE('',*,*,#19061,.T.);
#25892=ORIENTED_EDGE('',*,*,#19062,.T.);
#25893=ORIENTED_EDGE('',*,*,#19063,.F.);
#25894=ORIENTED_EDGE('',*,*,#19064,.F.);
#25895=ORIENTED_EDGE('',*,*,#19065,.T.);
#25896=ORIENTED_EDGE('',*,*,#19066,.T.);
#25897=ORIENTED_EDGE('',*,*,#19061,.F.);
#25898=ORIENTED_EDGE('',*,*,#19067,.F.);
#25899=ORIENTED_EDGE('',*,*,#19068,.T.);
#25900=ORIENTED_EDGE('',*,*,#19069,.T.);
#25901=ORIENTED_EDGE('',*,*,#19065,.F.);
#25902=ORIENTED_EDGE('',*,*,#19070,.F.);
#25903=ORIENTED_EDGE('',*,*,#19063,.T.);
#25904=ORIENTED_EDGE('',*,*,#19071,.T.);
#25905=ORIENTED_EDGE('',*,*,#19068,.F.);
#25906=ORIENTED_EDGE('',*,*,#19071,.F.);
#25907=ORIENTED_EDGE('',*,*,#19062,.F.);
#25908=ORIENTED_EDGE('',*,*,#19066,.F.);
#25909=ORIENTED_EDGE('',*,*,#19069,.F.);
#25910=ORIENTED_EDGE('',*,*,#19072,.F.);
#25911=ORIENTED_EDGE('',*,*,#19073,.T.);
#25912=ORIENTED_EDGE('',*,*,#19074,.T.);
#25913=ORIENTED_EDGE('',*,*,#19075,.F.);
#25914=ORIENTED_EDGE('',*,*,#19076,.F.);
#25915=ORIENTED_EDGE('',*,*,#19077,.T.);
#25916=ORIENTED_EDGE('',*,*,#19078,.T.);
#25917=ORIENTED_EDGE('',*,*,#19073,.F.);
#25918=ORIENTED_EDGE('',*,*,#19079,.F.);
#25919=ORIENTED_EDGE('',*,*,#19080,.T.);
#25920=ORIENTED_EDGE('',*,*,#19081,.T.);
#25921=ORIENTED_EDGE('',*,*,#19077,.F.);
#25922=ORIENTED_EDGE('',*,*,#19082,.F.);
#25923=ORIENTED_EDGE('',*,*,#19075,.T.);
#25924=ORIENTED_EDGE('',*,*,#19083,.T.);
#25925=ORIENTED_EDGE('',*,*,#19080,.F.);
#25926=ORIENTED_EDGE('',*,*,#19083,.F.);
#25927=ORIENTED_EDGE('',*,*,#19074,.F.);
#25928=ORIENTED_EDGE('',*,*,#19078,.F.);
#25929=ORIENTED_EDGE('',*,*,#19081,.F.);
#25930=ORIENTED_EDGE('',*,*,#19084,.F.);
#25931=ORIENTED_EDGE('',*,*,#19085,.T.);
#25932=ORIENTED_EDGE('',*,*,#19086,.T.);
#25933=ORIENTED_EDGE('',*,*,#19087,.F.);
#25934=ORIENTED_EDGE('',*,*,#19088,.F.);
#25935=ORIENTED_EDGE('',*,*,#19089,.T.);
#25936=ORIENTED_EDGE('',*,*,#19090,.T.);
#25937=ORIENTED_EDGE('',*,*,#19085,.F.);
#25938=ORIENTED_EDGE('',*,*,#19091,.F.);
#25939=ORIENTED_EDGE('',*,*,#19092,.T.);
#25940=ORIENTED_EDGE('',*,*,#19093,.T.);
#25941=ORIENTED_EDGE('',*,*,#19089,.F.);
#25942=ORIENTED_EDGE('',*,*,#19094,.F.);
#25943=ORIENTED_EDGE('',*,*,#19087,.T.);
#25944=ORIENTED_EDGE('',*,*,#19095,.T.);
#25945=ORIENTED_EDGE('',*,*,#19092,.F.);
#25946=ORIENTED_EDGE('',*,*,#19095,.F.);
#25947=ORIENTED_EDGE('',*,*,#19086,.F.);
#25948=ORIENTED_EDGE('',*,*,#19090,.F.);
#25949=ORIENTED_EDGE('',*,*,#19093,.F.);
#25950=ORIENTED_EDGE('',*,*,#19096,.F.);
#25951=ORIENTED_EDGE('',*,*,#19097,.T.);
#25952=ORIENTED_EDGE('',*,*,#19098,.T.);
#25953=ORIENTED_EDGE('',*,*,#19099,.F.);
#25954=ORIENTED_EDGE('',*,*,#19100,.F.);
#25955=ORIENTED_EDGE('',*,*,#19101,.T.);
#25956=ORIENTED_EDGE('',*,*,#19102,.T.);
#25957=ORIENTED_EDGE('',*,*,#19097,.F.);
#25958=ORIENTED_EDGE('',*,*,#19103,.F.);
#25959=ORIENTED_EDGE('',*,*,#19104,.T.);
#25960=ORIENTED_EDGE('',*,*,#19105,.T.);
#25961=ORIENTED_EDGE('',*,*,#19101,.F.);
#25962=ORIENTED_EDGE('',*,*,#19106,.F.);
#25963=ORIENTED_EDGE('',*,*,#19099,.T.);
#25964=ORIENTED_EDGE('',*,*,#19107,.T.);
#25965=ORIENTED_EDGE('',*,*,#19104,.F.);
#25966=ORIENTED_EDGE('',*,*,#19107,.F.);
#25967=ORIENTED_EDGE('',*,*,#19098,.F.);
#25968=ORIENTED_EDGE('',*,*,#19102,.F.);
#25969=ORIENTED_EDGE('',*,*,#19105,.F.);
#25970=ORIENTED_EDGE('',*,*,#19108,.F.);
#25971=ORIENTED_EDGE('',*,*,#19109,.T.);
#25972=ORIENTED_EDGE('',*,*,#19110,.T.);
#25973=ORIENTED_EDGE('',*,*,#19111,.F.);
#25974=ORIENTED_EDGE('',*,*,#19112,.F.);
#25975=ORIENTED_EDGE('',*,*,#19113,.T.);
#25976=ORIENTED_EDGE('',*,*,#19114,.T.);
#25977=ORIENTED_EDGE('',*,*,#19109,.F.);
#25978=ORIENTED_EDGE('',*,*,#19115,.F.);
#25979=ORIENTED_EDGE('',*,*,#19116,.T.);
#25980=ORIENTED_EDGE('',*,*,#19117,.T.);
#25981=ORIENTED_EDGE('',*,*,#19113,.F.);
#25982=ORIENTED_EDGE('',*,*,#19118,.F.);
#25983=ORIENTED_EDGE('',*,*,#19111,.T.);
#25984=ORIENTED_EDGE('',*,*,#19119,.T.);
#25985=ORIENTED_EDGE('',*,*,#19116,.F.);
#25986=ORIENTED_EDGE('',*,*,#19119,.F.);
#25987=ORIENTED_EDGE('',*,*,#19110,.F.);
#25988=ORIENTED_EDGE('',*,*,#19114,.F.);
#25989=ORIENTED_EDGE('',*,*,#19117,.F.);
#25990=ORIENTED_EDGE('',*,*,#19120,.F.);
#25991=ORIENTED_EDGE('',*,*,#19121,.T.);
#25992=ORIENTED_EDGE('',*,*,#19122,.T.);
#25993=ORIENTED_EDGE('',*,*,#19123,.F.);
#25994=ORIENTED_EDGE('',*,*,#19124,.F.);
#25995=ORIENTED_EDGE('',*,*,#19125,.T.);
#25996=ORIENTED_EDGE('',*,*,#19126,.T.);
#25997=ORIENTED_EDGE('',*,*,#19121,.F.);
#25998=ORIENTED_EDGE('',*,*,#19127,.F.);
#25999=ORIENTED_EDGE('',*,*,#19128,.T.);
#26000=ORIENTED_EDGE('',*,*,#19129,.T.);
#26001=ORIENTED_EDGE('',*,*,#19125,.F.);
#26002=ORIENTED_EDGE('',*,*,#19130,.F.);
#26003=ORIENTED_EDGE('',*,*,#19123,.T.);
#26004=ORIENTED_EDGE('',*,*,#19131,.T.);
#26005=ORIENTED_EDGE('',*,*,#19128,.F.);
#26006=ORIENTED_EDGE('',*,*,#19131,.F.);
#26007=ORIENTED_EDGE('',*,*,#19122,.F.);
#26008=ORIENTED_EDGE('',*,*,#19126,.F.);
#26009=ORIENTED_EDGE('',*,*,#19129,.F.);
#26010=ORIENTED_EDGE('',*,*,#19132,.F.);
#26011=ORIENTED_EDGE('',*,*,#19133,.T.);
#26012=ORIENTED_EDGE('',*,*,#19134,.T.);
#26013=ORIENTED_EDGE('',*,*,#19135,.F.);
#26014=ORIENTED_EDGE('',*,*,#19136,.F.);
#26015=ORIENTED_EDGE('',*,*,#19137,.T.);
#26016=ORIENTED_EDGE('',*,*,#19138,.T.);
#26017=ORIENTED_EDGE('',*,*,#19133,.F.);
#26018=ORIENTED_EDGE('',*,*,#19139,.F.);
#26019=ORIENTED_EDGE('',*,*,#19140,.T.);
#26020=ORIENTED_EDGE('',*,*,#19141,.T.);
#26021=ORIENTED_EDGE('',*,*,#19137,.F.);
#26022=ORIENTED_EDGE('',*,*,#19142,.F.);
#26023=ORIENTED_EDGE('',*,*,#19135,.T.);
#26024=ORIENTED_EDGE('',*,*,#19143,.T.);
#26025=ORIENTED_EDGE('',*,*,#19140,.F.);
#26026=ORIENTED_EDGE('',*,*,#19143,.F.);
#26027=ORIENTED_EDGE('',*,*,#19134,.F.);
#26028=ORIENTED_EDGE('',*,*,#19138,.F.);
#26029=ORIENTED_EDGE('',*,*,#19141,.F.);
#26030=ORIENTED_EDGE('',*,*,#19144,.F.);
#26031=ORIENTED_EDGE('',*,*,#19145,.T.);
#26032=ORIENTED_EDGE('',*,*,#19146,.T.);
#26033=ORIENTED_EDGE('',*,*,#19147,.F.);
#26034=ORIENTED_EDGE('',*,*,#19148,.F.);
#26035=ORIENTED_EDGE('',*,*,#19149,.T.);
#26036=ORIENTED_EDGE('',*,*,#19150,.T.);
#26037=ORIENTED_EDGE('',*,*,#19145,.F.);
#26038=ORIENTED_EDGE('',*,*,#19151,.F.);
#26039=ORIENTED_EDGE('',*,*,#19152,.T.);
#26040=ORIENTED_EDGE('',*,*,#19153,.T.);
#26041=ORIENTED_EDGE('',*,*,#19149,.F.);
#26042=ORIENTED_EDGE('',*,*,#19154,.F.);
#26043=ORIENTED_EDGE('',*,*,#19147,.T.);
#26044=ORIENTED_EDGE('',*,*,#19155,.T.);
#26045=ORIENTED_EDGE('',*,*,#19152,.F.);
#26046=ORIENTED_EDGE('',*,*,#19155,.F.);
#26047=ORIENTED_EDGE('',*,*,#19146,.F.);
#26048=ORIENTED_EDGE('',*,*,#19150,.F.);
#26049=ORIENTED_EDGE('',*,*,#19153,.F.);
#26050=ORIENTED_EDGE('',*,*,#19156,.F.);
#26051=ORIENTED_EDGE('',*,*,#19157,.T.);
#26052=ORIENTED_EDGE('',*,*,#19158,.T.);
#26053=ORIENTED_EDGE('',*,*,#19159,.F.);
#26054=ORIENTED_EDGE('',*,*,#19160,.F.);
#26055=ORIENTED_EDGE('',*,*,#19161,.T.);
#26056=ORIENTED_EDGE('',*,*,#19162,.T.);
#26057=ORIENTED_EDGE('',*,*,#19157,.F.);
#26058=ORIENTED_EDGE('',*,*,#19163,.F.);
#26059=ORIENTED_EDGE('',*,*,#19164,.T.);
#26060=ORIENTED_EDGE('',*,*,#19165,.T.);
#26061=ORIENTED_EDGE('',*,*,#19161,.F.);
#26062=ORIENTED_EDGE('',*,*,#19166,.F.);
#26063=ORIENTED_EDGE('',*,*,#19159,.T.);
#26064=ORIENTED_EDGE('',*,*,#19167,.T.);
#26065=ORIENTED_EDGE('',*,*,#19164,.F.);
#26066=ORIENTED_EDGE('',*,*,#19167,.F.);
#26067=ORIENTED_EDGE('',*,*,#19158,.F.);
#26068=ORIENTED_EDGE('',*,*,#19162,.F.);
#26069=ORIENTED_EDGE('',*,*,#19165,.F.);
#26070=ORIENTED_EDGE('',*,*,#19168,.F.);
#26071=ORIENTED_EDGE('',*,*,#19169,.T.);
#26072=ORIENTED_EDGE('',*,*,#19170,.T.);
#26073=ORIENTED_EDGE('',*,*,#19171,.F.);
#26074=ORIENTED_EDGE('',*,*,#19172,.F.);
#26075=ORIENTED_EDGE('',*,*,#19173,.T.);
#26076=ORIENTED_EDGE('',*,*,#19174,.T.);
#26077=ORIENTED_EDGE('',*,*,#19169,.F.);
#26078=ORIENTED_EDGE('',*,*,#19175,.F.);
#26079=ORIENTED_EDGE('',*,*,#19176,.T.);
#26080=ORIENTED_EDGE('',*,*,#19177,.T.);
#26081=ORIENTED_EDGE('',*,*,#19173,.F.);
#26082=ORIENTED_EDGE('',*,*,#19178,.F.);
#26083=ORIENTED_EDGE('',*,*,#19171,.T.);
#26084=ORIENTED_EDGE('',*,*,#19179,.T.);
#26085=ORIENTED_EDGE('',*,*,#19176,.F.);
#26086=ORIENTED_EDGE('',*,*,#19179,.F.);
#26087=ORIENTED_EDGE('',*,*,#19170,.F.);
#26088=ORIENTED_EDGE('',*,*,#19174,.F.);
#26089=ORIENTED_EDGE('',*,*,#19177,.F.);
#26090=ORIENTED_EDGE('',*,*,#19180,.F.);
#26091=ORIENTED_EDGE('',*,*,#19181,.T.);
#26092=ORIENTED_EDGE('',*,*,#19182,.T.);
#26093=ORIENTED_EDGE('',*,*,#19183,.F.);
#26094=ORIENTED_EDGE('',*,*,#19184,.F.);
#26095=ORIENTED_EDGE('',*,*,#19185,.T.);
#26096=ORIENTED_EDGE('',*,*,#19186,.T.);
#26097=ORIENTED_EDGE('',*,*,#19181,.F.);
#26098=ORIENTED_EDGE('',*,*,#19187,.F.);
#26099=ORIENTED_EDGE('',*,*,#19188,.T.);
#26100=ORIENTED_EDGE('',*,*,#19189,.T.);
#26101=ORIENTED_EDGE('',*,*,#19185,.F.);
#26102=ORIENTED_EDGE('',*,*,#19190,.F.);
#26103=ORIENTED_EDGE('',*,*,#19183,.T.);
#26104=ORIENTED_EDGE('',*,*,#19191,.T.);
#26105=ORIENTED_EDGE('',*,*,#19188,.F.);
#26106=ORIENTED_EDGE('',*,*,#19191,.F.);
#26107=ORIENTED_EDGE('',*,*,#19182,.F.);
#26108=ORIENTED_EDGE('',*,*,#19186,.F.);
#26109=ORIENTED_EDGE('',*,*,#19189,.F.);
#26110=ORIENTED_EDGE('',*,*,#19192,.F.);
#26111=ORIENTED_EDGE('',*,*,#19193,.T.);
#26112=ORIENTED_EDGE('',*,*,#19194,.T.);
#26113=ORIENTED_EDGE('',*,*,#19195,.F.);
#26114=ORIENTED_EDGE('',*,*,#19196,.F.);
#26115=ORIENTED_EDGE('',*,*,#19197,.T.);
#26116=ORIENTED_EDGE('',*,*,#19198,.T.);
#26117=ORIENTED_EDGE('',*,*,#19193,.F.);
#26118=ORIENTED_EDGE('',*,*,#19199,.F.);
#26119=ORIENTED_EDGE('',*,*,#19200,.T.);
#26120=ORIENTED_EDGE('',*,*,#19201,.T.);
#26121=ORIENTED_EDGE('',*,*,#19197,.F.);
#26122=ORIENTED_EDGE('',*,*,#19202,.F.);
#26123=ORIENTED_EDGE('',*,*,#19195,.T.);
#26124=ORIENTED_EDGE('',*,*,#19203,.T.);
#26125=ORIENTED_EDGE('',*,*,#19200,.F.);
#26126=ORIENTED_EDGE('',*,*,#19203,.F.);
#26127=ORIENTED_EDGE('',*,*,#19194,.F.);
#26128=ORIENTED_EDGE('',*,*,#19198,.F.);
#26129=ORIENTED_EDGE('',*,*,#19201,.F.);
#26130=ORIENTED_EDGE('',*,*,#19204,.F.);
#26131=ORIENTED_EDGE('',*,*,#19205,.T.);
#26132=ORIENTED_EDGE('',*,*,#19206,.T.);
#26133=ORIENTED_EDGE('',*,*,#19207,.F.);
#26134=ORIENTED_EDGE('',*,*,#19208,.F.);
#26135=ORIENTED_EDGE('',*,*,#19209,.T.);
#26136=ORIENTED_EDGE('',*,*,#19210,.T.);
#26137=ORIENTED_EDGE('',*,*,#19205,.F.);
#26138=ORIENTED_EDGE('',*,*,#19211,.F.);
#26139=ORIENTED_EDGE('',*,*,#19212,.T.);
#26140=ORIENTED_EDGE('',*,*,#19213,.T.);
#26141=ORIENTED_EDGE('',*,*,#19209,.F.);
#26142=ORIENTED_EDGE('',*,*,#19214,.F.);
#26143=ORIENTED_EDGE('',*,*,#19207,.T.);
#26144=ORIENTED_EDGE('',*,*,#19215,.T.);
#26145=ORIENTED_EDGE('',*,*,#19212,.F.);
#26146=ORIENTED_EDGE('',*,*,#19215,.F.);
#26147=ORIENTED_EDGE('',*,*,#19206,.F.);
#26148=ORIENTED_EDGE('',*,*,#19210,.F.);
#26149=ORIENTED_EDGE('',*,*,#19213,.F.);
#26150=ORIENTED_EDGE('',*,*,#19216,.F.);
#26151=ORIENTED_EDGE('',*,*,#19217,.T.);
#26152=ORIENTED_EDGE('',*,*,#19218,.T.);
#26153=ORIENTED_EDGE('',*,*,#19219,.F.);
#26154=ORIENTED_EDGE('',*,*,#19220,.F.);
#26155=ORIENTED_EDGE('',*,*,#19221,.T.);
#26156=ORIENTED_EDGE('',*,*,#19222,.T.);
#26157=ORIENTED_EDGE('',*,*,#19217,.F.);
#26158=ORIENTED_EDGE('',*,*,#19223,.F.);
#26159=ORIENTED_EDGE('',*,*,#19224,.T.);
#26160=ORIENTED_EDGE('',*,*,#19225,.T.);
#26161=ORIENTED_EDGE('',*,*,#19221,.F.);
#26162=ORIENTED_EDGE('',*,*,#19226,.F.);
#26163=ORIENTED_EDGE('',*,*,#19219,.T.);
#26164=ORIENTED_EDGE('',*,*,#19227,.T.);
#26165=ORIENTED_EDGE('',*,*,#19224,.F.);
#26166=ORIENTED_EDGE('',*,*,#19227,.F.);
#26167=ORIENTED_EDGE('',*,*,#19218,.F.);
#26168=ORIENTED_EDGE('',*,*,#19222,.F.);
#26169=ORIENTED_EDGE('',*,*,#19225,.F.);
#26170=ORIENTED_EDGE('',*,*,#19228,.F.);
#26171=ORIENTED_EDGE('',*,*,#19229,.T.);
#26172=ORIENTED_EDGE('',*,*,#19230,.T.);
#26173=ORIENTED_EDGE('',*,*,#19231,.F.);
#26174=ORIENTED_EDGE('',*,*,#19232,.F.);
#26175=ORIENTED_EDGE('',*,*,#19233,.T.);
#26176=ORIENTED_EDGE('',*,*,#19234,.T.);
#26177=ORIENTED_EDGE('',*,*,#19229,.F.);
#26178=ORIENTED_EDGE('',*,*,#19235,.F.);
#26179=ORIENTED_EDGE('',*,*,#19236,.T.);
#26180=ORIENTED_EDGE('',*,*,#19237,.T.);
#26181=ORIENTED_EDGE('',*,*,#19233,.F.);
#26182=ORIENTED_EDGE('',*,*,#19238,.F.);
#26183=ORIENTED_EDGE('',*,*,#19231,.T.);
#26184=ORIENTED_EDGE('',*,*,#19239,.T.);
#26185=ORIENTED_EDGE('',*,*,#19236,.F.);
#26186=ORIENTED_EDGE('',*,*,#19239,.F.);
#26187=ORIENTED_EDGE('',*,*,#19230,.F.);
#26188=ORIENTED_EDGE('',*,*,#19234,.F.);
#26189=ORIENTED_EDGE('',*,*,#19237,.F.);
#26190=ORIENTED_EDGE('',*,*,#19240,.F.);
#26191=ORIENTED_EDGE('',*,*,#19241,.T.);
#26192=ORIENTED_EDGE('',*,*,#19242,.T.);
#26193=ORIENTED_EDGE('',*,*,#19243,.F.);
#26194=ORIENTED_EDGE('',*,*,#19244,.F.);
#26195=ORIENTED_EDGE('',*,*,#19245,.T.);
#26196=ORIENTED_EDGE('',*,*,#19246,.T.);
#26197=ORIENTED_EDGE('',*,*,#19241,.F.);
#26198=ORIENTED_EDGE('',*,*,#19247,.F.);
#26199=ORIENTED_EDGE('',*,*,#19248,.T.);
#26200=ORIENTED_EDGE('',*,*,#19249,.T.);
#26201=ORIENTED_EDGE('',*,*,#19245,.F.);
#26202=ORIENTED_EDGE('',*,*,#19250,.F.);
#26203=ORIENTED_EDGE('',*,*,#19243,.T.);
#26204=ORIENTED_EDGE('',*,*,#19251,.T.);
#26205=ORIENTED_EDGE('',*,*,#19248,.F.);
#26206=ORIENTED_EDGE('',*,*,#19251,.F.);
#26207=ORIENTED_EDGE('',*,*,#19242,.F.);
#26208=ORIENTED_EDGE('',*,*,#19246,.F.);
#26209=ORIENTED_EDGE('',*,*,#19249,.F.);
#26210=ORIENTED_EDGE('',*,*,#19252,.F.);
#26211=ORIENTED_EDGE('',*,*,#19253,.T.);
#26212=ORIENTED_EDGE('',*,*,#19254,.F.);
#26213=ORIENTED_EDGE('',*,*,#19253,.F.);
#26214=ORIENTED_EDGE('',*,*,#19255,.F.);
#26215=ORIENTED_EDGE('',*,*,#19256,.T.);
#26216=ORIENTED_EDGE('',*,*,#19257,.F.);
#26217=ORIENTED_EDGE('',*,*,#19256,.F.);
#26218=ORIENTED_EDGE('',*,*,#19258,.T.);
#26219=ORIENTED_EDGE('',*,*,#19259,.T.);
#26220=ORIENTED_EDGE('',*,*,#19260,.F.);
#26221=ORIENTED_EDGE('',*,*,#19261,.F.);
#26222=ORIENTED_EDGE('',*,*,#19262,.T.);
#26223=ORIENTED_EDGE('',*,*,#19261,.T.);
#26224=ORIENTED_EDGE('',*,*,#19263,.F.);
#26225=ORIENTED_EDGE('',*,*,#19264,.F.);
#26226=ORIENTED_EDGE('',*,*,#19265,.T.);
#26227=ORIENTED_EDGE('',*,*,#19264,.T.);
#26228=ORIENTED_EDGE('',*,*,#19266,.F.);
#26229=ORIENTED_EDGE('',*,*,#19267,.F.);
#26230=ORIENTED_EDGE('',*,*,#19268,.T.);
#26231=ORIENTED_EDGE('',*,*,#19267,.T.);
#26232=ORIENTED_EDGE('',*,*,#19269,.F.);
#26233=ORIENTED_EDGE('',*,*,#19270,.F.);
#26234=ORIENTED_EDGE('',*,*,#19271,.T.);
#26235=ORIENTED_EDGE('',*,*,#19270,.T.);
#26236=ORIENTED_EDGE('',*,*,#19272,.F.);
#26237=ORIENTED_EDGE('',*,*,#19273,.F.);
#26238=ORIENTED_EDGE('',*,*,#19274,.T.);
#26239=ORIENTED_EDGE('',*,*,#19273,.T.);
#26240=ORIENTED_EDGE('',*,*,#19275,.F.);
#26241=ORIENTED_EDGE('',*,*,#19276,.F.);
#26242=ORIENTED_EDGE('',*,*,#19277,.T.);
#26243=ORIENTED_EDGE('',*,*,#19276,.T.);
#26244=ORIENTED_EDGE('',*,*,#19278,.F.);
#26245=ORIENTED_EDGE('',*,*,#19279,.F.);
#26246=ORIENTED_EDGE('',*,*,#19280,.T.);
#26247=ORIENTED_EDGE('',*,*,#19279,.T.);
#26248=ORIENTED_EDGE('',*,*,#19281,.F.);
#26249=ORIENTED_EDGE('',*,*,#19259,.F.);
#26250=ORIENTED_EDGE('',*,*,#19281,.T.);
#26251=ORIENTED_EDGE('',*,*,#19278,.T.);
#26252=ORIENTED_EDGE('',*,*,#19275,.T.);
#26253=ORIENTED_EDGE('',*,*,#19272,.T.);
#26254=ORIENTED_EDGE('',*,*,#19269,.T.);
#26255=ORIENTED_EDGE('',*,*,#19266,.T.);
#26256=ORIENTED_EDGE('',*,*,#19263,.T.);
#26257=ORIENTED_EDGE('',*,*,#19260,.T.);
#26258=ORIENTED_EDGE('',*,*,#17368,.T.);
#26259=ORIENTED_EDGE('',*,*,#17402,.T.);
#26260=ORIENTED_EDGE('',*,*,#17399,.T.);
#26261=ORIENTED_EDGE('',*,*,#17396,.T.);
#26262=ORIENTED_EDGE('',*,*,#17393,.T.);
#26263=ORIENTED_EDGE('',*,*,#17390,.T.);
#26264=ORIENTED_EDGE('',*,*,#17387,.T.);
#26265=ORIENTED_EDGE('',*,*,#17384,.T.);
#26266=ORIENTED_EDGE('',*,*,#17381,.T.);
#26267=ORIENTED_EDGE('',*,*,#17378,.T.);
#26268=ORIENTED_EDGE('',*,*,#17375,.T.);
#26269=ORIENTED_EDGE('',*,*,#17372,.T.);
#26270=ORIENTED_EDGE('',*,*,#17404,.T.);
#26271=ORIENTED_EDGE('',*,*,#17492,.T.);
#26272=ORIENTED_EDGE('',*,*,#17489,.T.);
#26273=ORIENTED_EDGE('',*,*,#17486,.T.);
#26274=ORIENTED_EDGE('',*,*,#17483,.T.);
#26275=ORIENTED_EDGE('',*,*,#17480,.T.);
#26276=ORIENTED_EDGE('',*,*,#17477,.T.);
#26277=ORIENTED_EDGE('',*,*,#17474,.T.);
#26278=ORIENTED_EDGE('',*,*,#17471,.T.);
#26279=ORIENTED_EDGE('',*,*,#17468,.T.);
#26280=ORIENTED_EDGE('',*,*,#17465,.T.);
#26281=ORIENTED_EDGE('',*,*,#17462,.T.);
#26282=ORIENTED_EDGE('',*,*,#17459,.T.);
#26283=ORIENTED_EDGE('',*,*,#17456,.T.);
#26284=ORIENTED_EDGE('',*,*,#17453,.T.);
#26285=ORIENTED_EDGE('',*,*,#17450,.T.);
#26286=ORIENTED_EDGE('',*,*,#17447,.T.);
#26287=ORIENTED_EDGE('',*,*,#17444,.T.);
#26288=ORIENTED_EDGE('',*,*,#17441,.T.);
#26289=ORIENTED_EDGE('',*,*,#17438,.T.);
#26290=ORIENTED_EDGE('',*,*,#17435,.T.);
#26291=ORIENTED_EDGE('',*,*,#17432,.T.);
#26292=ORIENTED_EDGE('',*,*,#17429,.T.);
#26293=ORIENTED_EDGE('',*,*,#17426,.T.);
#26294=ORIENTED_EDGE('',*,*,#17423,.T.);
#26295=ORIENTED_EDGE('',*,*,#17420,.T.);
#26296=ORIENTED_EDGE('',*,*,#17417,.T.);
#26297=ORIENTED_EDGE('',*,*,#17414,.T.);
#26298=ORIENTED_EDGE('',*,*,#17411,.T.);
#26299=ORIENTED_EDGE('',*,*,#17408,.T.);
#26300=ORIENTED_EDGE('',*,*,#17644,.T.);
#26301=ORIENTED_EDGE('',*,*,#17678,.T.);
#26302=ORIENTED_EDGE('',*,*,#17675,.T.);
#26303=ORIENTED_EDGE('',*,*,#17672,.T.);
#26304=ORIENTED_EDGE('',*,*,#17669,.T.);
#26305=ORIENTED_EDGE('',*,*,#17666,.T.);
#26306=ORIENTED_EDGE('',*,*,#17663,.T.);
#26307=ORIENTED_EDGE('',*,*,#17660,.T.);
#26308=ORIENTED_EDGE('',*,*,#17657,.T.);
#26309=ORIENTED_EDGE('',*,*,#17654,.T.);
#26310=ORIENTED_EDGE('',*,*,#17651,.T.);
#26311=ORIENTED_EDGE('',*,*,#17648,.T.);
#26312=ORIENTED_EDGE('',*,*,#17680,.T.);
#26313=ORIENTED_EDGE('',*,*,#17705,.T.);
#26314=ORIENTED_EDGE('',*,*,#17702,.T.);
#26315=ORIENTED_EDGE('',*,*,#17699,.T.);
#26316=ORIENTED_EDGE('',*,*,#17696,.T.);
#26317=ORIENTED_EDGE('',*,*,#17693,.T.);
#26318=ORIENTED_EDGE('',*,*,#17690,.T.);
#26319=ORIENTED_EDGE('',*,*,#17687,.T.);
#26320=ORIENTED_EDGE('',*,*,#17684,.T.);
#26321=ORIENTED_EDGE('',*,*,#17791,.T.);
#26322=ORIENTED_EDGE('',*,*,#17825,.T.);
#26323=ORIENTED_EDGE('',*,*,#17822,.T.);
#26324=ORIENTED_EDGE('',*,*,#17819,.T.);
#26325=ORIENTED_EDGE('',*,*,#17816,.T.);
#26326=ORIENTED_EDGE('',*,*,#17813,.T.);
#26327=ORIENTED_EDGE('',*,*,#17810,.T.);
#26328=ORIENTED_EDGE('',*,*,#17807,.T.);
#26329=ORIENTED_EDGE('',*,*,#17804,.T.);
#26330=ORIENTED_EDGE('',*,*,#17801,.T.);
#26331=ORIENTED_EDGE('',*,*,#17798,.T.);
#26332=ORIENTED_EDGE('',*,*,#17795,.T.);
#26333=ORIENTED_EDGE('',*,*,#17827,.T.);
#26334=ORIENTED_EDGE('',*,*,#17852,.T.);
#26335=ORIENTED_EDGE('',*,*,#17849,.T.);
#26336=ORIENTED_EDGE('',*,*,#17846,.T.);
#26337=ORIENTED_EDGE('',*,*,#17843,.T.);
#26338=ORIENTED_EDGE('',*,*,#17840,.T.);
#26339=ORIENTED_EDGE('',*,*,#17837,.T.);
#26340=ORIENTED_EDGE('',*,*,#17834,.T.);
#26341=ORIENTED_EDGE('',*,*,#17831,.T.);
#26342=ORIENTED_EDGE('',*,*,#18004,.T.);
#26343=ORIENTED_EDGE('',*,*,#18038,.T.);
#26344=ORIENTED_EDGE('',*,*,#18035,.T.);
#26345=ORIENTED_EDGE('',*,*,#18032,.T.);
#26346=ORIENTED_EDGE('',*,*,#18029,.T.);
#26347=ORIENTED_EDGE('',*,*,#18026,.T.);
#26348=ORIENTED_EDGE('',*,*,#18023,.T.);
#26349=ORIENTED_EDGE('',*,*,#18020,.T.);
#26350=ORIENTED_EDGE('',*,*,#18017,.T.);
#26351=ORIENTED_EDGE('',*,*,#18014,.T.);
#26352=ORIENTED_EDGE('',*,*,#18011,.T.);
#26353=ORIENTED_EDGE('',*,*,#18008,.T.);
#26354=ORIENTED_EDGE('',*,*,#18040,.T.);
#26355=ORIENTED_EDGE('',*,*,#18128,.T.);
#26356=ORIENTED_EDGE('',*,*,#18125,.T.);
#26357=ORIENTED_EDGE('',*,*,#18122,.T.);
#26358=ORIENTED_EDGE('',*,*,#18119,.T.);
#26359=ORIENTED_EDGE('',*,*,#18116,.T.);
#26360=ORIENTED_EDGE('',*,*,#18113,.T.);
#26361=ORIENTED_EDGE('',*,*,#18110,.T.);
#26362=ORIENTED_EDGE('',*,*,#18107,.T.);
#26363=ORIENTED_EDGE('',*,*,#18104,.T.);
#26364=ORIENTED_EDGE('',*,*,#18101,.T.);
#26365=ORIENTED_EDGE('',*,*,#18098,.T.);
#26366=ORIENTED_EDGE('',*,*,#18095,.T.);
#26367=ORIENTED_EDGE('',*,*,#18092,.T.);
#26368=ORIENTED_EDGE('',*,*,#18089,.T.);
#26369=ORIENTED_EDGE('',*,*,#18086,.T.);
#26370=ORIENTED_EDGE('',*,*,#18083,.T.);
#26371=ORIENTED_EDGE('',*,*,#18080,.T.);
#26372=ORIENTED_EDGE('',*,*,#18077,.T.);
#26373=ORIENTED_EDGE('',*,*,#18074,.T.);
#26374=ORIENTED_EDGE('',*,*,#18071,.T.);
#26375=ORIENTED_EDGE('',*,*,#18068,.T.);
#26376=ORIENTED_EDGE('',*,*,#18065,.T.);
#26377=ORIENTED_EDGE('',*,*,#18062,.T.);
#26378=ORIENTED_EDGE('',*,*,#18059,.T.);
#26379=ORIENTED_EDGE('',*,*,#18056,.T.);
#26380=ORIENTED_EDGE('',*,*,#18053,.T.);
#26381=ORIENTED_EDGE('',*,*,#18050,.T.);
#26382=ORIENTED_EDGE('',*,*,#18047,.T.);
#26383=ORIENTED_EDGE('',*,*,#18044,.T.);
#26384=ORIENTED_EDGE('',*,*,#18232,.T.);
#26385=ORIENTED_EDGE('',*,*,#18242,.T.);
#26386=ORIENTED_EDGE('',*,*,#18239,.T.);
#26387=ORIENTED_EDGE('',*,*,#18236,.T.);
#26388=ORIENTED_EDGE('',*,*,#18244,.T.);
#26389=ORIENTED_EDGE('',*,*,#18254,.T.);
#26390=ORIENTED_EDGE('',*,*,#18251,.T.);
#26391=ORIENTED_EDGE('',*,*,#18248,.T.);
#26392=ORIENTED_EDGE('',*,*,#18256,.T.);
#26393=ORIENTED_EDGE('',*,*,#18266,.T.);
#26394=ORIENTED_EDGE('',*,*,#18263,.T.);
#26395=ORIENTED_EDGE('',*,*,#18260,.T.);
#26396=ORIENTED_EDGE('',*,*,#18268,.T.);
#26397=ORIENTED_EDGE('',*,*,#18278,.T.);
#26398=ORIENTED_EDGE('',*,*,#18275,.T.);
#26399=ORIENTED_EDGE('',*,*,#18272,.T.);
#26400=ORIENTED_EDGE('',*,*,#18280,.T.);
#26401=ORIENTED_EDGE('',*,*,#18290,.T.);
#26402=ORIENTED_EDGE('',*,*,#18287,.T.);
#26403=ORIENTED_EDGE('',*,*,#18284,.T.);
#26404=ORIENTED_EDGE('',*,*,#18292,.T.);
#26405=ORIENTED_EDGE('',*,*,#18302,.T.);
#26406=ORIENTED_EDGE('',*,*,#18299,.T.);
#26407=ORIENTED_EDGE('',*,*,#18296,.T.);
#26408=ORIENTED_EDGE('',*,*,#18304,.T.);
#26409=ORIENTED_EDGE('',*,*,#18314,.T.);
#26410=ORIENTED_EDGE('',*,*,#18311,.T.);
#26411=ORIENTED_EDGE('',*,*,#18308,.T.);
#26412=ORIENTED_EDGE('',*,*,#18316,.T.);
#26413=ORIENTED_EDGE('',*,*,#18326,.T.);
#26414=ORIENTED_EDGE('',*,*,#18323,.T.);
#26415=ORIENTED_EDGE('',*,*,#18320,.T.);
#26416=ORIENTED_EDGE('',*,*,#18328,.T.);
#26417=ORIENTED_EDGE('',*,*,#18338,.T.);
#26418=ORIENTED_EDGE('',*,*,#18335,.T.);
#26419=ORIENTED_EDGE('',*,*,#18332,.T.);
#26420=ORIENTED_EDGE('',*,*,#18340,.T.);
#26421=ORIENTED_EDGE('',*,*,#18350,.T.);
#26422=ORIENTED_EDGE('',*,*,#18347,.T.);
#26423=ORIENTED_EDGE('',*,*,#18344,.T.);
#26424=ORIENTED_EDGE('',*,*,#18352,.T.);
#26425=ORIENTED_EDGE('',*,*,#18362,.T.);
#26426=ORIENTED_EDGE('',*,*,#18359,.T.);
#26427=ORIENTED_EDGE('',*,*,#18356,.T.);
#26428=ORIENTED_EDGE('',*,*,#18364,.T.);
#26429=ORIENTED_EDGE('',*,*,#18374,.T.);
#26430=ORIENTED_EDGE('',*,*,#18371,.T.);
#26431=ORIENTED_EDGE('',*,*,#18368,.T.);
#26432=ORIENTED_EDGE('',*,*,#18376,.T.);
#26433=ORIENTED_EDGE('',*,*,#18386,.T.);
#26434=ORIENTED_EDGE('',*,*,#18383,.T.);
#26435=ORIENTED_EDGE('',*,*,#18380,.T.);
#26436=ORIENTED_EDGE('',*,*,#18388,.T.);
#26437=ORIENTED_EDGE('',*,*,#18398,.T.);
#26438=ORIENTED_EDGE('',*,*,#18395,.T.);
#26439=ORIENTED_EDGE('',*,*,#18392,.T.);
#26440=ORIENTED_EDGE('',*,*,#18400,.T.);
#26441=ORIENTED_EDGE('',*,*,#18410,.T.);
#26442=ORIENTED_EDGE('',*,*,#18407,.T.);
#26443=ORIENTED_EDGE('',*,*,#18404,.T.);
#26444=ORIENTED_EDGE('',*,*,#18412,.T.);
#26445=ORIENTED_EDGE('',*,*,#18422,.T.);
#26446=ORIENTED_EDGE('',*,*,#18419,.T.);
#26447=ORIENTED_EDGE('',*,*,#18416,.T.);
#26448=ORIENTED_EDGE('',*,*,#18424,.T.);
#26449=ORIENTED_EDGE('',*,*,#18434,.T.);
#26450=ORIENTED_EDGE('',*,*,#18431,.T.);
#26451=ORIENTED_EDGE('',*,*,#18428,.T.);
#26452=ORIENTED_EDGE('',*,*,#18436,.T.);
#26453=ORIENTED_EDGE('',*,*,#18446,.T.);
#26454=ORIENTED_EDGE('',*,*,#18443,.T.);
#26455=ORIENTED_EDGE('',*,*,#18440,.T.);
#26456=ORIENTED_EDGE('',*,*,#18448,.T.);
#26457=ORIENTED_EDGE('',*,*,#18458,.T.);
#26458=ORIENTED_EDGE('',*,*,#18455,.T.);
#26459=ORIENTED_EDGE('',*,*,#18452,.T.);
#26460=ORIENTED_EDGE('',*,*,#18460,.T.);
#26461=ORIENTED_EDGE('',*,*,#18470,.T.);
#26462=ORIENTED_EDGE('',*,*,#18467,.T.);
#26463=ORIENTED_EDGE('',*,*,#18464,.T.);
#26464=ORIENTED_EDGE('',*,*,#18472,.T.);
#26465=ORIENTED_EDGE('',*,*,#18482,.T.);
#26466=ORIENTED_EDGE('',*,*,#18479,.T.);
#26467=ORIENTED_EDGE('',*,*,#18476,.T.);
#26468=ORIENTED_EDGE('',*,*,#18484,.T.);
#26469=ORIENTED_EDGE('',*,*,#18494,.T.);
#26470=ORIENTED_EDGE('',*,*,#18491,.T.);
#26471=ORIENTED_EDGE('',*,*,#18488,.T.);
#26472=ORIENTED_EDGE('',*,*,#18496,.T.);
#26473=ORIENTED_EDGE('',*,*,#18506,.T.);
#26474=ORIENTED_EDGE('',*,*,#18503,.T.);
#26475=ORIENTED_EDGE('',*,*,#18500,.T.);
#26476=ORIENTED_EDGE('',*,*,#18508,.T.);
#26477=ORIENTED_EDGE('',*,*,#18518,.T.);
#26478=ORIENTED_EDGE('',*,*,#18515,.T.);
#26479=ORIENTED_EDGE('',*,*,#18512,.T.);
#26480=ORIENTED_EDGE('',*,*,#18520,.T.);
#26481=ORIENTED_EDGE('',*,*,#18530,.T.);
#26482=ORIENTED_EDGE('',*,*,#18527,.T.);
#26483=ORIENTED_EDGE('',*,*,#18524,.T.);
#26484=ORIENTED_EDGE('',*,*,#18532,.T.);
#26485=ORIENTED_EDGE('',*,*,#18542,.T.);
#26486=ORIENTED_EDGE('',*,*,#18539,.T.);
#26487=ORIENTED_EDGE('',*,*,#18536,.T.);
#26488=ORIENTED_EDGE('',*,*,#18544,.T.);
#26489=ORIENTED_EDGE('',*,*,#18554,.T.);
#26490=ORIENTED_EDGE('',*,*,#18551,.T.);
#26491=ORIENTED_EDGE('',*,*,#18548,.T.);
#26492=ORIENTED_EDGE('',*,*,#18556,.T.);
#26493=ORIENTED_EDGE('',*,*,#18566,.T.);
#26494=ORIENTED_EDGE('',*,*,#18563,.T.);
#26495=ORIENTED_EDGE('',*,*,#18560,.T.);
#26496=ORIENTED_EDGE('',*,*,#18568,.T.);
#26497=ORIENTED_EDGE('',*,*,#18578,.T.);
#26498=ORIENTED_EDGE('',*,*,#18575,.T.);
#26499=ORIENTED_EDGE('',*,*,#18572,.T.);
#26500=ORIENTED_EDGE('',*,*,#18580,.T.);
#26501=ORIENTED_EDGE('',*,*,#18590,.T.);
#26502=ORIENTED_EDGE('',*,*,#18587,.T.);
#26503=ORIENTED_EDGE('',*,*,#18584,.T.);
#26504=ORIENTED_EDGE('',*,*,#18592,.T.);
#26505=ORIENTED_EDGE('',*,*,#18602,.T.);
#26506=ORIENTED_EDGE('',*,*,#18599,.T.);
#26507=ORIENTED_EDGE('',*,*,#18596,.T.);
#26508=ORIENTED_EDGE('',*,*,#18604,.T.);
#26509=ORIENTED_EDGE('',*,*,#18614,.T.);
#26510=ORIENTED_EDGE('',*,*,#18611,.T.);
#26511=ORIENTED_EDGE('',*,*,#18608,.T.);
#26512=ORIENTED_EDGE('',*,*,#18616,.T.);
#26513=ORIENTED_EDGE('',*,*,#18626,.T.);
#26514=ORIENTED_EDGE('',*,*,#18623,.T.);
#26515=ORIENTED_EDGE('',*,*,#18620,.T.);
#26516=ORIENTED_EDGE('',*,*,#18628,.T.);
#26517=ORIENTED_EDGE('',*,*,#18638,.T.);
#26518=ORIENTED_EDGE('',*,*,#18635,.T.);
#26519=ORIENTED_EDGE('',*,*,#18632,.T.);
#26520=ORIENTED_EDGE('',*,*,#18640,.T.);
#26521=ORIENTED_EDGE('',*,*,#18650,.T.);
#26522=ORIENTED_EDGE('',*,*,#18647,.T.);
#26523=ORIENTED_EDGE('',*,*,#18644,.T.);
#26524=ORIENTED_EDGE('',*,*,#18652,.T.);
#26525=ORIENTED_EDGE('',*,*,#18662,.T.);
#26526=ORIENTED_EDGE('',*,*,#18659,.T.);
#26527=ORIENTED_EDGE('',*,*,#18656,.T.);
#26528=ORIENTED_EDGE('',*,*,#18664,.T.);
#26529=ORIENTED_EDGE('',*,*,#18674,.T.);
#26530=ORIENTED_EDGE('',*,*,#18671,.T.);
#26531=ORIENTED_EDGE('',*,*,#18668,.T.);
#26532=ORIENTED_EDGE('',*,*,#18676,.T.);
#26533=ORIENTED_EDGE('',*,*,#18686,.T.);
#26534=ORIENTED_EDGE('',*,*,#18683,.T.);
#26535=ORIENTED_EDGE('',*,*,#18680,.T.);
#26536=ORIENTED_EDGE('',*,*,#18688,.T.);
#26537=ORIENTED_EDGE('',*,*,#18698,.T.);
#26538=ORIENTED_EDGE('',*,*,#18695,.T.);
#26539=ORIENTED_EDGE('',*,*,#18692,.T.);
#26540=ORIENTED_EDGE('',*,*,#18700,.T.);
#26541=ORIENTED_EDGE('',*,*,#18710,.T.);
#26542=ORIENTED_EDGE('',*,*,#18707,.T.);
#26543=ORIENTED_EDGE('',*,*,#18704,.T.);
#26544=ORIENTED_EDGE('',*,*,#18712,.T.);
#26545=ORIENTED_EDGE('',*,*,#18722,.T.);
#26546=ORIENTED_EDGE('',*,*,#18719,.T.);
#26547=ORIENTED_EDGE('',*,*,#18716,.T.);
#26548=ORIENTED_EDGE('',*,*,#18724,.T.);
#26549=ORIENTED_EDGE('',*,*,#18734,.T.);
#26550=ORIENTED_EDGE('',*,*,#18731,.T.);
#26551=ORIENTED_EDGE('',*,*,#18728,.T.);
#26552=ORIENTED_EDGE('',*,*,#18736,.T.);
#26553=ORIENTED_EDGE('',*,*,#18746,.T.);
#26554=ORIENTED_EDGE('',*,*,#18743,.T.);
#26555=ORIENTED_EDGE('',*,*,#18740,.T.);
#26556=ORIENTED_EDGE('',*,*,#18748,.T.);
#26557=ORIENTED_EDGE('',*,*,#18758,.T.);
#26558=ORIENTED_EDGE('',*,*,#18755,.T.);
#26559=ORIENTED_EDGE('',*,*,#18752,.T.);
#26560=ORIENTED_EDGE('',*,*,#18760,.T.);
#26561=ORIENTED_EDGE('',*,*,#18770,.T.);
#26562=ORIENTED_EDGE('',*,*,#18767,.T.);
#26563=ORIENTED_EDGE('',*,*,#18764,.T.);
#26564=ORIENTED_EDGE('',*,*,#18772,.T.);
#26565=ORIENTED_EDGE('',*,*,#18782,.T.);
#26566=ORIENTED_EDGE('',*,*,#18779,.T.);
#26567=ORIENTED_EDGE('',*,*,#18776,.T.);
#26568=ORIENTED_EDGE('',*,*,#18784,.T.);
#26569=ORIENTED_EDGE('',*,*,#18794,.T.);
#26570=ORIENTED_EDGE('',*,*,#18791,.T.);
#26571=ORIENTED_EDGE('',*,*,#18788,.T.);
#26572=ORIENTED_EDGE('',*,*,#18796,.T.);
#26573=ORIENTED_EDGE('',*,*,#18806,.T.);
#26574=ORIENTED_EDGE('',*,*,#18803,.T.);
#26575=ORIENTED_EDGE('',*,*,#18800,.T.);
#26576=ORIENTED_EDGE('',*,*,#18808,.T.);
#26577=ORIENTED_EDGE('',*,*,#18818,.T.);
#26578=ORIENTED_EDGE('',*,*,#18815,.T.);
#26579=ORIENTED_EDGE('',*,*,#18812,.T.);
#26580=ORIENTED_EDGE('',*,*,#18820,.T.);
#26581=ORIENTED_EDGE('',*,*,#18830,.T.);
#26582=ORIENTED_EDGE('',*,*,#18827,.T.);
#26583=ORIENTED_EDGE('',*,*,#18824,.T.);
#26584=ORIENTED_EDGE('',*,*,#18832,.T.);
#26585=ORIENTED_EDGE('',*,*,#18842,.T.);
#26586=ORIENTED_EDGE('',*,*,#18839,.T.);
#26587=ORIENTED_EDGE('',*,*,#18836,.T.);
#26588=ORIENTED_EDGE('',*,*,#18844,.T.);
#26589=ORIENTED_EDGE('',*,*,#18854,.T.);
#26590=ORIENTED_EDGE('',*,*,#18851,.T.);
#26591=ORIENTED_EDGE('',*,*,#18848,.T.);
#26592=ORIENTED_EDGE('',*,*,#18856,.T.);
#26593=ORIENTED_EDGE('',*,*,#18866,.T.);
#26594=ORIENTED_EDGE('',*,*,#18863,.T.);
#26595=ORIENTED_EDGE('',*,*,#18860,.T.);
#26596=ORIENTED_EDGE('',*,*,#18868,.T.);
#26597=ORIENTED_EDGE('',*,*,#18878,.T.);
#26598=ORIENTED_EDGE('',*,*,#18875,.T.);
#26599=ORIENTED_EDGE('',*,*,#18872,.T.);
#26600=ORIENTED_EDGE('',*,*,#18880,.T.);
#26601=ORIENTED_EDGE('',*,*,#18890,.T.);
#26602=ORIENTED_EDGE('',*,*,#18887,.T.);
#26603=ORIENTED_EDGE('',*,*,#18884,.T.);
#26604=ORIENTED_EDGE('',*,*,#18892,.T.);
#26605=ORIENTED_EDGE('',*,*,#18902,.T.);
#26606=ORIENTED_EDGE('',*,*,#18899,.T.);
#26607=ORIENTED_EDGE('',*,*,#18896,.T.);
#26608=ORIENTED_EDGE('',*,*,#18904,.T.);
#26609=ORIENTED_EDGE('',*,*,#18914,.T.);
#26610=ORIENTED_EDGE('',*,*,#18911,.T.);
#26611=ORIENTED_EDGE('',*,*,#18908,.T.);
#26612=ORIENTED_EDGE('',*,*,#18916,.T.);
#26613=ORIENTED_EDGE('',*,*,#18926,.T.);
#26614=ORIENTED_EDGE('',*,*,#18923,.T.);
#26615=ORIENTED_EDGE('',*,*,#18920,.T.);
#26616=ORIENTED_EDGE('',*,*,#18928,.T.);
#26617=ORIENTED_EDGE('',*,*,#18938,.T.);
#26618=ORIENTED_EDGE('',*,*,#18935,.T.);
#26619=ORIENTED_EDGE('',*,*,#18932,.T.);
#26620=ORIENTED_EDGE('',*,*,#18940,.T.);
#26621=ORIENTED_EDGE('',*,*,#18950,.T.);
#26622=ORIENTED_EDGE('',*,*,#18947,.T.);
#26623=ORIENTED_EDGE('',*,*,#18944,.T.);
#26624=ORIENTED_EDGE('',*,*,#18952,.T.);
#26625=ORIENTED_EDGE('',*,*,#18962,.T.);
#26626=ORIENTED_EDGE('',*,*,#18959,.T.);
#26627=ORIENTED_EDGE('',*,*,#18956,.T.);
#26628=ORIENTED_EDGE('',*,*,#18964,.T.);
#26629=ORIENTED_EDGE('',*,*,#18974,.T.);
#26630=ORIENTED_EDGE('',*,*,#18971,.T.);
#26631=ORIENTED_EDGE('',*,*,#18968,.T.);
#26632=ORIENTED_EDGE('',*,*,#18976,.T.);
#26633=ORIENTED_EDGE('',*,*,#18986,.T.);
#26634=ORIENTED_EDGE('',*,*,#18983,.T.);
#26635=ORIENTED_EDGE('',*,*,#18980,.T.);
#26636=ORIENTED_EDGE('',*,*,#18988,.T.);
#26637=ORIENTED_EDGE('',*,*,#18998,.T.);
#26638=ORIENTED_EDGE('',*,*,#18995,.T.);
#26639=ORIENTED_EDGE('',*,*,#18992,.T.);
#26640=ORIENTED_EDGE('',*,*,#19000,.T.);
#26641=ORIENTED_EDGE('',*,*,#19010,.T.);
#26642=ORIENTED_EDGE('',*,*,#19007,.T.);
#26643=ORIENTED_EDGE('',*,*,#19004,.T.);
#26644=ORIENTED_EDGE('',*,*,#19012,.T.);
#26645=ORIENTED_EDGE('',*,*,#19022,.T.);
#26646=ORIENTED_EDGE('',*,*,#19019,.T.);
#26647=ORIENTED_EDGE('',*,*,#19016,.T.);
#26648=ORIENTED_EDGE('',*,*,#19024,.T.);
#26649=ORIENTED_EDGE('',*,*,#19034,.T.);
#26650=ORIENTED_EDGE('',*,*,#19031,.T.);
#26651=ORIENTED_EDGE('',*,*,#19028,.T.);
#26652=ORIENTED_EDGE('',*,*,#19036,.T.);
#26653=ORIENTED_EDGE('',*,*,#19046,.T.);
#26654=ORIENTED_EDGE('',*,*,#19043,.T.);
#26655=ORIENTED_EDGE('',*,*,#19040,.T.);
#26656=ORIENTED_EDGE('',*,*,#19048,.T.);
#26657=ORIENTED_EDGE('',*,*,#19058,.T.);
#26658=ORIENTED_EDGE('',*,*,#19055,.T.);
#26659=ORIENTED_EDGE('',*,*,#19052,.T.);
#26660=ORIENTED_EDGE('',*,*,#19060,.T.);
#26661=ORIENTED_EDGE('',*,*,#19070,.T.);
#26662=ORIENTED_EDGE('',*,*,#19067,.T.);
#26663=ORIENTED_EDGE('',*,*,#19064,.T.);
#26664=ORIENTED_EDGE('',*,*,#19072,.T.);
#26665=ORIENTED_EDGE('',*,*,#19082,.T.);
#26666=ORIENTED_EDGE('',*,*,#19079,.T.);
#26667=ORIENTED_EDGE('',*,*,#19076,.T.);
#26668=ORIENTED_EDGE('',*,*,#19084,.T.);
#26669=ORIENTED_EDGE('',*,*,#19094,.T.);
#26670=ORIENTED_EDGE('',*,*,#19091,.T.);
#26671=ORIENTED_EDGE('',*,*,#19088,.T.);
#26672=ORIENTED_EDGE('',*,*,#19096,.T.);
#26673=ORIENTED_EDGE('',*,*,#19106,.T.);
#26674=ORIENTED_EDGE('',*,*,#19103,.T.);
#26675=ORIENTED_EDGE('',*,*,#19100,.T.);
#26676=ORIENTED_EDGE('',*,*,#19108,.T.);
#26677=ORIENTED_EDGE('',*,*,#19118,.T.);
#26678=ORIENTED_EDGE('',*,*,#19115,.T.);
#26679=ORIENTED_EDGE('',*,*,#19112,.T.);
#26680=ORIENTED_EDGE('',*,*,#19120,.T.);
#26681=ORIENTED_EDGE('',*,*,#19130,.T.);
#26682=ORIENTED_EDGE('',*,*,#19127,.T.);
#26683=ORIENTED_EDGE('',*,*,#19124,.T.);
#26684=ORIENTED_EDGE('',*,*,#19132,.T.);
#26685=ORIENTED_EDGE('',*,*,#19142,.T.);
#26686=ORIENTED_EDGE('',*,*,#19139,.T.);
#26687=ORIENTED_EDGE('',*,*,#19136,.T.);
#26688=ORIENTED_EDGE('',*,*,#19144,.T.);
#26689=ORIENTED_EDGE('',*,*,#19154,.T.);
#26690=ORIENTED_EDGE('',*,*,#19151,.T.);
#26691=ORIENTED_EDGE('',*,*,#19148,.T.);
#26692=ORIENTED_EDGE('',*,*,#19156,.T.);
#26693=ORIENTED_EDGE('',*,*,#19166,.T.);
#26694=ORIENTED_EDGE('',*,*,#19163,.T.);
#26695=ORIENTED_EDGE('',*,*,#19160,.T.);
#26696=ORIENTED_EDGE('',*,*,#19168,.T.);
#26697=ORIENTED_EDGE('',*,*,#19178,.T.);
#26698=ORIENTED_EDGE('',*,*,#19175,.T.);
#26699=ORIENTED_EDGE('',*,*,#19172,.T.);
#26700=ORIENTED_EDGE('',*,*,#19180,.T.);
#26701=ORIENTED_EDGE('',*,*,#19190,.T.);
#26702=ORIENTED_EDGE('',*,*,#19187,.T.);
#26703=ORIENTED_EDGE('',*,*,#19184,.T.);
#26704=ORIENTED_EDGE('',*,*,#19192,.T.);
#26705=ORIENTED_EDGE('',*,*,#19202,.T.);
#26706=ORIENTED_EDGE('',*,*,#19199,.T.);
#26707=ORIENTED_EDGE('',*,*,#19196,.T.);
#26708=ORIENTED_EDGE('',*,*,#19204,.T.);
#26709=ORIENTED_EDGE('',*,*,#19214,.T.);
#26710=ORIENTED_EDGE('',*,*,#19211,.T.);
#26711=ORIENTED_EDGE('',*,*,#19208,.T.);
#26712=ORIENTED_EDGE('',*,*,#19216,.T.);
#26713=ORIENTED_EDGE('',*,*,#19226,.T.);
#26714=ORIENTED_EDGE('',*,*,#19223,.T.);
#26715=ORIENTED_EDGE('',*,*,#19220,.T.);
#26716=ORIENTED_EDGE('',*,*,#19228,.T.);
#26717=ORIENTED_EDGE('',*,*,#19238,.T.);
#26718=ORIENTED_EDGE('',*,*,#19235,.T.);
#26719=ORIENTED_EDGE('',*,*,#19232,.T.);
#26720=ORIENTED_EDGE('',*,*,#19240,.T.);
#26721=ORIENTED_EDGE('',*,*,#19250,.T.);
#26722=ORIENTED_EDGE('',*,*,#19247,.T.);
#26723=ORIENTED_EDGE('',*,*,#19244,.T.);
#26724=ORIENTED_EDGE('',*,*,#19254,.T.);
#26725=ORIENTED_EDGE('',*,*,#19257,.T.);
#26726=ORIENTED_EDGE('',*,*,#18199,.T.);
#26727=ORIENTED_EDGE('',*,*,#18230,.T.);
#26728=ORIENTED_EDGE('',*,*,#18227,.T.);
#26729=ORIENTED_EDGE('',*,*,#18224,.T.);
#26730=ORIENTED_EDGE('',*,*,#18221,.T.);
#26731=ORIENTED_EDGE('',*,*,#18218,.T.);
#26732=ORIENTED_EDGE('',*,*,#18215,.T.);
#26733=ORIENTED_EDGE('',*,*,#18212,.T.);
#26734=ORIENTED_EDGE('',*,*,#18209,.T.);
#26735=ORIENTED_EDGE('',*,*,#18206,.T.);
#26736=ORIENTED_EDGE('',*,*,#18203,.T.);
#26737=ORIENTED_EDGE('',*,*,#18154,.T.);
#26738=ORIENTED_EDGE('',*,*,#18188,.T.);
#26739=ORIENTED_EDGE('',*,*,#18185,.T.);
#26740=ORIENTED_EDGE('',*,*,#18182,.T.);
#26741=ORIENTED_EDGE('',*,*,#18179,.T.);
#26742=ORIENTED_EDGE('',*,*,#18176,.T.);
#26743=ORIENTED_EDGE('',*,*,#18173,.T.);
#26744=ORIENTED_EDGE('',*,*,#18170,.T.);
#26745=ORIENTED_EDGE('',*,*,#18167,.T.);
#26746=ORIENTED_EDGE('',*,*,#18164,.T.);
#26747=ORIENTED_EDGE('',*,*,#18161,.T.);
#26748=ORIENTED_EDGE('',*,*,#18158,.T.);
#26749=ORIENTED_EDGE('',*,*,#17914,.T.);
#26750=ORIENTED_EDGE('',*,*,#17978,.T.);
#26751=ORIENTED_EDGE('',*,*,#17975,.T.);
#26752=ORIENTED_EDGE('',*,*,#17972,.T.);
#26753=ORIENTED_EDGE('',*,*,#17969,.T.);
#26754=ORIENTED_EDGE('',*,*,#17966,.T.);
#26755=ORIENTED_EDGE('',*,*,#17963,.T.);
#26756=ORIENTED_EDGE('',*,*,#17960,.T.);
#26757=ORIENTED_EDGE('',*,*,#17957,.T.);
#26758=ORIENTED_EDGE('',*,*,#17954,.T.);
#26759=ORIENTED_EDGE('',*,*,#17951,.T.);
#26760=ORIENTED_EDGE('',*,*,#17948,.T.);
#26761=ORIENTED_EDGE('',*,*,#17945,.T.);
#26762=ORIENTED_EDGE('',*,*,#17942,.T.);
#26763=ORIENTED_EDGE('',*,*,#17939,.T.);
#26764=ORIENTED_EDGE('',*,*,#17936,.T.);
#26765=ORIENTED_EDGE('',*,*,#17933,.T.);
#26766=ORIENTED_EDGE('',*,*,#17930,.T.);
#26767=ORIENTED_EDGE('',*,*,#17927,.T.);
#26768=ORIENTED_EDGE('',*,*,#17924,.T.);
#26769=ORIENTED_EDGE('',*,*,#17921,.T.);
#26770=ORIENTED_EDGE('',*,*,#17918,.T.);
#26771=ORIENTED_EDGE('',*,*,#17878,.T.);
#26772=ORIENTED_EDGE('',*,*,#17912,.T.);
#26773=ORIENTED_EDGE('',*,*,#17909,.T.);
#26774=ORIENTED_EDGE('',*,*,#17906,.T.);
#26775=ORIENTED_EDGE('',*,*,#17903,.T.);
#26776=ORIENTED_EDGE('',*,*,#17900,.T.);
#26777=ORIENTED_EDGE('',*,*,#17897,.T.);
#26778=ORIENTED_EDGE('',*,*,#17894,.T.);
#26779=ORIENTED_EDGE('',*,*,#17891,.T.);
#26780=ORIENTED_EDGE('',*,*,#17888,.T.);
#26781=ORIENTED_EDGE('',*,*,#17885,.T.);
#26782=ORIENTED_EDGE('',*,*,#17882,.T.);
#26783=ORIENTED_EDGE('',*,*,#17731,.T.);
#26784=ORIENTED_EDGE('',*,*,#17765,.T.);
#26785=ORIENTED_EDGE('',*,*,#17762,.T.);
#26786=ORIENTED_EDGE('',*,*,#17759,.T.);
#26787=ORIENTED_EDGE('',*,*,#17756,.T.);
#26788=ORIENTED_EDGE('',*,*,#17753,.T.);
#26789=ORIENTED_EDGE('',*,*,#17750,.T.);
#26790=ORIENTED_EDGE('',*,*,#17747,.T.);
#26791=ORIENTED_EDGE('',*,*,#17744,.T.);
#26792=ORIENTED_EDGE('',*,*,#17741,.T.);
#26793=ORIENTED_EDGE('',*,*,#17738,.T.);
#26794=ORIENTED_EDGE('',*,*,#17735,.T.);
#26795=ORIENTED_EDGE('',*,*,#17554,.T.);
#26796=ORIENTED_EDGE('',*,*,#17618,.T.);
#26797=ORIENTED_EDGE('',*,*,#17615,.T.);
#26798=ORIENTED_EDGE('',*,*,#17612,.T.);
#26799=ORIENTED_EDGE('',*,*,#17609,.T.);
#26800=ORIENTED_EDGE('',*,*,#17606,.T.);
#26801=ORIENTED_EDGE('',*,*,#17603,.T.);
#26802=ORIENTED_EDGE('',*,*,#17600,.T.);
#26803=ORIENTED_EDGE('',*,*,#17597,.T.);
#26804=ORIENTED_EDGE('',*,*,#17594,.T.);
#26805=ORIENTED_EDGE('',*,*,#17591,.T.);
#26806=ORIENTED_EDGE('',*,*,#17588,.T.);
#26807=ORIENTED_EDGE('',*,*,#17585,.T.);
#26808=ORIENTED_EDGE('',*,*,#17582,.T.);
#26809=ORIENTED_EDGE('',*,*,#17579,.T.);
#26810=ORIENTED_EDGE('',*,*,#17576,.T.);
#26811=ORIENTED_EDGE('',*,*,#17573,.T.);
#26812=ORIENTED_EDGE('',*,*,#17570,.T.);
#26813=ORIENTED_EDGE('',*,*,#17567,.T.);
#26814=ORIENTED_EDGE('',*,*,#17564,.T.);
#26815=ORIENTED_EDGE('',*,*,#17561,.T.);
#26816=ORIENTED_EDGE('',*,*,#17558,.T.);
#26817=ORIENTED_EDGE('',*,*,#17518,.T.);
#26818=ORIENTED_EDGE('',*,*,#17552,.T.);
#26819=ORIENTED_EDGE('',*,*,#17549,.T.);
#26820=ORIENTED_EDGE('',*,*,#17546,.T.);
#26821=ORIENTED_EDGE('',*,*,#17543,.T.);
#26822=ORIENTED_EDGE('',*,*,#17540,.T.);
#26823=ORIENTED_EDGE('',*,*,#17537,.T.);
#26824=ORIENTED_EDGE('',*,*,#17534,.T.);
#26825=ORIENTED_EDGE('',*,*,#17531,.T.);
#26826=ORIENTED_EDGE('',*,*,#17528,.T.);
#26827=ORIENTED_EDGE('',*,*,#17525,.T.);
#26828=ORIENTED_EDGE('',*,*,#17522,.T.);
#26829=ORIENTED_EDGE('',*,*,#17311,.T.);
#26830=ORIENTED_EDGE('',*,*,#17342,.T.);
#26831=ORIENTED_EDGE('',*,*,#17339,.T.);
#26832=ORIENTED_EDGE('',*,*,#17336,.T.);
#26833=ORIENTED_EDGE('',*,*,#17333,.T.);
#26834=ORIENTED_EDGE('',*,*,#17330,.T.);
#26835=ORIENTED_EDGE('',*,*,#17327,.T.);
#26836=ORIENTED_EDGE('',*,*,#17324,.T.);
#26837=ORIENTED_EDGE('',*,*,#17321,.T.);
#26838=ORIENTED_EDGE('',*,*,#17318,.T.);
#26839=ORIENTED_EDGE('',*,*,#17315,.T.);
#26840=ORIENTED_EDGE('',*,*,#17266,.T.);
#26841=ORIENTED_EDGE('',*,*,#17300,.T.);
#26842=ORIENTED_EDGE('',*,*,#17297,.T.);
#26843=ORIENTED_EDGE('',*,*,#17294,.T.);
#26844=ORIENTED_EDGE('',*,*,#17291,.T.);
#26845=ORIENTED_EDGE('',*,*,#17288,.T.);
#26846=ORIENTED_EDGE('',*,*,#17285,.T.);
#26847=ORIENTED_EDGE('',*,*,#17282,.T.);
#26848=ORIENTED_EDGE('',*,*,#17279,.T.);
#26849=ORIENTED_EDGE('',*,*,#17276,.T.);
#26850=ORIENTED_EDGE('',*,*,#17273,.T.);
#26851=ORIENTED_EDGE('',*,*,#17270,.T.);
#26852=ORIENTED_EDGE('',*,*,#19280,.F.);
#26853=ORIENTED_EDGE('',*,*,#19258,.F.);
#26854=ORIENTED_EDGE('',*,*,#19262,.F.);
#26855=ORIENTED_EDGE('',*,*,#19265,.F.);
#26856=ORIENTED_EDGE('',*,*,#19268,.F.);
#26857=ORIENTED_EDGE('',*,*,#19271,.F.);
#26858=ORIENTED_EDGE('',*,*,#19274,.F.);
#26859=ORIENTED_EDGE('',*,*,#19277,.F.);
#26860=ORIENTED_EDGE('',*,*,#19252,.T.);
#26861=ORIENTED_EDGE('',*,*,#19255,.T.);
#26862=ORIENTED_EDGE('',*,*,#19282,.F.);
#26863=ORIENTED_EDGE('',*,*,#19283,.T.);
#26864=ORIENTED_EDGE('',*,*,#19284,.T.);
#26865=ORIENTED_EDGE('',*,*,#19285,.F.);
#26866=ORIENTED_EDGE('',*,*,#19286,.F.);
#26867=ORIENTED_EDGE('',*,*,#19287,.T.);
#26868=ORIENTED_EDGE('',*,*,#19288,.T.);
#26869=ORIENTED_EDGE('',*,*,#19283,.F.);
#26870=ORIENTED_EDGE('',*,*,#19289,.F.);
#26871=ORIENTED_EDGE('',*,*,#19290,.T.);
#26872=ORIENTED_EDGE('',*,*,#19291,.T.);
#26873=ORIENTED_EDGE('',*,*,#19287,.F.);
#26874=ORIENTED_EDGE('',*,*,#19292,.F.);
#26875=ORIENTED_EDGE('',*,*,#19285,.T.);
#26876=ORIENTED_EDGE('',*,*,#19293,.T.);
#26877=ORIENTED_EDGE('',*,*,#19290,.F.);
#26878=ORIENTED_EDGE('',*,*,#19293,.F.);
#26879=ORIENTED_EDGE('',*,*,#19284,.F.);
#26880=ORIENTED_EDGE('',*,*,#19288,.F.);
#26881=ORIENTED_EDGE('',*,*,#19291,.F.);
#26882=ORIENTED_EDGE('',*,*,#19294,.F.);
#26883=ORIENTED_EDGE('',*,*,#19295,.T.);
#26884=ORIENTED_EDGE('',*,*,#19296,.T.);
#26885=ORIENTED_EDGE('',*,*,#19297,.F.);
#26886=ORIENTED_EDGE('',*,*,#19298,.F.);
#26887=ORIENTED_EDGE('',*,*,#19299,.T.);
#26888=ORIENTED_EDGE('',*,*,#19300,.T.);
#26889=ORIENTED_EDGE('',*,*,#19295,.F.);
#26890=ORIENTED_EDGE('',*,*,#19301,.F.);
#26891=ORIENTED_EDGE('',*,*,#19302,.T.);
#26892=ORIENTED_EDGE('',*,*,#19303,.T.);
#26893=ORIENTED_EDGE('',*,*,#19299,.F.);
#26894=ORIENTED_EDGE('',*,*,#19304,.F.);
#26895=ORIENTED_EDGE('',*,*,#19297,.T.);
#26896=ORIENTED_EDGE('',*,*,#19305,.T.);
#26897=ORIENTED_EDGE('',*,*,#19302,.F.);
#26898=ORIENTED_EDGE('',*,*,#19305,.F.);
#26899=ORIENTED_EDGE('',*,*,#19296,.F.);
#26900=ORIENTED_EDGE('',*,*,#19300,.F.);
#26901=ORIENTED_EDGE('',*,*,#19303,.F.);
#26902=ORIENTED_EDGE('',*,*,#19306,.F.);
#26903=ORIENTED_EDGE('',*,*,#19307,.T.);
#26904=ORIENTED_EDGE('',*,*,#19308,.T.);
#26905=ORIENTED_EDGE('',*,*,#19309,.F.);
#26906=ORIENTED_EDGE('',*,*,#19310,.F.);
#26907=ORIENTED_EDGE('',*,*,#19311,.T.);
#26908=ORIENTED_EDGE('',*,*,#19312,.T.);
#26909=ORIENTED_EDGE('',*,*,#19307,.F.);
#26910=ORIENTED_EDGE('',*,*,#19313,.F.);
#26911=ORIENTED_EDGE('',*,*,#19314,.T.);
#26912=ORIENTED_EDGE('',*,*,#19315,.T.);
#26913=ORIENTED_EDGE('',*,*,#19311,.F.);
#26914=ORIENTED_EDGE('',*,*,#19316,.F.);
#26915=ORIENTED_EDGE('',*,*,#19309,.T.);
#26916=ORIENTED_EDGE('',*,*,#19317,.T.);
#26917=ORIENTED_EDGE('',*,*,#19314,.F.);
#26918=ORIENTED_EDGE('',*,*,#19317,.F.);
#26919=ORIENTED_EDGE('',*,*,#19308,.F.);
#26920=ORIENTED_EDGE('',*,*,#19312,.F.);
#26921=ORIENTED_EDGE('',*,*,#19315,.F.);
#26922=ORIENTED_EDGE('',*,*,#19318,.F.);
#26923=ORIENTED_EDGE('',*,*,#19319,.T.);
#26924=ORIENTED_EDGE('',*,*,#19320,.T.);
#26925=ORIENTED_EDGE('',*,*,#19321,.F.);
#26926=ORIENTED_EDGE('',*,*,#19322,.F.);
#26927=ORIENTED_EDGE('',*,*,#19323,.T.);
#26928=ORIENTED_EDGE('',*,*,#19324,.T.);
#26929=ORIENTED_EDGE('',*,*,#19319,.F.);
#26930=ORIENTED_EDGE('',*,*,#19325,.F.);
#26931=ORIENTED_EDGE('',*,*,#19326,.T.);
#26932=ORIENTED_EDGE('',*,*,#19327,.T.);
#26933=ORIENTED_EDGE('',*,*,#19323,.F.);
#26934=ORIENTED_EDGE('',*,*,#19328,.F.);
#26935=ORIENTED_EDGE('',*,*,#19321,.T.);
#26936=ORIENTED_EDGE('',*,*,#19329,.T.);
#26937=ORIENTED_EDGE('',*,*,#19326,.F.);
#26938=ORIENTED_EDGE('',*,*,#19329,.F.);
#26939=ORIENTED_EDGE('',*,*,#19320,.F.);
#26940=ORIENTED_EDGE('',*,*,#19324,.F.);
#26941=ORIENTED_EDGE('',*,*,#19327,.F.);
#26942=ORIENTED_EDGE('',*,*,#19330,.F.);
#26943=ORIENTED_EDGE('',*,*,#19331,.T.);
#26944=ORIENTED_EDGE('',*,*,#19332,.T.);
#26945=ORIENTED_EDGE('',*,*,#19333,.F.);
#26946=ORIENTED_EDGE('',*,*,#19334,.F.);
#26947=ORIENTED_EDGE('',*,*,#19335,.T.);
#26948=ORIENTED_EDGE('',*,*,#19336,.T.);
#26949=ORIENTED_EDGE('',*,*,#19331,.F.);
#26950=ORIENTED_EDGE('',*,*,#19337,.F.);
#26951=ORIENTED_EDGE('',*,*,#19338,.T.);
#26952=ORIENTED_EDGE('',*,*,#19339,.T.);
#26953=ORIENTED_EDGE('',*,*,#19335,.F.);
#26954=ORIENTED_EDGE('',*,*,#19340,.F.);
#26955=ORIENTED_EDGE('',*,*,#19333,.T.);
#26956=ORIENTED_EDGE('',*,*,#19341,.T.);
#26957=ORIENTED_EDGE('',*,*,#19338,.F.);
#26958=ORIENTED_EDGE('',*,*,#19341,.F.);
#26959=ORIENTED_EDGE('',*,*,#19332,.F.);
#26960=ORIENTED_EDGE('',*,*,#19336,.F.);
#26961=ORIENTED_EDGE('',*,*,#19339,.F.);
#26962=ORIENTED_EDGE('',*,*,#19342,.F.);
#26963=ORIENTED_EDGE('',*,*,#19343,.T.);
#26964=ORIENTED_EDGE('',*,*,#19344,.T.);
#26965=ORIENTED_EDGE('',*,*,#19345,.F.);
#26966=ORIENTED_EDGE('',*,*,#19346,.F.);
#26967=ORIENTED_EDGE('',*,*,#19347,.T.);
#26968=ORIENTED_EDGE('',*,*,#19348,.T.);
#26969=ORIENTED_EDGE('',*,*,#19343,.F.);
#26970=ORIENTED_EDGE('',*,*,#19349,.F.);
#26971=ORIENTED_EDGE('',*,*,#19350,.T.);
#26972=ORIENTED_EDGE('',*,*,#19351,.T.);
#26973=ORIENTED_EDGE('',*,*,#19347,.F.);
#26974=ORIENTED_EDGE('',*,*,#19352,.F.);
#26975=ORIENTED_EDGE('',*,*,#19345,.T.);
#26976=ORIENTED_EDGE('',*,*,#19353,.T.);
#26977=ORIENTED_EDGE('',*,*,#19350,.F.);
#26978=ORIENTED_EDGE('',*,*,#19353,.F.);
#26979=ORIENTED_EDGE('',*,*,#19344,.F.);
#26980=ORIENTED_EDGE('',*,*,#19348,.F.);
#26981=ORIENTED_EDGE('',*,*,#19351,.F.);
#26982=ORIENTED_EDGE('',*,*,#19354,.F.);
#26983=ORIENTED_EDGE('',*,*,#19355,.T.);
#26984=ORIENTED_EDGE('',*,*,#19356,.T.);
#26985=ORIENTED_EDGE('',*,*,#19357,.F.);
#26986=ORIENTED_EDGE('',*,*,#19358,.F.);
#26987=ORIENTED_EDGE('',*,*,#19359,.T.);
#26988=ORIENTED_EDGE('',*,*,#19360,.T.);
#26989=ORIENTED_EDGE('',*,*,#19355,.F.);
#26990=ORIENTED_EDGE('',*,*,#19361,.F.);
#26991=ORIENTED_EDGE('',*,*,#19362,.T.);
#26992=ORIENTED_EDGE('',*,*,#19363,.T.);
#26993=ORIENTED_EDGE('',*,*,#19359,.F.);
#26994=ORIENTED_EDGE('',*,*,#19364,.F.);
#26995=ORIENTED_EDGE('',*,*,#19357,.T.);
#26996=ORIENTED_EDGE('',*,*,#19365,.T.);
#26997=ORIENTED_EDGE('',*,*,#19362,.F.);
#26998=ORIENTED_EDGE('',*,*,#19365,.F.);
#26999=ORIENTED_EDGE('',*,*,#19356,.F.);
#27000=ORIENTED_EDGE('',*,*,#19360,.F.);
#27001=ORIENTED_EDGE('',*,*,#19363,.F.);
#27002=ORIENTED_EDGE('',*,*,#19366,.F.);
#27003=ORIENTED_EDGE('',*,*,#19367,.T.);
#27004=ORIENTED_EDGE('',*,*,#19368,.T.);
#27005=ORIENTED_EDGE('',*,*,#19369,.F.);
#27006=ORIENTED_EDGE('',*,*,#19370,.F.);
#27007=ORIENTED_EDGE('',*,*,#19371,.T.);
#27008=ORIENTED_EDGE('',*,*,#19372,.T.);
#27009=ORIENTED_EDGE('',*,*,#19367,.F.);
#27010=ORIENTED_EDGE('',*,*,#19373,.F.);
#27011=ORIENTED_EDGE('',*,*,#19374,.T.);
#27012=ORIENTED_EDGE('',*,*,#19375,.T.);
#27013=ORIENTED_EDGE('',*,*,#19371,.F.);
#27014=ORIENTED_EDGE('',*,*,#19376,.F.);
#27015=ORIENTED_EDGE('',*,*,#19369,.T.);
#27016=ORIENTED_EDGE('',*,*,#19377,.T.);
#27017=ORIENTED_EDGE('',*,*,#19374,.F.);
#27018=ORIENTED_EDGE('',*,*,#19377,.F.);
#27019=ORIENTED_EDGE('',*,*,#19368,.F.);
#27020=ORIENTED_EDGE('',*,*,#19372,.F.);
#27021=ORIENTED_EDGE('',*,*,#19375,.F.);
#27022=ORIENTED_EDGE('',*,*,#19378,.F.);
#27023=ORIENTED_EDGE('',*,*,#19379,.T.);
#27024=ORIENTED_EDGE('',*,*,#19380,.T.);
#27025=ORIENTED_EDGE('',*,*,#19381,.F.);
#27026=ORIENTED_EDGE('',*,*,#19382,.F.);
#27027=ORIENTED_EDGE('',*,*,#19383,.T.);
#27028=ORIENTED_EDGE('',*,*,#19384,.T.);
#27029=ORIENTED_EDGE('',*,*,#19379,.F.);
#27030=ORIENTED_EDGE('',*,*,#19385,.F.);
#27031=ORIENTED_EDGE('',*,*,#19386,.T.);
#27032=ORIENTED_EDGE('',*,*,#19387,.T.);
#27033=ORIENTED_EDGE('',*,*,#19383,.F.);
#27034=ORIENTED_EDGE('',*,*,#19388,.F.);
#27035=ORIENTED_EDGE('',*,*,#19381,.T.);
#27036=ORIENTED_EDGE('',*,*,#19389,.T.);
#27037=ORIENTED_EDGE('',*,*,#19386,.F.);
#27038=ORIENTED_EDGE('',*,*,#19389,.F.);
#27039=ORIENTED_EDGE('',*,*,#19380,.F.);
#27040=ORIENTED_EDGE('',*,*,#19384,.F.);
#27041=ORIENTED_EDGE('',*,*,#19387,.F.);
#27042=ORIENTED_EDGE('',*,*,#19390,.F.);
#27043=ORIENTED_EDGE('',*,*,#19391,.T.);
#27044=ORIENTED_EDGE('',*,*,#19392,.T.);
#27045=ORIENTED_EDGE('',*,*,#19393,.F.);
#27046=ORIENTED_EDGE('',*,*,#19394,.F.);
#27047=ORIENTED_EDGE('',*,*,#19395,.T.);
#27048=ORIENTED_EDGE('',*,*,#19396,.T.);
#27049=ORIENTED_EDGE('',*,*,#19391,.F.);
#27050=ORIENTED_EDGE('',*,*,#19397,.F.);
#27051=ORIENTED_EDGE('',*,*,#19398,.T.);
#27052=ORIENTED_EDGE('',*,*,#19399,.T.);
#27053=ORIENTED_EDGE('',*,*,#19395,.F.);
#27054=ORIENTED_EDGE('',*,*,#19400,.F.);
#27055=ORIENTED_EDGE('',*,*,#19393,.T.);
#27056=ORIENTED_EDGE('',*,*,#19401,.T.);
#27057=ORIENTED_EDGE('',*,*,#19398,.F.);
#27058=ORIENTED_EDGE('',*,*,#19401,.F.);
#27059=ORIENTED_EDGE('',*,*,#19392,.F.);
#27060=ORIENTED_EDGE('',*,*,#19396,.F.);
#27061=ORIENTED_EDGE('',*,*,#19399,.F.);
#27062=ORIENTED_EDGE('',*,*,#19402,.F.);
#27063=ORIENTED_EDGE('',*,*,#19403,.T.);
#27064=ORIENTED_EDGE('',*,*,#19404,.T.);
#27065=ORIENTED_EDGE('',*,*,#19405,.F.);
#27066=ORIENTED_EDGE('',*,*,#19406,.F.);
#27067=ORIENTED_EDGE('',*,*,#19407,.T.);
#27068=ORIENTED_EDGE('',*,*,#19408,.T.);
#27069=ORIENTED_EDGE('',*,*,#19403,.F.);
#27070=ORIENTED_EDGE('',*,*,#19409,.F.);
#27071=ORIENTED_EDGE('',*,*,#19410,.T.);
#27072=ORIENTED_EDGE('',*,*,#19411,.T.);
#27073=ORIENTED_EDGE('',*,*,#19407,.F.);
#27074=ORIENTED_EDGE('',*,*,#19412,.F.);
#27075=ORIENTED_EDGE('',*,*,#19405,.T.);
#27076=ORIENTED_EDGE('',*,*,#19413,.T.);
#27077=ORIENTED_EDGE('',*,*,#19410,.F.);
#27078=ORIENTED_EDGE('',*,*,#19413,.F.);
#27079=ORIENTED_EDGE('',*,*,#19404,.F.);
#27080=ORIENTED_EDGE('',*,*,#19408,.F.);
#27081=ORIENTED_EDGE('',*,*,#19411,.F.);
#27082=ORIENTED_EDGE('',*,*,#19414,.F.);
#27083=ORIENTED_EDGE('',*,*,#19415,.T.);
#27084=ORIENTED_EDGE('',*,*,#19416,.F.);
#27085=ORIENTED_EDGE('',*,*,#19415,.F.);
#27086=ORIENTED_EDGE('',*,*,#19417,.F.);
#27087=ORIENTED_EDGE('',*,*,#19418,.T.);
#27088=ORIENTED_EDGE('',*,*,#19419,.F.);
#27089=ORIENTED_EDGE('',*,*,#19418,.F.);
#27090=ORIENTED_EDGE('',*,*,#19420,.F.);
#27091=ORIENTED_EDGE('',*,*,#19421,.T.);
#27092=ORIENTED_EDGE('',*,*,#19422,.F.);
#27093=ORIENTED_EDGE('',*,*,#19423,.F.);
#27094=ORIENTED_EDGE('',*,*,#19414,.T.);
#27095=ORIENTED_EDGE('',*,*,#19417,.T.);
#27096=ORIENTED_EDGE('',*,*,#19424,.F.);
#27097=ORIENTED_EDGE('',*,*,#19423,.T.);
#27098=ORIENTED_EDGE('',*,*,#19425,.F.);
#27099=ORIENTED_EDGE('',*,*,#19426,.F.);
#27100=ORIENTED_EDGE('',*,*,#19427,.F.);
#27101=ORIENTED_EDGE('',*,*,#19426,.T.);
#27102=ORIENTED_EDGE('',*,*,#19428,.F.);
#27103=ORIENTED_EDGE('',*,*,#19429,.F.);
#27104=ORIENTED_EDGE('',*,*,#19416,.T.);
#27105=ORIENTED_EDGE('',*,*,#19419,.T.);
#27106=ORIENTED_EDGE('',*,*,#19430,.F.);
#27107=ORIENTED_EDGE('',*,*,#19429,.T.);
#27108=ORIENTED_EDGE('',*,*,#19431,.F.);
#27109=ORIENTED_EDGE('',*,*,#19432,.F.);
#27110=ORIENTED_EDGE('',*,*,#19433,.F.);
#27111=ORIENTED_EDGE('',*,*,#19432,.T.);
#27112=ORIENTED_EDGE('',*,*,#19434,.F.);
#27113=ORIENTED_EDGE('',*,*,#19435,.F.);
#27114=ORIENTED_EDGE('',*,*,#19436,.F.);
#27115=ORIENTED_EDGE('',*,*,#19435,.T.);
#27116=ORIENTED_EDGE('',*,*,#19437,.F.);
#27117=ORIENTED_EDGE('',*,*,#19438,.F.);
#27118=ORIENTED_EDGE('',*,*,#19439,.F.);
#27119=ORIENTED_EDGE('',*,*,#19438,.T.);
#27120=ORIENTED_EDGE('',*,*,#19440,.F.);
#27121=ORIENTED_EDGE('',*,*,#19441,.F.);
#27122=ORIENTED_EDGE('',*,*,#19402,.T.);
#27123=ORIENTED_EDGE('',*,*,#19412,.T.);
#27124=ORIENTED_EDGE('',*,*,#19409,.T.);
#27125=ORIENTED_EDGE('',*,*,#19406,.T.);
#27126=ORIENTED_EDGE('',*,*,#19390,.T.);
#27127=ORIENTED_EDGE('',*,*,#19400,.T.);
#27128=ORIENTED_EDGE('',*,*,#19397,.T.);
#27129=ORIENTED_EDGE('',*,*,#19394,.T.);
#27130=ORIENTED_EDGE('',*,*,#19378,.T.);
#27131=ORIENTED_EDGE('',*,*,#19388,.T.);
#27132=ORIENTED_EDGE('',*,*,#19385,.T.);
#27133=ORIENTED_EDGE('',*,*,#19382,.T.);
#27134=ORIENTED_EDGE('',*,*,#19366,.T.);
#27135=ORIENTED_EDGE('',*,*,#19376,.T.);
#27136=ORIENTED_EDGE('',*,*,#19373,.T.);
#27137=ORIENTED_EDGE('',*,*,#19370,.T.);
#27138=ORIENTED_EDGE('',*,*,#19354,.T.);
#27139=ORIENTED_EDGE('',*,*,#19364,.T.);
#27140=ORIENTED_EDGE('',*,*,#19361,.T.);
#27141=ORIENTED_EDGE('',*,*,#19358,.T.);
#27142=ORIENTED_EDGE('',*,*,#19342,.T.);
#27143=ORIENTED_EDGE('',*,*,#19352,.T.);
#27144=ORIENTED_EDGE('',*,*,#19349,.T.);
#27145=ORIENTED_EDGE('',*,*,#19346,.T.);
#27146=ORIENTED_EDGE('',*,*,#19330,.T.);
#27147=ORIENTED_EDGE('',*,*,#19340,.T.);
#27148=ORIENTED_EDGE('',*,*,#19337,.T.);
#27149=ORIENTED_EDGE('',*,*,#19334,.T.);
#27150=ORIENTED_EDGE('',*,*,#19318,.T.);
#27151=ORIENTED_EDGE('',*,*,#19328,.T.);
#27152=ORIENTED_EDGE('',*,*,#19325,.T.);
#27153=ORIENTED_EDGE('',*,*,#19322,.T.);
#27154=ORIENTED_EDGE('',*,*,#19306,.T.);
#27155=ORIENTED_EDGE('',*,*,#19316,.T.);
#27156=ORIENTED_EDGE('',*,*,#19313,.T.);
#27157=ORIENTED_EDGE('',*,*,#19310,.T.);
#27158=ORIENTED_EDGE('',*,*,#19294,.T.);
#27159=ORIENTED_EDGE('',*,*,#19304,.T.);
#27160=ORIENTED_EDGE('',*,*,#19301,.T.);
#27161=ORIENTED_EDGE('',*,*,#19298,.T.);
#27162=ORIENTED_EDGE('',*,*,#19282,.T.);
#27163=ORIENTED_EDGE('',*,*,#19292,.T.);
#27164=ORIENTED_EDGE('',*,*,#19289,.T.);
#27165=ORIENTED_EDGE('',*,*,#19286,.T.);
#27166=ORIENTED_EDGE('',*,*,#19442,.F.);
#27167=ORIENTED_EDGE('',*,*,#19441,.T.);
#27168=ORIENTED_EDGE('',*,*,#19443,.F.);
#27169=ORIENTED_EDGE('',*,*,#19421,.F.);
#27170=ORIENTED_EDGE('',*,*,#19443,.T.);
#27171=ORIENTED_EDGE('',*,*,#19440,.T.);
#27172=ORIENTED_EDGE('',*,*,#19437,.T.);
#27173=ORIENTED_EDGE('',*,*,#19434,.T.);
#27174=ORIENTED_EDGE('',*,*,#19431,.T.);
#27175=ORIENTED_EDGE('',*,*,#19428,.T.);
#27176=ORIENTED_EDGE('',*,*,#19425,.T.);
#27177=ORIENTED_EDGE('',*,*,#19422,.T.);
#27178=ORIENTED_EDGE('',*,*,#19442,.T.);
#27179=ORIENTED_EDGE('',*,*,#19420,.T.);
#27180=ORIENTED_EDGE('',*,*,#19424,.T.);
#27181=ORIENTED_EDGE('',*,*,#19427,.T.);
#27182=ORIENTED_EDGE('',*,*,#19430,.T.);
#27183=ORIENTED_EDGE('',*,*,#19433,.T.);
#27184=ORIENTED_EDGE('',*,*,#19436,.T.);
#27185=ORIENTED_EDGE('',*,*,#19439,.T.);
#27186=ORIENTED_EDGE('',*,*,#19444,.T.);
#27187=ORIENTED_EDGE('',*,*,#19445,.T.);
#27188=ORIENTED_EDGE('',*,*,#19446,.T.);
#27189=ORIENTED_EDGE('',*,*,#19447,.T.);
#27190=ORIENTED_EDGE('',*,*,#19445,.F.);
#27191=ORIENTED_EDGE('',*,*,#19448,.T.);
#27192=ORIENTED_EDGE('',*,*,#19449,.F.);
#27193=ORIENTED_EDGE('',*,*,#19450,.T.);
#27194=ORIENTED_EDGE('',*,*,#19451,.T.);
#27195=ORIENTED_EDGE('',*,*,#19452,.T.);
#27196=ORIENTED_EDGE('',*,*,#19453,.T.);
#27197=ORIENTED_EDGE('',*,*,#19454,.T.);
#27198=ORIENTED_EDGE('',*,*,#19455,.T.);
#27199=ORIENTED_EDGE('',*,*,#19456,.T.);
#27200=ORIENTED_EDGE('',*,*,#19457,.T.);
#27201=ORIENTED_EDGE('',*,*,#19458,.T.);
#27202=ORIENTED_EDGE('',*,*,#19459,.T.);
#27203=ORIENTED_EDGE('',*,*,#19460,.T.);
#27204=ORIENTED_EDGE('',*,*,#19461,.T.);
#27205=ORIENTED_EDGE('',*,*,#19462,.T.);
#27206=ORIENTED_EDGE('',*,*,#19463,.T.);
#27207=ORIENTED_EDGE('',*,*,#19449,.T.);
#27208=ORIENTED_EDGE('',*,*,#19464,.T.);
#27209=ORIENTED_EDGE('',*,*,#19465,.T.);
#27210=ORIENTED_EDGE('',*,*,#19446,.F.);
#27211=ORIENTED_EDGE('',*,*,#19454,.F.);
#27212=ORIENTED_EDGE('',*,*,#19466,.T.);
#27213=ORIENTED_EDGE('',*,*,#19467,.F.);
#27214=ORIENTED_EDGE('',*,*,#19468,.F.);
#27215=ORIENTED_EDGE('',*,*,#19450,.F.);
#27216=ORIENTED_EDGE('',*,*,#19463,.F.);
#27217=ORIENTED_EDGE('',*,*,#19469,.T.);
#27218=ORIENTED_EDGE('',*,*,#19470,.T.);
#27219=ORIENTED_EDGE('',*,*,#19471,.T.);
#27220=ORIENTED_EDGE('',*,*,#19464,.F.);
#27221=ORIENTED_EDGE('',*,*,#19448,.F.);
#27222=ORIENTED_EDGE('',*,*,#19444,.F.);
#27223=ORIENTED_EDGE('',*,*,#19472,.T.);
#27224=ORIENTED_EDGE('',*,*,#19473,.T.);
#27225=ORIENTED_EDGE('',*,*,#19474,.T.);
#27226=ORIENTED_EDGE('',*,*,#19465,.F.);
#27227=ORIENTED_EDGE('',*,*,#19471,.F.);
#27228=ORIENTED_EDGE('',*,*,#19475,.T.);
#27229=ORIENTED_EDGE('',*,*,#19469,.F.);
#27230=ORIENTED_EDGE('',*,*,#19470,.F.);
#27231=ORIENTED_EDGE('',*,*,#19475,.F.);
#27232=ORIENTED_EDGE('',*,*,#19476,.F.);
#27233=ORIENTED_EDGE('',*,*,#19447,.F.);
#27234=ORIENTED_EDGE('',*,*,#19474,.F.);
#27235=ORIENTED_EDGE('',*,*,#19477,.T.);
#27236=ORIENTED_EDGE('',*,*,#19472,.F.);
#27237=ORIENTED_EDGE('',*,*,#19473,.F.);
#27238=ORIENTED_EDGE('',*,*,#19477,.F.);
#27239=ORIENTED_EDGE('',*,*,#19478,.F.);
#27240=ORIENTED_EDGE('',*,*,#19476,.T.);
#27241=ORIENTED_EDGE('',*,*,#19479,.T.);
#27242=ORIENTED_EDGE('',*,*,#19480,.F.);
#27243=ORIENTED_EDGE('',*,*,#19481,.F.);
#27244=ORIENTED_EDGE('',*,*,#19482,.F.);
#27245=ORIENTED_EDGE('',*,*,#19479,.F.);
#27246=ORIENTED_EDGE('',*,*,#19478,.T.);
#27247=ORIENTED_EDGE('',*,*,#19483,.T.);
#27248=ORIENTED_EDGE('',*,*,#19484,.F.);
#27249=ORIENTED_EDGE('',*,*,#19485,.F.);
#27250=ORIENTED_EDGE('',*,*,#19486,.F.);
#27251=ORIENTED_EDGE('',*,*,#19483,.F.);
#27252=ORIENTED_EDGE('',*,*,#19481,.T.);
#27253=ORIENTED_EDGE('',*,*,#19487,.T.);
#27254=ORIENTED_EDGE('',*,*,#19488,.T.);
#27255=ORIENTED_EDGE('',*,*,#19467,.T.);
#27256=ORIENTED_EDGE('',*,*,#19489,.F.);
#27257=ORIENTED_EDGE('',*,*,#19490,.T.);
#27258=ORIENTED_EDGE('',*,*,#19485,.T.);
#27259=ORIENTED_EDGE('',*,*,#19491,.T.);
#27260=ORIENTED_EDGE('',*,*,#19492,.F.);
#27261=ORIENTED_EDGE('',*,*,#19493,.T.);
#27262=ORIENTED_EDGE('',*,*,#19459,.F.);
#27263=ORIENTED_EDGE('',*,*,#19494,.F.);
#27264=ORIENTED_EDGE('',*,*,#19495,.F.);
#27265=ORIENTED_EDGE('',*,*,#19496,.F.);
#27266=ORIENTED_EDGE('',*,*,#19497,.T.);
#27267=ORIENTED_EDGE('',*,*,#19460,.F.);
#27268=ORIENTED_EDGE('',*,*,#19493,.F.);
#27269=ORIENTED_EDGE('',*,*,#19498,.F.);
#27270=ORIENTED_EDGE('',*,*,#19499,.F.);
#27271=ORIENTED_EDGE('',*,*,#19500,.T.);
#27272=ORIENTED_EDGE('',*,*,#19461,.F.);
#27273=ORIENTED_EDGE('',*,*,#19497,.F.);
#27274=ORIENTED_EDGE('',*,*,#19501,.F.);
#27275=ORIENTED_EDGE('',*,*,#19494,.T.);
#27276=ORIENTED_EDGE('',*,*,#19462,.F.);
#27277=ORIENTED_EDGE('',*,*,#19500,.F.);
#27278=ORIENTED_EDGE('',*,*,#19502,.F.);
#27279=ORIENTED_EDGE('',*,*,#19503,.T.);
#27280=ORIENTED_EDGE('',*,*,#19455,.F.);
#27281=ORIENTED_EDGE('',*,*,#19504,.F.);
#27282=ORIENTED_EDGE('',*,*,#19505,.F.);
#27283=ORIENTED_EDGE('',*,*,#19506,.F.);
#27284=ORIENTED_EDGE('',*,*,#19507,.T.);
#27285=ORIENTED_EDGE('',*,*,#19456,.F.);
#27286=ORIENTED_EDGE('',*,*,#19503,.F.);
#27287=ORIENTED_EDGE('',*,*,#19508,.F.);
#27288=ORIENTED_EDGE('',*,*,#19509,.F.);
#27289=ORIENTED_EDGE('',*,*,#19510,.T.);
#27290=ORIENTED_EDGE('',*,*,#19457,.F.);
#27291=ORIENTED_EDGE('',*,*,#19507,.F.);
#27292=ORIENTED_EDGE('',*,*,#19511,.F.);
#27293=ORIENTED_EDGE('',*,*,#19504,.T.);
#27294=ORIENTED_EDGE('',*,*,#19458,.F.);
#27295=ORIENTED_EDGE('',*,*,#19510,.F.);
#27296=ORIENTED_EDGE('',*,*,#19480,.T.);
#27297=ORIENTED_EDGE('',*,*,#19482,.T.);
#27298=ORIENTED_EDGE('',*,*,#19491,.F.);
#27299=ORIENTED_EDGE('',*,*,#19484,.T.);
#27300=ORIENTED_EDGE('',*,*,#19486,.T.);
#27301=ORIENTED_EDGE('',*,*,#19490,.F.);
#27302=ORIENTED_EDGE('',*,*,#19512,.F.);
#27303=ORIENTED_EDGE('',*,*,#19513,.F.);
#27304=ORIENTED_EDGE('',*,*,#19508,.T.);
#27305=ORIENTED_EDGE('',*,*,#19502,.T.);
#27306=ORIENTED_EDGE('',*,*,#19511,.T.);
#27307=ORIENTED_EDGE('',*,*,#19509,.T.);
#27308=ORIENTED_EDGE('',*,*,#19506,.T.);
#27309=ORIENTED_EDGE('',*,*,#19514,.F.);
#27310=ORIENTED_EDGE('',*,*,#19498,.T.);
#27311=ORIENTED_EDGE('',*,*,#19492,.T.);
#27312=ORIENTED_EDGE('',*,*,#19501,.T.);
#27313=ORIENTED_EDGE('',*,*,#19499,.T.);
#27314=ORIENTED_EDGE('',*,*,#19496,.T.);
#27315=ORIENTED_EDGE('',*,*,#19515,.F.);
#27316=ORIENTED_EDGE('',*,*,#19516,.F.);
#27317=ORIENTED_EDGE('',*,*,#19487,.F.);
#27318=ORIENTED_EDGE('',*,*,#19512,.T.);
#27319=ORIENTED_EDGE('',*,*,#19489,.T.);
#27320=ORIENTED_EDGE('',*,*,#19517,.T.);
#27321=ORIENTED_EDGE('',*,*,#19518,.F.);
#27322=ORIENTED_EDGE('',*,*,#19516,.T.);
#27323=ORIENTED_EDGE('',*,*,#19519,.T.);
#27324=ORIENTED_EDGE('',*,*,#19520,.T.);
#27325=ORIENTED_EDGE('',*,*,#19488,.F.);
#27326=ORIENTED_EDGE('',*,*,#19495,.T.);
#27327=ORIENTED_EDGE('',*,*,#19514,.T.);
#27328=ORIENTED_EDGE('',*,*,#19505,.T.);
#27329=ORIENTED_EDGE('',*,*,#19513,.T.);
#27330=ORIENTED_EDGE('',*,*,#19518,.T.);
#27331=ORIENTED_EDGE('',*,*,#19521,.T.);
#27332=ORIENTED_EDGE('',*,*,#19519,.F.);
#27333=ORIENTED_EDGE('',*,*,#19515,.T.);
#27334=ORIENTED_EDGE('',*,*,#19521,.F.);
#27335=ORIENTED_EDGE('',*,*,#19522,.F.);
#27336=ORIENTED_EDGE('',*,*,#19452,.F.);
#27337=ORIENTED_EDGE('',*,*,#19523,.T.);
#27338=ORIENTED_EDGE('',*,*,#19517,.F.);
#27339=ORIENTED_EDGE('',*,*,#19466,.F.);
#27340=ORIENTED_EDGE('',*,*,#19453,.F.);
#27341=ORIENTED_EDGE('',*,*,#19522,.T.);
#27342=ORIENTED_EDGE('',*,*,#19520,.F.);
#27343=ORIENTED_EDGE('',*,*,#19523,.F.);
#27344=ORIENTED_EDGE('',*,*,#19451,.F.);
#27345=ORIENTED_EDGE('',*,*,#19468,.T.);
#27346=ORIENTED_EDGE('',*,*,#19524,.F.);
#27347=ORIENTED_EDGE('',*,*,#19525,.T.);
#27348=ORIENTED_EDGE('',*,*,#19526,.T.);
#27349=ORIENTED_EDGE('',*,*,#19527,.T.);
#27350=ORIENTED_EDGE('',*,*,#19528,.F.);
#27351=ORIENTED_EDGE('',*,*,#19529,.T.);
#27352=ORIENTED_EDGE('',*,*,#19524,.T.);
#27353=ORIENTED_EDGE('',*,*,#19530,.T.);
#27354=ORIENTED_EDGE('',*,*,#19531,.F.);
#27355=ORIENTED_EDGE('',*,*,#19532,.T.);
#27356=ORIENTED_EDGE('',*,*,#19528,.T.);
#27357=ORIENTED_EDGE('',*,*,#19533,.T.);
#27358=ORIENTED_EDGE('',*,*,#19534,.F.);
#27359=ORIENTED_EDGE('',*,*,#19535,.T.);
#27360=ORIENTED_EDGE('',*,*,#19536,.T.);
#27361=ORIENTED_EDGE('',*,*,#19531,.T.);
#27362=ORIENTED_EDGE('',*,*,#19537,.T.);
#27363=ORIENTED_EDGE('',*,*,#19538,.T.);
#27364=ORIENTED_EDGE('',*,*,#19539,.F.);
#27365=ORIENTED_EDGE('',*,*,#19540,.T.);
#27366=ORIENTED_EDGE('',*,*,#19541,.T.);
#27367=ORIENTED_EDGE('',*,*,#19534,.T.);
#27368=ORIENTED_EDGE('',*,*,#19542,.T.);
#27369=ORIENTED_EDGE('',*,*,#19543,.F.);
#27370=ORIENTED_EDGE('',*,*,#19544,.T.);
#27371=ORIENTED_EDGE('',*,*,#19539,.T.);
#27372=ORIENTED_EDGE('',*,*,#19545,.T.);
#27373=ORIENTED_EDGE('',*,*,#19546,.F.);
#27374=ORIENTED_EDGE('',*,*,#19547,.T.);
#27375=ORIENTED_EDGE('',*,*,#19543,.T.);
#27376=ORIENTED_EDGE('',*,*,#19548,.T.);
#27377=ORIENTED_EDGE('',*,*,#19549,.T.);
#27378=ORIENTED_EDGE('',*,*,#19550,.F.);
#27379=ORIENTED_EDGE('',*,*,#19551,.T.);
#27380=ORIENTED_EDGE('',*,*,#19552,.T.);
#27381=ORIENTED_EDGE('',*,*,#19546,.T.);
#27382=ORIENTED_EDGE('',*,*,#19553,.T.);
#27383=ORIENTED_EDGE('',*,*,#19554,.T.);
#27384=ORIENTED_EDGE('',*,*,#19555,.F.);
#27385=ORIENTED_EDGE('',*,*,#19556,.T.);
#27386=ORIENTED_EDGE('',*,*,#19550,.T.);
#27387=ORIENTED_EDGE('',*,*,#19557,.T.);
#27388=ORIENTED_EDGE('',*,*,#19558,.F.);
#27389=ORIENTED_EDGE('',*,*,#19559,.F.);
#27390=ORIENTED_EDGE('',*,*,#19560,.F.);
#27391=ORIENTED_EDGE('',*,*,#19561,.T.);
#27392=ORIENTED_EDGE('',*,*,#19562,.F.);
#27393=ORIENTED_EDGE('',*,*,#19563,.F.);
#27394=ORIENTED_EDGE('',*,*,#19558,.T.);
#27395=ORIENTED_EDGE('',*,*,#19564,.T.);
#27396=ORIENTED_EDGE('',*,*,#19565,.F.);
#27397=ORIENTED_EDGE('',*,*,#19566,.F.);
#27398=ORIENTED_EDGE('',*,*,#19562,.T.);
#27399=ORIENTED_EDGE('',*,*,#19567,.T.);
#27400=ORIENTED_EDGE('',*,*,#19568,.F.);
#27401=ORIENTED_EDGE('',*,*,#19569,.F.);
#27402=ORIENTED_EDGE('',*,*,#19570,.F.);
#27403=ORIENTED_EDGE('',*,*,#19565,.T.);
#27404=ORIENTED_EDGE('',*,*,#19571,.T.);
#27405=ORIENTED_EDGE('',*,*,#19572,.F.);
#27406=ORIENTED_EDGE('',*,*,#19573,.F.);
#27407=ORIENTED_EDGE('',*,*,#19568,.T.);
#27408=ORIENTED_EDGE('',*,*,#19574,.T.);
#27409=ORIENTED_EDGE('',*,*,#19575,.F.);
#27410=ORIENTED_EDGE('',*,*,#19576,.F.);
#27411=ORIENTED_EDGE('',*,*,#19572,.T.);
#27412=ORIENTED_EDGE('',*,*,#19577,.T.);
#27413=ORIENTED_EDGE('',*,*,#19578,.F.);
#27414=ORIENTED_EDGE('',*,*,#19579,.F.);
#27415=ORIENTED_EDGE('',*,*,#19575,.T.);
#27416=ORIENTED_EDGE('',*,*,#19580,.T.);
#27417=ORIENTED_EDGE('',*,*,#19581,.T.);
#27418=ORIENTED_EDGE('',*,*,#19582,.F.);
#27419=ORIENTED_EDGE('',*,*,#19583,.F.);
#27420=ORIENTED_EDGE('',*,*,#19578,.T.);
#27421=ORIENTED_EDGE('',*,*,#19584,.T.);
#27422=ORIENTED_EDGE('',*,*,#19582,.T.);
#27423=ORIENTED_EDGE('',*,*,#19585,.T.);
#27424=ORIENTED_EDGE('',*,*,#19586,.F.);
#27425=ORIENTED_EDGE('',*,*,#19587,.F.);
#27426=ORIENTED_EDGE('',*,*,#19555,.T.);
#27427=ORIENTED_EDGE('',*,*,#19588,.T.);
#27428=ORIENTED_EDGE('',*,*,#19589,.F.);
#27429=ORIENTED_EDGE('',*,*,#19590,.T.);
#27430=ORIENTED_EDGE('',*,*,#19591,.F.);
#27431=ORIENTED_EDGE('',*,*,#19592,.T.);
#27432=ORIENTED_EDGE('',*,*,#19586,.T.);
#27433=ORIENTED_EDGE('',*,*,#19593,.T.);
#27434=ORIENTED_EDGE('',*,*,#19594,.F.);
#27435=ORIENTED_EDGE('',*,*,#19592,.F.);
#27436=ORIENTED_EDGE('',*,*,#19595,.F.);
#27437=ORIENTED_EDGE('',*,*,#19588,.F.);
#27438=ORIENTED_EDGE('',*,*,#19557,.F.);
#27439=ORIENTED_EDGE('',*,*,#19554,.F.);
#27440=ORIENTED_EDGE('',*,*,#19553,.F.);
#27441=ORIENTED_EDGE('',*,*,#19549,.F.);
#27442=ORIENTED_EDGE('',*,*,#19548,.F.);
#27443=ORIENTED_EDGE('',*,*,#19545,.F.);
#27444=ORIENTED_EDGE('',*,*,#19542,.F.);
#27445=ORIENTED_EDGE('',*,*,#19538,.F.);
#27446=ORIENTED_EDGE('',*,*,#19537,.F.);
#27447=ORIENTED_EDGE('',*,*,#19533,.F.);
#27448=ORIENTED_EDGE('',*,*,#19530,.F.);
#27449=ORIENTED_EDGE('',*,*,#19527,.F.);
#27450=ORIENTED_EDGE('',*,*,#19596,.F.);
#27451=ORIENTED_EDGE('',*,*,#19597,.T.);
#27452=ORIENTED_EDGE('',*,*,#19559,.T.);
#27453=ORIENTED_EDGE('',*,*,#19563,.T.);
#27454=ORIENTED_EDGE('',*,*,#19566,.T.);
#27455=ORIENTED_EDGE('',*,*,#19570,.T.);
#27456=ORIENTED_EDGE('',*,*,#19569,.T.);
#27457=ORIENTED_EDGE('',*,*,#19573,.T.);
#27458=ORIENTED_EDGE('',*,*,#19576,.T.);
#27459=ORIENTED_EDGE('',*,*,#19579,.T.);
#27460=ORIENTED_EDGE('',*,*,#19583,.T.);
#27461=ORIENTED_EDGE('',*,*,#19587,.T.);
#27462=ORIENTED_EDGE('',*,*,#19598,.T.);
#27463=ORIENTED_EDGE('',*,*,#19599,.T.);
#27464=ORIENTED_EDGE('',*,*,#19600,.T.);
#27465=ORIENTED_EDGE('',*,*,#19560,.T.);
#27466=ORIENTED_EDGE('',*,*,#19597,.F.);
#27467=ORIENTED_EDGE('',*,*,#19596,.T.);
#27468=ORIENTED_EDGE('',*,*,#19593,.F.);
#27469=ORIENTED_EDGE('',*,*,#19585,.F.);
#27470=ORIENTED_EDGE('',*,*,#19584,.F.);
#27471=ORIENTED_EDGE('',*,*,#19581,.F.);
#27472=ORIENTED_EDGE('',*,*,#19580,.F.);
#27473=ORIENTED_EDGE('',*,*,#19577,.F.);
#27474=ORIENTED_EDGE('',*,*,#19574,.F.);
#27475=ORIENTED_EDGE('',*,*,#19571,.F.);
#27476=ORIENTED_EDGE('',*,*,#19567,.F.);
#27477=ORIENTED_EDGE('',*,*,#19564,.F.);
#27478=ORIENTED_EDGE('',*,*,#19561,.F.);
#27479=ORIENTED_EDGE('',*,*,#19600,.F.);
#27480=ORIENTED_EDGE('',*,*,#19601,.T.);
#27481=ORIENTED_EDGE('',*,*,#19525,.F.);
#27482=ORIENTED_EDGE('',*,*,#19529,.F.);
#27483=ORIENTED_EDGE('',*,*,#19532,.F.);
#27484=ORIENTED_EDGE('',*,*,#19536,.F.);
#27485=ORIENTED_EDGE('',*,*,#19535,.F.);
#27486=ORIENTED_EDGE('',*,*,#19541,.F.);
#27487=ORIENTED_EDGE('',*,*,#19540,.F.);
#27488=ORIENTED_EDGE('',*,*,#19544,.F.);
#27489=ORIENTED_EDGE('',*,*,#19547,.F.);
#27490=ORIENTED_EDGE('',*,*,#19552,.F.);
#27491=ORIENTED_EDGE('',*,*,#19551,.F.);
#27492=ORIENTED_EDGE('',*,*,#19556,.F.);
#27493=ORIENTED_EDGE('',*,*,#19590,.F.);
#27494=ORIENTED_EDGE('',*,*,#19602,.F.);
#27495=ORIENTED_EDGE('',*,*,#19603,.F.);
#27496=ORIENTED_EDGE('',*,*,#19604,.F.);
#27497=ORIENTED_EDGE('',*,*,#19605,.F.);
#27498=ORIENTED_EDGE('',*,*,#19606,.F.);
#27499=ORIENTED_EDGE('',*,*,#19607,.F.);
#27500=ORIENTED_EDGE('',*,*,#19608,.F.);
#27501=ORIENTED_EDGE('',*,*,#19609,.F.);
#27502=ORIENTED_EDGE('',*,*,#19610,.F.);
#27503=ORIENTED_EDGE('',*,*,#19611,.F.);
#27504=ORIENTED_EDGE('',*,*,#19612,.F.);
#27505=ORIENTED_EDGE('',*,*,#19613,.F.);
#27506=ORIENTED_EDGE('',*,*,#19614,.F.);
#27507=ORIENTED_EDGE('',*,*,#19615,.F.);
#27508=ORIENTED_EDGE('',*,*,#19616,.F.);
#27509=ORIENTED_EDGE('',*,*,#19617,.F.);
#27510=ORIENTED_EDGE('',*,*,#19618,.F.);
#27511=ORIENTED_EDGE('',*,*,#19619,.F.);
#27512=ORIENTED_EDGE('',*,*,#19620,.T.);
#27513=ORIENTED_EDGE('',*,*,#19621,.F.);
#27514=ORIENTED_EDGE('',*,*,#19620,.F.);
#27515=ORIENTED_EDGE('',*,*,#19622,.F.);
#27516=ORIENTED_EDGE('',*,*,#19615,.T.);
#27517=ORIENTED_EDGE('',*,*,#19623,.F.);
#27518=ORIENTED_EDGE('',*,*,#19624,.F.);
#27519=ORIENTED_EDGE('',*,*,#19625,.F.);
#27520=ORIENTED_EDGE('',*,*,#19626,.F.);
#27521=ORIENTED_EDGE('',*,*,#19627,.F.);
#27522=ORIENTED_EDGE('',*,*,#19612,.T.);
#27523=ORIENTED_EDGE('',*,*,#19628,.F.);
#27524=ORIENTED_EDGE('',*,*,#19618,.T.);
#27525=ORIENTED_EDGE('',*,*,#19629,.F.);
#27526=ORIENTED_EDGE('',*,*,#19630,.F.);
#27527=ORIENTED_EDGE('',*,*,#19631,.F.);
#27528=ORIENTED_EDGE('',*,*,#19632,.F.);
#27529=ORIENTED_EDGE('',*,*,#19633,.F.);
#27530=ORIENTED_EDGE('',*,*,#19609,.T.);
#27531=ORIENTED_EDGE('',*,*,#19634,.F.);
#27532=ORIENTED_EDGE('',*,*,#19603,.T.);
#27533=ORIENTED_EDGE('',*,*,#19635,.F.);
#27534=ORIENTED_EDGE('',*,*,#19636,.F.);
#27535=ORIENTED_EDGE('',*,*,#19637,.F.);
#27536=ORIENTED_EDGE('',*,*,#19638,.F.);
#27537=ORIENTED_EDGE('',*,*,#19639,.F.);
#27538=ORIENTED_EDGE('',*,*,#19606,.T.);
#27539=ORIENTED_EDGE('',*,*,#19604,.T.);
#27540=ORIENTED_EDGE('',*,*,#19634,.T.);
#27541=ORIENTED_EDGE('',*,*,#19640,.F.);
#27542=ORIENTED_EDGE('',*,*,#19635,.T.);
#27543=ORIENTED_EDGE('',*,*,#19602,.T.);
#27544=ORIENTED_EDGE('',*,*,#19641,.T.);
#27545=ORIENTED_EDGE('',*,*,#19642,.T.);
#27546=ORIENTED_EDGE('',*,*,#19643,.F.);
#27547=ORIENTED_EDGE('',*,*,#19619,.T.);
#27548=ORIENTED_EDGE('',*,*,#19628,.T.);
#27549=ORIENTED_EDGE('',*,*,#19644,.F.);
#27550=ORIENTED_EDGE('',*,*,#19629,.T.);
#27551=ORIENTED_EDGE('',*,*,#19617,.T.);
#27552=ORIENTED_EDGE('',*,*,#19645,.T.);
#27553=ORIENTED_EDGE('',*,*,#19646,.T.);
#27554=ORIENTED_EDGE('',*,*,#19641,.F.);
#27555=ORIENTED_EDGE('',*,*,#19616,.T.);
#27556=ORIENTED_EDGE('',*,*,#19622,.T.);
#27557=ORIENTED_EDGE('',*,*,#19647,.F.);
#27558=ORIENTED_EDGE('',*,*,#19623,.T.);
#27559=ORIENTED_EDGE('',*,*,#19614,.T.);
#27560=ORIENTED_EDGE('',*,*,#19648,.T.);
#27561=ORIENTED_EDGE('',*,*,#19649,.T.);
#27562=ORIENTED_EDGE('',*,*,#19645,.F.);
#27563=ORIENTED_EDGE('',*,*,#19624,.T.);
#27564=ORIENTED_EDGE('',*,*,#19647,.T.);
#27565=ORIENTED_EDGE('',*,*,#19630,.T.);
#27566=ORIENTED_EDGE('',*,*,#19644,.T.);
#27567=ORIENTED_EDGE('',*,*,#19626,.T.);
#27568=ORIENTED_EDGE('',*,*,#19650,.T.);
#27569=ORIENTED_EDGE('',*,*,#19636,.T.);
#27570=ORIENTED_EDGE('',*,*,#19640,.T.);
#27571=ORIENTED_EDGE('',*,*,#19632,.T.);
#27572=ORIENTED_EDGE('',*,*,#19651,.T.);
#27573=ORIENTED_EDGE('',*,*,#19638,.T.);
#27574=ORIENTED_EDGE('',*,*,#19652,.T.);
#27575=ORIENTED_EDGE('',*,*,#19653,.F.);
#27576=ORIENTED_EDGE('',*,*,#19654,.F.);
#27577=ORIENTED_EDGE('',*,*,#19655,.F.);
#27578=ORIENTED_EDGE('',*,*,#19656,.F.);
#27579=ORIENTED_EDGE('',*,*,#19649,.F.);
#27580=ORIENTED_EDGE('',*,*,#19657,.F.);
#27581=ORIENTED_EDGE('',*,*,#19646,.F.);
#27582=ORIENTED_EDGE('',*,*,#19658,.F.);
#27583=ORIENTED_EDGE('',*,*,#19642,.F.);
#27584=ORIENTED_EDGE('',*,*,#19659,.F.);
#27585=ORIENTED_EDGE('',*,*,#19660,.F.);
#27586=ORIENTED_EDGE('',*,*,#19661,.F.);
#27587=ORIENTED_EDGE('',*,*,#19662,.T.);
#27588=ORIENTED_EDGE('',*,*,#19658,.T.);
#27589=ORIENTED_EDGE('',*,*,#19657,.T.);
#27590=ORIENTED_EDGE('',*,*,#19656,.T.);
#27591=ORIENTED_EDGE('',*,*,#19654,.T.);
#27592=ORIENTED_EDGE('',*,*,#19661,.T.);
#27593=ORIENTED_EDGE('',*,*,#19659,.T.);
#27594=ORIENTED_EDGE('',*,*,#19662,.F.);
#27595=ORIENTED_EDGE('',*,*,#19608,.T.);
#27596=ORIENTED_EDGE('',*,*,#19663,.T.);
#27597=ORIENTED_EDGE('',*,*,#19653,.T.);
#27598=ORIENTED_EDGE('',*,*,#19664,.F.);
#27599=ORIENTED_EDGE('',*,*,#19610,.T.);
#27600=ORIENTED_EDGE('',*,*,#19633,.T.);
#27601=ORIENTED_EDGE('',*,*,#19651,.F.);
#27602=ORIENTED_EDGE('',*,*,#19631,.T.);
#27603=ORIENTED_EDGE('',*,*,#19605,.T.);
#27604=ORIENTED_EDGE('',*,*,#19643,.T.);
#27605=ORIENTED_EDGE('',*,*,#19660,.T.);
#27606=ORIENTED_EDGE('',*,*,#19663,.F.);
#27607=ORIENTED_EDGE('',*,*,#19607,.T.);
#27608=ORIENTED_EDGE('',*,*,#19639,.T.);
#27609=ORIENTED_EDGE('',*,*,#19652,.F.);
#27610=ORIENTED_EDGE('',*,*,#19637,.T.);
#27611=ORIENTED_EDGE('',*,*,#19611,.T.);
#27612=ORIENTED_EDGE('',*,*,#19664,.T.);
#27613=ORIENTED_EDGE('',*,*,#19655,.T.);
#27614=ORIENTED_EDGE('',*,*,#19648,.F.);
#27615=ORIENTED_EDGE('',*,*,#19613,.T.);
#27616=ORIENTED_EDGE('',*,*,#19627,.T.);
#27617=ORIENTED_EDGE('',*,*,#19650,.F.);
#27618=ORIENTED_EDGE('',*,*,#19625,.T.);
#27619=ORIENTED_EDGE('',*,*,#19665,.F.);
#27620=ORIENTED_EDGE('',*,*,#19598,.F.);
#27621=ORIENTED_EDGE('',*,*,#19526,.F.);
#27622=ORIENTED_EDGE('',*,*,#19601,.F.);
#27623=ORIENTED_EDGE('',*,*,#19599,.F.);
#27624=ORIENTED_EDGE('',*,*,#19666,.T.);
#27625=ORIENTED_EDGE('',*,*,#19665,.T.);
#27626=ORIENTED_EDGE('',*,*,#19666,.F.);
#27627=ORIENTED_EDGE('',*,*,#19591,.T.);
#27628=ORIENTED_EDGE('',*,*,#19667,.T.);
#27629=ORIENTED_EDGE('',*,*,#19668,.F.);
#27630=ORIENTED_EDGE('',*,*,#19667,.F.);
#27631=ORIENTED_EDGE('',*,*,#19594,.T.);
#27632=ORIENTED_EDGE('',*,*,#19589,.T.);
#27633=ORIENTED_EDGE('',*,*,#19595,.T.);
#27634=ORIENTED_EDGE('',*,*,#19668,.T.);
#27635=ORIENTED_EDGE('',*,*,#19621,.T.);
#27636=ORIENTED_EDGE('',*,*,#19669,.T.);
#27637=ORIENTED_EDGE('',*,*,#19670,.T.);
#27638=ORIENTED_EDGE('',*,*,#19671,.T.);
#27639=ORIENTED_EDGE('',*,*,#19670,.F.);
#27640=ORIENTED_EDGE('',*,*,#19669,.F.);
#27641=ORIENTED_EDGE('',*,*,#19672,.T.);
#27642=ORIENTED_EDGE('',*,*,#19673,.T.);
#27643=ORIENTED_EDGE('',*,*,#19674,.T.);
#27644=ORIENTED_EDGE('',*,*,#19672,.F.);
#27645=ORIENTED_EDGE('',*,*,#19675,.F.);
#27646=ORIENTED_EDGE('',*,*,#19676,.F.);
#27647=ORIENTED_EDGE('',*,*,#19677,.F.);
#27648=ORIENTED_EDGE('',*,*,#19678,.F.);
#27649=ORIENTED_EDGE('',*,*,#19671,.F.);
#27650=ORIENTED_EDGE('',*,*,#19679,.T.);
#27651=ORIENTED_EDGE('',*,*,#19673,.F.);
#27652=ORIENTED_EDGE('',*,*,#19674,.F.);
#27653=ORIENTED_EDGE('',*,*,#19679,.F.);
#27654=ORIENTED_EDGE('',*,*,#19680,.T.);
#27655=ORIENTED_EDGE('',*,*,#19681,.T.);
#27656=ORIENTED_EDGE('',*,*,#19682,.T.);
#27657=ORIENTED_EDGE('',*,*,#19681,.F.);
#27658=ORIENTED_EDGE('',*,*,#19680,.F.);
#27659=ORIENTED_EDGE('',*,*,#19683,.T.);
#27660=ORIENTED_EDGE('',*,*,#19684,.T.);
#27661=ORIENTED_EDGE('',*,*,#19685,.T.);
#27662=ORIENTED_EDGE('',*,*,#19683,.F.);
#27663=ORIENTED_EDGE('',*,*,#19686,.F.);
#27664=ORIENTED_EDGE('',*,*,#19687,.F.);
#27665=ORIENTED_EDGE('',*,*,#19688,.F.);
#27666=ORIENTED_EDGE('',*,*,#19689,.F.);
#27667=ORIENTED_EDGE('',*,*,#19682,.F.);
#27668=ORIENTED_EDGE('',*,*,#19690,.T.);
#27669=ORIENTED_EDGE('',*,*,#19684,.F.);
#27670=ORIENTED_EDGE('',*,*,#19685,.F.);
#27671=ORIENTED_EDGE('',*,*,#19690,.F.);
#27672=ORIENTED_EDGE('',*,*,#19691,.T.);
#27673=ORIENTED_EDGE('',*,*,#19692,.T.);
#27674=ORIENTED_EDGE('',*,*,#19693,.T.);
#27675=ORIENTED_EDGE('',*,*,#19692,.F.);
#27676=ORIENTED_EDGE('',*,*,#19694,.F.);
#27677=ORIENTED_EDGE('',*,*,#19695,.T.);
#27678=ORIENTED_EDGE('',*,*,#19696,.F.);
#27679=ORIENTED_EDGE('',*,*,#19676,.T.);
#27680=ORIENTED_EDGE('',*,*,#19697,.F.);
#27681=ORIENTED_EDGE('',*,*,#19698,.T.);
#27682=ORIENTED_EDGE('',*,*,#19699,.F.);
#27683=ORIENTED_EDGE('',*,*,#19687,.T.);
#27684=ORIENTED_EDGE('',*,*,#19700,.F.);
#27685=ORIENTED_EDGE('',*,*,#19701,.F.);
#27686=ORIENTED_EDGE('',*,*,#19702,.F.);
#27687=ORIENTED_EDGE('',*,*,#19703,.F.);
#27688=ORIENTED_EDGE('',*,*,#19693,.F.);
#27689=ORIENTED_EDGE('',*,*,#19691,.F.);
#27690=ORIENTED_EDGE('',*,*,#19704,.T.);
#27691=ORIENTED_EDGE('',*,*,#19705,.T.);
#27692=ORIENTED_EDGE('',*,*,#19704,.F.);
#27693=ORIENTED_EDGE('',*,*,#19706,.T.);
#27694=ORIENTED_EDGE('',*,*,#19707,.T.);
#27695=ORIENTED_EDGE('',*,*,#19700,.T.);
#27696=ORIENTED_EDGE('',*,*,#19707,.F.);
#27697=ORIENTED_EDGE('',*,*,#19706,.F.);
#27698=ORIENTED_EDGE('',*,*,#19708,.T.);
#27699=ORIENTED_EDGE('',*,*,#19709,.T.);
#27700=ORIENTED_EDGE('',*,*,#19708,.F.);
#27701=ORIENTED_EDGE('',*,*,#19710,.T.);
#27702=ORIENTED_EDGE('',*,*,#19705,.F.);
#27703=ORIENTED_EDGE('',*,*,#19710,.F.);
#27704=ORIENTED_EDGE('',*,*,#19711,.T.);
#27705=ORIENTED_EDGE('',*,*,#19709,.F.);
#27706=ORIENTED_EDGE('',*,*,#19711,.F.);
#27707=ORIENTED_EDGE('',*,*,#19712,.T.);
#27708=ORIENTED_EDGE('',*,*,#19713,.T.);
#27709=ORIENTED_EDGE('',*,*,#19703,.T.);
#27710=ORIENTED_EDGE('',*,*,#19713,.F.);
#27711=ORIENTED_EDGE('',*,*,#19712,.F.);
#27712=ORIENTED_EDGE('',*,*,#19714,.T.);
#27713=ORIENTED_EDGE('',*,*,#19715,.T.);
#27714=ORIENTED_EDGE('',*,*,#19714,.F.);
#27715=ORIENTED_EDGE('',*,*,#19716,.T.);
#27716=ORIENTED_EDGE('',*,*,#19717,.T.);
#27717=ORIENTED_EDGE('',*,*,#19701,.T.);
#27718=ORIENTED_EDGE('',*,*,#19717,.F.);
#27719=ORIENTED_EDGE('',*,*,#19716,.F.);
#27720=ORIENTED_EDGE('',*,*,#19718,.T.);
#27721=ORIENTED_EDGE('',*,*,#19719,.T.);
#27722=ORIENTED_EDGE('',*,*,#19718,.F.);
#27723=ORIENTED_EDGE('',*,*,#19719,.F.);
#27724=ORIENTED_EDGE('',*,*,#19720,.F.);
#27725=ORIENTED_EDGE('',*,*,#19715,.F.);
#27726=ORIENTED_EDGE('',*,*,#19721,.F.);
#27727=ORIENTED_EDGE('',*,*,#19720,.T.);
#27728=ORIENTED_EDGE('',*,*,#19722,.T.);
#27729=ORIENTED_EDGE('',*,*,#19723,.F.);
#27730=ORIENTED_EDGE('',*,*,#19722,.F.);
#27731=ORIENTED_EDGE('',*,*,#19721,.T.);
#27732=ORIENTED_EDGE('',*,*,#19724,.T.);
#27733=ORIENTED_EDGE('',*,*,#19725,.F.);
#27734=ORIENTED_EDGE('',*,*,#19724,.F.);
#27735=ORIENTED_EDGE('',*,*,#19726,.T.);
#27736=ORIENTED_EDGE('',*,*,#19727,.T.);
#27737=ORIENTED_EDGE('',*,*,#19728,.T.);
#27738=ORIENTED_EDGE('',*,*,#19727,.F.);
#27739=ORIENTED_EDGE('',*,*,#19729,.F.);
#27740=ORIENTED_EDGE('',*,*,#19730,.T.);
#27741=ORIENTED_EDGE('',*,*,#19726,.F.);
#27742=ORIENTED_EDGE('',*,*,#19730,.F.);
#27743=ORIENTED_EDGE('',*,*,#19731,.F.);
#27744=ORIENTED_EDGE('',*,*,#19689,.T.);
#27745=ORIENTED_EDGE('',*,*,#19732,.F.);
#27746=ORIENTED_EDGE('',*,*,#19733,.T.);
#27747=ORIENTED_EDGE('',*,*,#19734,.F.);
#27748=ORIENTED_EDGE('',*,*,#19678,.T.);
#27749=ORIENTED_EDGE('',*,*,#19735,.F.);
#27750=ORIENTED_EDGE('',*,*,#19736,.T.);
#27751=ORIENTED_EDGE('',*,*,#19723,.T.);
#27752=ORIENTED_EDGE('',*,*,#19725,.T.);
#27753=ORIENTED_EDGE('',*,*,#19728,.F.);
#27754=ORIENTED_EDGE('',*,*,#19729,.T.);
#27755=ORIENTED_EDGE('',*,*,#19737,.T.);
#27756=ORIENTED_EDGE('',*,*,#19702,.T.);
#27757=ORIENTED_EDGE('',*,*,#19737,.F.);
#27758=ORIENTED_EDGE('',*,*,#19731,.T.);
#27759=ORIENTED_EDGE('',*,*,#19738,.T.);
#27760=ORIENTED_EDGE('',*,*,#19694,.T.);
#27761=ORIENTED_EDGE('',*,*,#19686,.T.);
#27762=ORIENTED_EDGE('',*,*,#19738,.F.);
#27763=ORIENTED_EDGE('',*,*,#19736,.F.);
#27764=ORIENTED_EDGE('',*,*,#19739,.F.);
#27765=ORIENTED_EDGE('',*,*,#19695,.F.);
#27766=ORIENTED_EDGE('',*,*,#19732,.T.);
#27767=ORIENTED_EDGE('',*,*,#19688,.T.);
#27768=ORIENTED_EDGE('',*,*,#19699,.T.);
#27769=ORIENTED_EDGE('',*,*,#19740,.T.);
#27770=ORIENTED_EDGE('',*,*,#19740,.F.);
#27771=ORIENTED_EDGE('',*,*,#19698,.F.);
#27772=ORIENTED_EDGE('',*,*,#19741,.F.);
#27773=ORIENTED_EDGE('',*,*,#19733,.F.);
#27774=ORIENTED_EDGE('',*,*,#19734,.T.);
#27775=ORIENTED_EDGE('',*,*,#19741,.T.);
#27776=ORIENTED_EDGE('',*,*,#19697,.T.);
#27777=ORIENTED_EDGE('',*,*,#19675,.T.);
#27778=ORIENTED_EDGE('',*,*,#19735,.T.);
#27779=ORIENTED_EDGE('',*,*,#19677,.T.);
#27780=ORIENTED_EDGE('',*,*,#19696,.T.);
#27781=ORIENTED_EDGE('',*,*,#19739,.T.);
#27782=ORIENTED_EDGE('',*,*,#19742,.F.);
#27783=ORIENTED_EDGE('',*,*,#19743,.T.);
#27784=ORIENTED_EDGE('',*,*,#19744,.F.);
#27785=ORIENTED_EDGE('',*,*,#19745,.T.);
#27786=ORIENTED_EDGE('',*,*,#19746,.F.);
#27787=ORIENTED_EDGE('',*,*,#19747,.T.);
#27788=ORIENTED_EDGE('',*,*,#19742,.T.);
#27789=ORIENTED_EDGE('',*,*,#19748,.T.);
#27790=ORIENTED_EDGE('',*,*,#19749,.F.);
#27791=ORIENTED_EDGE('',*,*,#19750,.T.);
#27792=ORIENTED_EDGE('',*,*,#19746,.T.);
#27793=ORIENTED_EDGE('',*,*,#19751,.T.);
#27794=ORIENTED_EDGE('',*,*,#19752,.F.);
#27795=ORIENTED_EDGE('',*,*,#19753,.T.);
#27796=ORIENTED_EDGE('',*,*,#19754,.T.);
#27797=ORIENTED_EDGE('',*,*,#19749,.T.);
#27798=ORIENTED_EDGE('',*,*,#19755,.T.);
#27799=ORIENTED_EDGE('',*,*,#19756,.T.);
#27800=ORIENTED_EDGE('',*,*,#19757,.F.);
#27801=ORIENTED_EDGE('',*,*,#19758,.T.);
#27802=ORIENTED_EDGE('',*,*,#19752,.T.);
#27803=ORIENTED_EDGE('',*,*,#19759,.T.);
#27804=ORIENTED_EDGE('',*,*,#19760,.F.);
#27805=ORIENTED_EDGE('',*,*,#19761,.T.);
#27806=ORIENTED_EDGE('',*,*,#19757,.T.);
#27807=ORIENTED_EDGE('',*,*,#19762,.T.);
#27808=ORIENTED_EDGE('',*,*,#19763,.F.);
#27809=ORIENTED_EDGE('',*,*,#19764,.T.);
#27810=ORIENTED_EDGE('',*,*,#19765,.T.);
#27811=ORIENTED_EDGE('',*,*,#19760,.T.);
#27812=ORIENTED_EDGE('',*,*,#19766,.T.);
#27813=ORIENTED_EDGE('',*,*,#19767,.T.);
#27814=ORIENTED_EDGE('',*,*,#19768,.F.);
#27815=ORIENTED_EDGE('',*,*,#19769,.T.);
#27816=ORIENTED_EDGE('',*,*,#19770,.T.);
#27817=ORIENTED_EDGE('',*,*,#19763,.T.);
#27818=ORIENTED_EDGE('',*,*,#19771,.T.);
#27819=ORIENTED_EDGE('',*,*,#19772,.T.);
#27820=ORIENTED_EDGE('',*,*,#19773,.F.);
#27821=ORIENTED_EDGE('',*,*,#19774,.T.);
#27822=ORIENTED_EDGE('',*,*,#19768,.T.);
#27823=ORIENTED_EDGE('',*,*,#19775,.T.);
#27824=ORIENTED_EDGE('',*,*,#19776,.F.);
#27825=ORIENTED_EDGE('',*,*,#19777,.T.);
#27826=ORIENTED_EDGE('',*,*,#19773,.T.);
#27827=ORIENTED_EDGE('',*,*,#19778,.T.);
#27828=ORIENTED_EDGE('',*,*,#19779,.F.);
#27829=ORIENTED_EDGE('',*,*,#19780,.T.);
#27830=ORIENTED_EDGE('',*,*,#19781,.T.);
#27831=ORIENTED_EDGE('',*,*,#19776,.T.);
#27832=ORIENTED_EDGE('',*,*,#19782,.T.);
#27833=ORIENTED_EDGE('',*,*,#19783,.T.);
#27834=ORIENTED_EDGE('',*,*,#19784,.F.);
#27835=ORIENTED_EDGE('',*,*,#19785,.T.);
#27836=ORIENTED_EDGE('',*,*,#19779,.T.);
#27837=ORIENTED_EDGE('',*,*,#19786,.T.);
#27838=ORIENTED_EDGE('',*,*,#19787,.F.);
#27839=ORIENTED_EDGE('',*,*,#19788,.T.);
#27840=ORIENTED_EDGE('',*,*,#19789,.T.);
#27841=ORIENTED_EDGE('',*,*,#19784,.T.);
#27842=ORIENTED_EDGE('',*,*,#19790,.T.);
#27843=ORIENTED_EDGE('',*,*,#19791,.T.);
#27844=ORIENTED_EDGE('',*,*,#19792,.F.);
#27845=ORIENTED_EDGE('',*,*,#19793,.T.);
#27846=ORIENTED_EDGE('',*,*,#19794,.T.);
#27847=ORIENTED_EDGE('',*,*,#19787,.T.);
#27848=ORIENTED_EDGE('',*,*,#19795,.T.);
#27849=ORIENTED_EDGE('',*,*,#19796,.T.);
#27850=ORIENTED_EDGE('',*,*,#19797,.F.);
#27851=ORIENTED_EDGE('',*,*,#19798,.T.);
#27852=ORIENTED_EDGE('',*,*,#19792,.T.);
#27853=ORIENTED_EDGE('',*,*,#19799,.T.);
#27854=ORIENTED_EDGE('',*,*,#19800,.F.);
#27855=ORIENTED_EDGE('',*,*,#19801,.T.);
#27856=ORIENTED_EDGE('',*,*,#19797,.T.);
#27857=ORIENTED_EDGE('',*,*,#19802,.T.);
#27858=ORIENTED_EDGE('',*,*,#19803,.F.);
#27859=ORIENTED_EDGE('',*,*,#19804,.T.);
#27860=ORIENTED_EDGE('',*,*,#19805,.T.);
#27861=ORIENTED_EDGE('',*,*,#19800,.T.);
#27862=ORIENTED_EDGE('',*,*,#19806,.T.);
#27863=ORIENTED_EDGE('',*,*,#19807,.T.);
#27864=ORIENTED_EDGE('',*,*,#19808,.F.);
#27865=ORIENTED_EDGE('',*,*,#19809,.T.);
#27866=ORIENTED_EDGE('',*,*,#19803,.T.);
#27867=ORIENTED_EDGE('',*,*,#19810,.T.);
#27868=ORIENTED_EDGE('',*,*,#19811,.F.);
#27869=ORIENTED_EDGE('',*,*,#19812,.T.);
#27870=ORIENTED_EDGE('',*,*,#19808,.T.);
#27871=ORIENTED_EDGE('',*,*,#19813,.T.);
#27872=ORIENTED_EDGE('',*,*,#19814,.F.);
#27873=ORIENTED_EDGE('',*,*,#19815,.T.);
#27874=ORIENTED_EDGE('',*,*,#19816,.T.);
#27875=ORIENTED_EDGE('',*,*,#19811,.T.);
#27876=ORIENTED_EDGE('',*,*,#19817,.T.);
#27877=ORIENTED_EDGE('',*,*,#19818,.T.);
#27878=ORIENTED_EDGE('',*,*,#19819,.F.);
#27879=ORIENTED_EDGE('',*,*,#19820,.T.);
#27880=ORIENTED_EDGE('',*,*,#19814,.T.);
#27881=ORIENTED_EDGE('',*,*,#19821,.T.);
#27882=ORIENTED_EDGE('',*,*,#19822,.F.);
#27883=ORIENTED_EDGE('',*,*,#19823,.T.);
#27884=ORIENTED_EDGE('',*,*,#19819,.T.);
#27885=ORIENTED_EDGE('',*,*,#19824,.T.);
#27886=ORIENTED_EDGE('',*,*,#19825,.F.);
#27887=ORIENTED_EDGE('',*,*,#19826,.T.);
#27888=ORIENTED_EDGE('',*,*,#19827,.T.);
#27889=ORIENTED_EDGE('',*,*,#19822,.T.);
#27890=ORIENTED_EDGE('',*,*,#19828,.T.);
#27891=ORIENTED_EDGE('',*,*,#19829,.F.);
#27892=ORIENTED_EDGE('',*,*,#19830,.F.);
#27893=ORIENTED_EDGE('',*,*,#19831,.F.);
#27894=ORIENTED_EDGE('',*,*,#19832,.T.);
#27895=ORIENTED_EDGE('',*,*,#19833,.F.);
#27896=ORIENTED_EDGE('',*,*,#19834,.F.);
#27897=ORIENTED_EDGE('',*,*,#19829,.T.);
#27898=ORIENTED_EDGE('',*,*,#19835,.T.);
#27899=ORIENTED_EDGE('',*,*,#19836,.F.);
#27900=ORIENTED_EDGE('',*,*,#19837,.F.);
#27901=ORIENTED_EDGE('',*,*,#19833,.T.);
#27902=ORIENTED_EDGE('',*,*,#19838,.T.);
#27903=ORIENTED_EDGE('',*,*,#19839,.F.);
#27904=ORIENTED_EDGE('',*,*,#19840,.F.);
#27905=ORIENTED_EDGE('',*,*,#19836,.T.);
#27906=ORIENTED_EDGE('',*,*,#19841,.T.);
#27907=ORIENTED_EDGE('',*,*,#19842,.F.);
#27908=ORIENTED_EDGE('',*,*,#19843,.F.);
#27909=ORIENTED_EDGE('',*,*,#19844,.F.);
#27910=ORIENTED_EDGE('',*,*,#19839,.T.);
#27911=ORIENTED_EDGE('',*,*,#19845,.T.);
#27912=ORIENTED_EDGE('',*,*,#19846,.F.);
#27913=ORIENTED_EDGE('',*,*,#19847,.F.);
#27914=ORIENTED_EDGE('',*,*,#19842,.T.);
#27915=ORIENTED_EDGE('',*,*,#19848,.T.);
#27916=ORIENTED_EDGE('',*,*,#19849,.T.);
#27917=ORIENTED_EDGE('',*,*,#19850,.F.);
#27918=ORIENTED_EDGE('',*,*,#19851,.F.);
#27919=ORIENTED_EDGE('',*,*,#19846,.T.);
#27920=ORIENTED_EDGE('',*,*,#19852,.T.);
#27921=ORIENTED_EDGE('',*,*,#19853,.F.);
#27922=ORIENTED_EDGE('',*,*,#19854,.F.);
#27923=ORIENTED_EDGE('',*,*,#19850,.T.);
#27924=ORIENTED_EDGE('',*,*,#19855,.T.);
#27925=ORIENTED_EDGE('',*,*,#19856,.F.);
#27926=ORIENTED_EDGE('',*,*,#19857,.F.);
#27927=ORIENTED_EDGE('',*,*,#19853,.T.);
#27928=ORIENTED_EDGE('',*,*,#19858,.T.);
#27929=ORIENTED_EDGE('',*,*,#19859,.F.);
#27930=ORIENTED_EDGE('',*,*,#19860,.F.);
#27931=ORIENTED_EDGE('',*,*,#19856,.T.);
#27932=ORIENTED_EDGE('',*,*,#19861,.T.);
#27933=ORIENTED_EDGE('',*,*,#19862,.F.);
#27934=ORIENTED_EDGE('',*,*,#19863,.F.);
#27935=ORIENTED_EDGE('',*,*,#19859,.T.);
#27936=ORIENTED_EDGE('',*,*,#19864,.T.);
#27937=ORIENTED_EDGE('',*,*,#19865,.F.);
#27938=ORIENTED_EDGE('',*,*,#19866,.F.);
#27939=ORIENTED_EDGE('',*,*,#19862,.T.);
#27940=ORIENTED_EDGE('',*,*,#19867,.T.);
#27941=ORIENTED_EDGE('',*,*,#19868,.F.);
#27942=ORIENTED_EDGE('',*,*,#19869,.F.);
#27943=ORIENTED_EDGE('',*,*,#19865,.T.);
#27944=ORIENTED_EDGE('',*,*,#19870,.T.);
#27945=ORIENTED_EDGE('',*,*,#19871,.F.);
#27946=ORIENTED_EDGE('',*,*,#19872,.F.);
#27947=ORIENTED_EDGE('',*,*,#19868,.T.);
#27948=ORIENTED_EDGE('',*,*,#19873,.T.);
#27949=ORIENTED_EDGE('',*,*,#19874,.F.);
#27950=ORIENTED_EDGE('',*,*,#19875,.F.);
#27951=ORIENTED_EDGE('',*,*,#19876,.F.);
#27952=ORIENTED_EDGE('',*,*,#19871,.T.);
#27953=ORIENTED_EDGE('',*,*,#19877,.T.);
#27954=ORIENTED_EDGE('',*,*,#19878,.F.);
#27955=ORIENTED_EDGE('',*,*,#19879,.F.);
#27956=ORIENTED_EDGE('',*,*,#19874,.T.);
#27957=ORIENTED_EDGE('',*,*,#19880,.T.);
#27958=ORIENTED_EDGE('',*,*,#19881,.F.);
#27959=ORIENTED_EDGE('',*,*,#19882,.F.);
#27960=ORIENTED_EDGE('',*,*,#19878,.T.);
#27961=ORIENTED_EDGE('',*,*,#19883,.T.);
#27962=ORIENTED_EDGE('',*,*,#19884,.F.);
#27963=ORIENTED_EDGE('',*,*,#19885,.F.);
#27964=ORIENTED_EDGE('',*,*,#19881,.T.);
#27965=ORIENTED_EDGE('',*,*,#19886,.T.);
#27966=ORIENTED_EDGE('',*,*,#19887,.F.);
#27967=ORIENTED_EDGE('',*,*,#19888,.F.);
#27968=ORIENTED_EDGE('',*,*,#19884,.T.);
#27969=ORIENTED_EDGE('',*,*,#19889,.T.);
#27970=ORIENTED_EDGE('',*,*,#19890,.F.);
#27971=ORIENTED_EDGE('',*,*,#19891,.F.);
#27972=ORIENTED_EDGE('',*,*,#19887,.T.);
#27973=ORIENTED_EDGE('',*,*,#19892,.T.);
#27974=ORIENTED_EDGE('',*,*,#19893,.F.);
#27975=ORIENTED_EDGE('',*,*,#19894,.F.);
#27976=ORIENTED_EDGE('',*,*,#19890,.T.);
#27977=ORIENTED_EDGE('',*,*,#19895,.T.);
#27978=ORIENTED_EDGE('',*,*,#19896,.T.);
#27979=ORIENTED_EDGE('',*,*,#19897,.F.);
#27980=ORIENTED_EDGE('',*,*,#19898,.F.);
#27981=ORIENTED_EDGE('',*,*,#19893,.T.);
#27982=ORIENTED_EDGE('',*,*,#19899,.T.);
#27983=ORIENTED_EDGE('',*,*,#19900,.F.);
#27984=ORIENTED_EDGE('',*,*,#19901,.F.);
#27985=ORIENTED_EDGE('',*,*,#19897,.T.);
#27986=ORIENTED_EDGE('',*,*,#19902,.T.);
#27987=ORIENTED_EDGE('',*,*,#19900,.T.);
#27988=ORIENTED_EDGE('',*,*,#19903,.T.);
#27989=ORIENTED_EDGE('',*,*,#19904,.F.);
#27990=ORIENTED_EDGE('',*,*,#19905,.F.);
#27991=ORIENTED_EDGE('',*,*,#19906,.F.);
#27992=ORIENTED_EDGE('',*,*,#19825,.T.);
#27993=ORIENTED_EDGE('',*,*,#19907,.T.);
#27994=ORIENTED_EDGE('',*,*,#19908,.F.);
#27995=ORIENTED_EDGE('',*,*,#19909,.T.);
#27996=ORIENTED_EDGE('',*,*,#19910,.F.);
#27997=ORIENTED_EDGE('',*,*,#19911,.T.);
#27998=ORIENTED_EDGE('',*,*,#19904,.T.);
#27999=ORIENTED_EDGE('',*,*,#19912,.T.);
#28000=ORIENTED_EDGE('',*,*,#19913,.F.);
#28001=ORIENTED_EDGE('',*,*,#19911,.F.);
#28002=ORIENTED_EDGE('',*,*,#19914,.F.);
#28003=ORIENTED_EDGE('',*,*,#19907,.F.);
#28004=ORIENTED_EDGE('',*,*,#19828,.F.);
#28005=ORIENTED_EDGE('',*,*,#19824,.F.);
#28006=ORIENTED_EDGE('',*,*,#19821,.F.);
#28007=ORIENTED_EDGE('',*,*,#19818,.F.);
#28008=ORIENTED_EDGE('',*,*,#19817,.F.);
#28009=ORIENTED_EDGE('',*,*,#19813,.F.);
#28010=ORIENTED_EDGE('',*,*,#19810,.F.);
#28011=ORIENTED_EDGE('',*,*,#19807,.F.);
#28012=ORIENTED_EDGE('',*,*,#19806,.F.);
#28013=ORIENTED_EDGE('',*,*,#19802,.F.);
#28014=ORIENTED_EDGE('',*,*,#19799,.F.);
#28015=ORIENTED_EDGE('',*,*,#19796,.F.);
#28016=ORIENTED_EDGE('',*,*,#19795,.F.);
#28017=ORIENTED_EDGE('',*,*,#19791,.F.);
#28018=ORIENTED_EDGE('',*,*,#19790,.F.);
#28019=ORIENTED_EDGE('',*,*,#19786,.F.);
#28020=ORIENTED_EDGE('',*,*,#19783,.F.);
#28021=ORIENTED_EDGE('',*,*,#19782,.F.);
#28022=ORIENTED_EDGE('',*,*,#19778,.F.);
#28023=ORIENTED_EDGE('',*,*,#19775,.F.);
#28024=ORIENTED_EDGE('',*,*,#19772,.F.);
#28025=ORIENTED_EDGE('',*,*,#19771,.F.);
#28026=ORIENTED_EDGE('',*,*,#19767,.F.);
#28027=ORIENTED_EDGE('',*,*,#19766,.F.);
#28028=ORIENTED_EDGE('',*,*,#19762,.F.);
#28029=ORIENTED_EDGE('',*,*,#19759,.F.);
#28030=ORIENTED_EDGE('',*,*,#19756,.F.);
#28031=ORIENTED_EDGE('',*,*,#19755,.F.);
#28032=ORIENTED_EDGE('',*,*,#19751,.F.);
#28033=ORIENTED_EDGE('',*,*,#19748,.F.);
#28034=ORIENTED_EDGE('',*,*,#19745,.F.);
#28035=ORIENTED_EDGE('',*,*,#19915,.F.);
#28036=ORIENTED_EDGE('',*,*,#19830,.T.);
#28037=ORIENTED_EDGE('',*,*,#19834,.T.);
#28038=ORIENTED_EDGE('',*,*,#19837,.T.);
#28039=ORIENTED_EDGE('',*,*,#19840,.T.);
#28040=ORIENTED_EDGE('',*,*,#19844,.T.);
#28041=ORIENTED_EDGE('',*,*,#19843,.T.);
#28042=ORIENTED_EDGE('',*,*,#19847,.T.);
#28043=ORIENTED_EDGE('',*,*,#19851,.T.);
#28044=ORIENTED_EDGE('',*,*,#19854,.T.);
#28045=ORIENTED_EDGE('',*,*,#19857,.T.);
#28046=ORIENTED_EDGE('',*,*,#19860,.T.);
#28047=ORIENTED_EDGE('',*,*,#19863,.T.);
#28048=ORIENTED_EDGE('',*,*,#19866,.T.);
#28049=ORIENTED_EDGE('',*,*,#19869,.T.);
#28050=ORIENTED_EDGE('',*,*,#19872,.T.);
#28051=ORIENTED_EDGE('',*,*,#19876,.T.);
#28052=ORIENTED_EDGE('',*,*,#19875,.T.);
#28053=ORIENTED_EDGE('',*,*,#19879,.T.);
#28054=ORIENTED_EDGE('',*,*,#19882,.T.);
#28055=ORIENTED_EDGE('',*,*,#19885,.T.);
#28056=ORIENTED_EDGE('',*,*,#19888,.T.);
#28057=ORIENTED_EDGE('',*,*,#19891,.T.);
#28058=ORIENTED_EDGE('',*,*,#19894,.T.);
#28059=ORIENTED_EDGE('',*,*,#19898,.T.);
#28060=ORIENTED_EDGE('',*,*,#19901,.T.);
#28061=ORIENTED_EDGE('',*,*,#19906,.T.);
#28062=ORIENTED_EDGE('',*,*,#19905,.T.);
#28063=ORIENTED_EDGE('',*,*,#19916,.F.);
#28064=ORIENTED_EDGE('',*,*,#19917,.T.);
#28065=ORIENTED_EDGE('',*,*,#19831,.T.);
#28066=ORIENTED_EDGE('',*,*,#19915,.T.);
#28067=ORIENTED_EDGE('',*,*,#19918,.F.);
#28068=ORIENTED_EDGE('',*,*,#19912,.F.);
#28069=ORIENTED_EDGE('',*,*,#19903,.F.);
#28070=ORIENTED_EDGE('',*,*,#19902,.F.);
#28071=ORIENTED_EDGE('',*,*,#19899,.F.);
#28072=ORIENTED_EDGE('',*,*,#19896,.F.);
#28073=ORIENTED_EDGE('',*,*,#19895,.F.);
#28074=ORIENTED_EDGE('',*,*,#19892,.F.);
#28075=ORIENTED_EDGE('',*,*,#19889,.F.);
#28076=ORIENTED_EDGE('',*,*,#19886,.F.);
#28077=ORIENTED_EDGE('',*,*,#19883,.F.);
#28078=ORIENTED_EDGE('',*,*,#19880,.F.);
#28079=ORIENTED_EDGE('',*,*,#19877,.F.);
#28080=ORIENTED_EDGE('',*,*,#19873,.F.);
#28081=ORIENTED_EDGE('',*,*,#19870,.F.);
#28082=ORIENTED_EDGE('',*,*,#19867,.F.);
#28083=ORIENTED_EDGE('',*,*,#19864,.F.);
#28084=ORIENTED_EDGE('',*,*,#19861,.F.);
#28085=ORIENTED_EDGE('',*,*,#19858,.F.);
#28086=ORIENTED_EDGE('',*,*,#19855,.F.);
#28087=ORIENTED_EDGE('',*,*,#19852,.F.);
#28088=ORIENTED_EDGE('',*,*,#19849,.F.);
#28089=ORIENTED_EDGE('',*,*,#19848,.F.);
#28090=ORIENTED_EDGE('',*,*,#19845,.F.);
#28091=ORIENTED_EDGE('',*,*,#19841,.F.);
#28092=ORIENTED_EDGE('',*,*,#19838,.F.);
#28093=ORIENTED_EDGE('',*,*,#19835,.F.);
#28094=ORIENTED_EDGE('',*,*,#19832,.F.);
#28095=ORIENTED_EDGE('',*,*,#19917,.F.);
#28096=ORIENTED_EDGE('',*,*,#19919,.F.);
#28097=ORIENTED_EDGE('',*,*,#19743,.F.);
#28098=ORIENTED_EDGE('',*,*,#19747,.F.);
#28099=ORIENTED_EDGE('',*,*,#19750,.F.);
#28100=ORIENTED_EDGE('',*,*,#19754,.F.);
#28101=ORIENTED_EDGE('',*,*,#19753,.F.);
#28102=ORIENTED_EDGE('',*,*,#19758,.F.);
#28103=ORIENTED_EDGE('',*,*,#19761,.F.);
#28104=ORIENTED_EDGE('',*,*,#19765,.F.);
#28105=ORIENTED_EDGE('',*,*,#19764,.F.);
#28106=ORIENTED_EDGE('',*,*,#19770,.F.);
#28107=ORIENTED_EDGE('',*,*,#19769,.F.);
#28108=ORIENTED_EDGE('',*,*,#19774,.F.);
#28109=ORIENTED_EDGE('',*,*,#19777,.F.);
#28110=ORIENTED_EDGE('',*,*,#19781,.F.);
#28111=ORIENTED_EDGE('',*,*,#19780,.F.);
#28112=ORIENTED_EDGE('',*,*,#19785,.F.);
#28113=ORIENTED_EDGE('',*,*,#19789,.F.);
#28114=ORIENTED_EDGE('',*,*,#19788,.F.);
#28115=ORIENTED_EDGE('',*,*,#19794,.F.);
#28116=ORIENTED_EDGE('',*,*,#19793,.F.);
#28117=ORIENTED_EDGE('',*,*,#19798,.F.);
#28118=ORIENTED_EDGE('',*,*,#19801,.F.);
#28119=ORIENTED_EDGE('',*,*,#19805,.F.);
#28120=ORIENTED_EDGE('',*,*,#19804,.F.);
#28121=ORIENTED_EDGE('',*,*,#19809,.F.);
#28122=ORIENTED_EDGE('',*,*,#19812,.F.);
#28123=ORIENTED_EDGE('',*,*,#19816,.F.);
#28124=ORIENTED_EDGE('',*,*,#19815,.F.);
#28125=ORIENTED_EDGE('',*,*,#19820,.F.);
#28126=ORIENTED_EDGE('',*,*,#19823,.F.);
#28127=ORIENTED_EDGE('',*,*,#19827,.F.);
#28128=ORIENTED_EDGE('',*,*,#19826,.F.);
#28129=ORIENTED_EDGE('',*,*,#19909,.F.);
#28130=ORIENTED_EDGE('',*,*,#19920,.T.);
#28131=ORIENTED_EDGE('',*,*,#19921,.T.);
#28132=ORIENTED_EDGE('',*,*,#19918,.T.);
#28133=ORIENTED_EDGE('',*,*,#19744,.T.);
#28134=ORIENTED_EDGE('',*,*,#19919,.T.);
#28135=ORIENTED_EDGE('',*,*,#19916,.T.);
#28136=ORIENTED_EDGE('',*,*,#19921,.F.);
#28137=ORIENTED_EDGE('',*,*,#19922,.F.);
#28138=ORIENTED_EDGE('',*,*,#19920,.F.);
#28139=ORIENTED_EDGE('',*,*,#19910,.T.);
#28140=ORIENTED_EDGE('',*,*,#19923,.T.);
#28141=ORIENTED_EDGE('',*,*,#19924,.T.);
#28142=ORIENTED_EDGE('',*,*,#19923,.F.);
#28143=ORIENTED_EDGE('',*,*,#19913,.T.);
#28144=ORIENTED_EDGE('',*,*,#19908,.T.);
#28145=ORIENTED_EDGE('',*,*,#19914,.T.);
#28146=ORIENTED_EDGE('',*,*,#19924,.F.);
#28147=ORIENTED_EDGE('',*,*,#19925,.F.);
#28148=ORIENTED_EDGE('',*,*,#19926,.F.);
#28149=ORIENTED_EDGE('',*,*,#19927,.F.);
#28150=ORIENTED_EDGE('',*,*,#19928,.F.);
#28151=ORIENTED_EDGE('',*,*,#19927,.T.);
#28152=ORIENTED_EDGE('',*,*,#19929,.F.);
#28153=ORIENTED_EDGE('',*,*,#19930,.F.);
#28154=ORIENTED_EDGE('',*,*,#19931,.F.);
#28155=ORIENTED_EDGE('',*,*,#19932,.F.);
#28156=ORIENTED_EDGE('',*,*,#19929,.T.);
#28157=ORIENTED_EDGE('',*,*,#19926,.T.);
#28158=ORIENTED_EDGE('',*,*,#19933,.T.);
#28159=ORIENTED_EDGE('',*,*,#19934,.T.);
#28160=ORIENTED_EDGE('',*,*,#19935,.F.);
#28161=ORIENTED_EDGE('',*,*,#19936,.F.);
#28162=ORIENTED_EDGE('',*,*,#19934,.F.);
#28163=ORIENTED_EDGE('',*,*,#19937,.T.);
#28164=ORIENTED_EDGE('',*,*,#19938,.T.);
#28165=ORIENTED_EDGE('',*,*,#19939,.F.);
#28166=ORIENTED_EDGE('',*,*,#19940,.T.);
#28167=ORIENTED_EDGE('',*,*,#19941,.T.);
#28168=ORIENTED_EDGE('',*,*,#19942,.T.);
#28169=ORIENTED_EDGE('',*,*,#19943,.F.);
#28170=ORIENTED_EDGE('',*,*,#19944,.T.);
#28171=ORIENTED_EDGE('',*,*,#19945,.T.);
#28172=ORIENTED_EDGE('',*,*,#19946,.T.);
#28173=ORIENTED_EDGE('',*,*,#19947,.F.);
#28174=ORIENTED_EDGE('',*,*,#19948,.T.);
#28175=ORIENTED_EDGE('',*,*,#19949,.T.);
#28176=ORIENTED_EDGE('',*,*,#19950,.T.);
#28177=ORIENTED_EDGE('',*,*,#19951,.F.);
#28178=ORIENTED_EDGE('',*,*,#19952,.T.);
#28179=ORIENTED_EDGE('',*,*,#19953,.T.);
#28180=ORIENTED_EDGE('',*,*,#19954,.T.);
#28181=ORIENTED_EDGE('',*,*,#19955,.F.);
#28182=ORIENTED_EDGE('',*,*,#19956,.T.);
#28183=ORIENTED_EDGE('',*,*,#19957,.T.);
#28184=ORIENTED_EDGE('',*,*,#19958,.T.);
#28185=ORIENTED_EDGE('',*,*,#19959,.F.);
#28186=ORIENTED_EDGE('',*,*,#19960,.T.);
#28187=ORIENTED_EDGE('',*,*,#19961,.T.);
#28188=ORIENTED_EDGE('',*,*,#19962,.T.);
#28189=ORIENTED_EDGE('',*,*,#19963,.F.);
#28190=ORIENTED_EDGE('',*,*,#19964,.T.);
#28191=ORIENTED_EDGE('',*,*,#19965,.T.);
#28192=ORIENTED_EDGE('',*,*,#19966,.T.);
#28193=ORIENTED_EDGE('',*,*,#19967,.F.);
#28194=ORIENTED_EDGE('',*,*,#19968,.T.);
#28195=ORIENTED_EDGE('',*,*,#19969,.T.);
#28196=ORIENTED_EDGE('',*,*,#19970,.T.);
#28197=ORIENTED_EDGE('',*,*,#19971,.F.);
#28198=ORIENTED_EDGE('',*,*,#19972,.T.);
#28199=ORIENTED_EDGE('',*,*,#19973,.T.);
#28200=ORIENTED_EDGE('',*,*,#19974,.T.);
#28201=ORIENTED_EDGE('',*,*,#19975,.F.);
#28202=ORIENTED_EDGE('',*,*,#19976,.T.);
#28203=ORIENTED_EDGE('',*,*,#19977,.T.);
#28204=ORIENTED_EDGE('',*,*,#19978,.T.);
#28205=ORIENTED_EDGE('',*,*,#19979,.F.);
#28206=ORIENTED_EDGE('',*,*,#19980,.T.);
#28207=ORIENTED_EDGE('',*,*,#19981,.T.);
#28208=ORIENTED_EDGE('',*,*,#19982,.T.);
#28209=ORIENTED_EDGE('',*,*,#19983,.F.);
#28210=ORIENTED_EDGE('',*,*,#19984,.T.);
#28211=ORIENTED_EDGE('',*,*,#19985,.T.);
#28212=ORIENTED_EDGE('',*,*,#19986,.T.);
#28213=ORIENTED_EDGE('',*,*,#19987,.F.);
#28214=ORIENTED_EDGE('',*,*,#19988,.T.);
#28215=ORIENTED_EDGE('',*,*,#19989,.T.);
#28216=ORIENTED_EDGE('',*,*,#19990,.T.);
#28217=ORIENTED_EDGE('',*,*,#19991,.F.);
#28218=ORIENTED_EDGE('',*,*,#19992,.T.);
#28219=ORIENTED_EDGE('',*,*,#19993,.T.);
#28220=ORIENTED_EDGE('',*,*,#19994,.T.);
#28221=ORIENTED_EDGE('',*,*,#19995,.F.);
#28222=ORIENTED_EDGE('',*,*,#19996,.T.);
#28223=ORIENTED_EDGE('',*,*,#19997,.T.);
#28224=ORIENTED_EDGE('',*,*,#19998,.T.);
#28225=ORIENTED_EDGE('',*,*,#19999,.F.);
#28226=ORIENTED_EDGE('',*,*,#20000,.T.);
#28227=ORIENTED_EDGE('',*,*,#20001,.T.);
#28228=ORIENTED_EDGE('',*,*,#20002,.T.);
#28229=ORIENTED_EDGE('',*,*,#20003,.F.);
#28230=ORIENTED_EDGE('',*,*,#19931,.T.);
#28231=ORIENTED_EDGE('',*,*,#19925,.T.);
#28232=ORIENTED_EDGE('',*,*,#19928,.T.);
#28233=ORIENTED_EDGE('',*,*,#20004,.F.);
#28234=ORIENTED_EDGE('',*,*,#20005,.T.);
#28235=ORIENTED_EDGE('',*,*,#20006,.T.);
#28236=ORIENTED_EDGE('',*,*,#20007,.T.);
#28237=ORIENTED_EDGE('',*,*,#20008,.F.);
#28238=ORIENTED_EDGE('',*,*,#20009,.T.);
#28239=ORIENTED_EDGE('',*,*,#20010,.T.);
#28240=ORIENTED_EDGE('',*,*,#20011,.T.);
#28241=ORIENTED_EDGE('',*,*,#20012,.F.);
#28242=ORIENTED_EDGE('',*,*,#20013,.T.);
#28243=ORIENTED_EDGE('',*,*,#20014,.T.);
#28244=ORIENTED_EDGE('',*,*,#20015,.T.);
#28245=ORIENTED_EDGE('',*,*,#20016,.F.);
#28246=ORIENTED_EDGE('',*,*,#20017,.T.);
#28247=ORIENTED_EDGE('',*,*,#20018,.T.);
#28248=ORIENTED_EDGE('',*,*,#20019,.T.);
#28249=ORIENTED_EDGE('',*,*,#20020,.F.);
#28250=ORIENTED_EDGE('',*,*,#20021,.T.);
#28251=ORIENTED_EDGE('',*,*,#20022,.T.);
#28252=ORIENTED_EDGE('',*,*,#20023,.T.);
#28253=ORIENTED_EDGE('',*,*,#20024,.F.);
#28254=ORIENTED_EDGE('',*,*,#20025,.T.);
#28255=ORIENTED_EDGE('',*,*,#20026,.T.);
#28256=ORIENTED_EDGE('',*,*,#20027,.T.);
#28257=ORIENTED_EDGE('',*,*,#20028,.F.);
#28258=ORIENTED_EDGE('',*,*,#20029,.T.);
#28259=ORIENTED_EDGE('',*,*,#20030,.T.);
#28260=ORIENTED_EDGE('',*,*,#20031,.T.);
#28261=ORIENTED_EDGE('',*,*,#20032,.F.);
#28262=ORIENTED_EDGE('',*,*,#20033,.T.);
#28263=ORIENTED_EDGE('',*,*,#20034,.T.);
#28264=ORIENTED_EDGE('',*,*,#20035,.T.);
#28265=ORIENTED_EDGE('',*,*,#20036,.F.);
#28266=ORIENTED_EDGE('',*,*,#20037,.T.);
#28267=ORIENTED_EDGE('',*,*,#20038,.T.);
#28268=ORIENTED_EDGE('',*,*,#20039,.T.);
#28269=ORIENTED_EDGE('',*,*,#20040,.F.);
#28270=ORIENTED_EDGE('',*,*,#20041,.T.);
#28271=ORIENTED_EDGE('',*,*,#20042,.T.);
#28272=ORIENTED_EDGE('',*,*,#20043,.T.);
#28273=ORIENTED_EDGE('',*,*,#20044,.F.);
#28274=ORIENTED_EDGE('',*,*,#20045,.T.);
#28275=ORIENTED_EDGE('',*,*,#20046,.T.);
#28276=ORIENTED_EDGE('',*,*,#20047,.T.);
#28277=ORIENTED_EDGE('',*,*,#20048,.F.);
#28278=ORIENTED_EDGE('',*,*,#20049,.T.);
#28279=ORIENTED_EDGE('',*,*,#20050,.T.);
#28280=ORIENTED_EDGE('',*,*,#20051,.T.);
#28281=ORIENTED_EDGE('',*,*,#20052,.F.);
#28282=ORIENTED_EDGE('',*,*,#20053,.T.);
#28283=ORIENTED_EDGE('',*,*,#20054,.T.);
#28284=ORIENTED_EDGE('',*,*,#20055,.T.);
#28285=ORIENTED_EDGE('',*,*,#20056,.F.);
#28286=ORIENTED_EDGE('',*,*,#20057,.T.);
#28287=ORIENTED_EDGE('',*,*,#20058,.T.);
#28288=ORIENTED_EDGE('',*,*,#20059,.T.);
#28289=ORIENTED_EDGE('',*,*,#20060,.F.);
#28290=ORIENTED_EDGE('',*,*,#20061,.T.);
#28291=ORIENTED_EDGE('',*,*,#20062,.T.);
#28292=ORIENTED_EDGE('',*,*,#20063,.T.);
#28293=ORIENTED_EDGE('',*,*,#20064,.F.);
#28294=ORIENTED_EDGE('',*,*,#20065,.T.);
#28295=ORIENTED_EDGE('',*,*,#20066,.T.);
#28296=ORIENTED_EDGE('',*,*,#20067,.T.);
#28297=ORIENTED_EDGE('',*,*,#20068,.F.);
#28298=ORIENTED_EDGE('',*,*,#20069,.T.);
#28299=ORIENTED_EDGE('',*,*,#20070,.T.);
#28300=ORIENTED_EDGE('',*,*,#20071,.T.);
#28301=ORIENTED_EDGE('',*,*,#20072,.F.);
#28302=ORIENTED_EDGE('',*,*,#20073,.T.);
#28303=ORIENTED_EDGE('',*,*,#20074,.T.);
#28304=ORIENTED_EDGE('',*,*,#20075,.T.);
#28305=ORIENTED_EDGE('',*,*,#20076,.F.);
#28306=ORIENTED_EDGE('',*,*,#20077,.T.);
#28307=ORIENTED_EDGE('',*,*,#20002,.F.);
#28308=ORIENTED_EDGE('',*,*,#20078,.T.);
#28309=ORIENTED_EDGE('',*,*,#20079,.F.);
#28310=ORIENTED_EDGE('',*,*,#20080,.F.);
#28311=ORIENTED_EDGE('',*,*,#20081,.F.);
#28312=ORIENTED_EDGE('',*,*,#20079,.T.);
#28313=ORIENTED_EDGE('',*,*,#20082,.T.);
#28314=ORIENTED_EDGE('',*,*,#20000,.F.);
#28315=ORIENTED_EDGE('',*,*,#20001,.F.);
#28316=ORIENTED_EDGE('',*,*,#20082,.F.);
#28317=ORIENTED_EDGE('',*,*,#20078,.F.);
#28318=ORIENTED_EDGE('',*,*,#20083,.T.);
#28319=ORIENTED_EDGE('',*,*,#20076,.T.);
#28320=ORIENTED_EDGE('',*,*,#20084,.T.);
#28321=ORIENTED_EDGE('',*,*,#20085,.T.);
#28322=ORIENTED_EDGE('',*,*,#20072,.T.);
#28323=ORIENTED_EDGE('',*,*,#20086,.T.);
#28324=ORIENTED_EDGE('',*,*,#20087,.T.);
#28325=ORIENTED_EDGE('',*,*,#20068,.T.);
#28326=ORIENTED_EDGE('',*,*,#20088,.T.);
#28327=ORIENTED_EDGE('',*,*,#20089,.T.);
#28328=ORIENTED_EDGE('',*,*,#20064,.T.);
#28329=ORIENTED_EDGE('',*,*,#20090,.T.);
#28330=ORIENTED_EDGE('',*,*,#20091,.T.);
#28331=ORIENTED_EDGE('',*,*,#20060,.T.);
#28332=ORIENTED_EDGE('',*,*,#20092,.T.);
#28333=ORIENTED_EDGE('',*,*,#20093,.T.);
#28334=ORIENTED_EDGE('',*,*,#20056,.T.);
#28335=ORIENTED_EDGE('',*,*,#20094,.T.);
#28336=ORIENTED_EDGE('',*,*,#20095,.T.);
#28337=ORIENTED_EDGE('',*,*,#20052,.T.);
#28338=ORIENTED_EDGE('',*,*,#20096,.T.);
#28339=ORIENTED_EDGE('',*,*,#20097,.T.);
#28340=ORIENTED_EDGE('',*,*,#20048,.T.);
#28341=ORIENTED_EDGE('',*,*,#20098,.T.);
#28342=ORIENTED_EDGE('',*,*,#20099,.T.);
#28343=ORIENTED_EDGE('',*,*,#20044,.T.);
#28344=ORIENTED_EDGE('',*,*,#20100,.T.);
#28345=ORIENTED_EDGE('',*,*,#20101,.T.);
#28346=ORIENTED_EDGE('',*,*,#20040,.T.);
#28347=ORIENTED_EDGE('',*,*,#20102,.T.);
#28348=ORIENTED_EDGE('',*,*,#20103,.T.);
#28349=ORIENTED_EDGE('',*,*,#20036,.T.);
#28350=ORIENTED_EDGE('',*,*,#20104,.T.);
#28351=ORIENTED_EDGE('',*,*,#20105,.T.);
#28352=ORIENTED_EDGE('',*,*,#20032,.T.);
#28353=ORIENTED_EDGE('',*,*,#20106,.T.);
#28354=ORIENTED_EDGE('',*,*,#20107,.T.);
#28355=ORIENTED_EDGE('',*,*,#20028,.T.);
#28356=ORIENTED_EDGE('',*,*,#20108,.T.);
#28357=ORIENTED_EDGE('',*,*,#20109,.T.);
#28358=ORIENTED_EDGE('',*,*,#20024,.T.);
#28359=ORIENTED_EDGE('',*,*,#20110,.T.);
#28360=ORIENTED_EDGE('',*,*,#20111,.T.);
#28361=ORIENTED_EDGE('',*,*,#20020,.T.);
#28362=ORIENTED_EDGE('',*,*,#20112,.T.);
#28363=ORIENTED_EDGE('',*,*,#20113,.T.);
#28364=ORIENTED_EDGE('',*,*,#20016,.T.);
#28365=ORIENTED_EDGE('',*,*,#20114,.T.);
#28366=ORIENTED_EDGE('',*,*,#20115,.T.);
#28367=ORIENTED_EDGE('',*,*,#20012,.T.);
#28368=ORIENTED_EDGE('',*,*,#20116,.T.);
#28369=ORIENTED_EDGE('',*,*,#20117,.T.);
#28370=ORIENTED_EDGE('',*,*,#20008,.T.);
#28371=ORIENTED_EDGE('',*,*,#20118,.T.);
#28372=ORIENTED_EDGE('',*,*,#20119,.T.);
#28373=ORIENTED_EDGE('',*,*,#20004,.T.);
#28374=ORIENTED_EDGE('',*,*,#19930,.T.);
#28375=ORIENTED_EDGE('',*,*,#19932,.T.);
#28376=ORIENTED_EDGE('',*,*,#20003,.T.);
#28377=ORIENTED_EDGE('',*,*,#20080,.T.);
#28378=ORIENTED_EDGE('',*,*,#20081,.T.);
#28379=ORIENTED_EDGE('',*,*,#19999,.T.);
#28380=ORIENTED_EDGE('',*,*,#20120,.T.);
#28381=ORIENTED_EDGE('',*,*,#20121,.T.);
#28382=ORIENTED_EDGE('',*,*,#19995,.T.);
#28383=ORIENTED_EDGE('',*,*,#20122,.T.);
#28384=ORIENTED_EDGE('',*,*,#20123,.T.);
#28385=ORIENTED_EDGE('',*,*,#19991,.T.);
#28386=ORIENTED_EDGE('',*,*,#20124,.T.);
#28387=ORIENTED_EDGE('',*,*,#20125,.T.);
#28388=ORIENTED_EDGE('',*,*,#19987,.T.);
#28389=ORIENTED_EDGE('',*,*,#20126,.T.);
#28390=ORIENTED_EDGE('',*,*,#20127,.T.);
#28391=ORIENTED_EDGE('',*,*,#19983,.T.);
#28392=ORIENTED_EDGE('',*,*,#20128,.T.);
#28393=ORIENTED_EDGE('',*,*,#20129,.T.);
#28394=ORIENTED_EDGE('',*,*,#19979,.T.);
#28395=ORIENTED_EDGE('',*,*,#20130,.T.);
#28396=ORIENTED_EDGE('',*,*,#20131,.T.);
#28397=ORIENTED_EDGE('',*,*,#19975,.T.);
#28398=ORIENTED_EDGE('',*,*,#20132,.T.);
#28399=ORIENTED_EDGE('',*,*,#20133,.T.);
#28400=ORIENTED_EDGE('',*,*,#19971,.T.);
#28401=ORIENTED_EDGE('',*,*,#20134,.T.);
#28402=ORIENTED_EDGE('',*,*,#20135,.T.);
#28403=ORIENTED_EDGE('',*,*,#19967,.T.);
#28404=ORIENTED_EDGE('',*,*,#20136,.T.);
#28405=ORIENTED_EDGE('',*,*,#20137,.T.);
#28406=ORIENTED_EDGE('',*,*,#19963,.T.);
#28407=ORIENTED_EDGE('',*,*,#20138,.T.);
#28408=ORIENTED_EDGE('',*,*,#20139,.T.);
#28409=ORIENTED_EDGE('',*,*,#19959,.T.);
#28410=ORIENTED_EDGE('',*,*,#20140,.T.);
#28411=ORIENTED_EDGE('',*,*,#20141,.T.);
#28412=ORIENTED_EDGE('',*,*,#19955,.T.);
#28413=ORIENTED_EDGE('',*,*,#20142,.T.);
#28414=ORIENTED_EDGE('',*,*,#20143,.T.);
#28415=ORIENTED_EDGE('',*,*,#19951,.T.);
#28416=ORIENTED_EDGE('',*,*,#20144,.T.);
#28417=ORIENTED_EDGE('',*,*,#20145,.T.);
#28418=ORIENTED_EDGE('',*,*,#19947,.T.);
#28419=ORIENTED_EDGE('',*,*,#20146,.T.);
#28420=ORIENTED_EDGE('',*,*,#20147,.T.);
#28421=ORIENTED_EDGE('',*,*,#19943,.T.);
#28422=ORIENTED_EDGE('',*,*,#20148,.T.);
#28423=ORIENTED_EDGE('',*,*,#20149,.T.);
#28424=ORIENTED_EDGE('',*,*,#19939,.T.);
#28425=ORIENTED_EDGE('',*,*,#20150,.T.);
#28426=ORIENTED_EDGE('',*,*,#20151,.T.);
#28427=ORIENTED_EDGE('',*,*,#20152,.T.);
#28428=ORIENTED_EDGE('',*,*,#20151,.F.);
#28429=ORIENTED_EDGE('',*,*,#19997,.F.);
#28430=ORIENTED_EDGE('',*,*,#20153,.F.);
#28431=ORIENTED_EDGE('',*,*,#20154,.F.);
#28432=ORIENTED_EDGE('',*,*,#19998,.F.);
#28433=ORIENTED_EDGE('',*,*,#20154,.T.);
#28434=ORIENTED_EDGE('',*,*,#20155,.F.);
#28435=ORIENTED_EDGE('',*,*,#20120,.F.);
#28436=ORIENTED_EDGE('',*,*,#19996,.F.);
#28437=ORIENTED_EDGE('',*,*,#20121,.F.);
#28438=ORIENTED_EDGE('',*,*,#20155,.T.);
#28439=ORIENTED_EDGE('',*,*,#20153,.T.);
#28440=ORIENTED_EDGE('',*,*,#19994,.F.);
#28441=ORIENTED_EDGE('',*,*,#20156,.T.);
#28442=ORIENTED_EDGE('',*,*,#20157,.F.);
#28443=ORIENTED_EDGE('',*,*,#20122,.F.);
#28444=ORIENTED_EDGE('',*,*,#20123,.F.);
#28445=ORIENTED_EDGE('',*,*,#20157,.T.);
#28446=ORIENTED_EDGE('',*,*,#20158,.T.);
#28447=ORIENTED_EDGE('',*,*,#19992,.F.);
#28448=ORIENTED_EDGE('',*,*,#19993,.F.);
#28449=ORIENTED_EDGE('',*,*,#20158,.F.);
#28450=ORIENTED_EDGE('',*,*,#20156,.F.);
#28451=ORIENTED_EDGE('',*,*,#19989,.F.);
#28452=ORIENTED_EDGE('',*,*,#20159,.F.);
#28453=ORIENTED_EDGE('',*,*,#20160,.F.);
#28454=ORIENTED_EDGE('',*,*,#19990,.F.);
#28455=ORIENTED_EDGE('',*,*,#20160,.T.);
#28456=ORIENTED_EDGE('',*,*,#20161,.F.);
#28457=ORIENTED_EDGE('',*,*,#20124,.F.);
#28458=ORIENTED_EDGE('',*,*,#19988,.F.);
#28459=ORIENTED_EDGE('',*,*,#20125,.F.);
#28460=ORIENTED_EDGE('',*,*,#20161,.T.);
#28461=ORIENTED_EDGE('',*,*,#20159,.T.);
#28462=ORIENTED_EDGE('',*,*,#19986,.F.);
#28463=ORIENTED_EDGE('',*,*,#20162,.T.);
#28464=ORIENTED_EDGE('',*,*,#20163,.F.);
#28465=ORIENTED_EDGE('',*,*,#20126,.F.);
#28466=ORIENTED_EDGE('',*,*,#20127,.F.);
#28467=ORIENTED_EDGE('',*,*,#20163,.T.);
#28468=ORIENTED_EDGE('',*,*,#20164,.T.);
#28469=ORIENTED_EDGE('',*,*,#19984,.F.);
#28470=ORIENTED_EDGE('',*,*,#19985,.F.);
#28471=ORIENTED_EDGE('',*,*,#20164,.F.);
#28472=ORIENTED_EDGE('',*,*,#20162,.F.);
#28473=ORIENTED_EDGE('',*,*,#19981,.F.);
#28474=ORIENTED_EDGE('',*,*,#20165,.F.);
#28475=ORIENTED_EDGE('',*,*,#20166,.F.);
#28476=ORIENTED_EDGE('',*,*,#19982,.F.);
#28477=ORIENTED_EDGE('',*,*,#20166,.T.);
#28478=ORIENTED_EDGE('',*,*,#20167,.F.);
#28479=ORIENTED_EDGE('',*,*,#20128,.F.);
#28480=ORIENTED_EDGE('',*,*,#19980,.F.);
#28481=ORIENTED_EDGE('',*,*,#20129,.F.);
#28482=ORIENTED_EDGE('',*,*,#20167,.T.);
#28483=ORIENTED_EDGE('',*,*,#20165,.T.);
#28484=ORIENTED_EDGE('',*,*,#19978,.F.);
#28485=ORIENTED_EDGE('',*,*,#20168,.T.);
#28486=ORIENTED_EDGE('',*,*,#20169,.F.);
#28487=ORIENTED_EDGE('',*,*,#20130,.F.);
#28488=ORIENTED_EDGE('',*,*,#20131,.F.);
#28489=ORIENTED_EDGE('',*,*,#20169,.T.);
#28490=ORIENTED_EDGE('',*,*,#20170,.T.);
#28491=ORIENTED_EDGE('',*,*,#19976,.F.);
#28492=ORIENTED_EDGE('',*,*,#19977,.F.);
#28493=ORIENTED_EDGE('',*,*,#20170,.F.);
#28494=ORIENTED_EDGE('',*,*,#20168,.F.);
#28495=ORIENTED_EDGE('',*,*,#19973,.F.);
#28496=ORIENTED_EDGE('',*,*,#20171,.F.);
#28497=ORIENTED_EDGE('',*,*,#20172,.F.);
#28498=ORIENTED_EDGE('',*,*,#19974,.F.);
#28499=ORIENTED_EDGE('',*,*,#20172,.T.);
#28500=ORIENTED_EDGE('',*,*,#20173,.F.);
#28501=ORIENTED_EDGE('',*,*,#20132,.F.);
#28502=ORIENTED_EDGE('',*,*,#19972,.F.);
#28503=ORIENTED_EDGE('',*,*,#20133,.F.);
#28504=ORIENTED_EDGE('',*,*,#20173,.T.);
#28505=ORIENTED_EDGE('',*,*,#20171,.T.);
#28506=ORIENTED_EDGE('',*,*,#19970,.F.);
#28507=ORIENTED_EDGE('',*,*,#20174,.T.);
#28508=ORIENTED_EDGE('',*,*,#20175,.F.);
#28509=ORIENTED_EDGE('',*,*,#20134,.F.);
#28510=ORIENTED_EDGE('',*,*,#20135,.F.);
#28511=ORIENTED_EDGE('',*,*,#20175,.T.);
#28512=ORIENTED_EDGE('',*,*,#20176,.T.);
#28513=ORIENTED_EDGE('',*,*,#19968,.F.);
#28514=ORIENTED_EDGE('',*,*,#19969,.F.);
#28515=ORIENTED_EDGE('',*,*,#20176,.F.);
#28516=ORIENTED_EDGE('',*,*,#20174,.F.);
#28517=ORIENTED_EDGE('',*,*,#19965,.F.);
#28518=ORIENTED_EDGE('',*,*,#20177,.F.);
#28519=ORIENTED_EDGE('',*,*,#20178,.F.);
#28520=ORIENTED_EDGE('',*,*,#19966,.F.);
#28521=ORIENTED_EDGE('',*,*,#20178,.T.);
#28522=ORIENTED_EDGE('',*,*,#20179,.F.);
#28523=ORIENTED_EDGE('',*,*,#20136,.F.);
#28524=ORIENTED_EDGE('',*,*,#19964,.F.);
#28525=ORIENTED_EDGE('',*,*,#20137,.F.);
#28526=ORIENTED_EDGE('',*,*,#20179,.T.);
#28527=ORIENTED_EDGE('',*,*,#20177,.T.);
#28528=ORIENTED_EDGE('',*,*,#19962,.F.);
#28529=ORIENTED_EDGE('',*,*,#20180,.T.);
#28530=ORIENTED_EDGE('',*,*,#20181,.F.);
#28531=ORIENTED_EDGE('',*,*,#20138,.F.);
#28532=ORIENTED_EDGE('',*,*,#20139,.F.);
#28533=ORIENTED_EDGE('',*,*,#20181,.T.);
#28534=ORIENTED_EDGE('',*,*,#20182,.T.);
#28535=ORIENTED_EDGE('',*,*,#19960,.F.);
#28536=ORIENTED_EDGE('',*,*,#19961,.F.);
#28537=ORIENTED_EDGE('',*,*,#20182,.F.);
#28538=ORIENTED_EDGE('',*,*,#20180,.F.);
#28539=ORIENTED_EDGE('',*,*,#19957,.F.);
#28540=ORIENTED_EDGE('',*,*,#20183,.F.);
#28541=ORIENTED_EDGE('',*,*,#20184,.F.);
#28542=ORIENTED_EDGE('',*,*,#19958,.F.);
#28543=ORIENTED_EDGE('',*,*,#20184,.T.);
#28544=ORIENTED_EDGE('',*,*,#20185,.F.);
#28545=ORIENTED_EDGE('',*,*,#20140,.F.);
#28546=ORIENTED_EDGE('',*,*,#19956,.F.);
#28547=ORIENTED_EDGE('',*,*,#20141,.F.);
#28548=ORIENTED_EDGE('',*,*,#20185,.T.);
#28549=ORIENTED_EDGE('',*,*,#20183,.T.);
#28550=ORIENTED_EDGE('',*,*,#19954,.F.);
#28551=ORIENTED_EDGE('',*,*,#20186,.T.);
#28552=ORIENTED_EDGE('',*,*,#20187,.F.);
#28553=ORIENTED_EDGE('',*,*,#20142,.F.);
#28554=ORIENTED_EDGE('',*,*,#20143,.F.);
#28555=ORIENTED_EDGE('',*,*,#20187,.T.);
#28556=ORIENTED_EDGE('',*,*,#20188,.T.);
#28557=ORIENTED_EDGE('',*,*,#19952,.F.);
#28558=ORIENTED_EDGE('',*,*,#19953,.F.);
#28559=ORIENTED_EDGE('',*,*,#20188,.F.);
#28560=ORIENTED_EDGE('',*,*,#20186,.F.);
#28561=ORIENTED_EDGE('',*,*,#19949,.F.);
#28562=ORIENTED_EDGE('',*,*,#20189,.F.);
#28563=ORIENTED_EDGE('',*,*,#20190,.F.);
#28564=ORIENTED_EDGE('',*,*,#19950,.F.);
#28565=ORIENTED_EDGE('',*,*,#20190,.T.);
#28566=ORIENTED_EDGE('',*,*,#20191,.F.);
#28567=ORIENTED_EDGE('',*,*,#20144,.F.);
#28568=ORIENTED_EDGE('',*,*,#19948,.F.);
#28569=ORIENTED_EDGE('',*,*,#20145,.F.);
#28570=ORIENTED_EDGE('',*,*,#20191,.T.);
#28571=ORIENTED_EDGE('',*,*,#20189,.T.);
#28572=ORIENTED_EDGE('',*,*,#19946,.F.);
#28573=ORIENTED_EDGE('',*,*,#20192,.T.);
#28574=ORIENTED_EDGE('',*,*,#20193,.F.);
#28575=ORIENTED_EDGE('',*,*,#20146,.F.);
#28576=ORIENTED_EDGE('',*,*,#20147,.F.);
#28577=ORIENTED_EDGE('',*,*,#20193,.T.);
#28578=ORIENTED_EDGE('',*,*,#20194,.T.);
#28579=ORIENTED_EDGE('',*,*,#19944,.F.);
#28580=ORIENTED_EDGE('',*,*,#19945,.F.);
#28581=ORIENTED_EDGE('',*,*,#20194,.F.);
#28582=ORIENTED_EDGE('',*,*,#20192,.F.);
#28583=ORIENTED_EDGE('',*,*,#19941,.F.);
#28584=ORIENTED_EDGE('',*,*,#20195,.F.);
#28585=ORIENTED_EDGE('',*,*,#20196,.F.);
#28586=ORIENTED_EDGE('',*,*,#19942,.F.);
#28587=ORIENTED_EDGE('',*,*,#20196,.T.);
#28588=ORIENTED_EDGE('',*,*,#20197,.F.);
#28589=ORIENTED_EDGE('',*,*,#20148,.F.);
#28590=ORIENTED_EDGE('',*,*,#19940,.F.);
#28591=ORIENTED_EDGE('',*,*,#20149,.F.);
#28592=ORIENTED_EDGE('',*,*,#20197,.T.);
#28593=ORIENTED_EDGE('',*,*,#20195,.T.);
#28594=ORIENTED_EDGE('',*,*,#19938,.F.);
#28595=ORIENTED_EDGE('',*,*,#20198,.T.);
#28596=ORIENTED_EDGE('',*,*,#20199,.F.);
#28597=ORIENTED_EDGE('',*,*,#20150,.F.);
#28598=ORIENTED_EDGE('',*,*,#20083,.F.);
#28599=ORIENTED_EDGE('',*,*,#20199,.T.);
#28600=ORIENTED_EDGE('',*,*,#20200,.T.);
#28601=ORIENTED_EDGE('',*,*,#20077,.F.);
#28602=ORIENTED_EDGE('',*,*,#19933,.F.);
#28603=ORIENTED_EDGE('',*,*,#20200,.F.);
#28604=ORIENTED_EDGE('',*,*,#20198,.F.);
#28605=ORIENTED_EDGE('',*,*,#19937,.F.);
#28606=ORIENTED_EDGE('',*,*,#20074,.F.);
#28607=ORIENTED_EDGE('',*,*,#20201,.F.);
#28608=ORIENTED_EDGE('',*,*,#20202,.F.);
#28609=ORIENTED_EDGE('',*,*,#20075,.F.);
#28610=ORIENTED_EDGE('',*,*,#20202,.T.);
#28611=ORIENTED_EDGE('',*,*,#20203,.F.);
#28612=ORIENTED_EDGE('',*,*,#20084,.F.);
#28613=ORIENTED_EDGE('',*,*,#20073,.F.);
#28614=ORIENTED_EDGE('',*,*,#20085,.F.);
#28615=ORIENTED_EDGE('',*,*,#20203,.T.);
#28616=ORIENTED_EDGE('',*,*,#20201,.T.);
#28617=ORIENTED_EDGE('',*,*,#20071,.F.);
#28618=ORIENTED_EDGE('',*,*,#20204,.T.);
#28619=ORIENTED_EDGE('',*,*,#20205,.F.);
#28620=ORIENTED_EDGE('',*,*,#20086,.F.);
#28621=ORIENTED_EDGE('',*,*,#20087,.F.);
#28622=ORIENTED_EDGE('',*,*,#20205,.T.);
#28623=ORIENTED_EDGE('',*,*,#20206,.T.);
#28624=ORIENTED_EDGE('',*,*,#20069,.F.);
#28625=ORIENTED_EDGE('',*,*,#20070,.F.);
#28626=ORIENTED_EDGE('',*,*,#20206,.F.);
#28627=ORIENTED_EDGE('',*,*,#20204,.F.);
#28628=ORIENTED_EDGE('',*,*,#20066,.F.);
#28629=ORIENTED_EDGE('',*,*,#20207,.F.);
#28630=ORIENTED_EDGE('',*,*,#20208,.F.);
#28631=ORIENTED_EDGE('',*,*,#20067,.F.);
#28632=ORIENTED_EDGE('',*,*,#20208,.T.);
#28633=ORIENTED_EDGE('',*,*,#20209,.F.);
#28634=ORIENTED_EDGE('',*,*,#20088,.F.);
#28635=ORIENTED_EDGE('',*,*,#20065,.F.);
#28636=ORIENTED_EDGE('',*,*,#20089,.F.);
#28637=ORIENTED_EDGE('',*,*,#20209,.T.);
#28638=ORIENTED_EDGE('',*,*,#20207,.T.);
#28639=ORIENTED_EDGE('',*,*,#20063,.F.);
#28640=ORIENTED_EDGE('',*,*,#20210,.T.);
#28641=ORIENTED_EDGE('',*,*,#20211,.F.);
#28642=ORIENTED_EDGE('',*,*,#20090,.F.);
#28643=ORIENTED_EDGE('',*,*,#20091,.F.);
#28644=ORIENTED_EDGE('',*,*,#20211,.T.);
#28645=ORIENTED_EDGE('',*,*,#20212,.T.);
#28646=ORIENTED_EDGE('',*,*,#20061,.F.);
#28647=ORIENTED_EDGE('',*,*,#20062,.F.);
#28648=ORIENTED_EDGE('',*,*,#20212,.F.);
#28649=ORIENTED_EDGE('',*,*,#20210,.F.);
#28650=ORIENTED_EDGE('',*,*,#20058,.F.);
#28651=ORIENTED_EDGE('',*,*,#20213,.F.);
#28652=ORIENTED_EDGE('',*,*,#20214,.F.);
#28653=ORIENTED_EDGE('',*,*,#20059,.F.);
#28654=ORIENTED_EDGE('',*,*,#20214,.T.);
#28655=ORIENTED_EDGE('',*,*,#20215,.F.);
#28656=ORIENTED_EDGE('',*,*,#20092,.F.);
#28657=ORIENTED_EDGE('',*,*,#20057,.F.);
#28658=ORIENTED_EDGE('',*,*,#20093,.F.);
#28659=ORIENTED_EDGE('',*,*,#20215,.T.);
#28660=ORIENTED_EDGE('',*,*,#20213,.T.);
#28661=ORIENTED_EDGE('',*,*,#20055,.F.);
#28662=ORIENTED_EDGE('',*,*,#20216,.T.);
#28663=ORIENTED_EDGE('',*,*,#20217,.F.);
#28664=ORIENTED_EDGE('',*,*,#20094,.F.);
#28665=ORIENTED_EDGE('',*,*,#20095,.F.);
#28666=ORIENTED_EDGE('',*,*,#20217,.T.);
#28667=ORIENTED_EDGE('',*,*,#20218,.T.);
#28668=ORIENTED_EDGE('',*,*,#20053,.F.);
#28669=ORIENTED_EDGE('',*,*,#20054,.F.);
#28670=ORIENTED_EDGE('',*,*,#20218,.F.);
#28671=ORIENTED_EDGE('',*,*,#20216,.F.);
#28672=ORIENTED_EDGE('',*,*,#20050,.F.);
#28673=ORIENTED_EDGE('',*,*,#20219,.F.);
#28674=ORIENTED_EDGE('',*,*,#20220,.F.);
#28675=ORIENTED_EDGE('',*,*,#20051,.F.);
#28676=ORIENTED_EDGE('',*,*,#20220,.T.);
#28677=ORIENTED_EDGE('',*,*,#20221,.F.);
#28678=ORIENTED_EDGE('',*,*,#20096,.F.);
#28679=ORIENTED_EDGE('',*,*,#20049,.F.);
#28680=ORIENTED_EDGE('',*,*,#20097,.F.);
#28681=ORIENTED_EDGE('',*,*,#20221,.T.);
#28682=ORIENTED_EDGE('',*,*,#20219,.T.);
#28683=ORIENTED_EDGE('',*,*,#20047,.F.);
#28684=ORIENTED_EDGE('',*,*,#20222,.T.);
#28685=ORIENTED_EDGE('',*,*,#20223,.F.);
#28686=ORIENTED_EDGE('',*,*,#20098,.F.);
#28687=ORIENTED_EDGE('',*,*,#20099,.F.);
#28688=ORIENTED_EDGE('',*,*,#20223,.T.);
#28689=ORIENTED_EDGE('',*,*,#20224,.T.);
#28690=ORIENTED_EDGE('',*,*,#20045,.F.);
#28691=ORIENTED_EDGE('',*,*,#20046,.F.);
#28692=ORIENTED_EDGE('',*,*,#20224,.F.);
#28693=ORIENTED_EDGE('',*,*,#20222,.F.);
#28694=ORIENTED_EDGE('',*,*,#20042,.F.);
#28695=ORIENTED_EDGE('',*,*,#20225,.F.);
#28696=ORIENTED_EDGE('',*,*,#20226,.F.);
#28697=ORIENTED_EDGE('',*,*,#20043,.F.);
#28698=ORIENTED_EDGE('',*,*,#20226,.T.);
#28699=ORIENTED_EDGE('',*,*,#20227,.F.);
#28700=ORIENTED_EDGE('',*,*,#20100,.F.);
#28701=ORIENTED_EDGE('',*,*,#20041,.F.);
#28702=ORIENTED_EDGE('',*,*,#20101,.F.);
#28703=ORIENTED_EDGE('',*,*,#20227,.T.);
#28704=ORIENTED_EDGE('',*,*,#20225,.T.);
#28705=ORIENTED_EDGE('',*,*,#20039,.F.);
#28706=ORIENTED_EDGE('',*,*,#20228,.T.);
#28707=ORIENTED_EDGE('',*,*,#20229,.F.);
#28708=ORIENTED_EDGE('',*,*,#20102,.F.);
#28709=ORIENTED_EDGE('',*,*,#20103,.F.);
#28710=ORIENTED_EDGE('',*,*,#20229,.T.);
#28711=ORIENTED_EDGE('',*,*,#20230,.T.);
#28712=ORIENTED_EDGE('',*,*,#20037,.F.);
#28713=ORIENTED_EDGE('',*,*,#20038,.F.);
#28714=ORIENTED_EDGE('',*,*,#20230,.F.);
#28715=ORIENTED_EDGE('',*,*,#20228,.F.);
#28716=ORIENTED_EDGE('',*,*,#20034,.F.);
#28717=ORIENTED_EDGE('',*,*,#20231,.F.);
#28718=ORIENTED_EDGE('',*,*,#20232,.F.);
#28719=ORIENTED_EDGE('',*,*,#20035,.F.);
#28720=ORIENTED_EDGE('',*,*,#20232,.T.);
#28721=ORIENTED_EDGE('',*,*,#20233,.F.);
#28722=ORIENTED_EDGE('',*,*,#20104,.F.);
#28723=ORIENTED_EDGE('',*,*,#20033,.F.);
#28724=ORIENTED_EDGE('',*,*,#20105,.F.);
#28725=ORIENTED_EDGE('',*,*,#20233,.T.);
#28726=ORIENTED_EDGE('',*,*,#20231,.T.);
#28727=ORIENTED_EDGE('',*,*,#20031,.F.);
#28728=ORIENTED_EDGE('',*,*,#20234,.T.);
#28729=ORIENTED_EDGE('',*,*,#20235,.F.);
#28730=ORIENTED_EDGE('',*,*,#20106,.F.);
#28731=ORIENTED_EDGE('',*,*,#20107,.F.);
#28732=ORIENTED_EDGE('',*,*,#20235,.T.);
#28733=ORIENTED_EDGE('',*,*,#20236,.T.);
#28734=ORIENTED_EDGE('',*,*,#20029,.F.);
#28735=ORIENTED_EDGE('',*,*,#20030,.F.);
#28736=ORIENTED_EDGE('',*,*,#20236,.F.);
#28737=ORIENTED_EDGE('',*,*,#20234,.F.);
#28738=ORIENTED_EDGE('',*,*,#20026,.F.);
#28739=ORIENTED_EDGE('',*,*,#20237,.F.);
#28740=ORIENTED_EDGE('',*,*,#20238,.F.);
#28741=ORIENTED_EDGE('',*,*,#20027,.F.);
#28742=ORIENTED_EDGE('',*,*,#20238,.T.);
#28743=ORIENTED_EDGE('',*,*,#20239,.F.);
#28744=ORIENTED_EDGE('',*,*,#20108,.F.);
#28745=ORIENTED_EDGE('',*,*,#20025,.F.);
#28746=ORIENTED_EDGE('',*,*,#20109,.F.);
#28747=ORIENTED_EDGE('',*,*,#20239,.T.);
#28748=ORIENTED_EDGE('',*,*,#20237,.T.);
#28749=ORIENTED_EDGE('',*,*,#20023,.F.);
#28750=ORIENTED_EDGE('',*,*,#20240,.T.);
#28751=ORIENTED_EDGE('',*,*,#20241,.F.);
#28752=ORIENTED_EDGE('',*,*,#20110,.F.);
#28753=ORIENTED_EDGE('',*,*,#20111,.F.);
#28754=ORIENTED_EDGE('',*,*,#20241,.T.);
#28755=ORIENTED_EDGE('',*,*,#20242,.T.);
#28756=ORIENTED_EDGE('',*,*,#20021,.F.);
#28757=ORIENTED_EDGE('',*,*,#20022,.F.);
#28758=ORIENTED_EDGE('',*,*,#20242,.F.);
#28759=ORIENTED_EDGE('',*,*,#20240,.F.);
#28760=ORIENTED_EDGE('',*,*,#20018,.F.);
#28761=ORIENTED_EDGE('',*,*,#20243,.F.);
#28762=ORIENTED_EDGE('',*,*,#20244,.F.);
#28763=ORIENTED_EDGE('',*,*,#20019,.F.);
#28764=ORIENTED_EDGE('',*,*,#20244,.T.);
#28765=ORIENTED_EDGE('',*,*,#20245,.F.);
#28766=ORIENTED_EDGE('',*,*,#20112,.F.);
#28767=ORIENTED_EDGE('',*,*,#20017,.F.);
#28768=ORIENTED_EDGE('',*,*,#20113,.F.);
#28769=ORIENTED_EDGE('',*,*,#20245,.T.);
#28770=ORIENTED_EDGE('',*,*,#20243,.T.);
#28771=ORIENTED_EDGE('',*,*,#20015,.F.);
#28772=ORIENTED_EDGE('',*,*,#20246,.T.);
#28773=ORIENTED_EDGE('',*,*,#20247,.F.);
#28774=ORIENTED_EDGE('',*,*,#20114,.F.);
#28775=ORIENTED_EDGE('',*,*,#20115,.F.);
#28776=ORIENTED_EDGE('',*,*,#20247,.T.);
#28777=ORIENTED_EDGE('',*,*,#20248,.T.);
#28778=ORIENTED_EDGE('',*,*,#20013,.F.);
#28779=ORIENTED_EDGE('',*,*,#20014,.F.);
#28780=ORIENTED_EDGE('',*,*,#20248,.F.);
#28781=ORIENTED_EDGE('',*,*,#20246,.F.);
#28782=ORIENTED_EDGE('',*,*,#20010,.F.);
#28783=ORIENTED_EDGE('',*,*,#20249,.F.);
#28784=ORIENTED_EDGE('',*,*,#20250,.F.);
#28785=ORIENTED_EDGE('',*,*,#20011,.F.);
#28786=ORIENTED_EDGE('',*,*,#20250,.T.);
#28787=ORIENTED_EDGE('',*,*,#20251,.F.);
#28788=ORIENTED_EDGE('',*,*,#20116,.F.);
#28789=ORIENTED_EDGE('',*,*,#20009,.F.);
#28790=ORIENTED_EDGE('',*,*,#20117,.F.);
#28791=ORIENTED_EDGE('',*,*,#20251,.T.);
#28792=ORIENTED_EDGE('',*,*,#20249,.T.);
#28793=ORIENTED_EDGE('',*,*,#20007,.F.);
#28794=ORIENTED_EDGE('',*,*,#20252,.T.);
#28795=ORIENTED_EDGE('',*,*,#20253,.F.);
#28796=ORIENTED_EDGE('',*,*,#20118,.F.);
#28797=ORIENTED_EDGE('',*,*,#20119,.F.);
#28798=ORIENTED_EDGE('',*,*,#20253,.T.);
#28799=ORIENTED_EDGE('',*,*,#20254,.T.);
#28800=ORIENTED_EDGE('',*,*,#20005,.F.);
#28801=ORIENTED_EDGE('',*,*,#20006,.F.);
#28802=ORIENTED_EDGE('',*,*,#20254,.F.);
#28803=ORIENTED_EDGE('',*,*,#20252,.F.);
#28804=ORIENTED_EDGE('',*,*,#19922,.T.);
#28805=ORIENTED_EDGE('',*,*,#20255,.T.);
#28806=ORIENTED_EDGE('',*,*,#19935,.T.);
#28807=ORIENTED_EDGE('',*,*,#19936,.T.);
#28808=ORIENTED_EDGE('',*,*,#20255,.F.);
#28809=ORIENTED_EDGE('',*,*,#20152,.F.);
#28810=ORIENTED_EDGE('',*,*,#20256,.T.);
#28811=ORIENTED_EDGE('',*,*,#20257,.F.);
#28812=ORIENTED_EDGE('',*,*,#20258,.F.);
#28813=ORIENTED_EDGE('',*,*,#20259,.F.);
#28814=ORIENTED_EDGE('',*,*,#20260,.F.);
#28815=ORIENTED_EDGE('',*,*,#20261,.F.);
#28816=ORIENTED_EDGE('',*,*,#20262,.F.);
#28817=ORIENTED_EDGE('',*,*,#20263,.F.);
#28818=ORIENTED_EDGE('',*,*,#20264,.F.);
#28819=ORIENTED_EDGE('',*,*,#20265,.F.);
#28820=ORIENTED_EDGE('',*,*,#20266,.F.);
#28821=ORIENTED_EDGE('',*,*,#20267,.F.);
#28822=ORIENTED_EDGE('',*,*,#20268,.F.);
#28823=ORIENTED_EDGE('',*,*,#20269,.F.);
#28824=ORIENTED_EDGE('',*,*,#20270,.F.);
#28825=ORIENTED_EDGE('',*,*,#20271,.F.);
#28826=ORIENTED_EDGE('',*,*,#20272,.F.);
#28827=ORIENTED_EDGE('',*,*,#20273,.F.);
#28828=ORIENTED_EDGE('',*,*,#20274,.F.);
#28829=ORIENTED_EDGE('',*,*,#20275,.T.);
#28830=ORIENTED_EDGE('',*,*,#20256,.F.);
#28831=ORIENTED_EDGE('',*,*,#20275,.F.);
#28832=ORIENTED_EDGE('',*,*,#20276,.F.);
#28833=ORIENTED_EDGE('',*,*,#20273,.T.);
#28834=ORIENTED_EDGE('',*,*,#20277,.F.);
#28835=ORIENTED_EDGE('',*,*,#20278,.F.);
#28836=ORIENTED_EDGE('',*,*,#20279,.F.);
#28837=ORIENTED_EDGE('',*,*,#20280,.F.);
#28838=ORIENTED_EDGE('',*,*,#20281,.F.);
#28839=ORIENTED_EDGE('',*,*,#20270,.T.);
#28840=ORIENTED_EDGE('',*,*,#20282,.F.);
#28841=ORIENTED_EDGE('',*,*,#20258,.T.);
#28842=ORIENTED_EDGE('',*,*,#20283,.F.);
#28843=ORIENTED_EDGE('',*,*,#20284,.F.);
#28844=ORIENTED_EDGE('',*,*,#20285,.F.);
#28845=ORIENTED_EDGE('',*,*,#20286,.F.);
#28846=ORIENTED_EDGE('',*,*,#20287,.F.);
#28847=ORIENTED_EDGE('',*,*,#20267,.T.);
#28848=ORIENTED_EDGE('',*,*,#20288,.F.);
#28849=ORIENTED_EDGE('',*,*,#20261,.T.);
#28850=ORIENTED_EDGE('',*,*,#20289,.F.);
#28851=ORIENTED_EDGE('',*,*,#20290,.F.);
#28852=ORIENTED_EDGE('',*,*,#20291,.F.);
#28853=ORIENTED_EDGE('',*,*,#20292,.F.);
#28854=ORIENTED_EDGE('',*,*,#20293,.F.);
#28855=ORIENTED_EDGE('',*,*,#20264,.T.);
#28856=ORIENTED_EDGE('',*,*,#20262,.T.);
#28857=ORIENTED_EDGE('',*,*,#20288,.T.);
#28858=ORIENTED_EDGE('',*,*,#20294,.F.);
#28859=ORIENTED_EDGE('',*,*,#20289,.T.);
#28860=ORIENTED_EDGE('',*,*,#20260,.T.);
#28861=ORIENTED_EDGE('',*,*,#20295,.T.);
#28862=ORIENTED_EDGE('',*,*,#20296,.T.);
#28863=ORIENTED_EDGE('',*,*,#20297,.F.);
#28864=ORIENTED_EDGE('',*,*,#20259,.T.);
#28865=ORIENTED_EDGE('',*,*,#20282,.T.);
#28866=ORIENTED_EDGE('',*,*,#20298,.F.);
#28867=ORIENTED_EDGE('',*,*,#20283,.T.);
#28868=ORIENTED_EDGE('',*,*,#20257,.T.);
#28869=ORIENTED_EDGE('',*,*,#20299,.T.);
#28870=ORIENTED_EDGE('',*,*,#20300,.T.);
#28871=ORIENTED_EDGE('',*,*,#20295,.F.);
#28872=ORIENTED_EDGE('',*,*,#20274,.T.);
#28873=ORIENTED_EDGE('',*,*,#20276,.T.);
#28874=ORIENTED_EDGE('',*,*,#20301,.F.);
#28875=ORIENTED_EDGE('',*,*,#20277,.T.);
#28876=ORIENTED_EDGE('',*,*,#20272,.T.);
#28877=ORIENTED_EDGE('',*,*,#20302,.T.);
#28878=ORIENTED_EDGE('',*,*,#20303,.T.);
#28879=ORIENTED_EDGE('',*,*,#20299,.F.);
#28880=ORIENTED_EDGE('',*,*,#20278,.T.);
#28881=ORIENTED_EDGE('',*,*,#20301,.T.);
#28882=ORIENTED_EDGE('',*,*,#20284,.T.);
#28883=ORIENTED_EDGE('',*,*,#20298,.T.);
#28884=ORIENTED_EDGE('',*,*,#20280,.T.);
#28885=ORIENTED_EDGE('',*,*,#20304,.T.);
#28886=ORIENTED_EDGE('',*,*,#20290,.T.);
#28887=ORIENTED_EDGE('',*,*,#20294,.T.);
#28888=ORIENTED_EDGE('',*,*,#20286,.T.);
#28889=ORIENTED_EDGE('',*,*,#20305,.T.);
#28890=ORIENTED_EDGE('',*,*,#20292,.T.);
#28891=ORIENTED_EDGE('',*,*,#20306,.T.);
#28892=ORIENTED_EDGE('',*,*,#20307,.F.);
#28893=ORIENTED_EDGE('',*,*,#20308,.F.);
#28894=ORIENTED_EDGE('',*,*,#20309,.F.);
#28895=ORIENTED_EDGE('',*,*,#20310,.F.);
#28896=ORIENTED_EDGE('',*,*,#20303,.F.);
#28897=ORIENTED_EDGE('',*,*,#20311,.F.);
#28898=ORIENTED_EDGE('',*,*,#20300,.F.);
#28899=ORIENTED_EDGE('',*,*,#20312,.F.);
#28900=ORIENTED_EDGE('',*,*,#20296,.F.);
#28901=ORIENTED_EDGE('',*,*,#20313,.F.);
#28902=ORIENTED_EDGE('',*,*,#20314,.F.);
#28903=ORIENTED_EDGE('',*,*,#20315,.F.);
#28904=ORIENTED_EDGE('',*,*,#20316,.T.);
#28905=ORIENTED_EDGE('',*,*,#20311,.T.);
#28906=ORIENTED_EDGE('',*,*,#20310,.T.);
#28907=ORIENTED_EDGE('',*,*,#20308,.T.);
#28908=ORIENTED_EDGE('',*,*,#20315,.T.);
#28909=ORIENTED_EDGE('',*,*,#20313,.T.);
#28910=ORIENTED_EDGE('',*,*,#20312,.T.);
#28911=ORIENTED_EDGE('',*,*,#20316,.F.);
#28912=ORIENTED_EDGE('',*,*,#20266,.T.);
#28913=ORIENTED_EDGE('',*,*,#20317,.T.);
#28914=ORIENTED_EDGE('',*,*,#20307,.T.);
#28915=ORIENTED_EDGE('',*,*,#20318,.F.);
#28916=ORIENTED_EDGE('',*,*,#20268,.T.);
#28917=ORIENTED_EDGE('',*,*,#20287,.T.);
#28918=ORIENTED_EDGE('',*,*,#20305,.F.);
#28919=ORIENTED_EDGE('',*,*,#20285,.T.);
#28920=ORIENTED_EDGE('',*,*,#20263,.T.);
#28921=ORIENTED_EDGE('',*,*,#20297,.T.);
#28922=ORIENTED_EDGE('',*,*,#20314,.T.);
#28923=ORIENTED_EDGE('',*,*,#20317,.F.);
#28924=ORIENTED_EDGE('',*,*,#20265,.T.);
#28925=ORIENTED_EDGE('',*,*,#20293,.T.);
#28926=ORIENTED_EDGE('',*,*,#20306,.F.);
#28927=ORIENTED_EDGE('',*,*,#20291,.T.);
#28928=ORIENTED_EDGE('',*,*,#20269,.T.);
#28929=ORIENTED_EDGE('',*,*,#20318,.T.);
#28930=ORIENTED_EDGE('',*,*,#20309,.T.);
#28931=ORIENTED_EDGE('',*,*,#20302,.F.);
#28932=ORIENTED_EDGE('',*,*,#20271,.T.);
#28933=ORIENTED_EDGE('',*,*,#20281,.T.);
#28934=ORIENTED_EDGE('',*,*,#20304,.F.);
#28935=ORIENTED_EDGE('',*,*,#20279,.T.);
#28936=ORIENTED_EDGE('',*,*,#20319,.F.);
#28937=ORIENTED_EDGE('',*,*,#20320,.T.);
#28938=ORIENTED_EDGE('',*,*,#20321,.F.);
#28939=ORIENTED_EDGE('',*,*,#20322,.T.);
#28940=ORIENTED_EDGE('',*,*,#20323,.F.);
#28941=ORIENTED_EDGE('',*,*,#20324,.T.);
#28942=ORIENTED_EDGE('',*,*,#20319,.T.);
#28943=ORIENTED_EDGE('',*,*,#20325,.T.);
#28944=ORIENTED_EDGE('',*,*,#20326,.F.);
#28945=ORIENTED_EDGE('',*,*,#20327,.T.);
#28946=ORIENTED_EDGE('',*,*,#20323,.T.);
#28947=ORIENTED_EDGE('',*,*,#20328,.T.);
#28948=ORIENTED_EDGE('',*,*,#20329,.F.);
#28949=ORIENTED_EDGE('',*,*,#20330,.T.);
#28950=ORIENTED_EDGE('',*,*,#20326,.T.);
#28951=ORIENTED_EDGE('',*,*,#20331,.T.);
#28952=ORIENTED_EDGE('',*,*,#20332,.T.);
#28953=ORIENTED_EDGE('',*,*,#20333,.F.);
#28954=ORIENTED_EDGE('',*,*,#20334,.T.);
#28955=ORIENTED_EDGE('',*,*,#20329,.T.);
#28956=ORIENTED_EDGE('',*,*,#20335,.T.);
#28957=ORIENTED_EDGE('',*,*,#20336,.F.);
#28958=ORIENTED_EDGE('',*,*,#20337,.T.);
#28959=ORIENTED_EDGE('',*,*,#20333,.T.);
#28960=ORIENTED_EDGE('',*,*,#20338,.T.);
#28961=ORIENTED_EDGE('',*,*,#20339,.F.);
#28962=ORIENTED_EDGE('',*,*,#20340,.T.);
#28963=ORIENTED_EDGE('',*,*,#20341,.T.);
#28964=ORIENTED_EDGE('',*,*,#20336,.T.);
#28965=ORIENTED_EDGE('',*,*,#20342,.T.);
#28966=ORIENTED_EDGE('',*,*,#20343,.F.);
#28967=ORIENTED_EDGE('',*,*,#20344,.T.);
#28968=ORIENTED_EDGE('',*,*,#20339,.T.);
#28969=ORIENTED_EDGE('',*,*,#20345,.T.);
#28970=ORIENTED_EDGE('',*,*,#20346,.F.);
#28971=ORIENTED_EDGE('',*,*,#20347,.T.);
#28972=ORIENTED_EDGE('',*,*,#20343,.T.);
#28973=ORIENTED_EDGE('',*,*,#20348,.T.);
#28974=ORIENTED_EDGE('',*,*,#20349,.F.);
#28975=ORIENTED_EDGE('',*,*,#20350,.T.);
#28976=ORIENTED_EDGE('',*,*,#20346,.T.);
#28977=ORIENTED_EDGE('',*,*,#20351,.T.);
#28978=ORIENTED_EDGE('',*,*,#20352,.T.);
#28979=ORIENTED_EDGE('',*,*,#20353,.F.);
#28980=ORIENTED_EDGE('',*,*,#20354,.T.);
#28981=ORIENTED_EDGE('',*,*,#20349,.T.);
#28982=ORIENTED_EDGE('',*,*,#20355,.T.);
#28983=ORIENTED_EDGE('',*,*,#20356,.F.);
#28984=ORIENTED_EDGE('',*,*,#20357,.T.);
#28985=ORIENTED_EDGE('',*,*,#20353,.T.);
#28986=ORIENTED_EDGE('',*,*,#20358,.T.);
#28987=ORIENTED_EDGE('',*,*,#20359,.F.);
#28988=ORIENTED_EDGE('',*,*,#20360,.T.);
#28989=ORIENTED_EDGE('',*,*,#20356,.T.);
#28990=ORIENTED_EDGE('',*,*,#20361,.T.);
#28991=ORIENTED_EDGE('',*,*,#20362,.F.);
#28992=ORIENTED_EDGE('',*,*,#20363,.T.);
#28993=ORIENTED_EDGE('',*,*,#20359,.T.);
#28994=ORIENTED_EDGE('',*,*,#20364,.T.);
#28995=ORIENTED_EDGE('',*,*,#20365,.F.);
#28996=ORIENTED_EDGE('',*,*,#20366,.T.);
#28997=ORIENTED_EDGE('',*,*,#20362,.T.);
#28998=ORIENTED_EDGE('',*,*,#20367,.T.);
#28999=ORIENTED_EDGE('',*,*,#20368,.F.);
#29000=ORIENTED_EDGE('',*,*,#20369,.T.);
#29001=ORIENTED_EDGE('',*,*,#20370,.T.);
#29002=ORIENTED_EDGE('',*,*,#20365,.T.);
#29003=ORIENTED_EDGE('',*,*,#20371,.T.);
#29004=ORIENTED_EDGE('',*,*,#20372,.F.);
#29005=ORIENTED_EDGE('',*,*,#20373,.T.);
#29006=ORIENTED_EDGE('',*,*,#20368,.T.);
#29007=ORIENTED_EDGE('',*,*,#20374,.T.);
#29008=ORIENTED_EDGE('',*,*,#20375,.F.);
#29009=ORIENTED_EDGE('',*,*,#20376,.T.);
#29010=ORIENTED_EDGE('',*,*,#20372,.T.);
#29011=ORIENTED_EDGE('',*,*,#20377,.T.);
#29012=ORIENTED_EDGE('',*,*,#20378,.F.);
#29013=ORIENTED_EDGE('',*,*,#20379,.T.);
#29014=ORIENTED_EDGE('',*,*,#20375,.T.);
#29015=ORIENTED_EDGE('',*,*,#20380,.T.);
#29016=ORIENTED_EDGE('',*,*,#20381,.F.);
#29017=ORIENTED_EDGE('',*,*,#20382,.F.);
#29018=ORIENTED_EDGE('',*,*,#20383,.F.);
#29019=ORIENTED_EDGE('',*,*,#20384,.T.);
#29020=ORIENTED_EDGE('',*,*,#20385,.F.);
#29021=ORIENTED_EDGE('',*,*,#20386,.F.);
#29022=ORIENTED_EDGE('',*,*,#20387,.F.);
#29023=ORIENTED_EDGE('',*,*,#20381,.T.);
#29024=ORIENTED_EDGE('',*,*,#20388,.T.);
#29025=ORIENTED_EDGE('',*,*,#20389,.F.);
#29026=ORIENTED_EDGE('',*,*,#20390,.F.);
#29027=ORIENTED_EDGE('',*,*,#20385,.T.);
#29028=ORIENTED_EDGE('',*,*,#20391,.T.);
#29029=ORIENTED_EDGE('',*,*,#20392,.F.);
#29030=ORIENTED_EDGE('',*,*,#20393,.F.);
#29031=ORIENTED_EDGE('',*,*,#20389,.T.);
#29032=ORIENTED_EDGE('',*,*,#20394,.T.);
#29033=ORIENTED_EDGE('',*,*,#20395,.F.);
#29034=ORIENTED_EDGE('',*,*,#20396,.F.);
#29035=ORIENTED_EDGE('',*,*,#20392,.T.);
#29036=ORIENTED_EDGE('',*,*,#20397,.T.);
#29037=ORIENTED_EDGE('',*,*,#20398,.F.);
#29038=ORIENTED_EDGE('',*,*,#20399,.F.);
#29039=ORIENTED_EDGE('',*,*,#20400,.F.);
#29040=ORIENTED_EDGE('',*,*,#20395,.T.);
#29041=ORIENTED_EDGE('',*,*,#20401,.T.);
#29042=ORIENTED_EDGE('',*,*,#20402,.F.);
#29043=ORIENTED_EDGE('',*,*,#20403,.F.);
#29044=ORIENTED_EDGE('',*,*,#20398,.T.);
#29045=ORIENTED_EDGE('',*,*,#20404,.T.);
#29046=ORIENTED_EDGE('',*,*,#20405,.F.);
#29047=ORIENTED_EDGE('',*,*,#20406,.F.);
#29048=ORIENTED_EDGE('',*,*,#20402,.T.);
#29049=ORIENTED_EDGE('',*,*,#20407,.T.);
#29050=ORIENTED_EDGE('',*,*,#20408,.F.);
#29051=ORIENTED_EDGE('',*,*,#20409,.F.);
#29052=ORIENTED_EDGE('',*,*,#20405,.T.);
#29053=ORIENTED_EDGE('',*,*,#20410,.T.);
#29054=ORIENTED_EDGE('',*,*,#20411,.F.);
#29055=ORIENTED_EDGE('',*,*,#20412,.F.);
#29056=ORIENTED_EDGE('',*,*,#20408,.T.);
#29057=ORIENTED_EDGE('',*,*,#20413,.T.);
#29058=ORIENTED_EDGE('',*,*,#20414,.F.);
#29059=ORIENTED_EDGE('',*,*,#20415,.F.);
#29060=ORIENTED_EDGE('',*,*,#20411,.T.);
#29061=ORIENTED_EDGE('',*,*,#20416,.T.);
#29062=ORIENTED_EDGE('',*,*,#20417,.F.);
#29063=ORIENTED_EDGE('',*,*,#20418,.F.);
#29064=ORIENTED_EDGE('',*,*,#20414,.T.);
#29065=ORIENTED_EDGE('',*,*,#20419,.T.);
#29066=ORIENTED_EDGE('',*,*,#20420,.F.);
#29067=ORIENTED_EDGE('',*,*,#20421,.F.);
#29068=ORIENTED_EDGE('',*,*,#20417,.T.);
#29069=ORIENTED_EDGE('',*,*,#20422,.T.);
#29070=ORIENTED_EDGE('',*,*,#20423,.F.);
#29071=ORIENTED_EDGE('',*,*,#20424,.F.);
#29072=ORIENTED_EDGE('',*,*,#20420,.T.);
#29073=ORIENTED_EDGE('',*,*,#20425,.T.);
#29074=ORIENTED_EDGE('',*,*,#20426,.F.);
#29075=ORIENTED_EDGE('',*,*,#20427,.F.);
#29076=ORIENTED_EDGE('',*,*,#20428,.F.);
#29077=ORIENTED_EDGE('',*,*,#20423,.T.);
#29078=ORIENTED_EDGE('',*,*,#20429,.T.);
#29079=ORIENTED_EDGE('',*,*,#20430,.F.);
#29080=ORIENTED_EDGE('',*,*,#20431,.F.);
#29081=ORIENTED_EDGE('',*,*,#20426,.T.);
#29082=ORIENTED_EDGE('',*,*,#20432,.T.);
#29083=ORIENTED_EDGE('',*,*,#20433,.F.);
#29084=ORIENTED_EDGE('',*,*,#20434,.F.);
#29085=ORIENTED_EDGE('',*,*,#20430,.T.);
#29086=ORIENTED_EDGE('',*,*,#20435,.T.);
#29087=ORIENTED_EDGE('',*,*,#20436,.F.);
#29088=ORIENTED_EDGE('',*,*,#20437,.F.);
#29089=ORIENTED_EDGE('',*,*,#20433,.T.);
#29090=ORIENTED_EDGE('',*,*,#20438,.T.);
#29091=ORIENTED_EDGE('',*,*,#20439,.T.);
#29092=ORIENTED_EDGE('',*,*,#20440,.F.);
#29093=ORIENTED_EDGE('',*,*,#20441,.F.);
#29094=ORIENTED_EDGE('',*,*,#20436,.T.);
#29095=ORIENTED_EDGE('',*,*,#20442,.T.);
#29096=ORIENTED_EDGE('',*,*,#20440,.T.);
#29097=ORIENTED_EDGE('',*,*,#20443,.T.);
#29098=ORIENTED_EDGE('',*,*,#20444,.F.);
#29099=ORIENTED_EDGE('',*,*,#20445,.F.);
#29100=ORIENTED_EDGE('',*,*,#20446,.F.);
#29101=ORIENTED_EDGE('',*,*,#20378,.T.);
#29102=ORIENTED_EDGE('',*,*,#20447,.T.);
#29103=ORIENTED_EDGE('',*,*,#20448,.F.);
#29104=ORIENTED_EDGE('',*,*,#20449,.T.);
#29105=ORIENTED_EDGE('',*,*,#20450,.F.);
#29106=ORIENTED_EDGE('',*,*,#20451,.T.);
#29107=ORIENTED_EDGE('',*,*,#20444,.T.);
#29108=ORIENTED_EDGE('',*,*,#20452,.T.);
#29109=ORIENTED_EDGE('',*,*,#20453,.F.);
#29110=ORIENTED_EDGE('',*,*,#20451,.F.);
#29111=ORIENTED_EDGE('',*,*,#20454,.F.);
#29112=ORIENTED_EDGE('',*,*,#20447,.F.);
#29113=ORIENTED_EDGE('',*,*,#20380,.F.);
#29114=ORIENTED_EDGE('',*,*,#20377,.F.);
#29115=ORIENTED_EDGE('',*,*,#20374,.F.);
#29116=ORIENTED_EDGE('',*,*,#20371,.F.);
#29117=ORIENTED_EDGE('',*,*,#20367,.F.);
#29118=ORIENTED_EDGE('',*,*,#20364,.F.);
#29119=ORIENTED_EDGE('',*,*,#20361,.F.);
#29120=ORIENTED_EDGE('',*,*,#20358,.F.);
#29121=ORIENTED_EDGE('',*,*,#20355,.F.);
#29122=ORIENTED_EDGE('',*,*,#20352,.F.);
#29123=ORIENTED_EDGE('',*,*,#20351,.F.);
#29124=ORIENTED_EDGE('',*,*,#20348,.F.);
#29125=ORIENTED_EDGE('',*,*,#20345,.F.);
#29126=ORIENTED_EDGE('',*,*,#20342,.F.);
#29127=ORIENTED_EDGE('',*,*,#20338,.F.);
#29128=ORIENTED_EDGE('',*,*,#20335,.F.);
#29129=ORIENTED_EDGE('',*,*,#20332,.F.);
#29130=ORIENTED_EDGE('',*,*,#20331,.F.);
#29131=ORIENTED_EDGE('',*,*,#20328,.F.);
#29132=ORIENTED_EDGE('',*,*,#20325,.F.);
#29133=ORIENTED_EDGE('',*,*,#20322,.F.);
#29134=ORIENTED_EDGE('',*,*,#20455,.F.);
#29135=ORIENTED_EDGE('',*,*,#20456,.T.);
#29136=ORIENTED_EDGE('',*,*,#20382,.T.);
#29137=ORIENTED_EDGE('',*,*,#20387,.T.);
#29138=ORIENTED_EDGE('',*,*,#20386,.T.);
#29139=ORIENTED_EDGE('',*,*,#20390,.T.);
#29140=ORIENTED_EDGE('',*,*,#20393,.T.);
#29141=ORIENTED_EDGE('',*,*,#20396,.T.);
#29142=ORIENTED_EDGE('',*,*,#20400,.T.);
#29143=ORIENTED_EDGE('',*,*,#20399,.T.);
#29144=ORIENTED_EDGE('',*,*,#20403,.T.);
#29145=ORIENTED_EDGE('',*,*,#20406,.T.);
#29146=ORIENTED_EDGE('',*,*,#20409,.T.);
#29147=ORIENTED_EDGE('',*,*,#20412,.T.);
#29148=ORIENTED_EDGE('',*,*,#20415,.T.);
#29149=ORIENTED_EDGE('',*,*,#20418,.T.);
#29150=ORIENTED_EDGE('',*,*,#20421,.T.);
#29151=ORIENTED_EDGE('',*,*,#20424,.T.);
#29152=ORIENTED_EDGE('',*,*,#20428,.T.);
#29153=ORIENTED_EDGE('',*,*,#20427,.T.);
#29154=ORIENTED_EDGE('',*,*,#20431,.T.);
#29155=ORIENTED_EDGE('',*,*,#20434,.T.);
#29156=ORIENTED_EDGE('',*,*,#20437,.T.);
#29157=ORIENTED_EDGE('',*,*,#20441,.T.);
#29158=ORIENTED_EDGE('',*,*,#20446,.T.);
#29159=ORIENTED_EDGE('',*,*,#20445,.T.);
#29160=ORIENTED_EDGE('',*,*,#20457,.F.);
#29161=ORIENTED_EDGE('',*,*,#20458,.T.);
#29162=ORIENTED_EDGE('',*,*,#20383,.T.);
#29163=ORIENTED_EDGE('',*,*,#20456,.F.);
#29164=ORIENTED_EDGE('',*,*,#20455,.T.);
#29165=ORIENTED_EDGE('',*,*,#20459,.F.);
#29166=ORIENTED_EDGE('',*,*,#20452,.F.);
#29167=ORIENTED_EDGE('',*,*,#20443,.F.);
#29168=ORIENTED_EDGE('',*,*,#20442,.F.);
#29169=ORIENTED_EDGE('',*,*,#20439,.F.);
#29170=ORIENTED_EDGE('',*,*,#20438,.F.);
#29171=ORIENTED_EDGE('',*,*,#20435,.F.);
#29172=ORIENTED_EDGE('',*,*,#20432,.F.);
#29173=ORIENTED_EDGE('',*,*,#20429,.F.);
#29174=ORIENTED_EDGE('',*,*,#20425,.F.);
#29175=ORIENTED_EDGE('',*,*,#20422,.F.);
#29176=ORIENTED_EDGE('',*,*,#20419,.F.);
#29177=ORIENTED_EDGE('',*,*,#20416,.F.);
#29178=ORIENTED_EDGE('',*,*,#20413,.F.);
#29179=ORIENTED_EDGE('',*,*,#20410,.F.);
#29180=ORIENTED_EDGE('',*,*,#20407,.F.);
#29181=ORIENTED_EDGE('',*,*,#20404,.F.);
#29182=ORIENTED_EDGE('',*,*,#20401,.F.);
#29183=ORIENTED_EDGE('',*,*,#20397,.F.);
#29184=ORIENTED_EDGE('',*,*,#20394,.F.);
#29185=ORIENTED_EDGE('',*,*,#20391,.F.);
#29186=ORIENTED_EDGE('',*,*,#20388,.F.);
#29187=ORIENTED_EDGE('',*,*,#20384,.F.);
#29188=ORIENTED_EDGE('',*,*,#20458,.F.);
#29189=ORIENTED_EDGE('',*,*,#20460,.F.);
#29190=ORIENTED_EDGE('',*,*,#20320,.F.);
#29191=ORIENTED_EDGE('',*,*,#20324,.F.);
#29192=ORIENTED_EDGE('',*,*,#20327,.F.);
#29193=ORIENTED_EDGE('',*,*,#20330,.F.);
#29194=ORIENTED_EDGE('',*,*,#20334,.F.);
#29195=ORIENTED_EDGE('',*,*,#20337,.F.);
#29196=ORIENTED_EDGE('',*,*,#20341,.F.);
#29197=ORIENTED_EDGE('',*,*,#20340,.F.);
#29198=ORIENTED_EDGE('',*,*,#20344,.F.);
#29199=ORIENTED_EDGE('',*,*,#20347,.F.);
#29200=ORIENTED_EDGE('',*,*,#20350,.F.);
#29201=ORIENTED_EDGE('',*,*,#20354,.F.);
#29202=ORIENTED_EDGE('',*,*,#20357,.F.);
#29203=ORIENTED_EDGE('',*,*,#20360,.F.);
#29204=ORIENTED_EDGE('',*,*,#20363,.F.);
#29205=ORIENTED_EDGE('',*,*,#20366,.F.);
#29206=ORIENTED_EDGE('',*,*,#20370,.F.);
#29207=ORIENTED_EDGE('',*,*,#20369,.F.);
#29208=ORIENTED_EDGE('',*,*,#20373,.F.);
#29209=ORIENTED_EDGE('',*,*,#20376,.F.);
#29210=ORIENTED_EDGE('',*,*,#20379,.F.);
#29211=ORIENTED_EDGE('',*,*,#20449,.F.);
#29212=ORIENTED_EDGE('',*,*,#20461,.T.);
#29213=ORIENTED_EDGE('',*,*,#20462,.T.);
#29214=ORIENTED_EDGE('',*,*,#20459,.T.);
#29215=ORIENTED_EDGE('',*,*,#20321,.T.);
#29216=ORIENTED_EDGE('',*,*,#20460,.T.);
#29217=ORIENTED_EDGE('',*,*,#20457,.T.);
#29218=ORIENTED_EDGE('',*,*,#20462,.F.);
#29219=ORIENTED_EDGE('',*,*,#20463,.F.);
#29220=ORIENTED_EDGE('',*,*,#20461,.F.);
#29221=ORIENTED_EDGE('',*,*,#20450,.T.);
#29222=ORIENTED_EDGE('',*,*,#20464,.T.);
#29223=ORIENTED_EDGE('',*,*,#20465,.T.);
#29224=ORIENTED_EDGE('',*,*,#20464,.F.);
#29225=ORIENTED_EDGE('',*,*,#20453,.T.);
#29226=ORIENTED_EDGE('',*,*,#20448,.T.);
#29227=ORIENTED_EDGE('',*,*,#20454,.T.);
#29228=ORIENTED_EDGE('',*,*,#20465,.F.);
#29229=ORIENTED_EDGE('',*,*,#20466,.F.);
#29230=ORIENTED_EDGE('',*,*,#20467,.F.);
#29231=ORIENTED_EDGE('',*,*,#20468,.F.);
#29232=ORIENTED_EDGE('',*,*,#20469,.F.);
#29233=ORIENTED_EDGE('',*,*,#20468,.T.);
#29234=ORIENTED_EDGE('',*,*,#20470,.F.);
#29235=ORIENTED_EDGE('',*,*,#20471,.F.);
#29236=ORIENTED_EDGE('',*,*,#20472,.F.);
#29237=ORIENTED_EDGE('',*,*,#20473,.F.);
#29238=ORIENTED_EDGE('',*,*,#20470,.T.);
#29239=ORIENTED_EDGE('',*,*,#20467,.T.);
#29240=ORIENTED_EDGE('',*,*,#20474,.T.);
#29241=ORIENTED_EDGE('',*,*,#20475,.T.);
#29242=ORIENTED_EDGE('',*,*,#20476,.F.);
#29243=ORIENTED_EDGE('',*,*,#20477,.F.);
#29244=ORIENTED_EDGE('',*,*,#20475,.F.);
#29245=ORIENTED_EDGE('',*,*,#20478,.T.);
#29246=ORIENTED_EDGE('',*,*,#20479,.T.);
#29247=ORIENTED_EDGE('',*,*,#20480,.F.);
#29248=ORIENTED_EDGE('',*,*,#20481,.T.);
#29249=ORIENTED_EDGE('',*,*,#20482,.T.);
#29250=ORIENTED_EDGE('',*,*,#20483,.T.);
#29251=ORIENTED_EDGE('',*,*,#20484,.F.);
#29252=ORIENTED_EDGE('',*,*,#20485,.T.);
#29253=ORIENTED_EDGE('',*,*,#20486,.T.);
#29254=ORIENTED_EDGE('',*,*,#20487,.T.);
#29255=ORIENTED_EDGE('',*,*,#20488,.F.);
#29256=ORIENTED_EDGE('',*,*,#20489,.T.);
#29257=ORIENTED_EDGE('',*,*,#20490,.T.);
#29258=ORIENTED_EDGE('',*,*,#20491,.T.);
#29259=ORIENTED_EDGE('',*,*,#20492,.F.);
#29260=ORIENTED_EDGE('',*,*,#20493,.T.);
#29261=ORIENTED_EDGE('',*,*,#20494,.T.);
#29262=ORIENTED_EDGE('',*,*,#20495,.T.);
#29263=ORIENTED_EDGE('',*,*,#20496,.F.);
#29264=ORIENTED_EDGE('',*,*,#20497,.T.);
#29265=ORIENTED_EDGE('',*,*,#20498,.T.);
#29266=ORIENTED_EDGE('',*,*,#20499,.T.);
#29267=ORIENTED_EDGE('',*,*,#20500,.F.);
#29268=ORIENTED_EDGE('',*,*,#20501,.T.);
#29269=ORIENTED_EDGE('',*,*,#20502,.T.);
#29270=ORIENTED_EDGE('',*,*,#20503,.T.);
#29271=ORIENTED_EDGE('',*,*,#20504,.F.);
#29272=ORIENTED_EDGE('',*,*,#20505,.T.);
#29273=ORIENTED_EDGE('',*,*,#20506,.T.);
#29274=ORIENTED_EDGE('',*,*,#20507,.T.);
#29275=ORIENTED_EDGE('',*,*,#20508,.F.);
#29276=ORIENTED_EDGE('',*,*,#20509,.T.);
#29277=ORIENTED_EDGE('',*,*,#20510,.T.);
#29278=ORIENTED_EDGE('',*,*,#20511,.T.);
#29279=ORIENTED_EDGE('',*,*,#20512,.F.);
#29280=ORIENTED_EDGE('',*,*,#20513,.T.);
#29281=ORIENTED_EDGE('',*,*,#20514,.T.);
#29282=ORIENTED_EDGE('',*,*,#20515,.T.);
#29283=ORIENTED_EDGE('',*,*,#20516,.F.);
#29284=ORIENTED_EDGE('',*,*,#20517,.T.);
#29285=ORIENTED_EDGE('',*,*,#20518,.T.);
#29286=ORIENTED_EDGE('',*,*,#20519,.T.);
#29287=ORIENTED_EDGE('',*,*,#20520,.F.);
#29288=ORIENTED_EDGE('',*,*,#20521,.T.);
#29289=ORIENTED_EDGE('',*,*,#20522,.T.);
#29290=ORIENTED_EDGE('',*,*,#20523,.T.);
#29291=ORIENTED_EDGE('',*,*,#20524,.F.);
#29292=ORIENTED_EDGE('',*,*,#20525,.T.);
#29293=ORIENTED_EDGE('',*,*,#20526,.T.);
#29294=ORIENTED_EDGE('',*,*,#20527,.T.);
#29295=ORIENTED_EDGE('',*,*,#20528,.F.);
#29296=ORIENTED_EDGE('',*,*,#20529,.T.);
#29297=ORIENTED_EDGE('',*,*,#20530,.T.);
#29298=ORIENTED_EDGE('',*,*,#20531,.T.);
#29299=ORIENTED_EDGE('',*,*,#20532,.F.);
#29300=ORIENTED_EDGE('',*,*,#20533,.T.);
#29301=ORIENTED_EDGE('',*,*,#20534,.T.);
#29302=ORIENTED_EDGE('',*,*,#20535,.T.);
#29303=ORIENTED_EDGE('',*,*,#20536,.F.);
#29304=ORIENTED_EDGE('',*,*,#20537,.T.);
#29305=ORIENTED_EDGE('',*,*,#20538,.T.);
#29306=ORIENTED_EDGE('',*,*,#20539,.T.);
#29307=ORIENTED_EDGE('',*,*,#20540,.F.);
#29308=ORIENTED_EDGE('',*,*,#20541,.T.);
#29309=ORIENTED_EDGE('',*,*,#20542,.T.);
#29310=ORIENTED_EDGE('',*,*,#20543,.T.);
#29311=ORIENTED_EDGE('',*,*,#20544,.F.);
#29312=ORIENTED_EDGE('',*,*,#20472,.T.);
#29313=ORIENTED_EDGE('',*,*,#20466,.T.);
#29314=ORIENTED_EDGE('',*,*,#20469,.T.);
#29315=ORIENTED_EDGE('',*,*,#20545,.F.);
#29316=ORIENTED_EDGE('',*,*,#20546,.T.);
#29317=ORIENTED_EDGE('',*,*,#20547,.T.);
#29318=ORIENTED_EDGE('',*,*,#20548,.T.);
#29319=ORIENTED_EDGE('',*,*,#20549,.F.);
#29320=ORIENTED_EDGE('',*,*,#20550,.T.);
#29321=ORIENTED_EDGE('',*,*,#20551,.T.);
#29322=ORIENTED_EDGE('',*,*,#20552,.T.);
#29323=ORIENTED_EDGE('',*,*,#20553,.F.);
#29324=ORIENTED_EDGE('',*,*,#20554,.T.);
#29325=ORIENTED_EDGE('',*,*,#20555,.T.);
#29326=ORIENTED_EDGE('',*,*,#20556,.T.);
#29327=ORIENTED_EDGE('',*,*,#20557,.F.);
#29328=ORIENTED_EDGE('',*,*,#20558,.T.);
#29329=ORIENTED_EDGE('',*,*,#20559,.T.);
#29330=ORIENTED_EDGE('',*,*,#20560,.T.);
#29331=ORIENTED_EDGE('',*,*,#20561,.F.);
#29332=ORIENTED_EDGE('',*,*,#20562,.T.);
#29333=ORIENTED_EDGE('',*,*,#20563,.T.);
#29334=ORIENTED_EDGE('',*,*,#20564,.T.);
#29335=ORIENTED_EDGE('',*,*,#20565,.F.);
#29336=ORIENTED_EDGE('',*,*,#20566,.T.);
#29337=ORIENTED_EDGE('',*,*,#20567,.T.);
#29338=ORIENTED_EDGE('',*,*,#20568,.T.);
#29339=ORIENTED_EDGE('',*,*,#20569,.F.);
#29340=ORIENTED_EDGE('',*,*,#20570,.T.);
#29341=ORIENTED_EDGE('',*,*,#20571,.T.);
#29342=ORIENTED_EDGE('',*,*,#20572,.T.);
#29343=ORIENTED_EDGE('',*,*,#20573,.F.);
#29344=ORIENTED_EDGE('',*,*,#20574,.T.);
#29345=ORIENTED_EDGE('',*,*,#20575,.T.);
#29346=ORIENTED_EDGE('',*,*,#20576,.T.);
#29347=ORIENTED_EDGE('',*,*,#20577,.F.);
#29348=ORIENTED_EDGE('',*,*,#20578,.T.);
#29349=ORIENTED_EDGE('',*,*,#20579,.T.);
#29350=ORIENTED_EDGE('',*,*,#20580,.T.);
#29351=ORIENTED_EDGE('',*,*,#20581,.F.);
#29352=ORIENTED_EDGE('',*,*,#20582,.T.);
#29353=ORIENTED_EDGE('',*,*,#20583,.T.);
#29354=ORIENTED_EDGE('',*,*,#20584,.T.);
#29355=ORIENTED_EDGE('',*,*,#20585,.F.);
#29356=ORIENTED_EDGE('',*,*,#20586,.T.);
#29357=ORIENTED_EDGE('',*,*,#20587,.T.);
#29358=ORIENTED_EDGE('',*,*,#20588,.T.);
#29359=ORIENTED_EDGE('',*,*,#20589,.F.);
#29360=ORIENTED_EDGE('',*,*,#20590,.T.);
#29361=ORIENTED_EDGE('',*,*,#20591,.T.);
#29362=ORIENTED_EDGE('',*,*,#20592,.T.);
#29363=ORIENTED_EDGE('',*,*,#20593,.F.);
#29364=ORIENTED_EDGE('',*,*,#20594,.T.);
#29365=ORIENTED_EDGE('',*,*,#20595,.T.);
#29366=ORIENTED_EDGE('',*,*,#20596,.T.);
#29367=ORIENTED_EDGE('',*,*,#20597,.F.);
#29368=ORIENTED_EDGE('',*,*,#20598,.T.);
#29369=ORIENTED_EDGE('',*,*,#20599,.T.);
#29370=ORIENTED_EDGE('',*,*,#20600,.T.);
#29371=ORIENTED_EDGE('',*,*,#20601,.F.);
#29372=ORIENTED_EDGE('',*,*,#20602,.T.);
#29373=ORIENTED_EDGE('',*,*,#20603,.T.);
#29374=ORIENTED_EDGE('',*,*,#20604,.T.);
#29375=ORIENTED_EDGE('',*,*,#20605,.F.);
#29376=ORIENTED_EDGE('',*,*,#20606,.T.);
#29377=ORIENTED_EDGE('',*,*,#20607,.T.);
#29378=ORIENTED_EDGE('',*,*,#20608,.T.);
#29379=ORIENTED_EDGE('',*,*,#20609,.F.);
#29380=ORIENTED_EDGE('',*,*,#20610,.T.);
#29381=ORIENTED_EDGE('',*,*,#20611,.T.);
#29382=ORIENTED_EDGE('',*,*,#20612,.T.);
#29383=ORIENTED_EDGE('',*,*,#20613,.F.);
#29384=ORIENTED_EDGE('',*,*,#20614,.T.);
#29385=ORIENTED_EDGE('',*,*,#20615,.T.);
#29386=ORIENTED_EDGE('',*,*,#20616,.T.);
#29387=ORIENTED_EDGE('',*,*,#20617,.F.);
#29388=ORIENTED_EDGE('',*,*,#20618,.T.);
#29389=ORIENTED_EDGE('',*,*,#20543,.F.);
#29390=ORIENTED_EDGE('',*,*,#20619,.T.);
#29391=ORIENTED_EDGE('',*,*,#20620,.F.);
#29392=ORIENTED_EDGE('',*,*,#20621,.F.);
#29393=ORIENTED_EDGE('',*,*,#20622,.F.);
#29394=ORIENTED_EDGE('',*,*,#20620,.T.);
#29395=ORIENTED_EDGE('',*,*,#20623,.T.);
#29396=ORIENTED_EDGE('',*,*,#20541,.F.);
#29397=ORIENTED_EDGE('',*,*,#20542,.F.);
#29398=ORIENTED_EDGE('',*,*,#20623,.F.);
#29399=ORIENTED_EDGE('',*,*,#20619,.F.);
#29400=ORIENTED_EDGE('',*,*,#20624,.T.);
#29401=ORIENTED_EDGE('',*,*,#20617,.T.);
#29402=ORIENTED_EDGE('',*,*,#20625,.T.);
#29403=ORIENTED_EDGE('',*,*,#20626,.T.);
#29404=ORIENTED_EDGE('',*,*,#20613,.T.);
#29405=ORIENTED_EDGE('',*,*,#20627,.T.);
#29406=ORIENTED_EDGE('',*,*,#20628,.T.);
#29407=ORIENTED_EDGE('',*,*,#20609,.T.);
#29408=ORIENTED_EDGE('',*,*,#20629,.T.);
#29409=ORIENTED_EDGE('',*,*,#20630,.T.);
#29410=ORIENTED_EDGE('',*,*,#20605,.T.);
#29411=ORIENTED_EDGE('',*,*,#20631,.T.);
#29412=ORIENTED_EDGE('',*,*,#20632,.T.);
#29413=ORIENTED_EDGE('',*,*,#20601,.T.);
#29414=ORIENTED_EDGE('',*,*,#20633,.T.);
#29415=ORIENTED_EDGE('',*,*,#20634,.T.);
#29416=ORIENTED_EDGE('',*,*,#20597,.T.);
#29417=ORIENTED_EDGE('',*,*,#20635,.T.);
#29418=ORIENTED_EDGE('',*,*,#20636,.T.);
#29419=ORIENTED_EDGE('',*,*,#20593,.T.);
#29420=ORIENTED_EDGE('',*,*,#20637,.T.);
#29421=ORIENTED_EDGE('',*,*,#20638,.T.);
#29422=ORIENTED_EDGE('',*,*,#20589,.T.);
#29423=ORIENTED_EDGE('',*,*,#20639,.T.);
#29424=ORIENTED_EDGE('',*,*,#20640,.T.);
#29425=ORIENTED_EDGE('',*,*,#20585,.T.);
#29426=ORIENTED_EDGE('',*,*,#20641,.T.);
#29427=ORIENTED_EDGE('',*,*,#20642,.T.);
#29428=ORIENTED_EDGE('',*,*,#20581,.T.);
#29429=ORIENTED_EDGE('',*,*,#20643,.T.);
#29430=ORIENTED_EDGE('',*,*,#20644,.T.);
#29431=ORIENTED_EDGE('',*,*,#20577,.T.);
#29432=ORIENTED_EDGE('',*,*,#20645,.T.);
#29433=ORIENTED_EDGE('',*,*,#20646,.T.);
#29434=ORIENTED_EDGE('',*,*,#20573,.T.);
#29435=ORIENTED_EDGE('',*,*,#20647,.T.);
#29436=ORIENTED_EDGE('',*,*,#20648,.T.);
#29437=ORIENTED_EDGE('',*,*,#20569,.T.);
#29438=ORIENTED_EDGE('',*,*,#20649,.T.);
#29439=ORIENTED_EDGE('',*,*,#20650,.T.);
#29440=ORIENTED_EDGE('',*,*,#20565,.T.);
#29441=ORIENTED_EDGE('',*,*,#20651,.T.);
#29442=ORIENTED_EDGE('',*,*,#20652,.T.);
#29443=ORIENTED_EDGE('',*,*,#20561,.T.);
#29444=ORIENTED_EDGE('',*,*,#20653,.T.);
#29445=ORIENTED_EDGE('',*,*,#20654,.T.);
#29446=ORIENTED_EDGE('',*,*,#20557,.T.);
#29447=ORIENTED_EDGE('',*,*,#20655,.T.);
#29448=ORIENTED_EDGE('',*,*,#20656,.T.);
#29449=ORIENTED_EDGE('',*,*,#20553,.T.);
#29450=ORIENTED_EDGE('',*,*,#20657,.T.);
#29451=ORIENTED_EDGE('',*,*,#20658,.T.);
#29452=ORIENTED_EDGE('',*,*,#20549,.T.);
#29453=ORIENTED_EDGE('',*,*,#20659,.T.);
#29454=ORIENTED_EDGE('',*,*,#20660,.T.);
#29455=ORIENTED_EDGE('',*,*,#20545,.T.);
#29456=ORIENTED_EDGE('',*,*,#20471,.T.);
#29457=ORIENTED_EDGE('',*,*,#20473,.T.);
#29458=ORIENTED_EDGE('',*,*,#20544,.T.);
#29459=ORIENTED_EDGE('',*,*,#20621,.T.);
#29460=ORIENTED_EDGE('',*,*,#20622,.T.);
#29461=ORIENTED_EDGE('',*,*,#20540,.T.);
#29462=ORIENTED_EDGE('',*,*,#20661,.T.);
#29463=ORIENTED_EDGE('',*,*,#20662,.T.);
#29464=ORIENTED_EDGE('',*,*,#20536,.T.);
#29465=ORIENTED_EDGE('',*,*,#20663,.T.);
#29466=ORIENTED_EDGE('',*,*,#20664,.T.);
#29467=ORIENTED_EDGE('',*,*,#20532,.T.);
#29468=ORIENTED_EDGE('',*,*,#20665,.T.);
#29469=ORIENTED_EDGE('',*,*,#20666,.T.);
#29470=ORIENTED_EDGE('',*,*,#20528,.T.);
#29471=ORIENTED_EDGE('',*,*,#20667,.T.);
#29472=ORIENTED_EDGE('',*,*,#20668,.T.);
#29473=ORIENTED_EDGE('',*,*,#20524,.T.);
#29474=ORIENTED_EDGE('',*,*,#20669,.T.);
#29475=ORIENTED_EDGE('',*,*,#20670,.T.);
#29476=ORIENTED_EDGE('',*,*,#20520,.T.);
#29477=ORIENTED_EDGE('',*,*,#20671,.T.);
#29478=ORIENTED_EDGE('',*,*,#20672,.T.);
#29479=ORIENTED_EDGE('',*,*,#20516,.T.);
#29480=ORIENTED_EDGE('',*,*,#20673,.T.);
#29481=ORIENTED_EDGE('',*,*,#20674,.T.);
#29482=ORIENTED_EDGE('',*,*,#20512,.T.);
#29483=ORIENTED_EDGE('',*,*,#20675,.T.);
#29484=ORIENTED_EDGE('',*,*,#20676,.T.);
#29485=ORIENTED_EDGE('',*,*,#20508,.T.);
#29486=ORIENTED_EDGE('',*,*,#20677,.T.);
#29487=ORIENTED_EDGE('',*,*,#20678,.T.);
#29488=ORIENTED_EDGE('',*,*,#20504,.T.);
#29489=ORIENTED_EDGE('',*,*,#20679,.T.);
#29490=ORIENTED_EDGE('',*,*,#20680,.T.);
#29491=ORIENTED_EDGE('',*,*,#20500,.T.);
#29492=ORIENTED_EDGE('',*,*,#20681,.T.);
#29493=ORIENTED_EDGE('',*,*,#20682,.T.);
#29494=ORIENTED_EDGE('',*,*,#20496,.T.);
#29495=ORIENTED_EDGE('',*,*,#20683,.T.);
#29496=ORIENTED_EDGE('',*,*,#20684,.T.);
#29497=ORIENTED_EDGE('',*,*,#20492,.T.);
#29498=ORIENTED_EDGE('',*,*,#20685,.T.);
#29499=ORIENTED_EDGE('',*,*,#20686,.T.);
#29500=ORIENTED_EDGE('',*,*,#20488,.T.);
#29501=ORIENTED_EDGE('',*,*,#20687,.T.);
#29502=ORIENTED_EDGE('',*,*,#20688,.T.);
#29503=ORIENTED_EDGE('',*,*,#20484,.T.);
#29504=ORIENTED_EDGE('',*,*,#20689,.T.);
#29505=ORIENTED_EDGE('',*,*,#20690,.T.);
#29506=ORIENTED_EDGE('',*,*,#20480,.T.);
#29507=ORIENTED_EDGE('',*,*,#20691,.T.);
#29508=ORIENTED_EDGE('',*,*,#20692,.T.);
#29509=ORIENTED_EDGE('',*,*,#20693,.T.);
#29510=ORIENTED_EDGE('',*,*,#20692,.F.);
#29511=ORIENTED_EDGE('',*,*,#20538,.F.);
#29512=ORIENTED_EDGE('',*,*,#20694,.F.);
#29513=ORIENTED_EDGE('',*,*,#20695,.F.);
#29514=ORIENTED_EDGE('',*,*,#20539,.F.);
#29515=ORIENTED_EDGE('',*,*,#20695,.T.);
#29516=ORIENTED_EDGE('',*,*,#20696,.F.);
#29517=ORIENTED_EDGE('',*,*,#20661,.F.);
#29518=ORIENTED_EDGE('',*,*,#20537,.F.);
#29519=ORIENTED_EDGE('',*,*,#20662,.F.);
#29520=ORIENTED_EDGE('',*,*,#20696,.T.);
#29521=ORIENTED_EDGE('',*,*,#20694,.T.);
#29522=ORIENTED_EDGE('',*,*,#20535,.F.);
#29523=ORIENTED_EDGE('',*,*,#20697,.T.);
#29524=ORIENTED_EDGE('',*,*,#20698,.F.);
#29525=ORIENTED_EDGE('',*,*,#20663,.F.);
#29526=ORIENTED_EDGE('',*,*,#20664,.F.);
#29527=ORIENTED_EDGE('',*,*,#20698,.T.);
#29528=ORIENTED_EDGE('',*,*,#20699,.T.);
#29529=ORIENTED_EDGE('',*,*,#20533,.F.);
#29530=ORIENTED_EDGE('',*,*,#20534,.F.);
#29531=ORIENTED_EDGE('',*,*,#20699,.F.);
#29532=ORIENTED_EDGE('',*,*,#20697,.F.);
#29533=ORIENTED_EDGE('',*,*,#20530,.F.);
#29534=ORIENTED_EDGE('',*,*,#20700,.F.);
#29535=ORIENTED_EDGE('',*,*,#20701,.F.);
#29536=ORIENTED_EDGE('',*,*,#20531,.F.);
#29537=ORIENTED_EDGE('',*,*,#20701,.T.);
#29538=ORIENTED_EDGE('',*,*,#20702,.F.);
#29539=ORIENTED_EDGE('',*,*,#20665,.F.);
#29540=ORIENTED_EDGE('',*,*,#20529,.F.);
#29541=ORIENTED_EDGE('',*,*,#20666,.F.);
#29542=ORIENTED_EDGE('',*,*,#20702,.T.);
#29543=ORIENTED_EDGE('',*,*,#20700,.T.);
#29544=ORIENTED_EDGE('',*,*,#20527,.F.);
#29545=ORIENTED_EDGE('',*,*,#20703,.T.);
#29546=ORIENTED_EDGE('',*,*,#20704,.F.);
#29547=ORIENTED_EDGE('',*,*,#20667,.F.);
#29548=ORIENTED_EDGE('',*,*,#20668,.F.);
#29549=ORIENTED_EDGE('',*,*,#20704,.T.);
#29550=ORIENTED_EDGE('',*,*,#20705,.T.);
#29551=ORIENTED_EDGE('',*,*,#20525,.F.);
#29552=ORIENTED_EDGE('',*,*,#20526,.F.);
#29553=ORIENTED_EDGE('',*,*,#20705,.F.);
#29554=ORIENTED_EDGE('',*,*,#20703,.F.);
#29555=ORIENTED_EDGE('',*,*,#20522,.F.);
#29556=ORIENTED_EDGE('',*,*,#20706,.F.);
#29557=ORIENTED_EDGE('',*,*,#20707,.F.);
#29558=ORIENTED_EDGE('',*,*,#20523,.F.);
#29559=ORIENTED_EDGE('',*,*,#20707,.T.);
#29560=ORIENTED_EDGE('',*,*,#20708,.F.);
#29561=ORIENTED_EDGE('',*,*,#20669,.F.);
#29562=ORIENTED_EDGE('',*,*,#20521,.F.);
#29563=ORIENTED_EDGE('',*,*,#20670,.F.);
#29564=ORIENTED_EDGE('',*,*,#20708,.T.);
#29565=ORIENTED_EDGE('',*,*,#20706,.T.);
#29566=ORIENTED_EDGE('',*,*,#20519,.F.);
#29567=ORIENTED_EDGE('',*,*,#20709,.T.);
#29568=ORIENTED_EDGE('',*,*,#20710,.F.);
#29569=ORIENTED_EDGE('',*,*,#20671,.F.);
#29570=ORIENTED_EDGE('',*,*,#20672,.F.);
#29571=ORIENTED_EDGE('',*,*,#20710,.T.);
#29572=ORIENTED_EDGE('',*,*,#20711,.T.);
#29573=ORIENTED_EDGE('',*,*,#20517,.F.);
#29574=ORIENTED_EDGE('',*,*,#20518,.F.);
#29575=ORIENTED_EDGE('',*,*,#20711,.F.);
#29576=ORIENTED_EDGE('',*,*,#20709,.F.);
#29577=ORIENTED_EDGE('',*,*,#20514,.F.);
#29578=ORIENTED_EDGE('',*,*,#20712,.F.);
#29579=ORIENTED_EDGE('',*,*,#20713,.F.);
#29580=ORIENTED_EDGE('',*,*,#20515,.F.);
#29581=ORIENTED_EDGE('',*,*,#20713,.T.);
#29582=ORIENTED_EDGE('',*,*,#20714,.F.);
#29583=ORIENTED_EDGE('',*,*,#20673,.F.);
#29584=ORIENTED_EDGE('',*,*,#20513,.F.);
#29585=ORIENTED_EDGE('',*,*,#20674,.F.);
#29586=ORIENTED_EDGE('',*,*,#20714,.T.);
#29587=ORIENTED_EDGE('',*,*,#20712,.T.);
#29588=ORIENTED_EDGE('',*,*,#20511,.F.);
#29589=ORIENTED_EDGE('',*,*,#20715,.T.);
#29590=ORIENTED_EDGE('',*,*,#20716,.F.);
#29591=ORIENTED_EDGE('',*,*,#20675,.F.);
#29592=ORIENTED_EDGE('',*,*,#20676,.F.);
#29593=ORIENTED_EDGE('',*,*,#20716,.T.);
#29594=ORIENTED_EDGE('',*,*,#20717,.T.);
#29595=ORIENTED_EDGE('',*,*,#20509,.F.);
#29596=ORIENTED_EDGE('',*,*,#20510,.F.);
#29597=ORIENTED_EDGE('',*,*,#20717,.F.);
#29598=ORIENTED_EDGE('',*,*,#20715,.F.);
#29599=ORIENTED_EDGE('',*,*,#20506,.F.);
#29600=ORIENTED_EDGE('',*,*,#20718,.F.);
#29601=ORIENTED_EDGE('',*,*,#20719,.F.);
#29602=ORIENTED_EDGE('',*,*,#20507,.F.);
#29603=ORIENTED_EDGE('',*,*,#20719,.T.);
#29604=ORIENTED_EDGE('',*,*,#20720,.F.);
#29605=ORIENTED_EDGE('',*,*,#20677,.F.);
#29606=ORIENTED_EDGE('',*,*,#20505,.F.);
#29607=ORIENTED_EDGE('',*,*,#20678,.F.);
#29608=ORIENTED_EDGE('',*,*,#20720,.T.);
#29609=ORIENTED_EDGE('',*,*,#20718,.T.);
#29610=ORIENTED_EDGE('',*,*,#20503,.F.);
#29611=ORIENTED_EDGE('',*,*,#20721,.T.);
#29612=ORIENTED_EDGE('',*,*,#20722,.F.);
#29613=ORIENTED_EDGE('',*,*,#20679,.F.);
#29614=ORIENTED_EDGE('',*,*,#20680,.F.);
#29615=ORIENTED_EDGE('',*,*,#20722,.T.);
#29616=ORIENTED_EDGE('',*,*,#20723,.T.);
#29617=ORIENTED_EDGE('',*,*,#20501,.F.);
#29618=ORIENTED_EDGE('',*,*,#20502,.F.);
#29619=ORIENTED_EDGE('',*,*,#20723,.F.);
#29620=ORIENTED_EDGE('',*,*,#20721,.F.);
#29621=ORIENTED_EDGE('',*,*,#20498,.F.);
#29622=ORIENTED_EDGE('',*,*,#20724,.F.);
#29623=ORIENTED_EDGE('',*,*,#20725,.F.);
#29624=ORIENTED_EDGE('',*,*,#20499,.F.);
#29625=ORIENTED_EDGE('',*,*,#20725,.T.);
#29626=ORIENTED_EDGE('',*,*,#20726,.F.);
#29627=ORIENTED_EDGE('',*,*,#20681,.F.);
#29628=ORIENTED_EDGE('',*,*,#20497,.F.);
#29629=ORIENTED_EDGE('',*,*,#20682,.F.);
#29630=ORIENTED_EDGE('',*,*,#20726,.T.);
#29631=ORIENTED_EDGE('',*,*,#20724,.T.);
#29632=ORIENTED_EDGE('',*,*,#20495,.F.);
#29633=ORIENTED_EDGE('',*,*,#20727,.T.);
#29634=ORIENTED_EDGE('',*,*,#20728,.F.);
#29635=ORIENTED_EDGE('',*,*,#20683,.F.);
#29636=ORIENTED_EDGE('',*,*,#20684,.F.);
#29637=ORIENTED_EDGE('',*,*,#20728,.T.);
#29638=ORIENTED_EDGE('',*,*,#20729,.T.);
#29639=ORIENTED_EDGE('',*,*,#20493,.F.);
#29640=ORIENTED_EDGE('',*,*,#20494,.F.);
#29641=ORIENTED_EDGE('',*,*,#20729,.F.);
#29642=ORIENTED_EDGE('',*,*,#20727,.F.);
#29643=ORIENTED_EDGE('',*,*,#20490,.F.);
#29644=ORIENTED_EDGE('',*,*,#20730,.F.);
#29645=ORIENTED_EDGE('',*,*,#20731,.F.);
#29646=ORIENTED_EDGE('',*,*,#20491,.F.);
#29647=ORIENTED_EDGE('',*,*,#20731,.T.);
#29648=ORIENTED_EDGE('',*,*,#20732,.F.);
#29649=ORIENTED_EDGE('',*,*,#20685,.F.);
#29650=ORIENTED_EDGE('',*,*,#20489,.F.);
#29651=ORIENTED_EDGE('',*,*,#20686,.F.);
#29652=ORIENTED_EDGE('',*,*,#20732,.T.);
#29653=ORIENTED_EDGE('',*,*,#20730,.T.);
#29654=ORIENTED_EDGE('',*,*,#20487,.F.);
#29655=ORIENTED_EDGE('',*,*,#20733,.T.);
#29656=ORIENTED_EDGE('',*,*,#20734,.F.);
#29657=ORIENTED_EDGE('',*,*,#20687,.F.);
#29658=ORIENTED_EDGE('',*,*,#20688,.F.);
#29659=ORIENTED_EDGE('',*,*,#20734,.T.);
#29660=ORIENTED_EDGE('',*,*,#20735,.T.);
#29661=ORIENTED_EDGE('',*,*,#20485,.F.);
#29662=ORIENTED_EDGE('',*,*,#20486,.F.);
#29663=ORIENTED_EDGE('',*,*,#20735,.F.);
#29664=ORIENTED_EDGE('',*,*,#20733,.F.);
#29665=ORIENTED_EDGE('',*,*,#20482,.F.);
#29666=ORIENTED_EDGE('',*,*,#20736,.F.);
#29667=ORIENTED_EDGE('',*,*,#20737,.F.);
#29668=ORIENTED_EDGE('',*,*,#20483,.F.);
#29669=ORIENTED_EDGE('',*,*,#20737,.T.);
#29670=ORIENTED_EDGE('',*,*,#20738,.F.);
#29671=ORIENTED_EDGE('',*,*,#20689,.F.);
#29672=ORIENTED_EDGE('',*,*,#20481,.F.);
#29673=ORIENTED_EDGE('',*,*,#20690,.F.);
#29674=ORIENTED_EDGE('',*,*,#20738,.T.);
#29675=ORIENTED_EDGE('',*,*,#20736,.T.);
#29676=ORIENTED_EDGE('',*,*,#20479,.F.);
#29677=ORIENTED_EDGE('',*,*,#20739,.T.);
#29678=ORIENTED_EDGE('',*,*,#20740,.F.);
#29679=ORIENTED_EDGE('',*,*,#20691,.F.);
#29680=ORIENTED_EDGE('',*,*,#20624,.F.);
#29681=ORIENTED_EDGE('',*,*,#20740,.T.);
#29682=ORIENTED_EDGE('',*,*,#20741,.T.);
#29683=ORIENTED_EDGE('',*,*,#20618,.F.);
#29684=ORIENTED_EDGE('',*,*,#20474,.F.);
#29685=ORIENTED_EDGE('',*,*,#20741,.F.);
#29686=ORIENTED_EDGE('',*,*,#20739,.F.);
#29687=ORIENTED_EDGE('',*,*,#20478,.F.);
#29688=ORIENTED_EDGE('',*,*,#20615,.F.);
#29689=ORIENTED_EDGE('',*,*,#20742,.F.);
#29690=ORIENTED_EDGE('',*,*,#20743,.F.);
#29691=ORIENTED_EDGE('',*,*,#20616,.F.);
#29692=ORIENTED_EDGE('',*,*,#20743,.T.);
#29693=ORIENTED_EDGE('',*,*,#20744,.F.);
#29694=ORIENTED_EDGE('',*,*,#20625,.F.);
#29695=ORIENTED_EDGE('',*,*,#20614,.F.);
#29696=ORIENTED_EDGE('',*,*,#20626,.F.);
#29697=ORIENTED_EDGE('',*,*,#20744,.T.);
#29698=ORIENTED_EDGE('',*,*,#20742,.T.);
#29699=ORIENTED_EDGE('',*,*,#20612,.F.);
#29700=ORIENTED_EDGE('',*,*,#20745,.T.);
#29701=ORIENTED_EDGE('',*,*,#20746,.F.);
#29702=ORIENTED_EDGE('',*,*,#20627,.F.);
#29703=ORIENTED_EDGE('',*,*,#20628,.F.);
#29704=ORIENTED_EDGE('',*,*,#20746,.T.);
#29705=ORIENTED_EDGE('',*,*,#20747,.T.);
#29706=ORIENTED_EDGE('',*,*,#20610,.F.);
#29707=ORIENTED_EDGE('',*,*,#20611,.F.);
#29708=ORIENTED_EDGE('',*,*,#20747,.F.);
#29709=ORIENTED_EDGE('',*,*,#20745,.F.);
#29710=ORIENTED_EDGE('',*,*,#20607,.F.);
#29711=ORIENTED_EDGE('',*,*,#20748,.F.);
#29712=ORIENTED_EDGE('',*,*,#20749,.F.);
#29713=ORIENTED_EDGE('',*,*,#20608,.F.);
#29714=ORIENTED_EDGE('',*,*,#20749,.T.);
#29715=ORIENTED_EDGE('',*,*,#20750,.F.);
#29716=ORIENTED_EDGE('',*,*,#20629,.F.);
#29717=ORIENTED_EDGE('',*,*,#20606,.F.);
#29718=ORIENTED_EDGE('',*,*,#20630,.F.);
#29719=ORIENTED_EDGE('',*,*,#20750,.T.);
#29720=ORIENTED_EDGE('',*,*,#20748,.T.);
#29721=ORIENTED_EDGE('',*,*,#20604,.F.);
#29722=ORIENTED_EDGE('',*,*,#20751,.T.);
#29723=ORIENTED_EDGE('',*,*,#20752,.F.);
#29724=ORIENTED_EDGE('',*,*,#20631,.F.);
#29725=ORIENTED_EDGE('',*,*,#20632,.F.);
#29726=ORIENTED_EDGE('',*,*,#20752,.T.);
#29727=ORIENTED_EDGE('',*,*,#20753,.T.);
#29728=ORIENTED_EDGE('',*,*,#20602,.F.);
#29729=ORIENTED_EDGE('',*,*,#20603,.F.);
#29730=ORIENTED_EDGE('',*,*,#20753,.F.);
#29731=ORIENTED_EDGE('',*,*,#20751,.F.);
#29732=ORIENTED_EDGE('',*,*,#20599,.F.);
#29733=ORIENTED_EDGE('',*,*,#20754,.F.);
#29734=ORIENTED_EDGE('',*,*,#20755,.F.);
#29735=ORIENTED_EDGE('',*,*,#20600,.F.);
#29736=ORIENTED_EDGE('',*,*,#20755,.T.);
#29737=ORIENTED_EDGE('',*,*,#20756,.F.);
#29738=ORIENTED_EDGE('',*,*,#20633,.F.);
#29739=ORIENTED_EDGE('',*,*,#20598,.F.);
#29740=ORIENTED_EDGE('',*,*,#20634,.F.);
#29741=ORIENTED_EDGE('',*,*,#20756,.T.);
#29742=ORIENTED_EDGE('',*,*,#20754,.T.);
#29743=ORIENTED_EDGE('',*,*,#20596,.F.);
#29744=ORIENTED_EDGE('',*,*,#20757,.T.);
#29745=ORIENTED_EDGE('',*,*,#20758,.F.);
#29746=ORIENTED_EDGE('',*,*,#20635,.F.);
#29747=ORIENTED_EDGE('',*,*,#20636,.F.);
#29748=ORIENTED_EDGE('',*,*,#20758,.T.);
#29749=ORIENTED_EDGE('',*,*,#20759,.T.);
#29750=ORIENTED_EDGE('',*,*,#20594,.F.);
#29751=ORIENTED_EDGE('',*,*,#20595,.F.);
#29752=ORIENTED_EDGE('',*,*,#20759,.F.);
#29753=ORIENTED_EDGE('',*,*,#20757,.F.);
#29754=ORIENTED_EDGE('',*,*,#20591,.F.);
#29755=ORIENTED_EDGE('',*,*,#20760,.F.);
#29756=ORIENTED_EDGE('',*,*,#20761,.F.);
#29757=ORIENTED_EDGE('',*,*,#20592,.F.);
#29758=ORIENTED_EDGE('',*,*,#20761,.T.);
#29759=ORIENTED_EDGE('',*,*,#20762,.F.);
#29760=ORIENTED_EDGE('',*,*,#20637,.F.);
#29761=ORIENTED_EDGE('',*,*,#20590,.F.);
#29762=ORIENTED_EDGE('',*,*,#20638,.F.);
#29763=ORIENTED_EDGE('',*,*,#20762,.T.);
#29764=ORIENTED_EDGE('',*,*,#20760,.T.);
#29765=ORIENTED_EDGE('',*,*,#20588,.F.);
#29766=ORIENTED_EDGE('',*,*,#20763,.T.);
#29767=ORIENTED_EDGE('',*,*,#20764,.F.);
#29768=ORIENTED_EDGE('',*,*,#20639,.F.);
#29769=ORIENTED_EDGE('',*,*,#20640,.F.);
#29770=ORIENTED_EDGE('',*,*,#20764,.T.);
#29771=ORIENTED_EDGE('',*,*,#20765,.T.);
#29772=ORIENTED_EDGE('',*,*,#20586,.F.);
#29773=ORIENTED_EDGE('',*,*,#20587,.F.);
#29774=ORIENTED_EDGE('',*,*,#20765,.F.);
#29775=ORIENTED_EDGE('',*,*,#20763,.F.);
#29776=ORIENTED_EDGE('',*,*,#20583,.F.);
#29777=ORIENTED_EDGE('',*,*,#20766,.F.);
#29778=ORIENTED_EDGE('',*,*,#20767,.F.);
#29779=ORIENTED_EDGE('',*,*,#20584,.F.);
#29780=ORIENTED_EDGE('',*,*,#20767,.T.);
#29781=ORIENTED_EDGE('',*,*,#20768,.F.);
#29782=ORIENTED_EDGE('',*,*,#20641,.F.);
#29783=ORIENTED_EDGE('',*,*,#20582,.F.);
#29784=ORIENTED_EDGE('',*,*,#20642,.F.);
#29785=ORIENTED_EDGE('',*,*,#20768,.T.);
#29786=ORIENTED_EDGE('',*,*,#20766,.T.);
#29787=ORIENTED_EDGE('',*,*,#20580,.F.);
#29788=ORIENTED_EDGE('',*,*,#20769,.T.);
#29789=ORIENTED_EDGE('',*,*,#20770,.F.);
#29790=ORIENTED_EDGE('',*,*,#20643,.F.);
#29791=ORIENTED_EDGE('',*,*,#20644,.F.);
#29792=ORIENTED_EDGE('',*,*,#20770,.T.);
#29793=ORIENTED_EDGE('',*,*,#20771,.T.);
#29794=ORIENTED_EDGE('',*,*,#20578,.F.);
#29795=ORIENTED_EDGE('',*,*,#20579,.F.);
#29796=ORIENTED_EDGE('',*,*,#20771,.F.);
#29797=ORIENTED_EDGE('',*,*,#20769,.F.);
#29798=ORIENTED_EDGE('',*,*,#20575,.F.);
#29799=ORIENTED_EDGE('',*,*,#20772,.F.);
#29800=ORIENTED_EDGE('',*,*,#20773,.F.);
#29801=ORIENTED_EDGE('',*,*,#20576,.F.);
#29802=ORIENTED_EDGE('',*,*,#20773,.T.);
#29803=ORIENTED_EDGE('',*,*,#20774,.F.);
#29804=ORIENTED_EDGE('',*,*,#20645,.F.);
#29805=ORIENTED_EDGE('',*,*,#20574,.F.);
#29806=ORIENTED_EDGE('',*,*,#20646,.F.);
#29807=ORIENTED_EDGE('',*,*,#20774,.T.);
#29808=ORIENTED_EDGE('',*,*,#20772,.T.);
#29809=ORIENTED_EDGE('',*,*,#20572,.F.);
#29810=ORIENTED_EDGE('',*,*,#20775,.T.);
#29811=ORIENTED_EDGE('',*,*,#20776,.F.);
#29812=ORIENTED_EDGE('',*,*,#20647,.F.);
#29813=ORIENTED_EDGE('',*,*,#20648,.F.);
#29814=ORIENTED_EDGE('',*,*,#20776,.T.);
#29815=ORIENTED_EDGE('',*,*,#20777,.T.);
#29816=ORIENTED_EDGE('',*,*,#20570,.F.);
#29817=ORIENTED_EDGE('',*,*,#20571,.F.);
#29818=ORIENTED_EDGE('',*,*,#20777,.F.);
#29819=ORIENTED_EDGE('',*,*,#20775,.F.);
#29820=ORIENTED_EDGE('',*,*,#20567,.F.);
#29821=ORIENTED_EDGE('',*,*,#20778,.F.);
#29822=ORIENTED_EDGE('',*,*,#20779,.F.);
#29823=ORIENTED_EDGE('',*,*,#20568,.F.);
#29824=ORIENTED_EDGE('',*,*,#20779,.T.);
#29825=ORIENTED_EDGE('',*,*,#20780,.F.);
#29826=ORIENTED_EDGE('',*,*,#20649,.F.);
#29827=ORIENTED_EDGE('',*,*,#20566,.F.);
#29828=ORIENTED_EDGE('',*,*,#20650,.F.);
#29829=ORIENTED_EDGE('',*,*,#20780,.T.);
#29830=ORIENTED_EDGE('',*,*,#20778,.T.);
#29831=ORIENTED_EDGE('',*,*,#20564,.F.);
#29832=ORIENTED_EDGE('',*,*,#20781,.T.);
#29833=ORIENTED_EDGE('',*,*,#20782,.F.);
#29834=ORIENTED_EDGE('',*,*,#20651,.F.);
#29835=ORIENTED_EDGE('',*,*,#20652,.F.);
#29836=ORIENTED_EDGE('',*,*,#20782,.T.);
#29837=ORIENTED_EDGE('',*,*,#20783,.T.);
#29838=ORIENTED_EDGE('',*,*,#20562,.F.);
#29839=ORIENTED_EDGE('',*,*,#20563,.F.);
#29840=ORIENTED_EDGE('',*,*,#20783,.F.);
#29841=ORIENTED_EDGE('',*,*,#20781,.F.);
#29842=ORIENTED_EDGE('',*,*,#20559,.F.);
#29843=ORIENTED_EDGE('',*,*,#20784,.F.);
#29844=ORIENTED_EDGE('',*,*,#20785,.F.);
#29845=ORIENTED_EDGE('',*,*,#20560,.F.);
#29846=ORIENTED_EDGE('',*,*,#20785,.T.);
#29847=ORIENTED_EDGE('',*,*,#20786,.F.);
#29848=ORIENTED_EDGE('',*,*,#20653,.F.);
#29849=ORIENTED_EDGE('',*,*,#20558,.F.);
#29850=ORIENTED_EDGE('',*,*,#20654,.F.);
#29851=ORIENTED_EDGE('',*,*,#20786,.T.);
#29852=ORIENTED_EDGE('',*,*,#20784,.T.);
#29853=ORIENTED_EDGE('',*,*,#20556,.F.);
#29854=ORIENTED_EDGE('',*,*,#20787,.T.);
#29855=ORIENTED_EDGE('',*,*,#20788,.F.);
#29856=ORIENTED_EDGE('',*,*,#20655,.F.);
#29857=ORIENTED_EDGE('',*,*,#20656,.F.);
#29858=ORIENTED_EDGE('',*,*,#20788,.T.);
#29859=ORIENTED_EDGE('',*,*,#20789,.T.);
#29860=ORIENTED_EDGE('',*,*,#20554,.F.);
#29861=ORIENTED_EDGE('',*,*,#20555,.F.);
#29862=ORIENTED_EDGE('',*,*,#20789,.F.);
#29863=ORIENTED_EDGE('',*,*,#20787,.F.);
#29864=ORIENTED_EDGE('',*,*,#20551,.F.);
#29865=ORIENTED_EDGE('',*,*,#20790,.F.);
#29866=ORIENTED_EDGE('',*,*,#20791,.F.);
#29867=ORIENTED_EDGE('',*,*,#20552,.F.);
#29868=ORIENTED_EDGE('',*,*,#20791,.T.);
#29869=ORIENTED_EDGE('',*,*,#20792,.F.);
#29870=ORIENTED_EDGE('',*,*,#20657,.F.);
#29871=ORIENTED_EDGE('',*,*,#20550,.F.);
#29872=ORIENTED_EDGE('',*,*,#20658,.F.);
#29873=ORIENTED_EDGE('',*,*,#20792,.T.);
#29874=ORIENTED_EDGE('',*,*,#20790,.T.);
#29875=ORIENTED_EDGE('',*,*,#20548,.F.);
#29876=ORIENTED_EDGE('',*,*,#20793,.T.);
#29877=ORIENTED_EDGE('',*,*,#20794,.F.);
#29878=ORIENTED_EDGE('',*,*,#20659,.F.);
#29879=ORIENTED_EDGE('',*,*,#20660,.F.);
#29880=ORIENTED_EDGE('',*,*,#20794,.T.);
#29881=ORIENTED_EDGE('',*,*,#20795,.T.);
#29882=ORIENTED_EDGE('',*,*,#20546,.F.);
#29883=ORIENTED_EDGE('',*,*,#20547,.F.);
#29884=ORIENTED_EDGE('',*,*,#20795,.F.);
#29885=ORIENTED_EDGE('',*,*,#20793,.F.);
#29886=ORIENTED_EDGE('',*,*,#20463,.T.);
#29887=ORIENTED_EDGE('',*,*,#20796,.T.);
#29888=ORIENTED_EDGE('',*,*,#20476,.T.);
#29889=ORIENTED_EDGE('',*,*,#20477,.T.);
#29890=ORIENTED_EDGE('',*,*,#20796,.F.);
#29891=ORIENTED_EDGE('',*,*,#20693,.F.);
#29892=ORIENTED_EDGE('',*,*,#20797,.T.);
#29893=ORIENTED_EDGE('',*,*,#20798,.F.);
#29894=ORIENTED_EDGE('',*,*,#20799,.F.);
#29895=ORIENTED_EDGE('',*,*,#20800,.F.);
#29896=ORIENTED_EDGE('',*,*,#20801,.F.);
#29897=ORIENTED_EDGE('',*,*,#20802,.F.);
#29898=ORIENTED_EDGE('',*,*,#20803,.F.);
#29899=ORIENTED_EDGE('',*,*,#20804,.F.);
#29900=ORIENTED_EDGE('',*,*,#20805,.F.);
#29901=ORIENTED_EDGE('',*,*,#20806,.F.);
#29902=ORIENTED_EDGE('',*,*,#20807,.F.);
#29903=ORIENTED_EDGE('',*,*,#20808,.F.);
#29904=ORIENTED_EDGE('',*,*,#20809,.F.);
#29905=ORIENTED_EDGE('',*,*,#20810,.F.);
#29906=ORIENTED_EDGE('',*,*,#20811,.F.);
#29907=ORIENTED_EDGE('',*,*,#20812,.F.);
#29908=ORIENTED_EDGE('',*,*,#20813,.F.);
#29909=ORIENTED_EDGE('',*,*,#20814,.F.);
#29910=ORIENTED_EDGE('',*,*,#20815,.F.);
#29911=ORIENTED_EDGE('',*,*,#20816,.T.);
#29912=ORIENTED_EDGE('',*,*,#20797,.F.);
#29913=ORIENTED_EDGE('',*,*,#20816,.F.);
#29914=ORIENTED_EDGE('',*,*,#20817,.F.);
#29915=ORIENTED_EDGE('',*,*,#20814,.T.);
#29916=ORIENTED_EDGE('',*,*,#20818,.F.);
#29917=ORIENTED_EDGE('',*,*,#20819,.F.);
#29918=ORIENTED_EDGE('',*,*,#20820,.F.);
#29919=ORIENTED_EDGE('',*,*,#20821,.F.);
#29920=ORIENTED_EDGE('',*,*,#20822,.F.);
#29921=ORIENTED_EDGE('',*,*,#20811,.T.);
#29922=ORIENTED_EDGE('',*,*,#20823,.F.);
#29923=ORIENTED_EDGE('',*,*,#20799,.T.);
#29924=ORIENTED_EDGE('',*,*,#20824,.F.);
#29925=ORIENTED_EDGE('',*,*,#20825,.F.);
#29926=ORIENTED_EDGE('',*,*,#20826,.F.);
#29927=ORIENTED_EDGE('',*,*,#20827,.F.);
#29928=ORIENTED_EDGE('',*,*,#20828,.F.);
#29929=ORIENTED_EDGE('',*,*,#20808,.T.);
#29930=ORIENTED_EDGE('',*,*,#20829,.F.);
#29931=ORIENTED_EDGE('',*,*,#20802,.T.);
#29932=ORIENTED_EDGE('',*,*,#20830,.F.);
#29933=ORIENTED_EDGE('',*,*,#20831,.F.);
#29934=ORIENTED_EDGE('',*,*,#20832,.F.);
#29935=ORIENTED_EDGE('',*,*,#20833,.F.);
#29936=ORIENTED_EDGE('',*,*,#20834,.F.);
#29937=ORIENTED_EDGE('',*,*,#20805,.T.);
#29938=ORIENTED_EDGE('',*,*,#20803,.T.);
#29939=ORIENTED_EDGE('',*,*,#20829,.T.);
#29940=ORIENTED_EDGE('',*,*,#20835,.F.);
#29941=ORIENTED_EDGE('',*,*,#20830,.T.);
#29942=ORIENTED_EDGE('',*,*,#20801,.T.);
#29943=ORIENTED_EDGE('',*,*,#20836,.T.);
#29944=ORIENTED_EDGE('',*,*,#20837,.T.);
#29945=ORIENTED_EDGE('',*,*,#20838,.F.);
#29946=ORIENTED_EDGE('',*,*,#20800,.T.);
#29947=ORIENTED_EDGE('',*,*,#20823,.T.);
#29948=ORIENTED_EDGE('',*,*,#20839,.F.);
#29949=ORIENTED_EDGE('',*,*,#20824,.T.);
#29950=ORIENTED_EDGE('',*,*,#20798,.T.);
#29951=ORIENTED_EDGE('',*,*,#20840,.T.);
#29952=ORIENTED_EDGE('',*,*,#20841,.T.);
#29953=ORIENTED_EDGE('',*,*,#20836,.F.);
#29954=ORIENTED_EDGE('',*,*,#20815,.T.);
#29955=ORIENTED_EDGE('',*,*,#20817,.T.);
#29956=ORIENTED_EDGE('',*,*,#20842,.F.);
#29957=ORIENTED_EDGE('',*,*,#20818,.T.);
#29958=ORIENTED_EDGE('',*,*,#20813,.T.);
#29959=ORIENTED_EDGE('',*,*,#20843,.T.);
#29960=ORIENTED_EDGE('',*,*,#20844,.T.);
#29961=ORIENTED_EDGE('',*,*,#20840,.F.);
#29962=ORIENTED_EDGE('',*,*,#20819,.T.);
#29963=ORIENTED_EDGE('',*,*,#20842,.T.);
#29964=ORIENTED_EDGE('',*,*,#20825,.T.);
#29965=ORIENTED_EDGE('',*,*,#20839,.T.);
#29966=ORIENTED_EDGE('',*,*,#20821,.T.);
#29967=ORIENTED_EDGE('',*,*,#20845,.T.);
#29968=ORIENTED_EDGE('',*,*,#20831,.T.);
#29969=ORIENTED_EDGE('',*,*,#20835,.T.);
#29970=ORIENTED_EDGE('',*,*,#20827,.T.);
#29971=ORIENTED_EDGE('',*,*,#20846,.T.);
#29972=ORIENTED_EDGE('',*,*,#20833,.T.);
#29973=ORIENTED_EDGE('',*,*,#20847,.T.);
#29974=ORIENTED_EDGE('',*,*,#20848,.F.);
#29975=ORIENTED_EDGE('',*,*,#20849,.F.);
#29976=ORIENTED_EDGE('',*,*,#20850,.F.);
#29977=ORIENTED_EDGE('',*,*,#20851,.F.);
#29978=ORIENTED_EDGE('',*,*,#20844,.F.);
#29979=ORIENTED_EDGE('',*,*,#20852,.F.);
#29980=ORIENTED_EDGE('',*,*,#20841,.F.);
#29981=ORIENTED_EDGE('',*,*,#20853,.F.);
#29982=ORIENTED_EDGE('',*,*,#20837,.F.);
#29983=ORIENTED_EDGE('',*,*,#20854,.F.);
#29984=ORIENTED_EDGE('',*,*,#20855,.F.);
#29985=ORIENTED_EDGE('',*,*,#20856,.F.);
#29986=ORIENTED_EDGE('',*,*,#20857,.T.);
#29987=ORIENTED_EDGE('',*,*,#20852,.T.);
#29988=ORIENTED_EDGE('',*,*,#20851,.T.);
#29989=ORIENTED_EDGE('',*,*,#20849,.T.);
#29990=ORIENTED_EDGE('',*,*,#20856,.T.);
#29991=ORIENTED_EDGE('',*,*,#20854,.T.);
#29992=ORIENTED_EDGE('',*,*,#20853,.T.);
#29993=ORIENTED_EDGE('',*,*,#20857,.F.);
#29994=ORIENTED_EDGE('',*,*,#20807,.T.);
#29995=ORIENTED_EDGE('',*,*,#20858,.T.);
#29996=ORIENTED_EDGE('',*,*,#20848,.T.);
#29997=ORIENTED_EDGE('',*,*,#20859,.F.);
#29998=ORIENTED_EDGE('',*,*,#20809,.T.);
#29999=ORIENTED_EDGE('',*,*,#20828,.T.);
#30000=ORIENTED_EDGE('',*,*,#20846,.F.);
#30001=ORIENTED_EDGE('',*,*,#20826,.T.);
#30002=ORIENTED_EDGE('',*,*,#20804,.T.);
#30003=ORIENTED_EDGE('',*,*,#20838,.T.);
#30004=ORIENTED_EDGE('',*,*,#20855,.T.);
#30005=ORIENTED_EDGE('',*,*,#20858,.F.);
#30006=ORIENTED_EDGE('',*,*,#20806,.T.);
#30007=ORIENTED_EDGE('',*,*,#20834,.T.);
#30008=ORIENTED_EDGE('',*,*,#20847,.F.);
#30009=ORIENTED_EDGE('',*,*,#20832,.T.);
#30010=ORIENTED_EDGE('',*,*,#20810,.T.);
#30011=ORIENTED_EDGE('',*,*,#20859,.T.);
#30012=ORIENTED_EDGE('',*,*,#20850,.T.);
#30013=ORIENTED_EDGE('',*,*,#20843,.F.);
#30014=ORIENTED_EDGE('',*,*,#20812,.T.);
#30015=ORIENTED_EDGE('',*,*,#20822,.T.);
#30016=ORIENTED_EDGE('',*,*,#20845,.F.);
#30017=ORIENTED_EDGE('',*,*,#20820,.T.);
#30018=ORIENTED_EDGE('',*,*,#20860,.F.);
#30019=ORIENTED_EDGE('',*,*,#20861,.T.);
#30020=ORIENTED_EDGE('',*,*,#20862,.T.);
#30021=ORIENTED_EDGE('',*,*,#20863,.T.);
#30022=ORIENTED_EDGE('',*,*,#20864,.F.);
#30023=ORIENTED_EDGE('',*,*,#20865,.T.);
#30024=ORIENTED_EDGE('',*,*,#20860,.T.);
#30025=ORIENTED_EDGE('',*,*,#20866,.T.);
#30026=ORIENTED_EDGE('',*,*,#20867,.F.);
#30027=ORIENTED_EDGE('',*,*,#20868,.T.);
#30028=ORIENTED_EDGE('',*,*,#20864,.T.);
#30029=ORIENTED_EDGE('',*,*,#20869,.T.);
#30030=ORIENTED_EDGE('',*,*,#20870,.F.);
#30031=ORIENTED_EDGE('',*,*,#20871,.T.);
#30032=ORIENTED_EDGE('',*,*,#20867,.T.);
#30033=ORIENTED_EDGE('',*,*,#20872,.T.);
#30034=ORIENTED_EDGE('',*,*,#20873,.F.);
#30035=ORIENTED_EDGE('',*,*,#20874,.T.);
#30036=ORIENTED_EDGE('',*,*,#20870,.T.);
#30037=ORIENTED_EDGE('',*,*,#20875,.T.);
#30038=ORIENTED_EDGE('',*,*,#20876,.F.);
#30039=ORIENTED_EDGE('',*,*,#20877,.T.);
#30040=ORIENTED_EDGE('',*,*,#20873,.T.);
#30041=ORIENTED_EDGE('',*,*,#20878,.T.);
#30042=ORIENTED_EDGE('',*,*,#20879,.F.);
#30043=ORIENTED_EDGE('',*,*,#20880,.T.);
#30044=ORIENTED_EDGE('',*,*,#20876,.T.);
#30045=ORIENTED_EDGE('',*,*,#20881,.T.);
#30046=ORIENTED_EDGE('',*,*,#20882,.F.);
#30047=ORIENTED_EDGE('',*,*,#20883,.T.);
#30048=ORIENTED_EDGE('',*,*,#20879,.T.);
#30049=ORIENTED_EDGE('',*,*,#20884,.T.);
#30050=ORIENTED_EDGE('',*,*,#20885,.F.);
#30051=ORIENTED_EDGE('',*,*,#20886,.T.);
#30052=ORIENTED_EDGE('',*,*,#20882,.T.);
#30053=ORIENTED_EDGE('',*,*,#20887,.T.);
#30054=ORIENTED_EDGE('',*,*,#20888,.F.);
#30055=ORIENTED_EDGE('',*,*,#20889,.T.);
#30056=ORIENTED_EDGE('',*,*,#20885,.T.);
#30057=ORIENTED_EDGE('',*,*,#20890,.T.);
#30058=ORIENTED_EDGE('',*,*,#20891,.F.);
#30059=ORIENTED_EDGE('',*,*,#20892,.T.);
#30060=ORIENTED_EDGE('',*,*,#20888,.T.);
#30061=ORIENTED_EDGE('',*,*,#20893,.T.);
#30062=ORIENTED_EDGE('',*,*,#20894,.F.);
#30063=ORIENTED_EDGE('',*,*,#20895,.F.);
#30064=ORIENTED_EDGE('',*,*,#20896,.F.);
#30065=ORIENTED_EDGE('',*,*,#20897,.T.);
#30066=ORIENTED_EDGE('',*,*,#20898,.F.);
#30067=ORIENTED_EDGE('',*,*,#20899,.F.);
#30068=ORIENTED_EDGE('',*,*,#20894,.T.);
#30069=ORIENTED_EDGE('',*,*,#20900,.T.);
#30070=ORIENTED_EDGE('',*,*,#20901,.T.);
#30071=ORIENTED_EDGE('',*,*,#20902,.F.);
#30072=ORIENTED_EDGE('',*,*,#20903,.F.);
#30073=ORIENTED_EDGE('',*,*,#20898,.T.);
#30074=ORIENTED_EDGE('',*,*,#20904,.T.);
#30075=ORIENTED_EDGE('',*,*,#20905,.T.);
#30076=ORIENTED_EDGE('',*,*,#20906,.F.);
#30077=ORIENTED_EDGE('',*,*,#20907,.F.);
#30078=ORIENTED_EDGE('',*,*,#20902,.T.);
#30079=ORIENTED_EDGE('',*,*,#20908,.T.);
#30080=ORIENTED_EDGE('',*,*,#20909,.T.);
#30081=ORIENTED_EDGE('',*,*,#20910,.F.);
#30082=ORIENTED_EDGE('',*,*,#20911,.F.);
#30083=ORIENTED_EDGE('',*,*,#20906,.T.);
#30084=ORIENTED_EDGE('',*,*,#20912,.T.);
#30085=ORIENTED_EDGE('',*,*,#20913,.T.);
#30086=ORIENTED_EDGE('',*,*,#20914,.F.);
#30087=ORIENTED_EDGE('',*,*,#20915,.F.);
#30088=ORIENTED_EDGE('',*,*,#20910,.T.);
#30089=ORIENTED_EDGE('',*,*,#20916,.T.);
#30090=ORIENTED_EDGE('',*,*,#20917,.T.);
#30091=ORIENTED_EDGE('',*,*,#20918,.F.);
#30092=ORIENTED_EDGE('',*,*,#20919,.F.);
#30093=ORIENTED_EDGE('',*,*,#20914,.T.);
#30094=ORIENTED_EDGE('',*,*,#20920,.T.);
#30095=ORIENTED_EDGE('',*,*,#20921,.T.);
#30096=ORIENTED_EDGE('',*,*,#20922,.F.);
#30097=ORIENTED_EDGE('',*,*,#20923,.F.);
#30098=ORIENTED_EDGE('',*,*,#20918,.T.);
#30099=ORIENTED_EDGE('',*,*,#20924,.T.);
#30100=ORIENTED_EDGE('',*,*,#20925,.T.);
#30101=ORIENTED_EDGE('',*,*,#20926,.F.);
#30102=ORIENTED_EDGE('',*,*,#20927,.F.);
#30103=ORIENTED_EDGE('',*,*,#20922,.T.);
#30104=ORIENTED_EDGE('',*,*,#20928,.T.);
#30105=ORIENTED_EDGE('',*,*,#20929,.T.);
#30106=ORIENTED_EDGE('',*,*,#20930,.F.);
#30107=ORIENTED_EDGE('',*,*,#20931,.F.);
#30108=ORIENTED_EDGE('',*,*,#20926,.T.);
#30109=ORIENTED_EDGE('',*,*,#20932,.T.);
#30110=ORIENTED_EDGE('',*,*,#20933,.T.);
#30111=ORIENTED_EDGE('',*,*,#20930,.T.);
#30112=ORIENTED_EDGE('',*,*,#20934,.T.);
#30113=ORIENTED_EDGE('',*,*,#20935,.T.);
#30114=ORIENTED_EDGE('',*,*,#20936,.F.);
#30115=ORIENTED_EDGE('',*,*,#20937,.F.);
#30116=ORIENTED_EDGE('',*,*,#20938,.F.);
#30117=ORIENTED_EDGE('',*,*,#20891,.T.);
#30118=ORIENTED_EDGE('',*,*,#20939,.T.);
#30119=ORIENTED_EDGE('',*,*,#20940,.F.);
#30120=ORIENTED_EDGE('',*,*,#20941,.T.);
#30121=ORIENTED_EDGE('',*,*,#20942,.F.);
#30122=ORIENTED_EDGE('',*,*,#20895,.T.);
#30123=ORIENTED_EDGE('',*,*,#20899,.T.);
#30124=ORIENTED_EDGE('',*,*,#20903,.T.);
#30125=ORIENTED_EDGE('',*,*,#20907,.T.);
#30126=ORIENTED_EDGE('',*,*,#20911,.T.);
#30127=ORIENTED_EDGE('',*,*,#20915,.T.);
#30128=ORIENTED_EDGE('',*,*,#20919,.T.);
#30129=ORIENTED_EDGE('',*,*,#20923,.T.);
#30130=ORIENTED_EDGE('',*,*,#20927,.T.);
#30131=ORIENTED_EDGE('',*,*,#20931,.T.);
#30132=ORIENTED_EDGE('',*,*,#20938,.T.);
#30133=ORIENTED_EDGE('',*,*,#20937,.T.);
#30134=ORIENTED_EDGE('',*,*,#20943,.F.);
#30135=ORIENTED_EDGE('',*,*,#20944,.F.);
#30136=ORIENTED_EDGE('',*,*,#20939,.F.);
#30137=ORIENTED_EDGE('',*,*,#20893,.F.);
#30138=ORIENTED_EDGE('',*,*,#20890,.F.);
#30139=ORIENTED_EDGE('',*,*,#20887,.F.);
#30140=ORIENTED_EDGE('',*,*,#20884,.F.);
#30141=ORIENTED_EDGE('',*,*,#20881,.F.);
#30142=ORIENTED_EDGE('',*,*,#20878,.F.);
#30143=ORIENTED_EDGE('',*,*,#20875,.F.);
#30144=ORIENTED_EDGE('',*,*,#20872,.F.);
#30145=ORIENTED_EDGE('',*,*,#20869,.F.);
#30146=ORIENTED_EDGE('',*,*,#20866,.F.);
#30147=ORIENTED_EDGE('',*,*,#20863,.F.);
#30148=ORIENTED_EDGE('',*,*,#20945,.F.);
#30149=ORIENTED_EDGE('',*,*,#20946,.F.);
#30150=ORIENTED_EDGE('',*,*,#20943,.T.);
#30151=ORIENTED_EDGE('',*,*,#20936,.T.);
#30152=ORIENTED_EDGE('',*,*,#20947,.T.);
#30153=ORIENTED_EDGE('',*,*,#20948,.T.);
#30154=ORIENTED_EDGE('',*,*,#20949,.F.);
#30155=ORIENTED_EDGE('',*,*,#20950,.F.);
#30156=ORIENTED_EDGE('',*,*,#20861,.F.);
#30157=ORIENTED_EDGE('',*,*,#20865,.F.);
#30158=ORIENTED_EDGE('',*,*,#20868,.F.);
#30159=ORIENTED_EDGE('',*,*,#20871,.F.);
#30160=ORIENTED_EDGE('',*,*,#20874,.F.);
#30161=ORIENTED_EDGE('',*,*,#20877,.F.);
#30162=ORIENTED_EDGE('',*,*,#20880,.F.);
#30163=ORIENTED_EDGE('',*,*,#20883,.F.);
#30164=ORIENTED_EDGE('',*,*,#20886,.F.);
#30165=ORIENTED_EDGE('',*,*,#20889,.F.);
#30166=ORIENTED_EDGE('',*,*,#20892,.F.);
#30167=ORIENTED_EDGE('',*,*,#20941,.F.);
#30168=ORIENTED_EDGE('',*,*,#20948,.F.);
#30169=ORIENTED_EDGE('',*,*,#20947,.F.);
#30170=ORIENTED_EDGE('',*,*,#20935,.F.);
#30171=ORIENTED_EDGE('',*,*,#20934,.F.);
#30172=ORIENTED_EDGE('',*,*,#20933,.F.);
#30173=ORIENTED_EDGE('',*,*,#20932,.F.);
#30174=ORIENTED_EDGE('',*,*,#20929,.F.);
#30175=ORIENTED_EDGE('',*,*,#20928,.F.);
#30176=ORIENTED_EDGE('',*,*,#20925,.F.);
#30177=ORIENTED_EDGE('',*,*,#20924,.F.);
#30178=ORIENTED_EDGE('',*,*,#20921,.F.);
#30179=ORIENTED_EDGE('',*,*,#20920,.F.);
#30180=ORIENTED_EDGE('',*,*,#20917,.F.);
#30181=ORIENTED_EDGE('',*,*,#20916,.F.);
#30182=ORIENTED_EDGE('',*,*,#20913,.F.);
#30183=ORIENTED_EDGE('',*,*,#20912,.F.);
#30184=ORIENTED_EDGE('',*,*,#20909,.F.);
#30185=ORIENTED_EDGE('',*,*,#20908,.F.);
#30186=ORIENTED_EDGE('',*,*,#20905,.F.);
#30187=ORIENTED_EDGE('',*,*,#20904,.F.);
#30188=ORIENTED_EDGE('',*,*,#20901,.F.);
#30189=ORIENTED_EDGE('',*,*,#20900,.F.);
#30190=ORIENTED_EDGE('',*,*,#20897,.F.);
#30191=ORIENTED_EDGE('',*,*,#20951,.T.);
#30192=ORIENTED_EDGE('',*,*,#20952,.T.);
#30193=ORIENTED_EDGE('',*,*,#20949,.T.);
#30194=ORIENTED_EDGE('',*,*,#20940,.T.);
#30195=ORIENTED_EDGE('',*,*,#20944,.T.);
#30196=ORIENTED_EDGE('',*,*,#20946,.T.);
#30197=ORIENTED_EDGE('',*,*,#20952,.F.);
#30198=ORIENTED_EDGE('',*,*,#20953,.F.);
#30199=ORIENTED_EDGE('',*,*,#20951,.F.);
#30200=ORIENTED_EDGE('',*,*,#20954,.F.);
#30201=ORIENTED_EDGE('',*,*,#20955,.F.);
#30202=ORIENTED_EDGE('',*,*,#20956,.F.);
#30203=ORIENTED_EDGE('',*,*,#20957,.F.);
#30204=ORIENTED_EDGE('',*,*,#20958,.F.);
#30205=ORIENTED_EDGE('',*,*,#20959,.F.);
#30206=ORIENTED_EDGE('',*,*,#20957,.T.);
#30207=ORIENTED_EDGE('',*,*,#20960,.F.);
#30208=ORIENTED_EDGE('',*,*,#20961,.F.);
#30209=ORIENTED_EDGE('',*,*,#20962,.F.);
#30210=ORIENTED_EDGE('',*,*,#20963,.F.);
#30211=ORIENTED_EDGE('',*,*,#20964,.F.);
#30212=ORIENTED_EDGE('',*,*,#20965,.F.);
#30213=ORIENTED_EDGE('',*,*,#20966,.F.);
#30214=ORIENTED_EDGE('',*,*,#20967,.F.);
#30215=ORIENTED_EDGE('',*,*,#20968,.F.);
#30216=ORIENTED_EDGE('',*,*,#20955,.T.);
#30217=ORIENTED_EDGE('',*,*,#20954,.T.);
#30218=ORIENTED_EDGE('',*,*,#20969,.T.);
#30219=ORIENTED_EDGE('',*,*,#20953,.T.);
#30220=ORIENTED_EDGE('',*,*,#20969,.F.);
#30221=ORIENTED_EDGE('',*,*,#20958,.T.);
#30222=ORIENTED_EDGE('',*,*,#20959,.T.);
#30223=ORIENTED_EDGE('',*,*,#20970,.F.);
#30224=ORIENTED_EDGE('',*,*,#20960,.T.);
#30225=ORIENTED_EDGE('',*,*,#20956,.T.);
#30226=ORIENTED_EDGE('',*,*,#20968,.T.);
#30227=ORIENTED_EDGE('',*,*,#20971,.F.);
#30228=ORIENTED_EDGE('',*,*,#20964,.T.);
#30229=ORIENTED_EDGE('',*,*,#20962,.T.);
#30230=ORIENTED_EDGE('',*,*,#20972,.T.);
#30231=ORIENTED_EDGE('',*,*,#20966,.T.);
#30232=ORIENTED_EDGE('',*,*,#20973,.T.);
#30233=ORIENTED_EDGE('',*,*,#20963,.T.);
#30234=ORIENTED_EDGE('',*,*,#20972,.F.);
#30235=ORIENTED_EDGE('',*,*,#20961,.T.);
#30236=ORIENTED_EDGE('',*,*,#20970,.T.);
#30237=ORIENTED_EDGE('',*,*,#20974,.F.);
#30238=ORIENTED_EDGE('',*,*,#20974,.T.);
#30239=ORIENTED_EDGE('',*,*,#20975,.T.);
#30240=ORIENTED_EDGE('',*,*,#20945,.T.);
#30241=ORIENTED_EDGE('',*,*,#20862,.F.);
#30242=ORIENTED_EDGE('',*,*,#20950,.T.);
#30243=ORIENTED_EDGE('',*,*,#20896,.T.);
#30244=ORIENTED_EDGE('',*,*,#20942,.T.);
#30245=ORIENTED_EDGE('',*,*,#20975,.F.);
#30246=ORIENTED_EDGE('',*,*,#20965,.T.);
#30247=ORIENTED_EDGE('',*,*,#20971,.T.);
#30248=ORIENTED_EDGE('',*,*,#20967,.T.);
#30249=ORIENTED_EDGE('',*,*,#20973,.F.);
#30250=CONICAL_SURFACE('',#32234,1.65,0.785398163397459);
#30251=CONICAL_SURFACE('',#32241,1.65,0.785398163397459);
#30252=CONICAL_SURFACE('',#32245,1.55,1.02974425867666);
#30253=CONICAL_SURFACE('',#32246,1.55,1.02974425867666);
#30254=CONICAL_SURFACE('',#32247,1.65,0.785398163397448);
#30255=CONICAL_SURFACE('',#32254,1.65,0.785398163397448);
#30256=CONICAL_SURFACE('',#32258,0.775000000000001,1.02974425867665);
#30257=CONICAL_SURFACE('',#32259,0.775,1.02974425867665);
#30258=CONICAL_SURFACE('',#32277,1.125,0.785398163397456);
#30259=CONICAL_SURFACE('',#32285,1.125,0.785398163397456);
#30260=CONICAL_SURFACE('',#32290,0.524999999999993,1.02974425867665);
#30261=CONICAL_SURFACE('',#32291,0.524999999999993,1.02974425867665);
#30262=CONICAL_SURFACE('',#32292,1.125,0.785398163397445);
#30263=CONICAL_SURFACE('',#32307,1.125,0.785398163397445);
#30264=CONICAL_SURFACE('',#32311,1.125,0.785398163397445);
#30265=CONICAL_SURFACE('',#32315,1.125,0.785398163397445);
#30266=CONICAL_SURFACE('',#32319,0.525,1.02974425867665);
#30267=CONICAL_SURFACE('',#32320,0.525,1.02974425867665);
#30268=CONICAL_SURFACE('',#32321,0.525,1.02974425867665);
#30269=CONICAL_SURFACE('',#32322,0.525,1.02974425867665);
#30270=CONICAL_SURFACE('',#32323,2.2,0.785398163397451);
#30271=CONICAL_SURFACE('',#32327,2.2,0.785398163397452);
#30272=CONICAL_SURFACE('',#32331,2.2,0.785398163397452);
#30273=CONICAL_SURFACE('',#32335,2.2,0.785398163397452);
#30274=CONICAL_SURFACE('',#32339,2.2,0.785398163397452);
#30275=CONICAL_SURFACE('',#32343,2.2,0.785398163397451);
#30276=CONICAL_SURFACE('',#32347,1.025,1.02974425867666);
#30277=CONICAL_SURFACE('',#32348,1.025,1.02974425867666);
#30278=CONICAL_SURFACE('',#32349,1.025,1.02974425867666);
#30279=CONICAL_SURFACE('',#32350,1.025,1.02974425867666);
#30280=CONICAL_SURFACE('',#32351,1.025,1.02974425867666);
#30281=CONICAL_SURFACE('',#32352,1.025,1.02974425867666);
#30282=CONICAL_SURFACE('',#32385,2.675,0.785398163397444);
#30283=CONICAL_SURFACE('',#32394,2.675,0.785398163397444);
#30284=CONICAL_SURFACE('',#32398,4.35,0.785398163397459);
#30285=CONICAL_SURFACE('',#32402,4.35,0.785398163397459);
#30286=CONICAL_SURFACE('',#32463,1.85,0.78539816339743);
#30287=CONICAL_SURFACE('',#32468,2.35,0.785398163397451);
#30288=CONICAL_SURFACE('',#32474,1.85,0.785398163397448);
#30289=CONICAL_SURFACE('',#32739,3.905,1.43962768039283);
#30290=CONICAL_SURFACE('',#32744,7.2,0.785398163397444);
#30291=CONICAL_SURFACE('',#32748,7.3,0.785398163397437);
#30292=CONICAL_SURFACE('',#33360,3.15,0.785398163397449);
#30293=CONICAL_SURFACE('',#33369,3.15,0.785398163397449);
#30294=CONICAL_SURFACE('',#33442,0.916025403784424,0.785398163397437);
#30295=CONICAL_SURFACE('',#33483,0.433012701892235,1.02974425867666);
#30296=CONICAL_SURFACE('',#33489,1.25,0.785398163397456);
#30297=CONICAL_SURFACE('',#33490,1.35,0.785398163397469);
#30298=CONICAL_SURFACE('',#33494,1.125,0.785398163397452);
#30299=CONICAL_SURFACE('',#33501,1.05,1.02974425867665);
#30300=CONICAL_SURFACE('',#33502,1.125,0.785398163397452);
#30301=CONICAL_SURFACE('',#33509,0.525,1.02974425867665);
#30302=CONICAL_SURFACE('',#33510,1.65,0.785398163397448);
#30303=CONICAL_SURFACE('',#33520,1.65,0.785398163397448);
#30304=CONICAL_SURFACE('',#33524,0.775000000000001,1.02974425867666);
#30305=CONICAL_SURFACE('',#33525,0.775,1.02974425867666);
#30306=CONICAL_SURFACE('',#33526,3.15,0.785398163397448);
#30307=CONICAL_SURFACE('',#33530,3.15,0.785398163397448);
#30308=CONICAL_SURFACE('',#33542,2.165,0.785398163397448);
#30309=CONICAL_SURFACE('',#33548,2.165,0.785398163397448);
#30310=CONICAL_SURFACE('',#33619,1.2885,0.785398163397447);
#30311=CONICAL_SURFACE('',#33704,2.6,0.785398163397448);
#30312=CONICAL_SURFACE('',#33812,1.49337567297406,0.785398163397454);
#30313=CONICAL_SURFACE('',#33852,0.721687836487032,1.02974425867665);
#30314=CONICAL_SURFACE('',#33912,1.2885,0.78539816339745);
#30315=CONICAL_SURFACE('',#33997,2.6,0.785398163397448);
#30316=CONICAL_SURFACE('',#34105,1.49337567297406,0.785398163397449);
#30317=CONICAL_SURFACE('',#34145,0.721687836487032,1.02974425867665);
#30318=CONICAL_SURFACE('',#34198,1.7,0.785398163397451);
#30319=CONICAL_SURFACE('',#34201,0.825,0.785398163397448);
#30320=CONICAL_SURFACE('',#34202,1.7,0.785398163397451);
#30321=ADVANCED_FACE('',(#3346),#30250,.F.);
#30322=ADVANCED_FACE('',(#3347,#2016,#2017),#2232,.T.);
#30323=ADVANCED_FACE('',(#3348),#1765,.F.);
#30324=ADVANCED_FACE('',(#3349),#30251,.F.);
#30325=ADVANCED_FACE('',(#3350),#1766,.F.);
#30326=ADVANCED_FACE('',(#3351),#30252,.F.);
#30327=ADVANCED_FACE('',(#3352),#30253,.F.);
#30328=ADVANCED_FACE('',(#3353),#30254,.F.);
#30329=ADVANCED_FACE('',(#3354,#2018,#2019),#2233,.F.);
#30330=ADVANCED_FACE('',(#3355),#1767,.F.);
#30331=ADVANCED_FACE('',(#3356),#30255,.F.);
#30332=ADVANCED_FACE('',(#3357),#1768,.F.);
#30333=ADVANCED_FACE('',(#3358),#30256,.F.);
#30334=ADVANCED_FACE('',(#3359),#30257,.F.);
#30335=ADVANCED_FACE('',(#3360),#2234,.T.);
#30336=ADVANCED_FACE('',(#3361),#2235,.T.);
#30337=ADVANCED_FACE('',(#3362),#2236,.T.);
#30338=ADVANCED_FACE('',(#3363),#2237,.T.);
#30339=ADVANCED_FACE('',(#3364),#2238,.T.);
#30340=ADVANCED_FACE('',(#3365),#2239,.T.);
#30341=ADVANCED_FACE('',(#3366),#2240,.T.);
#30342=ADVANCED_FACE('',(#3367),#2241,.T.);
#30343=ADVANCED_FACE('',(#3368),#2242,.T.);
#30344=ADVANCED_FACE('',(#3369),#2243,.T.);
#30345=ADVANCED_FACE('',(#3370),#2244,.T.);
#30346=ADVANCED_FACE('',(#3371),#2245,.T.);
#30347=ADVANCED_FACE('',(#3372),#2246,.T.);
#30348=ADVANCED_FACE('',(#3373),#2247,.T.);
#30349=ADVANCED_FACE('',(#3374),#2248,.T.);
#30350=ADVANCED_FACE('',(#3375),#2249,.T.);
#30351=ADVANCED_FACE('',(#3376),#30258,.F.);
#30352=ADVANCED_FACE('',(#3377,#2020,#2021),#2250,.T.);
#30353=ADVANCED_FACE('',(#3378),#1769,.F.);
#30354=ADVANCED_FACE('',(#3379),#30259,.F.);
#30355=ADVANCED_FACE('',(#3380),#1770,.F.);
#30356=ADVANCED_FACE('',(#3381),#30260,.F.);
#30357=ADVANCED_FACE('',(#3382),#30261,.F.);
#30358=ADVANCED_FACE('',(#3383),#30262,.F.);
#30359=ADVANCED_FACE('',(#3384,#2022,#2023,#2024,#2025,#2026,#2027,#2028,
#2029,#2030,#2031),#2251,.T.);
#30360=ADVANCED_FACE('',(#3385),#1771,.F.);
#30361=ADVANCED_FACE('',(#3386),#30263,.F.);
#30362=ADVANCED_FACE('',(#3387),#1772,.F.);
#30363=ADVANCED_FACE('',(#3388),#30264,.F.);
#30364=ADVANCED_FACE('',(#3389),#1773,.F.);
#30365=ADVANCED_FACE('',(#3390),#30265,.F.);
#30366=ADVANCED_FACE('',(#3391),#1774,.F.);
#30367=ADVANCED_FACE('',(#3392),#30266,.F.);
#30368=ADVANCED_FACE('',(#3393),#30267,.F.);
#30369=ADVANCED_FACE('',(#3394),#30268,.F.);
#30370=ADVANCED_FACE('',(#3395),#30269,.F.);
#30371=ADVANCED_FACE('',(#3396),#30270,.F.);
#30372=ADVANCED_FACE('',(#3397),#1775,.F.);
#30373=ADVANCED_FACE('',(#3398),#30271,.F.);
#30374=ADVANCED_FACE('',(#3399),#1776,.F.);
#30375=ADVANCED_FACE('',(#3400),#30272,.F.);
#30376=ADVANCED_FACE('',(#3401),#1777,.F.);
#30377=ADVANCED_FACE('',(#3402),#30273,.F.);
#30378=ADVANCED_FACE('',(#3403),#1778,.F.);
#30379=ADVANCED_FACE('',(#3404),#30274,.F.);
#30380=ADVANCED_FACE('',(#3405),#1779,.F.);
#30381=ADVANCED_FACE('',(#3406),#30275,.F.);
#30382=ADVANCED_FACE('',(#3407),#1780,.F.);
#30383=ADVANCED_FACE('',(#3408),#30276,.F.);
#30384=ADVANCED_FACE('',(#3409),#30277,.F.);
#30385=ADVANCED_FACE('',(#3410),#30278,.F.);
#30386=ADVANCED_FACE('',(#3411),#30279,.F.);
#30387=ADVANCED_FACE('',(#3412),#30280,.F.);
#30388=ADVANCED_FACE('',(#3413),#30281,.F.);
#30389=ADVANCED_FACE('',(#3414),#1781,.F.);
#30390=ADVANCED_FACE('',(#3415),#2252,.T.);
#30391=ADVANCED_FACE('',(#3416),#2253,.T.);
#30392=ADVANCED_FACE('',(#3417),#1782,.F.);
#30393=ADVANCED_FACE('',(#3418),#2254,.T.);
#30394=ADVANCED_FACE('',(#3419),#2255,.F.);
#30395=ADVANCED_FACE('',(#3420),#1783,.F.);
#30396=ADVANCED_FACE('',(#3421),#2256,.T.);
#30397=ADVANCED_FACE('',(#3422),#2257,.T.);
#30398=ADVANCED_FACE('',(#3423),#2258,.T.);
#30399=ADVANCED_FACE('',(#3424),#2259,.T.);
#30400=ADVANCED_FACE('',(#3425),#2260,.F.);
#30401=ADVANCED_FACE('',(#3426),#2261,.T.);
#30402=ADVANCED_FACE('',(#3427),#2262,.T.);
#30403=ADVANCED_FACE('',(#3428),#2263,.T.);
#30404=ADVANCED_FACE('',(#3429),#2264,.T.);
#30405=ADVANCED_FACE('',(#3430),#2265,.T.);
#30406=ADVANCED_FACE('',(#3431),#2266,.T.);
#30407=ADVANCED_FACE('',(#3432),#2267,.F.);
#30408=ADVANCED_FACE('',(#3433),#2268,.T.);
#30409=ADVANCED_FACE('',(#3434),#2269,.T.);
#30410=ADVANCED_FACE('',(#3435),#30282,.F.);
#30411=ADVANCED_FACE('',(#3436),#1784,.F.);
#30412=ADVANCED_FACE('',(#3437,#2032),#2270,.T.);
#30413=ADVANCED_FACE('',(#3438),#30283,.F.);
#30414=ADVANCED_FACE('',(#3439,#2033),#2271,.T.);
#30415=ADVANCED_FACE('',(#3440),#30284,.T.);
#30416=ADVANCED_FACE('',(#3441),#1785,.T.);
#30417=ADVANCED_FACE('',(#3442),#30285,.T.);
#30418=ADVANCED_FACE('',(#3443),#1786,.T.);
#30419=ADVANCED_FACE('',(#3444),#1787,.T.);
#30420=ADVANCED_FACE('',(#3445),#1788,.T.);
#30421=ADVANCED_FACE('',(#3446),#1789,.T.);
#30422=ADVANCED_FACE('',(#3447),#1790,.T.);
#30423=ADVANCED_FACE('',(#3448),#1791,.T.);
#30424=ADVANCED_FACE('',(#3449),#1792,.T.);
#30425=ADVANCED_FACE('',(#3450),#1793,.T.);
#30426=ADVANCED_FACE('',(#3451),#1794,.T.);
#30427=ADVANCED_FACE('',(#3452),#1795,.T.);
#30428=ADVANCED_FACE('',(#3453),#1796,.T.);
#30429=ADVANCED_FACE('',(#3454),#1797,.T.);
#30430=ADVANCED_FACE('',(#3455),#1798,.T.);
#30431=ADVANCED_FACE('',(#3456),#1799,.T.);
#30432=ADVANCED_FACE('',(#3457),#1800,.T.);
#30433=ADVANCED_FACE('',(#3458),#1801,.T.);
#30434=ADVANCED_FACE('',(#3459),#1802,.T.);
#30435=ADVANCED_FACE('',(#3460),#1803,.T.);
#30436=ADVANCED_FACE('',(#3461),#1804,.T.);
#30437=ADVANCED_FACE('',(#3462),#1805,.T.);
#30438=ADVANCED_FACE('',(#3463),#1806,.T.);
#30439=ADVANCED_FACE('',(#3464),#1807,.T.);
#30440=ADVANCED_FACE('',(#3465),#1808,.T.);
#30441=ADVANCED_FACE('',(#3466),#1809,.T.);
#30442=ADVANCED_FACE('',(#3467),#1810,.T.);
#30443=ADVANCED_FACE('',(#3468),#1811,.T.);
#30444=ADVANCED_FACE('',(#3469),#1812,.T.);
#30445=ADVANCED_FACE('',(#3470),#1813,.T.);
#30446=ADVANCED_FACE('',(#3471),#1814,.T.);
#30447=ADVANCED_FACE('',(#3472),#1815,.T.);
#30448=ADVANCED_FACE('',(#3473),#1816,.T.);
#30449=ADVANCED_FACE('',(#3474),#1817,.T.);
#30450=ADVANCED_FACE('',(#3475),#1818,.T.);
#30451=ADVANCED_FACE('',(#3476),#1819,.T.);
#30452=ADVANCED_FACE('',(#3477),#1820,.T.);
#30453=ADVANCED_FACE('',(#3478),#1821,.T.);
#30454=ADVANCED_FACE('',(#3479),#1822,.T.);
#30455=ADVANCED_FACE('',(#3480),#1823,.T.);
#30456=ADVANCED_FACE('',(#3481),#1824,.T.);
#30457=ADVANCED_FACE('',(#3482),#1825,.T.);
#30458=ADVANCED_FACE('',(#3483),#1826,.T.);
#30459=ADVANCED_FACE('',(#3484),#1827,.T.);
#30460=ADVANCED_FACE('',(#3485),#1828,.T.);
#30461=ADVANCED_FACE('',(#3486),#1829,.T.);
#30462=ADVANCED_FACE('',(#3487),#1830,.T.);
#30463=ADVANCED_FACE('',(#3488),#1831,.T.);
#30464=ADVANCED_FACE('',(#3489),#1832,.T.);
#30465=ADVANCED_FACE('',(#3490),#1833,.T.);
#30466=ADVANCED_FACE('',(#3491),#2272,.F.);
#30467=ADVANCED_FACE('',(#3492),#2273,.F.);
#30468=ADVANCED_FACE('',(#3493),#2274,.T.);
#30469=ADVANCED_FACE('',(#3494),#2275,.F.);
#30470=ADVANCED_FACE('',(#3495),#304,.F.);
#30471=ADVANCED_FACE('',(#3496),#305,.F.);
#30472=ADVANCED_FACE('',(#3497),#306,.F.);
#30473=ADVANCED_FACE('',(#3498),#307,.F.);
#30474=ADVANCED_FACE('',(#3499),#308,.F.);
#30475=ADVANCED_FACE('',(#3500),#309,.F.);
#30476=ADVANCED_FACE('',(#3501),#310,.F.);
#30477=ADVANCED_FACE('',(#3502),#311,.F.);
#30478=ADVANCED_FACE('',(#3503),#312,.F.);
#30479=ADVANCED_FACE('',(#3504),#313,.F.);
#30480=ADVANCED_FACE('',(#3505),#314,.F.);
#30481=ADVANCED_FACE('',(#3506),#315,.F.);
#30482=ADVANCED_FACE('',(#3507),#316,.F.);
#30483=ADVANCED_FACE('',(#3508),#317,.F.);
#30484=ADVANCED_FACE('',(#3509),#318,.F.);
#30485=ADVANCED_FACE('',(#3510),#319,.F.);
#30486=ADVANCED_FACE('',(#3511),#320,.F.);
#30487=ADVANCED_FACE('',(#3512),#321,.F.);
#30488=ADVANCED_FACE('',(#3513),#322,.F.);
#30489=ADVANCED_FACE('',(#3514),#323,.F.);
#30490=ADVANCED_FACE('',(#3515),#324,.F.);
#30491=ADVANCED_FACE('',(#3516),#325,.F.);
#30492=ADVANCED_FACE('',(#3517),#326,.F.);
#30493=ADVANCED_FACE('',(#3518),#327,.F.);
#30494=ADVANCED_FACE('',(#3519),#328,.F.);
#30495=ADVANCED_FACE('',(#3520),#329,.F.);
#30496=ADVANCED_FACE('',(#3521),#330,.F.);
#30497=ADVANCED_FACE('',(#3522),#2276,.T.);
#30498=ADVANCED_FACE('',(#3523),#2277,.T.);
#30499=ADVANCED_FACE('',(#3524),#30286,.T.);
#30500=ADVANCED_FACE('',(#3525,#2034),#1834,.T.);
#30501=ADVANCED_FACE('',(#3526,#2035),#2278,.T.);
#30502=ADVANCED_FACE('',(#3527),#30287,.T.);
#30503=ADVANCED_FACE('',(#3528,#2036),#2279,.T.);
#30504=ADVANCED_FACE('',(#3529),#1835,.T.);
#30505=ADVANCED_FACE('',(#3530),#30288,.T.);
#30506=ADVANCED_FACE('',(#3531),#2280,.T.);
#30507=ADVANCED_FACE('',(#3532),#1836,.F.);
#30508=ADVANCED_FACE('',(#3533),#2281,.F.);
#30509=ADVANCED_FACE('',(#3534),#2282,.F.);
#30510=ADVANCED_FACE('',(#3535),#2283,.F.);
#30511=ADVANCED_FACE('',(#3536),#2284,.F.);
#30512=ADVANCED_FACE('',(#3537),#2285,.F.);
#30513=ADVANCED_FACE('',(#3538),#2286,.F.);
#30514=ADVANCED_FACE('',(#3539),#2287,.F.);
#30515=ADVANCED_FACE('',(#3540),#2288,.F.);
#30516=ADVANCED_FACE('',(#3541),#2289,.F.);
#30517=ADVANCED_FACE('',(#3542),#2290,.F.);
#30518=ADVANCED_FACE('',(#3543),#2291,.T.);
#30519=ADVANCED_FACE('',(#3544),#2292,.F.);
#30520=ADVANCED_FACE('',(#3545),#2293,.F.);
#30521=ADVANCED_FACE('',(#3546),#2294,.T.);
#30522=ADVANCED_FACE('',(#3547),#2295,.F.);
#30523=ADVANCED_FACE('',(#3548),#2296,.F.);
#30524=ADVANCED_FACE('',(#3549),#2297,.F.);
#30525=ADVANCED_FACE('',(#3550),#2298,.T.);
#30526=ADVANCED_FACE('',(#3551),#2299,.F.);
#30527=ADVANCED_FACE('',(#3552),#2300,.F.);
#30528=ADVANCED_FACE('',(#3553),#2301,.F.);
#30529=ADVANCED_FACE('',(#3554),#2302,.T.);
#30530=ADVANCED_FACE('',(#3555),#2303,.F.);
#30531=ADVANCED_FACE('',(#3556),#2304,.F.);
#30532=ADVANCED_FACE('',(#3557),#2305,.F.);
#30533=ADVANCED_FACE('',(#3558),#2306,.T.);
#30534=ADVANCED_FACE('',(#3559),#2307,.F.);
#30535=ADVANCED_FACE('',(#3560),#2308,.F.);
#30536=ADVANCED_FACE('',(#3561),#2309,.F.);
#30537=ADVANCED_FACE('',(#3562),#2310,.T.);
#30538=ADVANCED_FACE('',(#3563),#2311,.F.);
#30539=ADVANCED_FACE('',(#3564),#2312,.F.);
#30540=ADVANCED_FACE('',(#3565),#2313,.F.);
#30541=ADVANCED_FACE('',(#3566),#2314,.T.);
#30542=ADVANCED_FACE('',(#3567),#2315,.F.);
#30543=ADVANCED_FACE('',(#3568),#2316,.F.);
#30544=ADVANCED_FACE('',(#3569),#2317,.F.);
#30545=ADVANCED_FACE('',(#3570),#2318,.T.);
#30546=ADVANCED_FACE('',(#3571),#2319,.F.);
#30547=ADVANCED_FACE('',(#3572),#2320,.F.);
#30548=ADVANCED_FACE('',(#3573),#2321,.F.);
#30549=ADVANCED_FACE('',(#3574),#2322,.T.);
#30550=ADVANCED_FACE('',(#3575),#2323,.F.);
#30551=ADVANCED_FACE('',(#3576),#2324,.F.);
#30552=ADVANCED_FACE('',(#3577),#2325,.F.);
#30553=ADVANCED_FACE('',(#3578),#2326,.T.);
#30554=ADVANCED_FACE('',(#3579),#2327,.F.);
#30555=ADVANCED_FACE('',(#3580),#2328,.F.);
#30556=ADVANCED_FACE('',(#3581),#2329,.F.);
#30557=ADVANCED_FACE('',(#3582),#2330,.T.);
#30558=ADVANCED_FACE('',(#3583),#2331,.F.);
#30559=ADVANCED_FACE('',(#3584),#2332,.F.);
#30560=ADVANCED_FACE('',(#3585),#2333,.F.);
#30561=ADVANCED_FACE('',(#3586),#2334,.T.);
#30562=ADVANCED_FACE('',(#3587),#2335,.F.);
#30563=ADVANCED_FACE('',(#3588),#2336,.F.);
#30564=ADVANCED_FACE('',(#3589),#2337,.F.);
#30565=ADVANCED_FACE('',(#3590),#2338,.T.);
#30566=ADVANCED_FACE('',(#3591),#2339,.F.);
#30567=ADVANCED_FACE('',(#3592),#2340,.F.);
#30568=ADVANCED_FACE('',(#3593),#2341,.F.);
#30569=ADVANCED_FACE('',(#3594),#2342,.T.);
#30570=ADVANCED_FACE('',(#3595),#2343,.F.);
#30571=ADVANCED_FACE('',(#3596),#2344,.F.);
#30572=ADVANCED_FACE('',(#3597),#2345,.F.);
#30573=ADVANCED_FACE('',(#3598),#2346,.T.);
#30574=ADVANCED_FACE('',(#3599),#2347,.F.);
#30575=ADVANCED_FACE('',(#3600),#2348,.F.);
#30576=ADVANCED_FACE('',(#3601),#2349,.F.);
#30577=ADVANCED_FACE('',(#3602),#2350,.T.);
#30578=ADVANCED_FACE('',(#3603),#2351,.F.);
#30579=ADVANCED_FACE('',(#3604),#2352,.F.);
#30580=ADVANCED_FACE('',(#3605),#2353,.F.);
#30581=ADVANCED_FACE('',(#3606),#2354,.T.);
#30582=ADVANCED_FACE('',(#3607),#2355,.F.);
#30583=ADVANCED_FACE('',(#3608),#2356,.F.);
#30584=ADVANCED_FACE('',(#3609),#2357,.F.);
#30585=ADVANCED_FACE('',(#3610),#2358,.T.);
#30586=ADVANCED_FACE('',(#3611),#2359,.F.);
#30587=ADVANCED_FACE('',(#3612),#2360,.F.);
#30588=ADVANCED_FACE('',(#3613),#2361,.F.);
#30589=ADVANCED_FACE('',(#3614),#2362,.T.);
#30590=ADVANCED_FACE('',(#3615),#2363,.F.);
#30591=ADVANCED_FACE('',(#3616),#2364,.F.);
#30592=ADVANCED_FACE('',(#3617),#2365,.F.);
#30593=ADVANCED_FACE('',(#3618),#2366,.T.);
#30594=ADVANCED_FACE('',(#3619),#2367,.F.);
#30595=ADVANCED_FACE('',(#3620),#2368,.F.);
#30596=ADVANCED_FACE('',(#3621),#2369,.F.);
#30597=ADVANCED_FACE('',(#3622),#2370,.T.);
#30598=ADVANCED_FACE('',(#3623),#2371,.F.);
#30599=ADVANCED_FACE('',(#3624),#2372,.F.);
#30600=ADVANCED_FACE('',(#3625),#2373,.F.);
#30601=ADVANCED_FACE('',(#3626),#2374,.T.);
#30602=ADVANCED_FACE('',(#3627),#2375,.F.);
#30603=ADVANCED_FACE('',(#3628),#2376,.F.);
#30604=ADVANCED_FACE('',(#3629),#2377,.F.);
#30605=ADVANCED_FACE('',(#3630),#2378,.T.);
#30606=ADVANCED_FACE('',(#3631),#2379,.F.);
#30607=ADVANCED_FACE('',(#3632),#2380,.F.);
#30608=ADVANCED_FACE('',(#3633),#2381,.F.);
#30609=ADVANCED_FACE('',(#3634),#2382,.T.);
#30610=ADVANCED_FACE('',(#3635),#2383,.F.);
#30611=ADVANCED_FACE('',(#3636),#2384,.F.);
#30612=ADVANCED_FACE('',(#3637),#2385,.F.);
#30613=ADVANCED_FACE('',(#3638),#2386,.T.);
#30614=ADVANCED_FACE('',(#3639),#2387,.F.);
#30615=ADVANCED_FACE('',(#3640),#2388,.F.);
#30616=ADVANCED_FACE('',(#3641),#2389,.F.);
#30617=ADVANCED_FACE('',(#3642),#2390,.T.);
#30618=ADVANCED_FACE('',(#3643),#2391,.F.);
#30619=ADVANCED_FACE('',(#3644),#2392,.F.);
#30620=ADVANCED_FACE('',(#3645),#2393,.F.);
#30621=ADVANCED_FACE('',(#3646),#2394,.T.);
#30622=ADVANCED_FACE('',(#3647),#2395,.F.);
#30623=ADVANCED_FACE('',(#3648),#2396,.F.);
#30624=ADVANCED_FACE('',(#3649),#2397,.F.);
#30625=ADVANCED_FACE('',(#3650),#2398,.T.);
#30626=ADVANCED_FACE('',(#3651),#2399,.F.);
#30627=ADVANCED_FACE('',(#3652),#2400,.F.);
#30628=ADVANCED_FACE('',(#3653),#2401,.F.);
#30629=ADVANCED_FACE('',(#3654),#2402,.T.);
#30630=ADVANCED_FACE('',(#3655),#2403,.F.);
#30631=ADVANCED_FACE('',(#3656),#2404,.F.);
#30632=ADVANCED_FACE('',(#3657),#2405,.F.);
#30633=ADVANCED_FACE('',(#3658),#2406,.T.);
#30634=ADVANCED_FACE('',(#3659),#2407,.F.);
#30635=ADVANCED_FACE('',(#3660),#2408,.F.);
#30636=ADVANCED_FACE('',(#3661),#2409,.F.);
#30637=ADVANCED_FACE('',(#3662),#2410,.T.);
#30638=ADVANCED_FACE('',(#3663),#2411,.F.);
#30639=ADVANCED_FACE('',(#3664),#2412,.F.);
#30640=ADVANCED_FACE('',(#3665),#2413,.F.);
#30641=ADVANCED_FACE('',(#3666),#2414,.T.);
#30642=ADVANCED_FACE('',(#3667),#2415,.F.);
#30643=ADVANCED_FACE('',(#3668),#2416,.F.);
#30644=ADVANCED_FACE('',(#3669),#2417,.F.);
#30645=ADVANCED_FACE('',(#3670),#2418,.T.);
#30646=ADVANCED_FACE('',(#3671),#2419,.F.);
#30647=ADVANCED_FACE('',(#3672),#2420,.F.);
#30648=ADVANCED_FACE('',(#3673),#2421,.F.);
#30649=ADVANCED_FACE('',(#3674),#2422,.T.);
#30650=ADVANCED_FACE('',(#3675),#2423,.F.);
#30651=ADVANCED_FACE('',(#3676),#2424,.F.);
#30652=ADVANCED_FACE('',(#3677),#2425,.F.);
#30653=ADVANCED_FACE('',(#3678),#2426,.T.);
#30654=ADVANCED_FACE('',(#3679),#2427,.F.);
#30655=ADVANCED_FACE('',(#3680),#2428,.F.);
#30656=ADVANCED_FACE('',(#3681),#2429,.F.);
#30657=ADVANCED_FACE('',(#3682),#2430,.T.);
#30658=ADVANCED_FACE('',(#3683),#2431,.F.);
#30659=ADVANCED_FACE('',(#3684),#2432,.F.);
#30660=ADVANCED_FACE('',(#3685),#2433,.F.);
#30661=ADVANCED_FACE('',(#3686),#2434,.T.);
#30662=ADVANCED_FACE('',(#3687),#2435,.F.);
#30663=ADVANCED_FACE('',(#3688),#2436,.F.);
#30664=ADVANCED_FACE('',(#3689),#2437,.F.);
#30665=ADVANCED_FACE('',(#3690),#2438,.T.);
#30666=ADVANCED_FACE('',(#3691),#2439,.F.);
#30667=ADVANCED_FACE('',(#3692),#2440,.F.);
#30668=ADVANCED_FACE('',(#3693),#2441,.F.);
#30669=ADVANCED_FACE('',(#3694),#2442,.T.);
#30670=ADVANCED_FACE('',(#3695),#2443,.F.);
#30671=ADVANCED_FACE('',(#3696),#2444,.F.);
#30672=ADVANCED_FACE('',(#3697),#2445,.T.);
#30673=ADVANCED_FACE('',(#3698),#2446,.F.);
#30674=ADVANCED_FACE('',(#3699),#30289,.F.);
#30675=ADVANCED_FACE('',(#3700,#2037),#2447,.T.);
#30676=ADVANCED_FACE('',(#3701),#30290,.T.);
#30677=ADVANCED_FACE('',(#3702,#2038,#2039,#2040,#2041,#2042,#2043,#2044,
#2045,#2046,#2047,#2048,#2049,#2050,#2051,#2052,#2053,#2054,#2055,#2056,
#2057,#2058,#2059,#2060,#2061,#2062,#2063,#2064,#2065,#2066,#2067,#2068,
#2069,#2070,#2071,#2072,#2073,#2074),#1837,.T.);
#30678=ADVANCED_FACE('',(#3703),#30291,.T.);
#30679=ADVANCED_FACE('',(#3704,#2075),#2448,.T.);
#30680=ADVANCED_FACE('',(#3705),#1838,.T.);
#30681=ADVANCED_FACE('',(#3706,#2076),#2449,.T.);
#30682=ADVANCED_FACE('',(#3707,#2077),#1839,.F.);
#30683=ADVANCED_FACE('',(#3708),#331,.F.);
#30684=ADVANCED_FACE('',(#3709),#332,.F.);
#30685=ADVANCED_FACE('',(#3710),#333,.F.);
#30686=ADVANCED_FACE('',(#3711),#334,.F.);
#30687=ADVANCED_FACE('',(#3712),#335,.F.);
#30688=ADVANCED_FACE('',(#3713),#336,.F.);
#30689=ADVANCED_FACE('',(#3714),#337,.F.);
#30690=ADVANCED_FACE('',(#3715),#338,.F.);
#30691=ADVANCED_FACE('',(#3716),#339,.F.);
#30692=ADVANCED_FACE('',(#3717),#340,.F.);
#30693=ADVANCED_FACE('',(#3718),#341,.F.);
#30694=ADVANCED_FACE('',(#3719),#342,.F.);
#30695=ADVANCED_FACE('',(#3720),#343,.F.);
#30696=ADVANCED_FACE('',(#3721),#344,.F.);
#30697=ADVANCED_FACE('',(#3722),#345,.F.);
#30698=ADVANCED_FACE('',(#3723),#346,.F.);
#30699=ADVANCED_FACE('',(#3724),#347,.F.);
#30700=ADVANCED_FACE('',(#3725),#348,.F.);
#30701=ADVANCED_FACE('',(#3726),#349,.F.);
#30702=ADVANCED_FACE('',(#3727),#350,.F.);
#30703=ADVANCED_FACE('',(#3728,#2078),#2450,.T.);
#30704=ADVANCED_FACE('',(#3729),#2451,.F.);
#30705=ADVANCED_FACE('',(#3730),#2452,.F.);
#30706=ADVANCED_FACE('',(#3731),#2453,.F.);
#30707=ADVANCED_FACE('',(#3732),#2454,.F.);
#30708=ADVANCED_FACE('',(#3733),#2455,.F.);
#30709=ADVANCED_FACE('',(#3734),#2456,.F.);
#30710=ADVANCED_FACE('',(#3735),#2457,.F.);
#30711=ADVANCED_FACE('',(#3736),#2458,.F.);
#30712=ADVANCED_FACE('',(#3737),#2459,.F.);
#30713=ADVANCED_FACE('',(#3738),#2460,.F.);
#30714=ADVANCED_FACE('',(#3739),#2461,.F.);
#30715=ADVANCED_FACE('',(#3740),#2462,.F.);
#30716=ADVANCED_FACE('',(#3741),#2463,.F.);
#30717=ADVANCED_FACE('',(#3742),#2464,.F.);
#30718=ADVANCED_FACE('',(#3743,#2079),#2465,.F.);
#30719=ADVANCED_FACE('',(#3744),#2466,.T.);
#30720=ADVANCED_FACE('',(#3745),#2467,.T.);
#30721=ADVANCED_FACE('',(#3746),#351,.F.);
#30722=ADVANCED_FACE('',(#3747),#352,.F.);
#30723=ADVANCED_FACE('',(#3748),#353,.F.);
#30724=ADVANCED_FACE('',(#3749),#354,.F.);
#30725=ADVANCED_FACE('',(#3750),#355,.F.);
#30726=ADVANCED_FACE('',(#3751),#356,.F.);
#30727=ADVANCED_FACE('',(#3752),#357,.F.);
#30728=ADVANCED_FACE('',(#3753),#358,.F.);
#30729=ADVANCED_FACE('',(#3754),#359,.F.);
#30730=ADVANCED_FACE('',(#3755),#360,.F.);
#30731=ADVANCED_FACE('',(#3756),#361,.F.);
#30732=ADVANCED_FACE('',(#3757),#362,.F.);
#30733=ADVANCED_FACE('',(#3758),#363,.F.);
#30734=ADVANCED_FACE('',(#3759),#364,.F.);
#30735=ADVANCED_FACE('',(#3760),#365,.F.);
#30736=ADVANCED_FACE('',(#3761),#366,.F.);
#30737=ADVANCED_FACE('',(#3762),#367,.F.);
#30738=ADVANCED_FACE('',(#3763),#368,.F.);
#30739=ADVANCED_FACE('',(#3764),#369,.F.);
#30740=ADVANCED_FACE('',(#3765),#370,.F.);
#30741=ADVANCED_FACE('',(#3766,#2080),#2468,.T.);
#30742=ADVANCED_FACE('',(#3767),#371,.F.);
#30743=ADVANCED_FACE('',(#3768),#372,.F.);
#30744=ADVANCED_FACE('',(#3769),#373,.F.);
#30745=ADVANCED_FACE('',(#3770),#374,.F.);
#30746=ADVANCED_FACE('',(#3771),#375,.F.);
#30747=ADVANCED_FACE('',(#3772),#376,.F.);
#30748=ADVANCED_FACE('',(#3773),#377,.F.);
#30749=ADVANCED_FACE('',(#3774),#378,.F.);
#30750=ADVANCED_FACE('',(#3775),#379,.F.);
#30751=ADVANCED_FACE('',(#3776),#380,.F.);
#30752=ADVANCED_FACE('',(#3777),#381,.F.);
#30753=ADVANCED_FACE('',(#3778),#382,.F.);
#30754=ADVANCED_FACE('',(#3779),#2469,.F.);
#30755=ADVANCED_FACE('',(#3780),#383,.F.);
#30756=ADVANCED_FACE('',(#3781),#384,.F.);
#30757=ADVANCED_FACE('',(#3782),#385,.F.);
#30758=ADVANCED_FACE('',(#3783),#386,.F.);
#30759=ADVANCED_FACE('',(#3784),#387,.F.);
#30760=ADVANCED_FACE('',(#3785),#388,.F.);
#30761=ADVANCED_FACE('',(#3786),#389,.F.);
#30762=ADVANCED_FACE('',(#3787),#2470,.F.);
#30763=ADVANCED_FACE('',(#3788),#390,.F.);
#30764=ADVANCED_FACE('',(#3789),#391,.F.);
#30765=ADVANCED_FACE('',(#3790),#392,.F.);
#30766=ADVANCED_FACE('',(#3791),#393,.F.);
#30767=ADVANCED_FACE('',(#3792),#394,.F.);
#30768=ADVANCED_FACE('',(#3793),#395,.F.);
#30769=ADVANCED_FACE('',(#3794),#396,.F.);
#30770=ADVANCED_FACE('',(#3795),#2471,.F.);
#30771=ADVANCED_FACE('',(#3796),#397,.F.);
#30772=ADVANCED_FACE('',(#3797),#2472,.T.);
#30773=ADVANCED_FACE('',(#3798),#2473,.T.);
#30774=ADVANCED_FACE('',(#3799),#398,.F.);
#30775=ADVANCED_FACE('',(#3800),#399,.F.);
#30776=ADVANCED_FACE('',(#3801),#400,.F.);
#30777=ADVANCED_FACE('',(#3802),#401,.F.);
#30778=ADVANCED_FACE('',(#3803),#402,.F.);
#30779=ADVANCED_FACE('',(#3804),#403,.F.);
#30780=ADVANCED_FACE('',(#3805),#404,.F.);
#30781=ADVANCED_FACE('',(#3806),#405,.F.);
#30782=ADVANCED_FACE('',(#3807),#406,.F.);
#30783=ADVANCED_FACE('',(#3808),#407,.F.);
#30784=ADVANCED_FACE('',(#3809),#408,.F.);
#30785=ADVANCED_FACE('',(#3810),#409,.F.);
#30786=ADVANCED_FACE('',(#3811),#410,.F.);
#30787=ADVANCED_FACE('',(#3812),#411,.F.);
#30788=ADVANCED_FACE('',(#3813),#412,.F.);
#30789=ADVANCED_FACE('',(#3814),#413,.F.);
#30790=ADVANCED_FACE('',(#3815),#414,.F.);
#30791=ADVANCED_FACE('',(#3816),#415,.F.);
#30792=ADVANCED_FACE('',(#3817),#416,.F.);
#30793=ADVANCED_FACE('',(#3818),#417,.F.);
#30794=ADVANCED_FACE('',(#3819,#2081),#2474,.T.);
#30795=ADVANCED_FACE('',(#3820),#418,.F.);
#30796=ADVANCED_FACE('',(#3821),#419,.F.);
#30797=ADVANCED_FACE('',(#3822),#420,.F.);
#30798=ADVANCED_FACE('',(#3823),#421,.F.);
#30799=ADVANCED_FACE('',(#3824),#422,.F.);
#30800=ADVANCED_FACE('',(#3825),#423,.F.);
#30801=ADVANCED_FACE('',(#3826),#424,.F.);
#30802=ADVANCED_FACE('',(#3827),#425,.F.);
#30803=ADVANCED_FACE('',(#3828),#426,.F.);
#30804=ADVANCED_FACE('',(#3829),#2475,.F.);
#30805=ADVANCED_FACE('',(#3830),#427,.F.);
#30806=ADVANCED_FACE('',(#3831),#428,.F.);
#30807=ADVANCED_FACE('',(#3832),#429,.F.);
#30808=ADVANCED_FACE('',(#3833),#430,.F.);
#30809=ADVANCED_FACE('',(#3834),#431,.F.);
#30810=ADVANCED_FACE('',(#3835),#432,.F.);
#30811=ADVANCED_FACE('',(#3836),#433,.F.);
#30812=ADVANCED_FACE('',(#3837),#434,.F.);
#30813=ADVANCED_FACE('',(#3838),#435,.F.);
#30814=ADVANCED_FACE('',(#3839),#2476,.F.);
#30815=ADVANCED_FACE('',(#3840),#2477,.F.);
#30816=ADVANCED_FACE('',(#3841),#2478,.F.);
#30817=ADVANCED_FACE('',(#3842),#2479,.T.);
#30818=ADVANCED_FACE('',(#3843),#2480,.T.);
#30819=ADVANCED_FACE('',(#3844),#436,.F.);
#30820=ADVANCED_FACE('',(#3845),#437,.F.);
#30821=ADVANCED_FACE('',(#3846),#438,.F.);
#30822=ADVANCED_FACE('',(#3847),#439,.F.);
#30823=ADVANCED_FACE('',(#3848),#440,.F.);
#30824=ADVANCED_FACE('',(#3849),#441,.F.);
#30825=ADVANCED_FACE('',(#3850),#442,.F.);
#30826=ADVANCED_FACE('',(#3851),#443,.F.);
#30827=ADVANCED_FACE('',(#3852),#444,.F.);
#30828=ADVANCED_FACE('',(#3853),#445,.F.);
#30829=ADVANCED_FACE('',(#3854),#446,.F.);
#30830=ADVANCED_FACE('',(#3855),#447,.F.);
#30831=ADVANCED_FACE('',(#3856),#448,.F.);
#30832=ADVANCED_FACE('',(#3857),#449,.F.);
#30833=ADVANCED_FACE('',(#3858),#450,.F.);
#30834=ADVANCED_FACE('',(#3859),#451,.F.);
#30835=ADVANCED_FACE('',(#3860),#452,.F.);
#30836=ADVANCED_FACE('',(#3861),#453,.F.);
#30837=ADVANCED_FACE('',(#3862),#454,.F.);
#30838=ADVANCED_FACE('',(#3863),#455,.F.);
#30839=ADVANCED_FACE('',(#3864,#2082),#2481,.T.);
#30840=ADVANCED_FACE('',(#3865),#2482,.F.);
#30841=ADVANCED_FACE('',(#3866),#456,.F.);
#30842=ADVANCED_FACE('',(#3867),#457,.F.);
#30843=ADVANCED_FACE('',(#3868),#2483,.F.);
#30844=ADVANCED_FACE('',(#3869),#458,.F.);
#30845=ADVANCED_FACE('',(#3870),#459,.F.);
#30846=ADVANCED_FACE('',(#3871),#2484,.F.);
#30847=ADVANCED_FACE('',(#3872),#2485,.F.);
#30848=ADVANCED_FACE('',(#3873),#2486,.F.);
#30849=ADVANCED_FACE('',(#3874),#2487,.T.);
#30850=ADVANCED_FACE('',(#3875),#2488,.T.);
#30851=ADVANCED_FACE('',(#3876),#460,.F.);
#30852=ADVANCED_FACE('',(#3877),#461,.F.);
#30853=ADVANCED_FACE('',(#3878),#462,.F.);
#30854=ADVANCED_FACE('',(#3879),#463,.F.);
#30855=ADVANCED_FACE('',(#3880),#464,.F.);
#30856=ADVANCED_FACE('',(#3881),#465,.F.);
#30857=ADVANCED_FACE('',(#3882),#466,.F.);
#30858=ADVANCED_FACE('',(#3883),#467,.F.);
#30859=ADVANCED_FACE('',(#3884),#468,.F.);
#30860=ADVANCED_FACE('',(#3885),#469,.F.);
#30861=ADVANCED_FACE('',(#3886),#470,.F.);
#30862=ADVANCED_FACE('',(#3887),#471,.F.);
#30863=ADVANCED_FACE('',(#3888),#472,.F.);
#30864=ADVANCED_FACE('',(#3889),#473,.F.);
#30865=ADVANCED_FACE('',(#3890),#474,.F.);
#30866=ADVANCED_FACE('',(#3891),#475,.F.);
#30867=ADVANCED_FACE('',(#3892),#476,.F.);
#30868=ADVANCED_FACE('',(#3893),#477,.F.);
#30869=ADVANCED_FACE('',(#3894),#478,.F.);
#30870=ADVANCED_FACE('',(#3895),#479,.F.);
#30871=ADVANCED_FACE('',(#3896,#2083),#2489,.T.);
#30872=ADVANCED_FACE('',(#3897),#2490,.T.);
#30873=ADVANCED_FACE('',(#3898),#480,.F.);
#30874=ADVANCED_FACE('',(#3899),#481,.F.);
#30875=ADVANCED_FACE('',(#3900),#482,.F.);
#30876=ADVANCED_FACE('',(#3901),#483,.F.);
#30877=ADVANCED_FACE('',(#3902),#484,.F.);
#30878=ADVANCED_FACE('',(#3903),#485,.F.);
#30879=ADVANCED_FACE('',(#3904),#486,.F.);
#30880=ADVANCED_FACE('',(#3905),#487,.F.);
#30881=ADVANCED_FACE('',(#3906),#488,.F.);
#30882=ADVANCED_FACE('',(#3907),#489,.F.);
#30883=ADVANCED_FACE('',(#3908),#490,.F.);
#30884=ADVANCED_FACE('',(#3909),#491,.F.);
#30885=ADVANCED_FACE('',(#3910),#492,.F.);
#30886=ADVANCED_FACE('',(#3911),#493,.F.);
#30887=ADVANCED_FACE('',(#3912),#494,.F.);
#30888=ADVANCED_FACE('',(#3913),#495,.F.);
#30889=ADVANCED_FACE('',(#3914),#496,.F.);
#30890=ADVANCED_FACE('',(#3915),#497,.F.);
#30891=ADVANCED_FACE('',(#3916),#498,.F.);
#30892=ADVANCED_FACE('',(#3917),#499,.F.);
#30893=ADVANCED_FACE('',(#3918,#2084),#2491,.T.);
#30894=ADVANCED_FACE('',(#3919),#2492,.F.);
#30895=ADVANCED_FACE('',(#3920),#500,.F.);
#30896=ADVANCED_FACE('',(#3921),#501,.F.);
#30897=ADVANCED_FACE('',(#3922),#2493,.F.);
#30898=ADVANCED_FACE('',(#3923),#502,.F.);
#30899=ADVANCED_FACE('',(#3924),#503,.F.);
#30900=ADVANCED_FACE('',(#3925),#2494,.F.);
#30901=ADVANCED_FACE('',(#3926),#2495,.F.);
#30902=ADVANCED_FACE('',(#3927),#2496,.F.);
#30903=ADVANCED_FACE('',(#3928),#2497,.T.);
#30904=ADVANCED_FACE('',(#3929),#2498,.T.);
#30905=ADVANCED_FACE('',(#3930),#504,.F.);
#30906=ADVANCED_FACE('',(#3931),#505,.F.);
#30907=ADVANCED_FACE('',(#3932),#506,.F.);
#30908=ADVANCED_FACE('',(#3933),#507,.F.);
#30909=ADVANCED_FACE('',(#3934),#508,.F.);
#30910=ADVANCED_FACE('',(#3935),#509,.F.);
#30911=ADVANCED_FACE('',(#3936),#510,.F.);
#30912=ADVANCED_FACE('',(#3937),#511,.F.);
#30913=ADVANCED_FACE('',(#3938),#512,.F.);
#30914=ADVANCED_FACE('',(#3939),#513,.F.);
#30915=ADVANCED_FACE('',(#3940),#514,.F.);
#30916=ADVANCED_FACE('',(#3941),#515,.F.);
#30917=ADVANCED_FACE('',(#3942),#516,.F.);
#30918=ADVANCED_FACE('',(#3943),#517,.F.);
#30919=ADVANCED_FACE('',(#3944),#518,.F.);
#30920=ADVANCED_FACE('',(#3945),#519,.F.);
#30921=ADVANCED_FACE('',(#3946),#520,.F.);
#30922=ADVANCED_FACE('',(#3947),#521,.F.);
#30923=ADVANCED_FACE('',(#3948),#522,.F.);
#30924=ADVANCED_FACE('',(#3949),#523,.F.);
#30925=ADVANCED_FACE('',(#3950,#2085),#2499,.T.);
#30926=ADVANCED_FACE('',(#3951),#524,.F.);
#30927=ADVANCED_FACE('',(#3952),#525,.F.);
#30928=ADVANCED_FACE('',(#3953),#526,.F.);
#30929=ADVANCED_FACE('',(#3954),#527,.F.);
#30930=ADVANCED_FACE('',(#3955),#528,.F.);
#30931=ADVANCED_FACE('',(#3956),#529,.F.);
#30932=ADVANCED_FACE('',(#3957),#530,.F.);
#30933=ADVANCED_FACE('',(#3958),#531,.F.);
#30934=ADVANCED_FACE('',(#3959),#532,.F.);
#30935=ADVANCED_FACE('',(#3960),#2500,.F.);
#30936=ADVANCED_FACE('',(#3961),#533,.F.);
#30937=ADVANCED_FACE('',(#3962),#534,.F.);
#30938=ADVANCED_FACE('',(#3963),#535,.F.);
#30939=ADVANCED_FACE('',(#3964),#536,.F.);
#30940=ADVANCED_FACE('',(#3965),#537,.F.);
#30941=ADVANCED_FACE('',(#3966),#538,.F.);
#30942=ADVANCED_FACE('',(#3967),#539,.F.);
#30943=ADVANCED_FACE('',(#3968),#540,.F.);
#30944=ADVANCED_FACE('',(#3969),#541,.F.);
#30945=ADVANCED_FACE('',(#3970),#2501,.F.);
#30946=ADVANCED_FACE('',(#3971),#2502,.F.);
#30947=ADVANCED_FACE('',(#3972),#2503,.F.);
#30948=ADVANCED_FACE('',(#3973),#2504,.T.);
#30949=ADVANCED_FACE('',(#3974),#2505,.T.);
#30950=ADVANCED_FACE('',(#3975),#542,.F.);
#30951=ADVANCED_FACE('',(#3976),#543,.F.);
#30952=ADVANCED_FACE('',(#3977),#544,.F.);
#30953=ADVANCED_FACE('',(#3978),#545,.F.);
#30954=ADVANCED_FACE('',(#3979),#546,.F.);
#30955=ADVANCED_FACE('',(#3980),#547,.F.);
#30956=ADVANCED_FACE('',(#3981),#548,.F.);
#30957=ADVANCED_FACE('',(#3982),#549,.F.);
#30958=ADVANCED_FACE('',(#3983),#550,.F.);
#30959=ADVANCED_FACE('',(#3984),#551,.F.);
#30960=ADVANCED_FACE('',(#3985),#552,.F.);
#30961=ADVANCED_FACE('',(#3986),#553,.F.);
#30962=ADVANCED_FACE('',(#3987),#554,.F.);
#30963=ADVANCED_FACE('',(#3988),#555,.F.);
#30964=ADVANCED_FACE('',(#3989),#556,.F.);
#30965=ADVANCED_FACE('',(#3990),#557,.F.);
#30966=ADVANCED_FACE('',(#3991),#558,.F.);
#30967=ADVANCED_FACE('',(#3992),#559,.F.);
#30968=ADVANCED_FACE('',(#3993),#560,.F.);
#30969=ADVANCED_FACE('',(#3994),#561,.F.);
#30970=ADVANCED_FACE('',(#3995,#2086),#2506,.T.);
#30971=ADVANCED_FACE('',(#3996),#562,.F.);
#30972=ADVANCED_FACE('',(#3997),#563,.F.);
#30973=ADVANCED_FACE('',(#3998),#564,.F.);
#30974=ADVANCED_FACE('',(#3999),#565,.F.);
#30975=ADVANCED_FACE('',(#4000),#566,.F.);
#30976=ADVANCED_FACE('',(#4001),#567,.F.);
#30977=ADVANCED_FACE('',(#4002),#568,.F.);
#30978=ADVANCED_FACE('',(#4003),#569,.F.);
#30979=ADVANCED_FACE('',(#4004),#570,.F.);
#30980=ADVANCED_FACE('',(#4005),#571,.F.);
#30981=ADVANCED_FACE('',(#4006),#572,.F.);
#30982=ADVANCED_FACE('',(#4007),#573,.F.);
#30983=ADVANCED_FACE('',(#4008),#2507,.F.);
#30984=ADVANCED_FACE('',(#4009),#574,.F.);
#30985=ADVANCED_FACE('',(#4010),#575,.F.);
#30986=ADVANCED_FACE('',(#4011),#576,.F.);
#30987=ADVANCED_FACE('',(#4012),#577,.F.);
#30988=ADVANCED_FACE('',(#4013),#578,.F.);
#30989=ADVANCED_FACE('',(#4014),#579,.F.);
#30990=ADVANCED_FACE('',(#4015),#580,.F.);
#30991=ADVANCED_FACE('',(#4016),#2508,.F.);
#30992=ADVANCED_FACE('',(#4017),#581,.F.);
#30993=ADVANCED_FACE('',(#4018),#582,.F.);
#30994=ADVANCED_FACE('',(#4019),#583,.F.);
#30995=ADVANCED_FACE('',(#4020),#584,.F.);
#30996=ADVANCED_FACE('',(#4021),#585,.F.);
#30997=ADVANCED_FACE('',(#4022),#586,.F.);
#30998=ADVANCED_FACE('',(#4023),#587,.F.);
#30999=ADVANCED_FACE('',(#4024),#2509,.F.);
#31000=ADVANCED_FACE('',(#4025),#588,.F.);
#31001=ADVANCED_FACE('',(#4026),#2510,.T.);
#31002=ADVANCED_FACE('',(#4027),#2511,.T.);
#31003=ADVANCED_FACE('',(#4028),#589,.F.);
#31004=ADVANCED_FACE('',(#4029),#590,.F.);
#31005=ADVANCED_FACE('',(#4030),#591,.F.);
#31006=ADVANCED_FACE('',(#4031),#592,.F.);
#31007=ADVANCED_FACE('',(#4032),#593,.F.);
#31008=ADVANCED_FACE('',(#4033),#594,.F.);
#31009=ADVANCED_FACE('',(#4034),#595,.F.);
#31010=ADVANCED_FACE('',(#4035),#596,.F.);
#31011=ADVANCED_FACE('',(#4036),#597,.F.);
#31012=ADVANCED_FACE('',(#4037),#598,.F.);
#31013=ADVANCED_FACE('',(#4038),#599,.F.);
#31014=ADVANCED_FACE('',(#4039),#600,.F.);
#31015=ADVANCED_FACE('',(#4040),#601,.F.);
#31016=ADVANCED_FACE('',(#4041),#602,.F.);
#31017=ADVANCED_FACE('',(#4042),#603,.F.);
#31018=ADVANCED_FACE('',(#4043),#604,.F.);
#31019=ADVANCED_FACE('',(#4044),#605,.F.);
#31020=ADVANCED_FACE('',(#4045),#606,.F.);
#31021=ADVANCED_FACE('',(#4046),#607,.F.);
#31022=ADVANCED_FACE('',(#4047),#608,.F.);
#31023=ADVANCED_FACE('',(#4048,#2087),#2512,.T.);
#31024=ADVANCED_FACE('',(#4049),#2513,.F.);
#31025=ADVANCED_FACE('',(#4050),#2514,.F.);
#31026=ADVANCED_FACE('',(#4051),#2515,.F.);
#31027=ADVANCED_FACE('',(#4052),#2516,.F.);
#31028=ADVANCED_FACE('',(#4053),#2517,.F.);
#31029=ADVANCED_FACE('',(#4054),#2518,.F.);
#31030=ADVANCED_FACE('',(#4055),#2519,.F.);
#31031=ADVANCED_FACE('',(#4056),#2520,.F.);
#31032=ADVANCED_FACE('',(#4057),#2521,.F.);
#31033=ADVANCED_FACE('',(#4058),#2522,.F.);
#31034=ADVANCED_FACE('',(#4059),#2523,.F.);
#31035=ADVANCED_FACE('',(#4060),#2524,.F.);
#31036=ADVANCED_FACE('',(#4061),#2525,.F.);
#31037=ADVANCED_FACE('',(#4062),#2526,.F.);
#31038=ADVANCED_FACE('',(#4063,#2088),#2527,.F.);
#31039=ADVANCED_FACE('',(#4064),#2528,.T.);
#31040=ADVANCED_FACE('',(#4065),#2529,.T.);
#31041=ADVANCED_FACE('',(#4066),#2530,.F.);
#31042=ADVANCED_FACE('',(#4067),#2531,.F.);
#31043=ADVANCED_FACE('',(#4068),#2532,.F.);
#31044=ADVANCED_FACE('',(#4069),#2533,.F.);
#31045=ADVANCED_FACE('',(#4070),#2534,.F.);
#31046=ADVANCED_FACE('',(#4071),#2535,.F.);
#31047=ADVANCED_FACE('',(#4072),#2536,.F.);
#31048=ADVANCED_FACE('',(#4073),#2537,.F.);
#31049=ADVANCED_FACE('',(#4074),#2538,.F.);
#31050=ADVANCED_FACE('',(#4075),#2539,.F.);
#31051=ADVANCED_FACE('',(#4076),#2540,.F.);
#31052=ADVANCED_FACE('',(#4077),#2541,.F.);
#31053=ADVANCED_FACE('',(#4078),#2542,.F.);
#31054=ADVANCED_FACE('',(#4079),#2543,.F.);
#31055=ADVANCED_FACE('',(#4080),#2544,.F.);
#31056=ADVANCED_FACE('',(#4081),#2545,.F.);
#31057=ADVANCED_FACE('',(#4082),#2546,.F.);
#31058=ADVANCED_FACE('',(#4083),#2547,.F.);
#31059=ADVANCED_FACE('',(#4084),#2548,.F.);
#31060=ADVANCED_FACE('',(#4085),#2549,.F.);
#31061=ADVANCED_FACE('',(#4086),#2550,.F.);
#31062=ADVANCED_FACE('',(#4087),#2551,.F.);
#31063=ADVANCED_FACE('',(#4088),#2552,.F.);
#31064=ADVANCED_FACE('',(#4089),#2553,.F.);
#31065=ADVANCED_FACE('',(#4090),#2554,.F.);
#31066=ADVANCED_FACE('',(#4091),#2555,.F.);
#31067=ADVANCED_FACE('',(#4092),#2556,.F.);
#31068=ADVANCED_FACE('',(#4093),#2557,.F.);
#31069=ADVANCED_FACE('',(#4094),#2558,.F.);
#31070=ADVANCED_FACE('',(#4095),#2559,.F.);
#31071=ADVANCED_FACE('',(#4096),#2560,.F.);
#31072=ADVANCED_FACE('',(#4097),#2561,.F.);
#31073=ADVANCED_FACE('',(#4098),#2562,.F.);
#31074=ADVANCED_FACE('',(#4099),#2563,.F.);
#31075=ADVANCED_FACE('',(#4100),#2564,.F.);
#31076=ADVANCED_FACE('',(#4101),#2565,.F.);
#31077=ADVANCED_FACE('',(#4102),#2566,.F.);
#31078=ADVANCED_FACE('',(#4103),#2567,.F.);
#31079=ADVANCED_FACE('',(#4104),#2568,.F.);
#31080=ADVANCED_FACE('',(#4105),#2569,.F.);
#31081=ADVANCED_FACE('',(#4106),#2570,.F.);
#31082=ADVANCED_FACE('',(#4107),#2571,.F.);
#31083=ADVANCED_FACE('',(#4108),#2572,.F.);
#31084=ADVANCED_FACE('',(#4109),#2573,.F.);
#31085=ADVANCED_FACE('',(#4110),#2574,.F.);
#31086=ADVANCED_FACE('',(#4111),#2575,.F.);
#31087=ADVANCED_FACE('',(#4112),#2576,.F.);
#31088=ADVANCED_FACE('',(#4113),#2577,.F.);
#31089=ADVANCED_FACE('',(#4114),#2578,.F.);
#31090=ADVANCED_FACE('',(#4115),#2579,.F.);
#31091=ADVANCED_FACE('',(#4116),#2580,.F.);
#31092=ADVANCED_FACE('',(#4117),#2581,.F.);
#31093=ADVANCED_FACE('',(#4118),#2582,.F.);
#31094=ADVANCED_FACE('',(#4119),#2583,.F.);
#31095=ADVANCED_FACE('',(#4120),#2584,.F.);
#31096=ADVANCED_FACE('',(#4121),#2585,.F.);
#31097=ADVANCED_FACE('',(#4122),#2586,.F.);
#31098=ADVANCED_FACE('',(#4123),#2587,.F.);
#31099=ADVANCED_FACE('',(#4124),#2588,.F.);
#31100=ADVANCED_FACE('',(#4125),#2589,.F.);
#31101=ADVANCED_FACE('',(#4126),#2590,.F.);
#31102=ADVANCED_FACE('',(#4127),#2591,.F.);
#31103=ADVANCED_FACE('',(#4128),#2592,.F.);
#31104=ADVANCED_FACE('',(#4129),#2593,.F.);
#31105=ADVANCED_FACE('',(#4130),#2594,.F.);
#31106=ADVANCED_FACE('',(#4131),#2595,.F.);
#31107=ADVANCED_FACE('',(#4132),#2596,.F.);
#31108=ADVANCED_FACE('',(#4133),#2597,.F.);
#31109=ADVANCED_FACE('',(#4134),#2598,.F.);
#31110=ADVANCED_FACE('',(#4135),#2599,.F.);
#31111=ADVANCED_FACE('',(#4136),#2600,.F.);
#31112=ADVANCED_FACE('',(#4137),#2601,.F.);
#31113=ADVANCED_FACE('',(#4138),#2602,.F.);
#31114=ADVANCED_FACE('',(#4139),#2603,.F.);
#31115=ADVANCED_FACE('',(#4140),#2604,.F.);
#31116=ADVANCED_FACE('',(#4141),#2605,.F.);
#31117=ADVANCED_FACE('',(#4142),#2606,.F.);
#31118=ADVANCED_FACE('',(#4143),#2607,.F.);
#31119=ADVANCED_FACE('',(#4144),#2608,.F.);
#31120=ADVANCED_FACE('',(#4145),#2609,.F.);
#31121=ADVANCED_FACE('',(#4146),#2610,.F.);
#31122=ADVANCED_FACE('',(#4147),#2611,.F.);
#31123=ADVANCED_FACE('',(#4148),#2612,.F.);
#31124=ADVANCED_FACE('',(#4149),#2613,.F.);
#31125=ADVANCED_FACE('',(#4150),#2614,.F.);
#31126=ADVANCED_FACE('',(#4151),#2615,.F.);
#31127=ADVANCED_FACE('',(#4152),#2616,.F.);
#31128=ADVANCED_FACE('',(#4153),#2617,.F.);
#31129=ADVANCED_FACE('',(#4154),#2618,.F.);
#31130=ADVANCED_FACE('',(#4155),#2619,.F.);
#31131=ADVANCED_FACE('',(#4156),#2620,.F.);
#31132=ADVANCED_FACE('',(#4157),#2621,.F.);
#31133=ADVANCED_FACE('',(#4158),#2622,.F.);
#31134=ADVANCED_FACE('',(#4159),#2623,.F.);
#31135=ADVANCED_FACE('',(#4160),#2624,.F.);
#31136=ADVANCED_FACE('',(#4161),#2625,.F.);
#31137=ADVANCED_FACE('',(#4162),#2626,.F.);
#31138=ADVANCED_FACE('',(#4163),#2627,.F.);
#31139=ADVANCED_FACE('',(#4164),#2628,.F.);
#31140=ADVANCED_FACE('',(#4165),#2629,.F.);
#31141=ADVANCED_FACE('',(#4166),#2630,.F.);
#31142=ADVANCED_FACE('',(#4167),#2631,.F.);
#31143=ADVANCED_FACE('',(#4168),#2632,.F.);
#31144=ADVANCED_FACE('',(#4169),#2633,.F.);
#31145=ADVANCED_FACE('',(#4170),#2634,.F.);
#31146=ADVANCED_FACE('',(#4171),#2635,.F.);
#31147=ADVANCED_FACE('',(#4172),#2636,.F.);
#31148=ADVANCED_FACE('',(#4173),#2637,.F.);
#31149=ADVANCED_FACE('',(#4174),#2638,.F.);
#31150=ADVANCED_FACE('',(#4175),#2639,.F.);
#31151=ADVANCED_FACE('',(#4176),#2640,.F.);
#31152=ADVANCED_FACE('',(#4177),#2641,.F.);
#31153=ADVANCED_FACE('',(#4178),#2642,.F.);
#31154=ADVANCED_FACE('',(#4179),#2643,.F.);
#31155=ADVANCED_FACE('',(#4180),#2644,.F.);
#31156=ADVANCED_FACE('',(#4181),#2645,.F.);
#31157=ADVANCED_FACE('',(#4182),#2646,.F.);
#31158=ADVANCED_FACE('',(#4183),#2647,.F.);
#31159=ADVANCED_FACE('',(#4184),#2648,.F.);
#31160=ADVANCED_FACE('',(#4185),#2649,.F.);
#31161=ADVANCED_FACE('',(#4186),#2650,.F.);
#31162=ADVANCED_FACE('',(#4187),#2651,.F.);
#31163=ADVANCED_FACE('',(#4188),#2652,.F.);
#31164=ADVANCED_FACE('',(#4189),#2653,.F.);
#31165=ADVANCED_FACE('',(#4190),#2654,.F.);
#31166=ADVANCED_FACE('',(#4191),#2655,.F.);
#31167=ADVANCED_FACE('',(#4192),#2656,.F.);
#31168=ADVANCED_FACE('',(#4193),#2657,.F.);
#31169=ADVANCED_FACE('',(#4194),#2658,.F.);
#31170=ADVANCED_FACE('',(#4195),#2659,.F.);
#31171=ADVANCED_FACE('',(#4196),#2660,.F.);
#31172=ADVANCED_FACE('',(#4197),#2661,.F.);
#31173=ADVANCED_FACE('',(#4198),#2662,.F.);
#31174=ADVANCED_FACE('',(#4199),#2663,.F.);
#31175=ADVANCED_FACE('',(#4200),#2664,.F.);
#31176=ADVANCED_FACE('',(#4201),#2665,.F.);
#31177=ADVANCED_FACE('',(#4202),#2666,.F.);
#31178=ADVANCED_FACE('',(#4203),#2667,.F.);
#31179=ADVANCED_FACE('',(#4204),#2668,.F.);
#31180=ADVANCED_FACE('',(#4205),#2669,.F.);
#31181=ADVANCED_FACE('',(#4206),#2670,.F.);
#31182=ADVANCED_FACE('',(#4207),#2671,.F.);
#31183=ADVANCED_FACE('',(#4208),#2672,.F.);
#31184=ADVANCED_FACE('',(#4209),#2673,.F.);
#31185=ADVANCED_FACE('',(#4210),#2674,.F.);
#31186=ADVANCED_FACE('',(#4211),#2675,.F.);
#31187=ADVANCED_FACE('',(#4212),#2676,.F.);
#31188=ADVANCED_FACE('',(#4213),#2677,.F.);
#31189=ADVANCED_FACE('',(#4214),#2678,.F.);
#31190=ADVANCED_FACE('',(#4215),#2679,.F.);
#31191=ADVANCED_FACE('',(#4216),#2680,.F.);
#31192=ADVANCED_FACE('',(#4217),#2681,.F.);
#31193=ADVANCED_FACE('',(#4218),#2682,.F.);
#31194=ADVANCED_FACE('',(#4219),#2683,.F.);
#31195=ADVANCED_FACE('',(#4220),#2684,.F.);
#31196=ADVANCED_FACE('',(#4221),#2685,.F.);
#31197=ADVANCED_FACE('',(#4222),#2686,.F.);
#31198=ADVANCED_FACE('',(#4223),#2687,.F.);
#31199=ADVANCED_FACE('',(#4224),#2688,.F.);
#31200=ADVANCED_FACE('',(#4225),#2689,.F.);
#31201=ADVANCED_FACE('',(#4226),#2690,.F.);
#31202=ADVANCED_FACE('',(#4227),#2691,.F.);
#31203=ADVANCED_FACE('',(#4228),#2692,.F.);
#31204=ADVANCED_FACE('',(#4229),#2693,.F.);
#31205=ADVANCED_FACE('',(#4230),#2694,.F.);
#31206=ADVANCED_FACE('',(#4231),#2695,.F.);
#31207=ADVANCED_FACE('',(#4232),#2696,.F.);
#31208=ADVANCED_FACE('',(#4233),#2697,.F.);
#31209=ADVANCED_FACE('',(#4234),#2698,.F.);
#31210=ADVANCED_FACE('',(#4235),#2699,.F.);
#31211=ADVANCED_FACE('',(#4236),#2700,.F.);
#31212=ADVANCED_FACE('',(#4237),#2701,.F.);
#31213=ADVANCED_FACE('',(#4238),#2702,.F.);
#31214=ADVANCED_FACE('',(#4239),#2703,.F.);
#31215=ADVANCED_FACE('',(#4240),#2704,.F.);
#31216=ADVANCED_FACE('',(#4241),#2705,.F.);
#31217=ADVANCED_FACE('',(#4242),#2706,.F.);
#31218=ADVANCED_FACE('',(#4243),#2707,.F.);
#31219=ADVANCED_FACE('',(#4244),#2708,.F.);
#31220=ADVANCED_FACE('',(#4245),#2709,.F.);
#31221=ADVANCED_FACE('',(#4246),#2710,.F.);
#31222=ADVANCED_FACE('',(#4247),#2711,.F.);
#31223=ADVANCED_FACE('',(#4248),#2712,.F.);
#31224=ADVANCED_FACE('',(#4249),#2713,.F.);
#31225=ADVANCED_FACE('',(#4250),#2714,.F.);
#31226=ADVANCED_FACE('',(#4251),#2715,.F.);
#31227=ADVANCED_FACE('',(#4252),#2716,.F.);
#31228=ADVANCED_FACE('',(#4253),#2717,.F.);
#31229=ADVANCED_FACE('',(#4254),#2718,.F.);
#31230=ADVANCED_FACE('',(#4255),#2719,.F.);
#31231=ADVANCED_FACE('',(#4256),#2720,.F.);
#31232=ADVANCED_FACE('',(#4257),#2721,.F.);
#31233=ADVANCED_FACE('',(#4258),#2722,.F.);
#31234=ADVANCED_FACE('',(#4259),#2723,.F.);
#31235=ADVANCED_FACE('',(#4260),#2724,.F.);
#31236=ADVANCED_FACE('',(#4261),#2725,.F.);
#31237=ADVANCED_FACE('',(#4262),#2726,.F.);
#31238=ADVANCED_FACE('',(#4263),#2727,.F.);
#31239=ADVANCED_FACE('',(#4264),#2728,.F.);
#31240=ADVANCED_FACE('',(#4265),#2729,.F.);
#31241=ADVANCED_FACE('',(#4266),#2730,.F.);
#31242=ADVANCED_FACE('',(#4267),#2731,.F.);
#31243=ADVANCED_FACE('',(#4268),#2732,.F.);
#31244=ADVANCED_FACE('',(#4269),#2733,.F.);
#31245=ADVANCED_FACE('',(#4270),#2734,.F.);
#31246=ADVANCED_FACE('',(#4271),#2735,.F.);
#31247=ADVANCED_FACE('',(#4272),#2736,.F.);
#31248=ADVANCED_FACE('',(#4273),#2737,.F.);
#31249=ADVANCED_FACE('',(#4274),#2738,.F.);
#31250=ADVANCED_FACE('',(#4275),#2739,.F.);
#31251=ADVANCED_FACE('',(#4276),#2740,.F.);
#31252=ADVANCED_FACE('',(#4277),#2741,.F.);
#31253=ADVANCED_FACE('',(#4278),#2742,.F.);
#31254=ADVANCED_FACE('',(#4279),#2743,.F.);
#31255=ADVANCED_FACE('',(#4280),#2744,.F.);
#31256=ADVANCED_FACE('',(#4281),#2745,.F.);
#31257=ADVANCED_FACE('',(#4282),#2746,.F.);
#31258=ADVANCED_FACE('',(#4283),#2747,.F.);
#31259=ADVANCED_FACE('',(#4284),#2748,.F.);
#31260=ADVANCED_FACE('',(#4285),#2749,.F.);
#31261=ADVANCED_FACE('',(#4286),#2750,.F.);
#31262=ADVANCED_FACE('',(#4287),#2751,.F.);
#31263=ADVANCED_FACE('',(#4288),#2752,.F.);
#31264=ADVANCED_FACE('',(#4289),#2753,.F.);
#31265=ADVANCED_FACE('',(#4290),#2754,.F.);
#31266=ADVANCED_FACE('',(#4291),#2755,.F.);
#31267=ADVANCED_FACE('',(#4292),#2756,.F.);
#31268=ADVANCED_FACE('',(#4293),#2757,.F.);
#31269=ADVANCED_FACE('',(#4294),#2758,.F.);
#31270=ADVANCED_FACE('',(#4295),#2759,.F.);
#31271=ADVANCED_FACE('',(#4296),#2760,.F.);
#31272=ADVANCED_FACE('',(#4297),#2761,.F.);
#31273=ADVANCED_FACE('',(#4298),#2762,.F.);
#31274=ADVANCED_FACE('',(#4299),#2763,.F.);
#31275=ADVANCED_FACE('',(#4300),#2764,.F.);
#31276=ADVANCED_FACE('',(#4301),#2765,.F.);
#31277=ADVANCED_FACE('',(#4302),#2766,.F.);
#31278=ADVANCED_FACE('',(#4303),#2767,.F.);
#31279=ADVANCED_FACE('',(#4304),#2768,.F.);
#31280=ADVANCED_FACE('',(#4305),#2769,.F.);
#31281=ADVANCED_FACE('',(#4306),#2770,.F.);
#31282=ADVANCED_FACE('',(#4307),#2771,.F.);
#31283=ADVANCED_FACE('',(#4308),#2772,.F.);
#31284=ADVANCED_FACE('',(#4309),#2773,.F.);
#31285=ADVANCED_FACE('',(#4310),#2774,.F.);
#31286=ADVANCED_FACE('',(#4311),#2775,.F.);
#31287=ADVANCED_FACE('',(#4312),#2776,.F.);
#31288=ADVANCED_FACE('',(#4313),#2777,.F.);
#31289=ADVANCED_FACE('',(#4314),#2778,.F.);
#31290=ADVANCED_FACE('',(#4315),#2779,.F.);
#31291=ADVANCED_FACE('',(#4316),#2780,.F.);
#31292=ADVANCED_FACE('',(#4317),#2781,.F.);
#31293=ADVANCED_FACE('',(#4318),#2782,.F.);
#31294=ADVANCED_FACE('',(#4319),#2783,.F.);
#31295=ADVANCED_FACE('',(#4320),#2784,.F.);
#31296=ADVANCED_FACE('',(#4321),#2785,.F.);
#31297=ADVANCED_FACE('',(#4322),#2786,.F.);
#31298=ADVANCED_FACE('',(#4323),#2787,.F.);
#31299=ADVANCED_FACE('',(#4324),#2788,.F.);
#31300=ADVANCED_FACE('',(#4325),#2789,.F.);
#31301=ADVANCED_FACE('',(#4326),#2790,.F.);
#31302=ADVANCED_FACE('',(#4327),#2791,.F.);
#31303=ADVANCED_FACE('',(#4328),#2792,.F.);
#31304=ADVANCED_FACE('',(#4329),#2793,.F.);
#31305=ADVANCED_FACE('',(#4330),#2794,.F.);
#31306=ADVANCED_FACE('',(#4331),#2795,.F.);
#31307=ADVANCED_FACE('',(#4332),#2796,.F.);
#31308=ADVANCED_FACE('',(#4333),#2797,.F.);
#31309=ADVANCED_FACE('',(#4334),#2798,.F.);
#31310=ADVANCED_FACE('',(#4335),#2799,.F.);
#31311=ADVANCED_FACE('',(#4336),#2800,.F.);
#31312=ADVANCED_FACE('',(#4337),#2801,.F.);
#31313=ADVANCED_FACE('',(#4338),#2802,.F.);
#31314=ADVANCED_FACE('',(#4339),#2803,.F.);
#31315=ADVANCED_FACE('',(#4340),#2804,.F.);
#31316=ADVANCED_FACE('',(#4341),#2805,.F.);
#31317=ADVANCED_FACE('',(#4342),#2806,.F.);
#31318=ADVANCED_FACE('',(#4343),#2807,.F.);
#31319=ADVANCED_FACE('',(#4344),#2808,.F.);
#31320=ADVANCED_FACE('',(#4345),#2809,.F.);
#31321=ADVANCED_FACE('',(#4346),#2810,.F.);
#31322=ADVANCED_FACE('',(#4347),#2811,.F.);
#31323=ADVANCED_FACE('',(#4348),#2812,.F.);
#31324=ADVANCED_FACE('',(#4349),#2813,.F.);
#31325=ADVANCED_FACE('',(#4350),#2814,.F.);
#31326=ADVANCED_FACE('',(#4351),#2815,.F.);
#31327=ADVANCED_FACE('',(#4352),#2816,.F.);
#31328=ADVANCED_FACE('',(#4353),#2817,.F.);
#31329=ADVANCED_FACE('',(#4354),#2818,.F.);
#31330=ADVANCED_FACE('',(#4355),#2819,.F.);
#31331=ADVANCED_FACE('',(#4356),#2820,.F.);
#31332=ADVANCED_FACE('',(#4357),#2821,.F.);
#31333=ADVANCED_FACE('',(#4358),#2822,.F.);
#31334=ADVANCED_FACE('',(#4359),#2823,.F.);
#31335=ADVANCED_FACE('',(#4360),#2824,.F.);
#31336=ADVANCED_FACE('',(#4361),#2825,.F.);
#31337=ADVANCED_FACE('',(#4362),#2826,.F.);
#31338=ADVANCED_FACE('',(#4363),#2827,.F.);
#31339=ADVANCED_FACE('',(#4364),#2828,.F.);
#31340=ADVANCED_FACE('',(#4365),#2829,.F.);
#31341=ADVANCED_FACE('',(#4366),#2830,.F.);
#31342=ADVANCED_FACE('',(#4367),#2831,.F.);
#31343=ADVANCED_FACE('',(#4368),#2832,.F.);
#31344=ADVANCED_FACE('',(#4369),#2833,.F.);
#31345=ADVANCED_FACE('',(#4370),#2834,.F.);
#31346=ADVANCED_FACE('',(#4371),#2835,.F.);
#31347=ADVANCED_FACE('',(#4372),#2836,.F.);
#31348=ADVANCED_FACE('',(#4373),#2837,.F.);
#31349=ADVANCED_FACE('',(#4374),#2838,.F.);
#31350=ADVANCED_FACE('',(#4375),#2839,.F.);
#31351=ADVANCED_FACE('',(#4376),#2840,.F.);
#31352=ADVANCED_FACE('',(#4377),#2841,.F.);
#31353=ADVANCED_FACE('',(#4378),#2842,.F.);
#31354=ADVANCED_FACE('',(#4379),#2843,.F.);
#31355=ADVANCED_FACE('',(#4380),#2844,.F.);
#31356=ADVANCED_FACE('',(#4381),#2845,.F.);
#31357=ADVANCED_FACE('',(#4382),#2846,.F.);
#31358=ADVANCED_FACE('',(#4383),#2847,.F.);
#31359=ADVANCED_FACE('',(#4384),#2848,.F.);
#31360=ADVANCED_FACE('',(#4385),#2849,.F.);
#31361=ADVANCED_FACE('',(#4386),#2850,.F.);
#31362=ADVANCED_FACE('',(#4387),#2851,.F.);
#31363=ADVANCED_FACE('',(#4388),#2852,.F.);
#31364=ADVANCED_FACE('',(#4389),#2853,.F.);
#31365=ADVANCED_FACE('',(#4390),#2854,.F.);
#31366=ADVANCED_FACE('',(#4391),#2855,.F.);
#31367=ADVANCED_FACE('',(#4392),#2856,.F.);
#31368=ADVANCED_FACE('',(#4393),#2857,.F.);
#31369=ADVANCED_FACE('',(#4394),#2858,.F.);
#31370=ADVANCED_FACE('',(#4395),#2859,.F.);
#31371=ADVANCED_FACE('',(#4396),#2860,.F.);
#31372=ADVANCED_FACE('',(#4397),#2861,.F.);
#31373=ADVANCED_FACE('',(#4398),#2862,.F.);
#31374=ADVANCED_FACE('',(#4399),#2863,.F.);
#31375=ADVANCED_FACE('',(#4400),#2864,.F.);
#31376=ADVANCED_FACE('',(#4401),#2865,.F.);
#31377=ADVANCED_FACE('',(#4402),#2866,.F.);
#31378=ADVANCED_FACE('',(#4403),#2867,.F.);
#31379=ADVANCED_FACE('',(#4404),#2868,.F.);
#31380=ADVANCED_FACE('',(#4405),#2869,.F.);
#31381=ADVANCED_FACE('',(#4406),#2870,.F.);
#31382=ADVANCED_FACE('',(#4407),#2871,.F.);
#31383=ADVANCED_FACE('',(#4408),#2872,.F.);
#31384=ADVANCED_FACE('',(#4409),#2873,.F.);
#31385=ADVANCED_FACE('',(#4410),#2874,.F.);
#31386=ADVANCED_FACE('',(#4411),#2875,.F.);
#31387=ADVANCED_FACE('',(#4412),#2876,.F.);
#31388=ADVANCED_FACE('',(#4413),#2877,.F.);
#31389=ADVANCED_FACE('',(#4414),#2878,.F.);
#31390=ADVANCED_FACE('',(#4415),#2879,.F.);
#31391=ADVANCED_FACE('',(#4416),#2880,.F.);
#31392=ADVANCED_FACE('',(#4417),#2881,.F.);
#31393=ADVANCED_FACE('',(#4418),#2882,.F.);
#31394=ADVANCED_FACE('',(#4419),#2883,.F.);
#31395=ADVANCED_FACE('',(#4420),#2884,.F.);
#31396=ADVANCED_FACE('',(#4421),#2885,.F.);
#31397=ADVANCED_FACE('',(#4422),#2886,.F.);
#31398=ADVANCED_FACE('',(#4423),#2887,.F.);
#31399=ADVANCED_FACE('',(#4424),#2888,.F.);
#31400=ADVANCED_FACE('',(#4425),#2889,.F.);
#31401=ADVANCED_FACE('',(#4426),#2890,.F.);
#31402=ADVANCED_FACE('',(#4427),#2891,.F.);
#31403=ADVANCED_FACE('',(#4428),#2892,.F.);
#31404=ADVANCED_FACE('',(#4429),#2893,.F.);
#31405=ADVANCED_FACE('',(#4430),#2894,.F.);
#31406=ADVANCED_FACE('',(#4431),#2895,.F.);
#31407=ADVANCED_FACE('',(#4432),#2896,.F.);
#31408=ADVANCED_FACE('',(#4433),#2897,.F.);
#31409=ADVANCED_FACE('',(#4434),#2898,.F.);
#31410=ADVANCED_FACE('',(#4435),#2899,.F.);
#31411=ADVANCED_FACE('',(#4436),#2900,.F.);
#31412=ADVANCED_FACE('',(#4437),#2901,.F.);
#31413=ADVANCED_FACE('',(#4438),#2902,.F.);
#31414=ADVANCED_FACE('',(#4439),#2903,.F.);
#31415=ADVANCED_FACE('',(#4440),#2904,.F.);
#31416=ADVANCED_FACE('',(#4441),#2905,.F.);
#31417=ADVANCED_FACE('',(#4442),#2906,.F.);
#31418=ADVANCED_FACE('',(#4443),#2907,.F.);
#31419=ADVANCED_FACE('',(#4444),#2908,.F.);
#31420=ADVANCED_FACE('',(#4445),#2909,.F.);
#31421=ADVANCED_FACE('',(#4446),#2910,.F.);
#31422=ADVANCED_FACE('',(#4447),#2911,.F.);
#31423=ADVANCED_FACE('',(#4448),#2912,.F.);
#31424=ADVANCED_FACE('',(#4449),#2913,.F.);
#31425=ADVANCED_FACE('',(#4450),#2914,.F.);
#31426=ADVANCED_FACE('',(#4451),#2915,.F.);
#31427=ADVANCED_FACE('',(#4452),#2916,.F.);
#31428=ADVANCED_FACE('',(#4453),#2917,.F.);
#31429=ADVANCED_FACE('',(#4454),#2918,.F.);
#31430=ADVANCED_FACE('',(#4455),#2919,.F.);
#31431=ADVANCED_FACE('',(#4456),#2920,.F.);
#31432=ADVANCED_FACE('',(#4457),#2921,.F.);
#31433=ADVANCED_FACE('',(#4458),#2922,.F.);
#31434=ADVANCED_FACE('',(#4459),#2923,.F.);
#31435=ADVANCED_FACE('',(#4460),#2924,.F.);
#31436=ADVANCED_FACE('',(#4461),#2925,.F.);
#31437=ADVANCED_FACE('',(#4462),#2926,.F.);
#31438=ADVANCED_FACE('',(#4463),#2927,.F.);
#31439=ADVANCED_FACE('',(#4464),#2928,.F.);
#31440=ADVANCED_FACE('',(#4465),#2929,.F.);
#31441=ADVANCED_FACE('',(#4466),#2930,.F.);
#31442=ADVANCED_FACE('',(#4467),#2931,.F.);
#31443=ADVANCED_FACE('',(#4468),#2932,.F.);
#31444=ADVANCED_FACE('',(#4469),#2933,.F.);
#31445=ADVANCED_FACE('',(#4470),#2934,.F.);
#31446=ADVANCED_FACE('',(#4471),#2935,.F.);
#31447=ADVANCED_FACE('',(#4472),#2936,.F.);
#31448=ADVANCED_FACE('',(#4473),#2937,.F.);
#31449=ADVANCED_FACE('',(#4474),#2938,.F.);
#31450=ADVANCED_FACE('',(#4475),#2939,.F.);
#31451=ADVANCED_FACE('',(#4476),#2940,.F.);
#31452=ADVANCED_FACE('',(#4477),#2941,.F.);
#31453=ADVANCED_FACE('',(#4478),#2942,.F.);
#31454=ADVANCED_FACE('',(#4479),#2943,.F.);
#31455=ADVANCED_FACE('',(#4480),#2944,.F.);
#31456=ADVANCED_FACE('',(#4481),#2945,.F.);
#31457=ADVANCED_FACE('',(#4482),#2946,.F.);
#31458=ADVANCED_FACE('',(#4483),#2947,.F.);
#31459=ADVANCED_FACE('',(#4484),#2948,.F.);
#31460=ADVANCED_FACE('',(#4485),#2949,.F.);
#31461=ADVANCED_FACE('',(#4486),#2950,.F.);
#31462=ADVANCED_FACE('',(#4487),#2951,.F.);
#31463=ADVANCED_FACE('',(#4488),#2952,.F.);
#31464=ADVANCED_FACE('',(#4489),#2953,.F.);
#31465=ADVANCED_FACE('',(#4490),#2954,.F.);
#31466=ADVANCED_FACE('',(#4491),#1840,.F.);
#31467=ADVANCED_FACE('',(#4492),#1841,.F.);
#31468=ADVANCED_FACE('',(#4493),#2955,.T.);
#31469=ADVANCED_FACE('',(#4494),#1842,.T.);
#31470=ADVANCED_FACE('',(#4495),#2956,.T.);
#31471=ADVANCED_FACE('',(#4496),#1843,.T.);
#31472=ADVANCED_FACE('',(#4497),#2957,.T.);
#31473=ADVANCED_FACE('',(#4498),#1844,.T.);
#31474=ADVANCED_FACE('',(#4499),#2958,.T.);
#31475=ADVANCED_FACE('',(#4500),#1845,.T.);
#31476=ADVANCED_FACE('',(#4501,#2089,#2090,#2091,#2092,#2093,#2094,#2095,
#2096,#2097,#2098,#2099,#2100,#2101,#2102,#2103,#2104,#2105,#2106,#2107,
#2108,#2109,#2110,#2111,#2112,#2113,#2114,#2115,#2116,#2117,#2118,#2119,
#2120,#2121,#2122,#2123,#2124,#2125,#2126,#2127,#2128,#2129,#2130,#2131,
#2132,#2133,#2134,#2135,#2136,#2137,#2138,#2139,#2140,#2141,#2142,#2143,
#2144,#2145,#2146,#2147,#2148,#2149,#2150,#2151,#2152,#2153,#2154,#2155,
#2156,#2157,#2158,#2159,#2160,#2161,#2162,#2163,#2164,#2165,#2166,#2167,
#2168,#2169,#2170,#2171,#2172,#2173,#2174,#2175,#2176,#2177,#2178,#2179,
#2180,#2181,#2182,#2183,#2184,#2185,#2186,#2187,#2188,#2189,#2190,#2191,
#2192),#2959,.T.);
#31477=ADVANCED_FACE('',(#4502,#2193,#2194),#2960,.F.);
#31478=ADVANCED_FACE('',(#4503),#2961,.F.);
#31479=ADVANCED_FACE('',(#4504),#2962,.F.);
#31480=ADVANCED_FACE('',(#4505),#2963,.F.);
#31481=ADVANCED_FACE('',(#4506),#2964,.F.);
#31482=ADVANCED_FACE('',(#4507),#2965,.F.);
#31483=ADVANCED_FACE('',(#4508),#2966,.F.);
#31484=ADVANCED_FACE('',(#4509),#2967,.F.);
#31485=ADVANCED_FACE('',(#4510),#2968,.F.);
#31486=ADVANCED_FACE('',(#4511),#2969,.F.);
#31487=ADVANCED_FACE('',(#4512),#2970,.F.);
#31488=ADVANCED_FACE('',(#4513),#2971,.F.);
#31489=ADVANCED_FACE('',(#4514),#2972,.F.);
#31490=ADVANCED_FACE('',(#4515),#2973,.F.);
#31491=ADVANCED_FACE('',(#4516),#2974,.F.);
#31492=ADVANCED_FACE('',(#4517),#2975,.F.);
#31493=ADVANCED_FACE('',(#4518),#2976,.F.);
#31494=ADVANCED_FACE('',(#4519),#2977,.F.);
#31495=ADVANCED_FACE('',(#4520),#2978,.F.);
#31496=ADVANCED_FACE('',(#4521),#2979,.F.);
#31497=ADVANCED_FACE('',(#4522),#2980,.F.);
#31498=ADVANCED_FACE('',(#4523),#2981,.F.);
#31499=ADVANCED_FACE('',(#4524),#2982,.F.);
#31500=ADVANCED_FACE('',(#4525),#2983,.F.);
#31501=ADVANCED_FACE('',(#4526),#2984,.F.);
#31502=ADVANCED_FACE('',(#4527),#2985,.F.);
#31503=ADVANCED_FACE('',(#4528),#2986,.F.);
#31504=ADVANCED_FACE('',(#4529),#2987,.F.);
#31505=ADVANCED_FACE('',(#4530),#2988,.F.);
#31506=ADVANCED_FACE('',(#4531),#2989,.F.);
#31507=ADVANCED_FACE('',(#4532),#2990,.F.);
#31508=ADVANCED_FACE('',(#4533),#2991,.F.);
#31509=ADVANCED_FACE('',(#4534),#2992,.F.);
#31510=ADVANCED_FACE('',(#4535),#2993,.F.);
#31511=ADVANCED_FACE('',(#4536),#2994,.F.);
#31512=ADVANCED_FACE('',(#4537),#2995,.F.);
#31513=ADVANCED_FACE('',(#4538),#2996,.F.);
#31514=ADVANCED_FACE('',(#4539),#2997,.F.);
#31515=ADVANCED_FACE('',(#4540),#2998,.F.);
#31516=ADVANCED_FACE('',(#4541),#2999,.F.);
#31517=ADVANCED_FACE('',(#4542),#3000,.F.);
#31518=ADVANCED_FACE('',(#4543),#3001,.F.);
#31519=ADVANCED_FACE('',(#4544),#3002,.F.);
#31520=ADVANCED_FACE('',(#4545),#3003,.F.);
#31521=ADVANCED_FACE('',(#4546),#3004,.F.);
#31522=ADVANCED_FACE('',(#4547),#3005,.F.);
#31523=ADVANCED_FACE('',(#4548),#3006,.F.);
#31524=ADVANCED_FACE('',(#4549),#3007,.F.);
#31525=ADVANCED_FACE('',(#4550),#3008,.F.);
#31526=ADVANCED_FACE('',(#4551),#3009,.F.);
#31527=ADVANCED_FACE('',(#4552),#3010,.F.);
#31528=ADVANCED_FACE('',(#4553),#3011,.F.);
#31529=ADVANCED_FACE('',(#4554),#3012,.F.);
#31530=ADVANCED_FACE('',(#4555),#3013,.F.);
#31531=ADVANCED_FACE('',(#4556),#3014,.F.);
#31532=ADVANCED_FACE('',(#4557),#3015,.F.);
#31533=ADVANCED_FACE('',(#4558),#1846,.F.);
#31534=ADVANCED_FACE('',(#4559),#1847,.F.);
#31535=ADVANCED_FACE('',(#4560,#2195,#2196),#3016,.T.);
#31536=ADVANCED_FACE('',(#4561),#3017,.T.);
#31537=ADVANCED_FACE('',(#4562,#2197,#2198),#3018,.T.);
#31538=ADVANCED_FACE('',(#4563),#3019,.T.);
#31539=ADVANCED_FACE('',(#4564),#3020,.T.);
#31540=ADVANCED_FACE('',(#4565),#3021,.T.);
#31541=ADVANCED_FACE('',(#4566,#2199,#2200,#2201,#2202,#2203,#2204,#2205,
#2206,#2207,#2208,#2209),#3022,.T.);
#31542=ADVANCED_FACE('',(#4567),#3023,.T.);
#31543=ADVANCED_FACE('',(#4568),#3024,.T.);
#31544=ADVANCED_FACE('',(#4569),#3025,.F.);
#31545=ADVANCED_FACE('',(#4570),#30292,.F.);
#31546=ADVANCED_FACE('',(#4571,#2210,#2211),#3026,.F.);
#31547=ADVANCED_FACE('',(#4572),#30293,.F.);
#31548=ADVANCED_FACE('',(#4573),#3027,.T.);
#31549=ADVANCED_FACE('',(#4574),#1848,.F.);
#31550=ADVANCED_FACE('',(#4575,#2212),#3028,.F.);
#31551=ADVANCED_FACE('',(#4576),#1849,.F.);
#31552=ADVANCED_FACE('',(#4577,#2213),#3029,.F.);
#31553=ADVANCED_FACE('',(#4578),#1850,.F.);
#31554=ADVANCED_FACE('',(#4579),#1851,.F.);
#31555=ADVANCED_FACE('',(#4580),#3030,.T.);
#31556=ADVANCED_FACE('',(#4581),#3031,.F.);
#31557=ADVANCED_FACE('',(#4582),#1852,.F.);
#31558=ADVANCED_FACE('',(#4583),#3032,.F.);
#31559=ADVANCED_FACE('',(#4584),#1853,.F.);
#31560=ADVANCED_FACE('',(#4585),#3033,.F.);
#31561=ADVANCED_FACE('',(#4586),#1854,.F.);
#31562=ADVANCED_FACE('',(#4587),#3034,.F.);
#31563=ADVANCED_FACE('',(#4588),#1855,.F.);
#31564=ADVANCED_FACE('',(#4589),#3035,.T.);
#31565=ADVANCED_FACE('',(#4590),#3036,.T.);
#31566=ADVANCED_FACE('',(#4591),#3037,.T.);
#31567=ADVANCED_FACE('',(#4592),#3038,.T.);
#31568=ADVANCED_FACE('',(#4593),#3039,.T.);
#31569=ADVANCED_FACE('',(#4594),#3040,.T.);
#31570=ADVANCED_FACE('',(#4595),#3041,.T.);
#31571=ADVANCED_FACE('',(#4596),#1856,.T.);
#31572=ADVANCED_FACE('',(#4597),#1857,.T.);
#31573=ADVANCED_FACE('',(#4598),#1858,.T.);
#31574=ADVANCED_FACE('',(#4599),#1859,.T.);
#31575=ADVANCED_FACE('',(#4600),#1860,.T.);
#31576=ADVANCED_FACE('',(#4601),#1861,.T.);
#31577=ADVANCED_FACE('',(#4602),#1862,.T.);
#31578=ADVANCED_FACE('',(#4603),#1863,.T.);
#31579=ADVANCED_FACE('',(#4604),#1864,.T.);
#31580=ADVANCED_FACE('',(#4605),#1865,.T.);
#31581=ADVANCED_FACE('',(#4606),#1866,.T.);
#31582=ADVANCED_FACE('',(#4607),#1867,.T.);
#31583=ADVANCED_FACE('',(#4608),#1868,.T.);
#31584=ADVANCED_FACE('',(#4609),#1869,.T.);
#31585=ADVANCED_FACE('',(#4610),#1870,.T.);
#31586=ADVANCED_FACE('',(#4611),#1871,.T.);
#31587=ADVANCED_FACE('',(#4612),#1872,.T.);
#31588=ADVANCED_FACE('',(#4613),#1873,.T.);
#31589=ADVANCED_FACE('',(#4614),#1874,.T.);
#31590=ADVANCED_FACE('',(#4615),#3042,.F.);
#31591=ADVANCED_FACE('',(#4616),#609,.F.);
#31592=ADVANCED_FACE('',(#4617),#3043,.T.);
#31593=ADVANCED_FACE('',(#4618),#610,.F.);
#31594=ADVANCED_FACE('',(#4619),#30294,.F.);
#31595=ADVANCED_FACE('',(#4620),#1875,.T.);
#31596=ADVANCED_FACE('',(#4621),#1876,.T.);
#31597=ADVANCED_FACE('',(#4622),#1877,.T.);
#31598=ADVANCED_FACE('',(#4623),#1878,.T.);
#31599=ADVANCED_FACE('',(#4624),#1879,.T.);
#31600=ADVANCED_FACE('',(#4625),#1880,.T.);
#31601=ADVANCED_FACE('',(#4626),#3044,.F.);
#31602=ADVANCED_FACE('',(#4627),#3045,.F.);
#31603=ADVANCED_FACE('',(#4628),#3046,.F.);
#31604=ADVANCED_FACE('',(#4629),#3047,.T.);
#31605=ADVANCED_FACE('',(#4630),#3048,.T.);
#31606=ADVANCED_FACE('',(#4631),#3049,.T.);
#31607=ADVANCED_FACE('',(#4632),#3050,.T.);
#31608=ADVANCED_FACE('',(#4633),#3051,.T.);
#31609=ADVANCED_FACE('',(#4634),#3052,.T.);
#31610=ADVANCED_FACE('',(#4635),#3053,.F.);
#31611=ADVANCED_FACE('',(#4636),#3054,.F.);
#31612=ADVANCED_FACE('',(#4637),#3055,.F.);
#31613=ADVANCED_FACE('',(#4638),#3056,.F.);
#31614=ADVANCED_FACE('',(#4639),#3057,.F.);
#31615=ADVANCED_FACE('',(#4640),#3058,.F.);
#31616=ADVANCED_FACE('',(#4641),#30295,.F.);
#31617=ADVANCED_FACE('',(#4642),#3059,.F.);
#31618=ADVANCED_FACE('',(#4643),#3060,.F.);
#31619=ADVANCED_FACE('',(#4644),#3061,.F.);
#31620=ADVANCED_FACE('',(#4645),#3062,.T.);
#31621=ADVANCED_FACE('',(#4646),#30296,.T.);
#31622=ADVANCED_FACE('',(#4647),#30297,.T.);
#31623=ADVANCED_FACE('',(#4648,#2214),#3063,.T.);
#31624=ADVANCED_FACE('',(#4649),#30298,.F.);
#31625=ADVANCED_FACE('',(#4650),#1881,.F.);
#31626=ADVANCED_FACE('',(#4651,#2215),#3064,.T.);
#31627=ADVANCED_FACE('',(#4652),#30299,.F.);
#31628=ADVANCED_FACE('',(#4653),#30300,.F.);
#31629=ADVANCED_FACE('',(#4654),#1882,.F.);
#31630=ADVANCED_FACE('',(#4655,#2216),#3065,.T.);
#31631=ADVANCED_FACE('',(#4656),#30301,.F.);
#31632=ADVANCED_FACE('',(#4657),#30302,.F.);
#31633=ADVANCED_FACE('',(#4658,#2217,#2218,#2219,#2220,#2221),#3066,.F.);
#31634=ADVANCED_FACE('',(#4659),#1883,.F.);
#31635=ADVANCED_FACE('',(#4660),#30303,.F.);
#31636=ADVANCED_FACE('',(#4661),#1884,.F.);
#31637=ADVANCED_FACE('',(#4662),#30304,.F.);
#31638=ADVANCED_FACE('',(#4663),#30305,.F.);
#31639=ADVANCED_FACE('',(#4664),#30306,.F.);
#31640=ADVANCED_FACE('',(#4665),#1885,.F.);
#31641=ADVANCED_FACE('',(#4666),#30307,.F.);
#31642=ADVANCED_FACE('',(#4667),#1886,.F.);
#31643=ADVANCED_FACE('',(#4668,#2222),#3067,.F.);
#31644=ADVANCED_FACE('',(#4669,#2223),#3068,.F.);
#31645=ADVANCED_FACE('',(#4670),#1887,.F.);
#31646=ADVANCED_FACE('',(#4671),#1888,.F.);
#31647=ADVANCED_FACE('',(#4672),#30308,.F.);
#31648=ADVANCED_FACE('',(#4673),#1889,.F.);
#31649=ADVANCED_FACE('',(#4674,#2224,#2225,#2226),#3069,.T.);
#31650=ADVANCED_FACE('',(#4675),#30309,.F.);
#31651=ADVANCED_FACE('',(#4676),#3070,.T.);
#31652=ADVANCED_FACE('',(#4677),#3071,.T.);
#31653=ADVANCED_FACE('',(#4678),#3072,.T.);
#31654=ADVANCED_FACE('',(#4679),#3073,.T.);
#31655=ADVANCED_FACE('',(#4680),#3074,.T.);
#31656=ADVANCED_FACE('',(#4681),#3075,.T.);
#31657=ADVANCED_FACE('',(#4682),#1890,.T.);
#31658=ADVANCED_FACE('',(#4683),#1891,.T.);
#31659=ADVANCED_FACE('',(#4684),#1892,.T.);
#31660=ADVANCED_FACE('',(#4685),#1893,.T.);
#31661=ADVANCED_FACE('',(#4686),#1894,.T.);
#31662=ADVANCED_FACE('',(#4687),#1895,.T.);
#31663=ADVANCED_FACE('',(#4688),#1896,.T.);
#31664=ADVANCED_FACE('',(#4689),#1897,.T.);
#31665=ADVANCED_FACE('',(#4690),#1898,.T.);
#31666=ADVANCED_FACE('',(#4691),#1899,.T.);
#31667=ADVANCED_FACE('',(#4692),#1900,.T.);
#31668=ADVANCED_FACE('',(#4693),#1901,.T.);
#31669=ADVANCED_FACE('',(#4694),#1902,.T.);
#31670=ADVANCED_FACE('',(#4695),#1903,.T.);
#31671=ADVANCED_FACE('',(#4696),#1904,.T.);
#31672=ADVANCED_FACE('',(#4697),#1905,.T.);
#31673=ADVANCED_FACE('',(#4698),#1906,.T.);
#31674=ADVANCED_FACE('',(#4699),#1907,.T.);
#31675=ADVANCED_FACE('',(#4700),#1908,.T.);
#31676=ADVANCED_FACE('',(#4701),#1909,.T.);
#31677=ADVANCED_FACE('',(#4702),#1910,.T.);
#31678=ADVANCED_FACE('',(#4703),#1911,.T.);
#31679=ADVANCED_FACE('',(#4704),#1912,.T.);
#31680=ADVANCED_FACE('',(#4705),#1913,.T.);
#31681=ADVANCED_FACE('',(#4706),#1914,.T.);
#31682=ADVANCED_FACE('',(#4707),#1915,.T.);
#31683=ADVANCED_FACE('',(#4708),#1916,.T.);
#31684=ADVANCED_FACE('',(#4709),#1917,.T.);
#31685=ADVANCED_FACE('',(#4710),#1918,.T.);
#31686=ADVANCED_FACE('',(#4711),#1919,.T.);
#31687=ADVANCED_FACE('',(#4712),#1920,.T.);
#31688=ADVANCED_FACE('',(#4713),#1921,.T.);
#31689=ADVANCED_FACE('',(#4714),#1922,.T.);
#31690=ADVANCED_FACE('',(#4715),#1923,.T.);
#31691=ADVANCED_FACE('',(#4716),#1924,.T.);
#31692=ADVANCED_FACE('',(#4717),#1925,.T.);
#31693=ADVANCED_FACE('',(#4718),#1926,.T.);
#31694=ADVANCED_FACE('',(#4719),#1927,.T.);
#31695=ADVANCED_FACE('',(#4720),#1928,.T.);
#31696=ADVANCED_FACE('',(#4721),#1929,.T.);
#31697=ADVANCED_FACE('',(#4722),#1930,.T.);
#31698=ADVANCED_FACE('',(#4723),#1931,.T.);
#31699=ADVANCED_FACE('',(#4724),#1932,.T.);
#31700=ADVANCED_FACE('',(#4725),#1933,.T.);
#31701=ADVANCED_FACE('',(#4726),#1934,.T.);
#31702=ADVANCED_FACE('',(#4727),#1935,.T.);
#31703=ADVANCED_FACE('',(#4728),#1936,.T.);
#31704=ADVANCED_FACE('',(#4729),#1937,.T.);
#31705=ADVANCED_FACE('',(#4730),#3076,.F.);
#31706=ADVANCED_FACE('',(#4731),#611,.F.);
#31707=ADVANCED_FACE('',(#4732),#3077,.T.);
#31708=ADVANCED_FACE('',(#4733),#612,.F.);
#31709=ADVANCED_FACE('',(#4734),#95,.F.);
#31710=ADVANCED_FACE('',(#4735,#2227),#3078,.T.);
#31711=ADVANCED_FACE('',(#4736),#30310,.T.);
#31712=ADVANCED_FACE('',(#4737),#3079,.T.);
#31713=ADVANCED_FACE('',(#4738),#3080,.F.);
#31714=ADVANCED_FACE('',(#4739),#3081,.F.);
#31715=ADVANCED_FACE('',(#4740),#3082,.F.);
#31716=ADVANCED_FACE('',(#4741),#1938,.T.);
#31717=ADVANCED_FACE('',(#4742),#3083,.F.);
#31718=ADVANCED_FACE('',(#4743),#3084,.F.);
#31719=ADVANCED_FACE('',(#4744),#3085,.F.);
#31720=ADVANCED_FACE('',(#4745),#30311,.T.);
#31721=ADVANCED_FACE('',(#4746),#3086,.F.);
#31722=ADVANCED_FACE('',(#4747),#3087,.F.);
#31723=ADVANCED_FACE('',(#4748),#3088,.F.);
#31724=ADVANCED_FACE('',(#4749),#3089,.F.);
#31725=ADVANCED_FACE('',(#4750),#3090,.F.);
#31726=ADVANCED_FACE('',(#4751),#3091,.F.);
#31727=ADVANCED_FACE('',(#4752),#3092,.F.);
#31728=ADVANCED_FACE('',(#4753),#3093,.F.);
#31729=ADVANCED_FACE('',(#4754),#3094,.F.);
#31730=ADVANCED_FACE('',(#4755),#3095,.F.);
#31731=ADVANCED_FACE('',(#4756),#3096,.F.);
#31732=ADVANCED_FACE('',(#4757),#3097,.F.);
#31733=ADVANCED_FACE('',(#4758),#3098,.F.);
#31734=ADVANCED_FACE('',(#4759),#3099,.F.);
#31735=ADVANCED_FACE('',(#4760),#3100,.F.);
#31736=ADVANCED_FACE('',(#4761),#3101,.F.);
#31737=ADVANCED_FACE('',(#4762),#3102,.F.);
#31738=ADVANCED_FACE('',(#4763),#3103,.F.);
#31739=ADVANCED_FACE('',(#4764),#3104,.F.);
#31740=ADVANCED_FACE('',(#4765),#3105,.F.);
#31741=ADVANCED_FACE('',(#4766),#3106,.F.);
#31742=ADVANCED_FACE('',(#4767),#3107,.F.);
#31743=ADVANCED_FACE('',(#4768),#3108,.F.);
#31744=ADVANCED_FACE('',(#4769),#3109,.F.);
#31745=ADVANCED_FACE('',(#4770),#3110,.F.);
#31746=ADVANCED_FACE('',(#4771),#3111,.F.);
#31747=ADVANCED_FACE('',(#4772),#3112,.F.);
#31748=ADVANCED_FACE('',(#4773),#3113,.F.);
#31749=ADVANCED_FACE('',(#4774),#3114,.F.);
#31750=ADVANCED_FACE('',(#4775),#3115,.F.);
#31751=ADVANCED_FACE('',(#4776),#3116,.F.);
#31752=ADVANCED_FACE('',(#4777),#3117,.F.);
#31753=ADVANCED_FACE('',(#4778),#3118,.F.);
#31754=ADVANCED_FACE('',(#4779),#3119,.F.);
#31755=ADVANCED_FACE('',(#4780),#3120,.F.);
#31756=ADVANCED_FACE('',(#4781),#3121,.F.);
#31757=ADVANCED_FACE('',(#4782),#3122,.F.);
#31758=ADVANCED_FACE('',(#4783),#3123,.F.);
#31759=ADVANCED_FACE('',(#4784),#3124,.F.);
#31760=ADVANCED_FACE('',(#4785),#3125,.F.);
#31761=ADVANCED_FACE('',(#4786),#3126,.F.);
#31762=ADVANCED_FACE('',(#4787),#3127,.F.);
#31763=ADVANCED_FACE('',(#4788),#3128,.F.);
#31764=ADVANCED_FACE('',(#4789),#3129,.F.);
#31765=ADVANCED_FACE('',(#4790),#3130,.F.);
#31766=ADVANCED_FACE('',(#4791),#3131,.F.);
#31767=ADVANCED_FACE('',(#4792),#3132,.F.);
#31768=ADVANCED_FACE('',(#4793),#3133,.F.);
#31769=ADVANCED_FACE('',(#4794),#3134,.F.);
#31770=ADVANCED_FACE('',(#4795),#3135,.F.);
#31771=ADVANCED_FACE('',(#4796),#3136,.F.);
#31772=ADVANCED_FACE('',(#4797),#3137,.F.);
#31773=ADVANCED_FACE('',(#4798),#3138,.F.);
#31774=ADVANCED_FACE('',(#4799),#3139,.F.);
#31775=ADVANCED_FACE('',(#4800),#3140,.F.);
#31776=ADVANCED_FACE('',(#4801),#3141,.F.);
#31777=ADVANCED_FACE('',(#4802),#3142,.F.);
#31778=ADVANCED_FACE('',(#4803),#3143,.F.);
#31779=ADVANCED_FACE('',(#4804),#3144,.F.);
#31780=ADVANCED_FACE('',(#4805),#3145,.F.);
#31781=ADVANCED_FACE('',(#4806),#3146,.F.);
#31782=ADVANCED_FACE('',(#4807),#3147,.F.);
#31783=ADVANCED_FACE('',(#4808),#3148,.F.);
#31784=ADVANCED_FACE('',(#4809),#3149,.F.);
#31785=ADVANCED_FACE('',(#4810),#3150,.F.);
#31786=ADVANCED_FACE('',(#4811),#3151,.F.);
#31787=ADVANCED_FACE('',(#4812),#3152,.F.);
#31788=ADVANCED_FACE('',(#4813),#3153,.F.);
#31789=ADVANCED_FACE('',(#4814),#3154,.F.);
#31790=ADVANCED_FACE('',(#4815),#3155,.F.);
#31791=ADVANCED_FACE('',(#4816),#3156,.F.);
#31792=ADVANCED_FACE('',(#4817),#3157,.F.);
#31793=ADVANCED_FACE('',(#4818),#3158,.F.);
#31794=ADVANCED_FACE('',(#4819),#3159,.F.);
#31795=ADVANCED_FACE('',(#4820),#3160,.F.);
#31796=ADVANCED_FACE('',(#4821),#3161,.F.);
#31797=ADVANCED_FACE('',(#4822),#3162,.F.);
#31798=ADVANCED_FACE('',(#4823),#3163,.F.);
#31799=ADVANCED_FACE('',(#4824),#3164,.F.);
#31800=ADVANCED_FACE('',(#4825),#3165,.F.);
#31801=ADVANCED_FACE('',(#4826),#3166,.F.);
#31802=ADVANCED_FACE('',(#4827),#3167,.F.);
#31803=ADVANCED_FACE('',(#4828),#3168,.F.);
#31804=ADVANCED_FACE('',(#4829),#3169,.F.);
#31805=ADVANCED_FACE('',(#4830),#3170,.F.);
#31806=ADVANCED_FACE('',(#4831),#3171,.F.);
#31807=ADVANCED_FACE('',(#4832),#3172,.F.);
#31808=ADVANCED_FACE('',(#4833),#3173,.F.);
#31809=ADVANCED_FACE('',(#4834),#3174,.F.);
#31810=ADVANCED_FACE('',(#4835),#3175,.F.);
#31811=ADVANCED_FACE('',(#4836),#3176,.F.);
#31812=ADVANCED_FACE('',(#4837),#3177,.F.);
#31813=ADVANCED_FACE('',(#4838),#3178,.F.);
#31814=ADVANCED_FACE('',(#4839),#3179,.F.);
#31815=ADVANCED_FACE('',(#4840),#3180,.F.);
#31816=ADVANCED_FACE('',(#4841),#3181,.F.);
#31817=ADVANCED_FACE('',(#4842),#3182,.F.);
#31818=ADVANCED_FACE('',(#4843),#3183,.F.);
#31819=ADVANCED_FACE('',(#4844),#3184,.F.);
#31820=ADVANCED_FACE('',(#4845),#3185,.F.);
#31821=ADVANCED_FACE('',(#4846),#3186,.F.);
#31822=ADVANCED_FACE('',(#4847),#3187,.F.);
#31823=ADVANCED_FACE('',(#4848),#96,.T.);
#31824=ADVANCED_FACE('',(#4849,#2228),#3188,.F.);
#31825=ADVANCED_FACE('',(#4850),#30312,.F.);
#31826=ADVANCED_FACE('',(#4851),#1939,.T.);
#31827=ADVANCED_FACE('',(#4852),#1940,.T.);
#31828=ADVANCED_FACE('',(#4853),#1941,.T.);
#31829=ADVANCED_FACE('',(#4854),#1942,.T.);
#31830=ADVANCED_FACE('',(#4855),#1943,.T.);
#31831=ADVANCED_FACE('',(#4856),#1944,.T.);
#31832=ADVANCED_FACE('',(#4857),#3189,.F.);
#31833=ADVANCED_FACE('',(#4858),#3190,.F.);
#31834=ADVANCED_FACE('',(#4859),#3191,.F.);
#31835=ADVANCED_FACE('',(#4860),#3192,.F.);
#31836=ADVANCED_FACE('',(#4861),#3193,.F.);
#31837=ADVANCED_FACE('',(#4862),#3194,.F.);
#31838=ADVANCED_FACE('',(#4863),#3195,.F.);
#31839=ADVANCED_FACE('',(#4864),#3196,.F.);
#31840=ADVANCED_FACE('',(#4865),#3197,.F.);
#31841=ADVANCED_FACE('',(#4866),#3198,.F.);
#31842=ADVANCED_FACE('',(#4867),#3199,.F.);
#31843=ADVANCED_FACE('',(#4868),#3200,.F.);
#31844=ADVANCED_FACE('',(#4869),#3201,.F.);
#31845=ADVANCED_FACE('',(#4870),#3202,.F.);
#31846=ADVANCED_FACE('',(#4871),#3203,.F.);
#31847=ADVANCED_FACE('',(#4872),#30313,.F.);
#31848=ADVANCED_FACE('',(#4873),#3204,.F.);
#31849=ADVANCED_FACE('',(#4874),#3205,.F.);
#31850=ADVANCED_FACE('',(#4875),#3206,.F.);
#31851=ADVANCED_FACE('',(#4876),#1945,.T.);
#31852=ADVANCED_FACE('',(#4877),#1946,.T.);
#31853=ADVANCED_FACE('',(#4878),#1947,.T.);
#31854=ADVANCED_FACE('',(#4879),#1948,.T.);
#31855=ADVANCED_FACE('',(#4880),#1949,.T.);
#31856=ADVANCED_FACE('',(#4881),#1950,.T.);
#31857=ADVANCED_FACE('',(#4882),#1951,.T.);
#31858=ADVANCED_FACE('',(#4883),#1952,.T.);
#31859=ADVANCED_FACE('',(#4884),#1953,.T.);
#31860=ADVANCED_FACE('',(#4885),#1954,.T.);
#31861=ADVANCED_FACE('',(#4886),#1955,.T.);
#31862=ADVANCED_FACE('',(#4887),#1956,.T.);
#31863=ADVANCED_FACE('',(#4888),#1957,.T.);
#31864=ADVANCED_FACE('',(#4889),#1958,.T.);
#31865=ADVANCED_FACE('',(#4890),#1959,.T.);
#31866=ADVANCED_FACE('',(#4891),#1960,.T.);
#31867=ADVANCED_FACE('',(#4892),#1961,.T.);
#31868=ADVANCED_FACE('',(#4893),#1962,.T.);
#31869=ADVANCED_FACE('',(#4894),#1963,.T.);
#31870=ADVANCED_FACE('',(#4895),#1964,.T.);
#31871=ADVANCED_FACE('',(#4896),#1965,.T.);
#31872=ADVANCED_FACE('',(#4897),#1966,.T.);
#31873=ADVANCED_FACE('',(#4898),#1967,.T.);
#31874=ADVANCED_FACE('',(#4899),#1968,.T.);
#31875=ADVANCED_FACE('',(#4900),#1969,.T.);
#31876=ADVANCED_FACE('',(#4901),#1970,.T.);
#31877=ADVANCED_FACE('',(#4902),#1971,.T.);
#31878=ADVANCED_FACE('',(#4903),#1972,.T.);
#31879=ADVANCED_FACE('',(#4904),#1973,.T.);
#31880=ADVANCED_FACE('',(#4905),#1974,.T.);
#31881=ADVANCED_FACE('',(#4906),#1975,.T.);
#31882=ADVANCED_FACE('',(#4907),#1976,.T.);
#31883=ADVANCED_FACE('',(#4908),#1977,.T.);
#31884=ADVANCED_FACE('',(#4909),#1978,.T.);
#31885=ADVANCED_FACE('',(#4910),#1979,.T.);
#31886=ADVANCED_FACE('',(#4911),#1980,.T.);
#31887=ADVANCED_FACE('',(#4912),#1981,.T.);
#31888=ADVANCED_FACE('',(#4913),#1982,.T.);
#31889=ADVANCED_FACE('',(#4914),#1983,.T.);
#31890=ADVANCED_FACE('',(#4915),#1984,.T.);
#31891=ADVANCED_FACE('',(#4916),#3207,.F.);
#31892=ADVANCED_FACE('',(#4917),#613,.F.);
#31893=ADVANCED_FACE('',(#4918),#3208,.T.);
#31894=ADVANCED_FACE('',(#4919),#614,.F.);
#31895=ADVANCED_FACE('',(#4920),#97,.F.);
#31896=ADVANCED_FACE('',(#4921,#2229),#3209,.T.);
#31897=ADVANCED_FACE('',(#4922),#30314,.T.);
#31898=ADVANCED_FACE('',(#4923),#3210,.T.);
#31899=ADVANCED_FACE('',(#4924),#3211,.F.);
#31900=ADVANCED_FACE('',(#4925),#3212,.F.);
#31901=ADVANCED_FACE('',(#4926),#3213,.F.);
#31902=ADVANCED_FACE('',(#4927),#1985,.T.);
#31903=ADVANCED_FACE('',(#4928),#3214,.F.);
#31904=ADVANCED_FACE('',(#4929),#3215,.F.);
#31905=ADVANCED_FACE('',(#4930),#3216,.F.);
#31906=ADVANCED_FACE('',(#4931),#30315,.T.);
#31907=ADVANCED_FACE('',(#4932),#3217,.F.);
#31908=ADVANCED_FACE('',(#4933),#3218,.F.);
#31909=ADVANCED_FACE('',(#4934),#3219,.F.);
#31910=ADVANCED_FACE('',(#4935),#3220,.F.);
#31911=ADVANCED_FACE('',(#4936),#3221,.F.);
#31912=ADVANCED_FACE('',(#4937),#3222,.F.);
#31913=ADVANCED_FACE('',(#4938),#3223,.F.);
#31914=ADVANCED_FACE('',(#4939),#3224,.F.);
#31915=ADVANCED_FACE('',(#4940),#3225,.F.);
#31916=ADVANCED_FACE('',(#4941),#3226,.F.);
#31917=ADVANCED_FACE('',(#4942),#3227,.F.);
#31918=ADVANCED_FACE('',(#4943),#3228,.F.);
#31919=ADVANCED_FACE('',(#4944),#3229,.F.);
#31920=ADVANCED_FACE('',(#4945),#3230,.F.);
#31921=ADVANCED_FACE('',(#4946),#3231,.F.);
#31922=ADVANCED_FACE('',(#4947),#3232,.F.);
#31923=ADVANCED_FACE('',(#4948),#3233,.F.);
#31924=ADVANCED_FACE('',(#4949),#3234,.F.);
#31925=ADVANCED_FACE('',(#4950),#3235,.F.);
#31926=ADVANCED_FACE('',(#4951),#3236,.F.);
#31927=ADVANCED_FACE('',(#4952),#3237,.F.);
#31928=ADVANCED_FACE('',(#4953),#3238,.F.);
#31929=ADVANCED_FACE('',(#4954),#3239,.F.);
#31930=ADVANCED_FACE('',(#4955),#3240,.F.);
#31931=ADVANCED_FACE('',(#4956),#3241,.F.);
#31932=ADVANCED_FACE('',(#4957),#3242,.F.);
#31933=ADVANCED_FACE('',(#4958),#3243,.F.);
#31934=ADVANCED_FACE('',(#4959),#3244,.F.);
#31935=ADVANCED_FACE('',(#4960),#3245,.F.);
#31936=ADVANCED_FACE('',(#4961),#3246,.F.);
#31937=ADVANCED_FACE('',(#4962),#3247,.F.);
#31938=ADVANCED_FACE('',(#4963),#3248,.F.);
#31939=ADVANCED_FACE('',(#4964),#3249,.F.);
#31940=ADVANCED_FACE('',(#4965),#3250,.F.);
#31941=ADVANCED_FACE('',(#4966),#3251,.F.);
#31942=ADVANCED_FACE('',(#4967),#3252,.F.);
#31943=ADVANCED_FACE('',(#4968),#3253,.F.);
#31944=ADVANCED_FACE('',(#4969),#3254,.F.);
#31945=ADVANCED_FACE('',(#4970),#3255,.F.);
#31946=ADVANCED_FACE('',(#4971),#3256,.F.);
#31947=ADVANCED_FACE('',(#4972),#3257,.F.);
#31948=ADVANCED_FACE('',(#4973),#3258,.F.);
#31949=ADVANCED_FACE('',(#4974),#3259,.F.);
#31950=ADVANCED_FACE('',(#4975),#3260,.F.);
#31951=ADVANCED_FACE('',(#4976),#3261,.F.);
#31952=ADVANCED_FACE('',(#4977),#3262,.F.);
#31953=ADVANCED_FACE('',(#4978),#3263,.F.);
#31954=ADVANCED_FACE('',(#4979),#3264,.F.);
#31955=ADVANCED_FACE('',(#4980),#3265,.F.);
#31956=ADVANCED_FACE('',(#4981),#3266,.F.);
#31957=ADVANCED_FACE('',(#4982),#3267,.F.);
#31958=ADVANCED_FACE('',(#4983),#3268,.F.);
#31959=ADVANCED_FACE('',(#4984),#3269,.F.);
#31960=ADVANCED_FACE('',(#4985),#3270,.F.);
#31961=ADVANCED_FACE('',(#4986),#3271,.F.);
#31962=ADVANCED_FACE('',(#4987),#3272,.F.);
#31963=ADVANCED_FACE('',(#4988),#3273,.F.);
#31964=ADVANCED_FACE('',(#4989),#3274,.F.);
#31965=ADVANCED_FACE('',(#4990),#3275,.F.);
#31966=ADVANCED_FACE('',(#4991),#3276,.F.);
#31967=ADVANCED_FACE('',(#4992),#3277,.F.);
#31968=ADVANCED_FACE('',(#4993),#3278,.F.);
#31969=ADVANCED_FACE('',(#4994),#3279,.F.);
#31970=ADVANCED_FACE('',(#4995),#3280,.F.);
#31971=ADVANCED_FACE('',(#4996),#3281,.F.);
#31972=ADVANCED_FACE('',(#4997),#3282,.F.);
#31973=ADVANCED_FACE('',(#4998),#3283,.F.);
#31974=ADVANCED_FACE('',(#4999),#3284,.F.);
#31975=ADVANCED_FACE('',(#5000),#3285,.F.);
#31976=ADVANCED_FACE('',(#5001),#3286,.F.);
#31977=ADVANCED_FACE('',(#5002),#3287,.F.);
#31978=ADVANCED_FACE('',(#5003),#3288,.F.);
#31979=ADVANCED_FACE('',(#5004),#3289,.F.);
#31980=ADVANCED_FACE('',(#5005),#3290,.F.);
#31981=ADVANCED_FACE('',(#5006),#3291,.F.);
#31982=ADVANCED_FACE('',(#5007),#3292,.F.);
#31983=ADVANCED_FACE('',(#5008),#3293,.F.);
#31984=ADVANCED_FACE('',(#5009),#3294,.F.);
#31985=ADVANCED_FACE('',(#5010),#3295,.F.);
#31986=ADVANCED_FACE('',(#5011),#3296,.F.);
#31987=ADVANCED_FACE('',(#5012),#3297,.F.);
#31988=ADVANCED_FACE('',(#5013),#3298,.F.);
#31989=ADVANCED_FACE('',(#5014),#3299,.F.);
#31990=ADVANCED_FACE('',(#5015),#3300,.F.);
#31991=ADVANCED_FACE('',(#5016),#3301,.F.);
#31992=ADVANCED_FACE('',(#5017),#3302,.F.);
#31993=ADVANCED_FACE('',(#5018),#3303,.F.);
#31994=ADVANCED_FACE('',(#5019),#3304,.F.);
#31995=ADVANCED_FACE('',(#5020),#3305,.F.);
#31996=ADVANCED_FACE('',(#5021),#3306,.F.);
#31997=ADVANCED_FACE('',(#5022),#3307,.F.);
#31998=ADVANCED_FACE('',(#5023),#3308,.F.);
#31999=ADVANCED_FACE('',(#5024),#3309,.F.);
#32000=ADVANCED_FACE('',(#5025),#3310,.F.);
#32001=ADVANCED_FACE('',(#5026),#3311,.F.);
#32002=ADVANCED_FACE('',(#5027),#3312,.F.);
#32003=ADVANCED_FACE('',(#5028),#3313,.F.);
#32004=ADVANCED_FACE('',(#5029),#3314,.F.);
#32005=ADVANCED_FACE('',(#5030),#3315,.F.);
#32006=ADVANCED_FACE('',(#5031),#3316,.F.);
#32007=ADVANCED_FACE('',(#5032),#3317,.F.);
#32008=ADVANCED_FACE('',(#5033),#3318,.F.);
#32009=ADVANCED_FACE('',(#5034),#98,.T.);
#32010=ADVANCED_FACE('',(#5035,#2230),#3319,.F.);
#32011=ADVANCED_FACE('',(#5036),#30316,.F.);
#32012=ADVANCED_FACE('',(#5037),#1986,.T.);
#32013=ADVANCED_FACE('',(#5038),#1987,.T.);
#32014=ADVANCED_FACE('',(#5039),#1988,.T.);
#32015=ADVANCED_FACE('',(#5040),#1989,.T.);
#32016=ADVANCED_FACE('',(#5041),#1990,.T.);
#32017=ADVANCED_FACE('',(#5042),#1991,.T.);
#32018=ADVANCED_FACE('',(#5043),#3320,.F.);
#32019=ADVANCED_FACE('',(#5044),#3321,.F.);
#32020=ADVANCED_FACE('',(#5045),#3322,.F.);
#32021=ADVANCED_FACE('',(#5046),#3323,.F.);
#32022=ADVANCED_FACE('',(#5047),#3324,.F.);
#32023=ADVANCED_FACE('',(#5048),#3325,.F.);
#32024=ADVANCED_FACE('',(#5049),#3326,.F.);
#32025=ADVANCED_FACE('',(#5050),#3327,.F.);
#32026=ADVANCED_FACE('',(#5051),#3328,.F.);
#32027=ADVANCED_FACE('',(#5052),#3329,.F.);
#32028=ADVANCED_FACE('',(#5053),#3330,.F.);
#32029=ADVANCED_FACE('',(#5054),#3331,.F.);
#32030=ADVANCED_FACE('',(#5055),#3332,.F.);
#32031=ADVANCED_FACE('',(#5056),#3333,.F.);
#32032=ADVANCED_FACE('',(#5057),#3334,.F.);
#32033=ADVANCED_FACE('',(#5058),#30317,.F.);
#32034=ADVANCED_FACE('',(#5059),#3335,.F.);
#32035=ADVANCED_FACE('',(#5060),#3336,.F.);
#32036=ADVANCED_FACE('',(#5061),#3337,.F.);
#32037=ADVANCED_FACE('',(#5062),#1992,.T.);
#32038=ADVANCED_FACE('',(#5063),#1993,.T.);
#32039=ADVANCED_FACE('',(#5064),#1994,.T.);
#32040=ADVANCED_FACE('',(#5065),#1995,.T.);
#32041=ADVANCED_FACE('',(#5066),#1996,.T.);
#32042=ADVANCED_FACE('',(#5067),#1997,.T.);
#32043=ADVANCED_FACE('',(#5068),#1998,.T.);
#32044=ADVANCED_FACE('',(#5069),#1999,.T.);
#32045=ADVANCED_FACE('',(#5070),#2000,.T.);
#32046=ADVANCED_FACE('',(#5071),#2001,.T.);
#32047=ADVANCED_FACE('',(#5072),#2002,.T.);
#32048=ADVANCED_FACE('',(#5073),#2003,.T.);
#32049=ADVANCED_FACE('',(#5074),#2004,.T.);
#32050=ADVANCED_FACE('',(#5075),#2005,.T.);
#32051=ADVANCED_FACE('',(#5076),#2006,.T.);
#32052=ADVANCED_FACE('',(#5077),#2007,.T.);
#32053=ADVANCED_FACE('',(#5078),#2008,.T.);
#32054=ADVANCED_FACE('',(#5079),#2009,.T.);
#32055=ADVANCED_FACE('',(#5080),#2010,.T.);
#32056=ADVANCED_FACE('',(#5081),#2011,.T.);
#32057=ADVANCED_FACE('',(#5082),#2012,.T.);
#32058=ADVANCED_FACE('',(#5083),#2013,.T.);
#32059=ADVANCED_FACE('',(#5084),#2014,.T.);
#32060=ADVANCED_FACE('',(#5085),#615,.F.);
#32061=ADVANCED_FACE('',(#5086),#3338,.F.);
#32062=ADVANCED_FACE('',(#5087),#616,.F.);
#32063=ADVANCED_FACE('',(#5088),#99,.F.);
#32064=ADVANCED_FACE('',(#5089,#2231),#3339,.T.);
#32065=ADVANCED_FACE('',(#5090),#3340,.F.);
#32066=ADVANCED_FACE('',(#5091),#3341,.F.);
#32067=ADVANCED_FACE('',(#5092),#3342,.F.);
#32068=ADVANCED_FACE('',(#5093),#2015,.T.);
#32069=ADVANCED_FACE('',(#5094),#3343,.T.);
#32070=ADVANCED_FACE('',(#5095),#3344,.T.);
#32071=ADVANCED_FACE('',(#5096),#30318,.T.);
#32072=ADVANCED_FACE('',(#5097),#3345,.T.);
#32073=ADVANCED_FACE('',(#5098),#30319,.F.);
#32074=ADVANCED_FACE('',(#5099),#30320,.T.);
#32075=CLOSED_SHELL('',(#30321,#30322,#30323,#30324,#30325,#30326,#30327,
#30328,#30329,#30330,#30331,#30332,#30333,#30334,#30335,#30336,#30337,#30338,
#30339,#30340,#30341,#30342,#30343,#30344,#30345,#30346,#30347,#30348,#30349,
#30350));
#32076=CLOSED_SHELL('',(#30351,#30352,#30353,#30354,#30355,#30356,#30357,
#30358,#30359,#30360,#30361,#30362,#30363,#30364,#30365,#30366,#30367,#30368,
#30369,#30370,#30371,#30372,#30373,#30374,#30375,#30376,#30377,#30378,#30379,
#30380,#30381,#30382,#30383,#30384,#30385,#30386,#30387,#30388,#30389,#30390,
#30391,#30392,#30393,#30394,#30395,#30396,#30397,#30398,#30399,#30400,#30401,
#30402,#30403,#30404,#30405,#30406,#30407,#30408,#30409));
#32077=CLOSED_SHELL('',(#30410,#30411,#30412,#30413,#30414,#30415,#30416,
#30417));
#32078=CLOSED_SHELL('',(#30418,#30419,#30420,#30421,#30422,#30423,#30424,
#30425,#30426,#30427,#30428,#30429,#30430,#30431,#30432,#30433,#30434,#30435,
#30436,#30437,#30438,#30439,#30440,#30441,#30442,#30443,#30444,#30445,#30446,
#30447,#30448,#30449,#30450,#30451,#30452,#30453,#30454,#30455,#30456,#30457,
#30458,#30459,#30460,#30461,#30462,#30463,#30464,#30465,#30466,#30467,#30468,
#30469,#30470,#30471,#30472,#30473,#30474,#30475,#30476,#30477,#30478,#30479,
#30480,#30481,#30482,#30483,#30484,#30485,#30486,#30487,#30488,#30489,#30490,
#30491,#30492,#30493,#30494,#30495,#30496,#30497,#30498,#30499,#30500,#30501,
#30502,#30503,#30504,#30505,#30506));
#32079=CLOSED_SHELL('',(#30507,#30508,#30509,#30510,#30511,#30512,#30513,
#30514,#30515,#30516,#30517,#30518,#30519,#30520,#30521,#30522,#30523,#30524,
#30525,#30526,#30527,#30528,#30529,#30530,#30531,#30532,#30533,#30534,#30535,
#30536,#30537,#30538,#30539,#30540,#30541,#30542,#30543,#30544,#30545,#30546,
#30547,#30548,#30549,#30550,#30551,#30552,#30553,#30554,#30555,#30556,#30557,
#30558,#30559,#30560,#30561,#30562,#30563,#30564,#30565,#30566,#30567,#30568,
#30569,#30570,#30571,#30572,#30573,#30574,#30575,#30576,#30577,#30578,#30579,
#30580,#30581,#30582,#30583,#30584,#30585,#30586,#30587,#30588,#30589,#30590,
#30591,#30592,#30593,#30594,#30595,#30596,#30597,#30598,#30599,#30600,#30601,
#30602,#30603,#30604,#30605,#30606,#30607,#30608,#30609,#30610,#30611,#30612,
#30613,#30614,#30615,#30616,#30617,#30618,#30619,#30620,#30621,#30622,#30623,
#30624,#30625,#30626,#30627,#30628,#30629,#30630,#30631,#30632,#30633,#30634,
#30635,#30636,#30637,#30638,#30639,#30640,#30641,#30642,#30643,#30644,#30645,
#30646,#30647,#30648,#30649,#30650,#30651,#30652,#30653,#30654,#30655,#30656,
#30657,#30658,#30659,#30660,#30661,#30662,#30663,#30664,#30665,#30666,#30667,
#30668,#30669,#30670,#30671,#30672,#30673,#30674,#30675,#30676,#30677,#30678,
#30679,#30680,#30681,#30682));
#32080=CLOSED_SHELL('',(#30683,#30684,#30685,#30686,#30687,#30688,#30689,
#30690,#30691,#30692,#30693,#30694,#30695,#30696,#30697,#30698,#30699,#30700,
#30701,#30702,#30703,#30704,#30705,#30706,#30707,#30708,#30709,#30710,#30711,
#30712,#30713,#30714,#30715,#30716,#30717,#30718,#30719,#30720,#30721,#30722,
#30723,#30724,#30725,#30726,#30727,#30728,#30729,#30730,#30731,#30732,#30733,
#30734,#30735,#30736,#30737,#30738,#30739,#30740,#30741,#30742,#30743,#30744,
#30745,#30746,#30747,#30748,#30749,#30750,#30751,#30752,#30753,#30754,#30755,
#30756,#30757,#30758,#30759,#30760,#30761,#30762,#30763,#30764,#30765,#30766,
#30767,#30768,#30769,#30770,#30771,#30772,#30773,#30774,#30775,#30776,#30777,
#30778,#30779,#30780,#30781,#30782,#30783,#30784,#30785,#30786,#30787,#30788,
#30789,#30790,#30791,#30792,#30793,#30794,#30795,#30796,#30797,#30798,#30799,
#30800,#30801,#30802,#30803,#30804,#30805,#30806,#30807,#30808,#30809,#30810,
#30811,#30812,#30813,#30814,#30815,#30816,#30817,#30818,#30819,#30820,#30821,
#30822,#30823,#30824,#30825,#30826,#30827,#30828,#30829,#30830,#30831,#30832,
#30833,#30834,#30835,#30836,#30837,#30838,#30839,#30840,#30841,#30842,#30843,
#30844,#30845,#30846,#30847,#30848,#30849,#30850,#30851,#30852,#30853,#30854,
#30855,#30856,#30857,#30858,#30859,#30860,#30861,#30862,#30863,#30864,#30865,
#30866,#30867,#30868,#30869,#30870,#30871,#30872,#30873,#30874,#30875,#30876,
#30877,#30878,#30879,#30880,#30881,#30882,#30883,#30884,#30885,#30886,#30887,
#30888,#30889,#30890,#30891,#30892,#30893,#30894,#30895,#30896,#30897,#30898,
#30899,#30900,#30901,#30902,#30903,#30904,#30905,#30906,#30907,#30908,#30909,
#30910,#30911,#30912,#30913,#30914,#30915,#30916,#30917,#30918,#30919,#30920,
#30921,#30922,#30923,#30924,#30925,#30926,#30927,#30928,#30929,#30930,#30931,
#30932,#30933,#30934,#30935,#30936,#30937,#30938,#30939,#30940,#30941,#30942,
#30943,#30944,#30945,#30946,#30947,#30948,#30949,#30950,#30951,#30952,#30953,
#30954,#30955,#30956,#30957,#30958,#30959,#30960,#30961,#30962,#30963,#30964,
#30965,#30966,#30967,#30968,#30969,#30970,#30971,#30972,#30973,#30974,#30975,
#30976,#30977,#30978,#30979,#30980,#30981,#30982,#30983,#30984,#30985,#30986,
#30987,#30988,#30989,#30990,#30991,#30992,#30993,#30994,#30995,#30996,#30997,
#30998,#30999,#31000,#31001,#31002,#31003,#31004,#31005,#31006,#31007,#31008,
#31009,#31010,#31011,#31012,#31013,#31014,#31015,#31016,#31017,#31018,#31019,
#31020,#31021,#31022,#31023,#31024,#31025,#31026,#31027,#31028,#31029,#31030,
#31031,#31032,#31033,#31034,#31035,#31036,#31037,#31038,#31039,#31040,#31041,
#31042,#31043,#31044,#31045,#31046,#31047,#31048,#31049,#31050,#31051,#31052,
#31053,#31054,#31055,#31056,#31057,#31058,#31059,#31060,#31061,#31062,#31063,
#31064,#31065,#31066,#31067,#31068,#31069,#31070,#31071,#31072,#31073,#31074,
#31075,#31076,#31077,#31078,#31079,#31080,#31081,#31082,#31083,#31084,#31085,
#31086,#31087,#31088,#31089,#31090,#31091,#31092,#31093,#31094,#31095,#31096,
#31097,#31098,#31099,#31100,#31101,#31102,#31103,#31104,#31105,#31106,#31107,
#31108,#31109,#31110,#31111,#31112,#31113,#31114,#31115,#31116,#31117,#31118,
#31119,#31120,#31121,#31122,#31123,#31124,#31125,#31126,#31127,#31128,#31129,
#31130,#31131,#31132,#31133,#31134,#31135,#31136,#31137,#31138,#31139,#31140,
#31141,#31142,#31143,#31144,#31145,#31146,#31147,#31148,#31149,#31150,#31151,
#31152,#31153,#31154,#31155,#31156,#31157,#31158,#31159,#31160,#31161,#31162,
#31163,#31164,#31165,#31166,#31167,#31168,#31169,#31170,#31171,#31172,#31173,
#31174,#31175,#31176,#31177,#31178,#31179,#31180,#31181,#31182,#31183,#31184,
#31185,#31186,#31187,#31188,#31189,#31190,#31191,#31192,#31193,#31194,#31195,
#31196,#31197,#31198,#31199,#31200,#31201,#31202,#31203,#31204,#31205,#31206,
#31207,#31208,#31209,#31210,#31211,#31212,#31213,#31214,#31215,#31216,#31217,
#31218,#31219,#31220,#31221,#31222,#31223,#31224,#31225,#31226,#31227,#31228,
#31229,#31230,#31231,#31232,#31233,#31234,#31235,#31236,#31237,#31238,#31239,
#31240,#31241,#31242,#31243,#31244,#31245,#31246,#31247,#31248,#31249,#31250,
#31251,#31252,#31253,#31254,#31255,#31256,#31257,#31258,#31259,#31260,#31261,
#31262,#31263,#31264,#31265,#31266,#31267,#31268,#31269,#31270,#31271,#31272,
#31273,#31274,#31275,#31276,#31277,#31278,#31279,#31280,#31281,#31282,#31283,
#31284,#31285,#31286,#31287,#31288,#31289,#31290,#31291,#31292,#31293,#31294,
#31295,#31296,#31297,#31298,#31299,#31300,#31301,#31302,#31303,#31304,#31305,
#31306,#31307,#31308,#31309,#31310,#31311,#31312,#31313,#31314,#31315,#31316,
#31317,#31318,#31319,#31320,#31321,#31322,#31323,#31324,#31325,#31326,#31327,
#31328,#31329,#31330,#31331,#31332,#31333,#31334,#31335,#31336,#31337,#31338,
#31339,#31340,#31341,#31342,#31343,#31344,#31345,#31346,#31347,#31348,#31349,
#31350,#31351,#31352,#31353,#31354,#31355,#31356,#31357,#31358,#31359,#31360,
#31361,#31362,#31363,#31364,#31365,#31366,#31367,#31368,#31369,#31370,#31371,
#31372,#31373,#31374,#31375,#31376,#31377,#31378,#31379,#31380,#31381,#31382,
#31383,#31384,#31385,#31386,#31387,#31388,#31389,#31390,#31391,#31392,#31393,
#31394,#31395,#31396,#31397,#31398,#31399,#31400,#31401,#31402,#31403,#31404,
#31405,#31406,#31407,#31408,#31409,#31410,#31411,#31412,#31413,#31414,#31415,
#31416,#31417,#31418,#31419,#31420,#31421,#31422,#31423,#31424,#31425,#31426,
#31427,#31428,#31429,#31430,#31431,#31432,#31433,#31434,#31435,#31436,#31437,
#31438,#31439,#31440,#31441,#31442,#31443,#31444,#31445,#31446,#31447,#31448,
#31449,#31450,#31451,#31452,#31453,#31454,#31455,#31456,#31457,#31458,#31459,
#31460,#31461,#31462,#31463,#31464,#31465,#31466,#31467,#31468,#31469,#31470,
#31471,#31472,#31473,#31474,#31475,#31476,#31477));
#32081=CLOSED_SHELL('',(#31478,#31479,#31480,#31481,#31482,#31483,#31484,
#31485,#31486,#31487,#31488,#31489,#31490,#31491,#31492,#31493,#31494,#31495,
#31496,#31497,#31498,#31499,#31500,#31501,#31502,#31503,#31504,#31505,#31506,
#31507,#31508,#31509,#31510,#31511,#31512,#31513,#31514,#31515,#31516,#31517,
#31518,#31519,#31520,#31521,#31522,#31523,#31524,#31525,#31526,#31527,#31528,
#31529,#31530,#31531,#31532,#31533,#31534,#31535,#31536,#31537,#31538,#31539,
#31540,#31541,#31542,#31543,#31544));
#32082=CLOSED_SHELL('',(#31545,#31546,#31547,#31548,#31549,#31550,#31551,
#31552,#31553,#31554,#31555,#31556,#31557,#31558,#31559,#31560,#31561,#31562,
#31563,#31564,#31565,#31566,#31567,#31568,#31569,#31570));
#32083=CLOSED_SHELL('',(#31571,#31572,#31573,#31574,#31575,#31576,#31577,
#31578,#31579,#31580,#31581,#31582,#31583,#31584,#31585,#31586,#31587,#31588,
#31589,#31590,#31591,#31592,#31593,#31594,#31595,#31596,#31597,#31598,#31599,
#31600,#31601,#31602,#31603,#31604,#31605,#31606,#31607,#31608,#31609,#31610,
#31611,#31612,#31613,#31614,#31615,#31616,#31617,#31618,#31619,#31620,#31621,
#31622,#31623));
#32084=CLOSED_SHELL('',(#31624,#31625,#31626,#31627,#31628,#31629,#31630,
#31631,#31632,#31633,#31634,#31635,#31636,#31637,#31638,#31639,#31640,#31641,
#31642,#31643,#31644,#31645,#31646,#31647,#31648,#31649,#31650,#31651,#31652,
#31653,#31654,#31655,#31656));
#32085=CLOSED_SHELL('',(#31657,#31658,#31659,#31660,#31661,#31662,#31663,
#31664,#31665,#31666,#31667,#31668,#31669,#31670,#31671,#31672,#31673,#31674,
#31675,#31676,#31677,#31678,#31679,#31680,#31681,#31682,#31683,#31684,#31685,
#31686,#31687,#31688,#31689,#31690,#31691,#31692,#31693,#31694,#31695,#31696,
#31697,#31698,#31699,#31700,#31701,#31702,#31703,#31704,#31705,#31706,#31707,
#31708,#31709,#31710,#31711,#31712,#31713,#31714,#31715,#31716,#31717,#31718,
#31719,#31720,#31721,#31722,#31723,#31724,#31725,#31726,#31727,#31728,#31729,
#31730,#31731,#31732,#31733,#31734,#31735,#31736,#31737,#31738,#31739,#31740,
#31741,#31742,#31743,#31744,#31745,#31746,#31747,#31748,#31749,#31750,#31751,
#31752,#31753,#31754,#31755,#31756,#31757,#31758,#31759,#31760,#31761,#31762,
#31763,#31764,#31765,#31766,#31767,#31768,#31769,#31770,#31771,#31772,#31773,
#31774,#31775,#31776,#31777,#31778,#31779,#31780,#31781,#31782,#31783,#31784,
#31785,#31786,#31787,#31788,#31789,#31790,#31791,#31792,#31793,#31794,#31795,
#31796,#31797,#31798,#31799,#31800,#31801,#31802,#31803,#31804,#31805,#31806,
#31807,#31808,#31809,#31810,#31811,#31812,#31813,#31814,#31815,#31816,#31817,
#31818,#31819,#31820,#31821,#31822,#31823,#31824,#31825,#31826,#31827,#31828,
#31829,#31830,#31831,#31832,#31833,#31834,#31835,#31836,#31837,#31838,#31839,
#31840,#31841,#31842,#31843,#31844,#31845,#31846,#31847,#31848,#31849,#31850));
#32086=CLOSED_SHELL('',(#31851,#31852,#31853,#31854,#31855,#31856,#31857,
#31858,#31859,#31860,#31861,#31862,#31863,#31864,#31865,#31866,#31867,#31868,
#31869,#31870,#31871,#31872,#31873,#31874,#31875,#31876,#31877,#31878,#31879,
#31880,#31881,#31882,#31883,#31884,#31885,#31886,#31887,#31888,#31889,#31890,
#31891,#31892,#31893,#31894,#31895,#31896,#31897,#31898,#31899,#31900,#31901,
#31902,#31903,#31904,#31905,#31906,#31907,#31908,#31909,#31910,#31911,#31912,
#31913,#31914,#31915,#31916,#31917,#31918,#31919,#31920,#31921,#31922,#31923,
#31924,#31925,#31926,#31927,#31928,#31929,#31930,#31931,#31932,#31933,#31934,
#31935,#31936,#31937,#31938,#31939,#31940,#31941,#31942,#31943,#31944,#31945,
#31946,#31947,#31948,#31949,#31950,#31951,#31952,#31953,#31954,#31955,#31956,
#31957,#31958,#31959,#31960,#31961,#31962,#31963,#31964,#31965,#31966,#31967,
#31968,#31969,#31970,#31971,#31972,#31973,#31974,#31975,#31976,#31977,#31978,
#31979,#31980,#31981,#31982,#31983,#31984,#31985,#31986,#31987,#31988,#31989,
#31990,#31991,#31992,#31993,#31994,#31995,#31996,#31997,#31998,#31999,#32000,
#32001,#32002,#32003,#32004,#32005,#32006,#32007,#32008,#32009,#32010,#32011,
#32012,#32013,#32014,#32015,#32016,#32017,#32018,#32019,#32020,#32021,#32022,
#32023,#32024,#32025,#32026,#32027,#32028,#32029,#32030,#32031,#32032,#32033,
#32034,#32035,#32036));
#32087=CLOSED_SHELL('',(#32037,#32038,#32039,#32040,#32041,#32042,#32043,
#32044,#32045,#32046,#32047,#32048,#32049,#32050,#32051,#32052,#32053,#32054,
#32055,#32056,#32057,#32058,#32059,#32060,#32061,#32062,#32063,#32064,#32065,
#32066,#32067,#32068,#32069,#32070,#32071,#32072,#32073,#32074));
#32088=DERIVED_UNIT_ELEMENT(#32114,1.);
#32089=DERIVED_UNIT_ELEMENT(#135284,-3.);
#32090=DERIVED_UNIT_ELEMENT(#32114,1.);
#32091=DERIVED_UNIT_ELEMENT(#135284,-3.);
#32092=DERIVED_UNIT_ELEMENT(#32114,1.);
#32093=DERIVED_UNIT_ELEMENT(#135284,-3.);
#32094=DERIVED_UNIT_ELEMENT(#32114,1.);
#32095=DERIVED_UNIT_ELEMENT(#135284,-3.);
#32096=DERIVED_UNIT_ELEMENT(#32114,1.);
#32097=DERIVED_UNIT_ELEMENT(#135284,-3.);
#32098=DERIVED_UNIT_ELEMENT(#32114,1.);
#32099=DERIVED_UNIT_ELEMENT(#135284,-3.);
#32100=DERIVED_UNIT_ELEMENT(#32114,1.);
#32101=DERIVED_UNIT_ELEMENT(#135284,-3.);
#32102=DERIVED_UNIT_ELEMENT(#32114,1.);
#32103=DERIVED_UNIT_ELEMENT(#135284,-3.);
#32104=DERIVED_UNIT_ELEMENT(#32114,1.);
#32105=DERIVED_UNIT_ELEMENT(#135284,-3.);
#32106=DERIVED_UNIT_ELEMENT(#32114,1.);
#32107=DERIVED_UNIT_ELEMENT(#135284,-3.);
#32108=DERIVED_UNIT_ELEMENT(#32114,1.);
#32109=DERIVED_UNIT_ELEMENT(#135284,-3.);
#32110=DERIVED_UNIT_ELEMENT(#32114,1.);
#32111=DERIVED_UNIT_ELEMENT(#135284,-3.);
#32112=DERIVED_UNIT_ELEMENT(#32114,1.);
#32113=DERIVED_UNIT_ELEMENT(#135284,-3.);
#32114=(
MASS_UNIT()
NAMED_UNIT(*)
SI_UNIT(.KILO.,.GRAM.)
);
#32115=DERIVED_UNIT((#32088,#32089));
#32116=DERIVED_UNIT((#32090,#32091));
#32117=DERIVED_UNIT((#32092,#32093));
#32118=DERIVED_UNIT((#32094,#32095));
#32119=DERIVED_UNIT((#32096,#32097));
#32120=DERIVED_UNIT((#32098,#32099));
#32121=DERIVED_UNIT((#32100,#32101));
#32122=DERIVED_UNIT((#32102,#32103));
#32123=DERIVED_UNIT((#32104,#32105));
#32124=DERIVED_UNIT((#32106,#32107));
#32125=DERIVED_UNIT((#32108,#32109));
#32126=DERIVED_UNIT((#32110,#32111));
#32127=DERIVED_UNIT((#32112,#32113));
#32128=MEASURE_REPRESENTATION_ITEM('density measure',
POSITIVE_RATIO_MEASURE(7850.),#32115);
#32129=MEASURE_REPRESENTATION_ITEM('density measure',
POSITIVE_RATIO_MEASURE(7850.),#32116);
#32130=MEASURE_REPRESENTATION_ITEM('density measure',
POSITIVE_RATIO_MEASURE(7850.),#32117);
#32131=MEASURE_REPRESENTATION_ITEM('density measure',
POSITIVE_RATIO_MEASURE(7850.),#32118);
#32132=MEASURE_REPRESENTATION_ITEM('density measure',
POSITIVE_RATIO_MEASURE(7850.),#32119);
#32133=MEASURE_REPRESENTATION_ITEM('density measure',
POSITIVE_RATIO_MEASURE(7850.),#32120);
#32134=MEASURE_REPRESENTATION_ITEM('density measure',
POSITIVE_RATIO_MEASURE(7850.),#32121);
#32135=MEASURE_REPRESENTATION_ITEM('density measure',
POSITIVE_RATIO_MEASURE(7850.),#32122);
#32136=MEASURE_REPRESENTATION_ITEM('density measure',
POSITIVE_RATIO_MEASURE(7850.),#32123);
#32137=MEASURE_REPRESENTATION_ITEM('density measure',
POSITIVE_RATIO_MEASURE(7850.),#32124);
#32138=MEASURE_REPRESENTATION_ITEM('density measure',
POSITIVE_RATIO_MEASURE(7850.),#32125);
#32139=MEASURE_REPRESENTATION_ITEM('density measure',
POSITIVE_RATIO_MEASURE(7850.),#32126);
#32140=MEASURE_REPRESENTATION_ITEM('density measure',
POSITIVE_RATIO_MEASURE(7850.),#32127);
#32141=PROPERTY_DEFINITION_REPRESENTATION(#32206,#32167);
#32142=PROPERTY_DEFINITION_REPRESENTATION(#32207,#32168);
#32143=PROPERTY_DEFINITION_REPRESENTATION(#32208,#32169);
#32144=PROPERTY_DEFINITION_REPRESENTATION(#32209,#32170);
#32145=PROPERTY_DEFINITION_REPRESENTATION(#32210,#32171);
#32146=PROPERTY_DEFINITION_REPRESENTATION(#32211,#32172);
#32147=PROPERTY_DEFINITION_REPRESENTATION(#32212,#32173);
#32148=PROPERTY_DEFINITION_REPRESENTATION(#32213,#32174);
#32149=PROPERTY_DEFINITION_REPRESENTATION(#32214,#32175);
#32150=PROPERTY_DEFINITION_REPRESENTATION(#32215,#32176);
#32151=PROPERTY_DEFINITION_REPRESENTATION(#32216,#32177);
#32152=PROPERTY_DEFINITION_REPRESENTATION(#32217,#32178);
#32153=PROPERTY_DEFINITION_REPRESENTATION(#32218,#32179);
#32154=PROPERTY_DEFINITION_REPRESENTATION(#32219,#32180);
#32155=PROPERTY_DEFINITION_REPRESENTATION(#32220,#32181);
#32156=PROPERTY_DEFINITION_REPRESENTATION(#32221,#32182);
#32157=PROPERTY_DEFINITION_REPRESENTATION(#32222,#32183);
#32158=PROPERTY_DEFINITION_REPRESENTATION(#32223,#32184);
#32159=PROPERTY_DEFINITION_REPRESENTATION(#32224,#32185);
#32160=PROPERTY_DEFINITION_REPRESENTATION(#32225,#32186);
#32161=PROPERTY_DEFINITION_REPRESENTATION(#32226,#32187);
#32162=PROPERTY_DEFINITION_REPRESENTATION(#32227,#32188);
#32163=PROPERTY_DEFINITION_REPRESENTATION(#32228,#32189);
#32164=PROPERTY_DEFINITION_REPRESENTATION(#32229,#32190);
#32165=PROPERTY_DEFINITION_REPRESENTATION(#32230,#32191);
#32166=PROPERTY_DEFINITION_REPRESENTATION(#32231,#32192);
#32167=REPRESENTATION('material name',(#32193),#135269);
#32168=REPRESENTATION('density',(#32128),#135269);
#32169=REPRESENTATION('material name',(#32194),#135270);
#32170=REPRESENTATION('density',(#32129),#135270);
#32171=REPRESENTATION('material name',(#32195),#135271);
#32172=REPRESENTATION('density',(#32130),#135271);
#32173=REPRESENTATION('material name',(#32196),#135272);
#32174=REPRESENTATION('density',(#32131),#135272);
#32175=REPRESENTATION('material name',(#32197),#135273);
#32176=REPRESENTATION('density',(#32132),#135273);
#32177=REPRESENTATION('material name',(#32198),#135274);
#32178=REPRESENTATION('density',(#32133),#135274);
#32179=REPRESENTATION('material name',(#32199),#135275);
#32180=REPRESENTATION('density',(#32134),#135275);
#32181=REPRESENTATION('material name',(#32200),#135276);
#32182=REPRESENTATION('density',(#32135),#135276);
#32183=REPRESENTATION('material name',(#32201),#135277);
#32184=REPRESENTATION('density',(#32136),#135277);
#32185=REPRESENTATION('material name',(#32202),#135278);
#32186=REPRESENTATION('density',(#32137),#135278);
#32187=REPRESENTATION('material name',(#32203),#135279);
#32188=REPRESENTATION('density',(#32138),#135279);
#32189=REPRESENTATION('material name',(#32204),#135280);
#32190=REPRESENTATION('density',(#32139),#135280);
#32191=REPRESENTATION('material name',(#32205),#135281);
#32192=REPRESENTATION('density',(#32140),#135281);
#32193=DESCRIPTIVE_REPRESENTATION_ITEM('Steel','Steel');
#32194=DESCRIPTIVE_REPRESENTATION_ITEM('Steel','Steel');
#32195=DESCRIPTIVE_REPRESENTATION_ITEM('Steel','Steel');
#32196=DESCRIPTIVE_REPRESENTATION_ITEM('Steel','Steel');
#32197=DESCRIPTIVE_REPRESENTATION_ITEM('Steel','Steel');
#32198=DESCRIPTIVE_REPRESENTATION_ITEM('Steel','Steel');
#32199=DESCRIPTIVE_REPRESENTATION_ITEM('Steel','Steel');
#32200=DESCRIPTIVE_REPRESENTATION_ITEM('Steel','Steel');
#32201=DESCRIPTIVE_REPRESENTATION_ITEM('Steel','Steel');
#32202=DESCRIPTIVE_REPRESENTATION_ITEM('Steel','Steel');
#32203=DESCRIPTIVE_REPRESENTATION_ITEM('Steel','Steel');
#32204=DESCRIPTIVE_REPRESENTATION_ITEM('Steel','Steel');
#32205=DESCRIPTIVE_REPRESENTATION_ITEM('Steel','Steel');
#32206=PROPERTY_DEFINITION('material property','material name',#135352);
#32207=PROPERTY_DEFINITION('material property','density of part',#135352);
#32208=PROPERTY_DEFINITION('material property','material name',#135353);
#32209=PROPERTY_DEFINITION('material property','density of part',#135353);
#32210=PROPERTY_DEFINITION('material property','material name',#135354);
#32211=PROPERTY_DEFINITION('material property','density of part',#135354);
#32212=PROPERTY_DEFINITION('material property','material name',#135355);
#32213=PROPERTY_DEFINITION('material property','density of part',#135355);
#32214=PROPERTY_DEFINITION('material property','material name',#135356);
#32215=PROPERTY_DEFINITION('material property','density of part',#135356);
#32216=PROPERTY_DEFINITION('material property','material name',#135357);
#32217=PROPERTY_DEFINITION('material property','density of part',#135357);
#32218=PROPERTY_DEFINITION('material property','material name',#135358);
#32219=PROPERTY_DEFINITION('material property','density of part',#135358);
#32220=PROPERTY_DEFINITION('material property','material name',#135359);
#32221=PROPERTY_DEFINITION('material property','density of part',#135359);
#32222=PROPERTY_DEFINITION('material property','material name',#135360);
#32223=PROPERTY_DEFINITION('material property','density of part',#135360);
#32224=PROPERTY_DEFINITION('material property','material name',#135361);
#32225=PROPERTY_DEFINITION('material property','density of part',#135361);
#32226=PROPERTY_DEFINITION('material property','material name',#135362);
#32227=PROPERTY_DEFINITION('material property','density of part',#135362);
#32228=PROPERTY_DEFINITION('material property','material name',#135363);
#32229=PROPERTY_DEFINITION('material property','density of part',#135363);
#32230=PROPERTY_DEFINITION('material property','material name',#135364);
#32231=PROPERTY_DEFINITION('material property','density of part',#135364);
#32232=AXIS2_PLACEMENT_3D('',#41045,#34224,#34225);
#32233=AXIS2_PLACEMENT_3D('',#41046,#34226,#34227);
#32234=AXIS2_PLACEMENT_3D('',#41047,#34228,#34229);
#32235=AXIS2_PLACEMENT_3D('',#41049,#34230,#34231);
#32236=AXIS2_PLACEMENT_3D('',#41052,#34233,#34234);
#32237=AXIS2_PLACEMENT_3D('',#41053,#34235,#34236);
#32238=AXIS2_PLACEMENT_3D('',#41087,#34253,#34254);
#32239=AXIS2_PLACEMENT_3D('',#41088,#34255,#34256);
#32240=AXIS2_PLACEMENT_3D('',#41091,#34258,#34259);
#32241=AXIS2_PLACEMENT_3D('',#41092,#34260,#34261);
#32242=AXIS2_PLACEMENT_3D('',#41094,#34262,#34263);
#32243=AXIS2_PLACEMENT_3D('',#41096,#34265,#34266);
#32244=AXIS2_PLACEMENT_3D('',#41099,#34268,#34269);
#32245=AXIS2_PLACEMENT_3D('',#41100,#34270,#34271);
#32246=AXIS2_PLACEMENT_3D('',#41103,#34273,#34274);
#32247=AXIS2_PLACEMENT_3D('',#41106,#34276,#34277);
#32248=AXIS2_PLACEMENT_3D('',#41108,#34278,#34279);
#32249=AXIS2_PLACEMENT_3D('',#41111,#34281,#34282);
#32250=AXIS2_PLACEMENT_3D('',#41112,#34283,#34284);
#32251=AXIS2_PLACEMENT_3D('',#41146,#34301,#34302);
#32252=AXIS2_PLACEMENT_3D('',#41147,#34303,#34304);
#32253=AXIS2_PLACEMENT_3D('',#41150,#34306,#34307);
#32254=AXIS2_PLACEMENT_3D('',#41151,#34308,#34309);
#32255=AXIS2_PLACEMENT_3D('',#41153,#34310,#34311);
#32256=AXIS2_PLACEMENT_3D('',#41155,#34313,#34314);
#32257=AXIS2_PLACEMENT_3D('',#41158,#34316,#34317);
#32258=AXIS2_PLACEMENT_3D('',#41159,#34318,#34319);
#32259=AXIS2_PLACEMENT_3D('',#41162,#34321,#34322);
#32260=AXIS2_PLACEMENT_3D('',#41165,#34324,#34325);
#32261=AXIS2_PLACEMENT_3D('',#41168,#34328,#34329);
#32262=AXIS2_PLACEMENT_3D('',#41170,#34331,#34332);
#32263=AXIS2_PLACEMENT_3D('',#41173,#34335,#34336);
#32264=AXIS2_PLACEMENT_3D('',#41175,#34338,#34339);
#32265=AXIS2_PLACEMENT_3D('',#41177,#34341,#34342);
#32266=AXIS2_PLACEMENT_3D('',#41180,#34345,#34346);
#32267=AXIS2_PLACEMENT_3D('',#41182,#34348,#34349);
#32268=AXIS2_PLACEMENT_3D('',#41184,#34351,#34352);
#32269=AXIS2_PLACEMENT_3D('',#41186,#34354,#34355);
#32270=AXIS2_PLACEMENT_3D('',#41187,#34356,#34357);
#32271=AXIS2_PLACEMENT_3D('',#41188,#34358,#34359);
#32272=AXIS2_PLACEMENT_3D('',#41190,#34361,#34362);
#32273=AXIS2_PLACEMENT_3D('',#41192,#34364,#34365);
#32274=AXIS2_PLACEMENT_3D('',#41194,#34367,#34368);
#32275=AXIS2_PLACEMENT_3D('',#41196,#34370,#34371);
#32276=AXIS2_PLACEMENT_3D('',#41197,#34372,#34373);
#32277=AXIS2_PLACEMENT_3D('',#41198,#34374,#34375);
#32278=AXIS2_PLACEMENT_3D('',#41200,#34376,#34377);
#32279=AXIS2_PLACEMENT_3D('',#41203,#34379,#34380);
#32280=AXIS2_PLACEMENT_3D('',#41204,#34381,#34382);
#32281=AXIS2_PLACEMENT_3D('',#41214,#34387,#34388);
#32282=AXIS2_PLACEMENT_3D('',#41215,#34389,#34390);
#32283=AXIS2_PLACEMENT_3D('',#41219,#34392,#34393);
#32284=AXIS2_PLACEMENT_3D('',#41220,#34394,#34395);
#32285=AXIS2_PLACEMENT_3D('',#41221,#34396,#34397);
#32286=AXIS2_PLACEMENT_3D('',#41223,#34398,#34399);
#32287=AXIS2_PLACEMENT_3D('',#41225,#34401,#34402);
#32288=AXIS2_PLACEMENT_3D('',#41229,#34404,#34405);
#32289=AXIS2_PLACEMENT_3D('',#41230,#34406,#34407);
#32290=AXIS2_PLACEMENT_3D('',#41231,#34408,#34409);
#32291=AXIS2_PLACEMENT_3D('',#41234,#34411,#34412);
#32292=AXIS2_PLACEMENT_3D('',#41237,#34414,#34415);
#32293=AXIS2_PLACEMENT_3D('',#41239,#34416,#34417);
#32294=AXIS2_PLACEMENT_3D('',#41242,#34419,#34420);
#32295=AXIS2_PLACEMENT_3D('',#41243,#34421,#34422);
#32296=AXIS2_PLACEMENT_3D('',#41253,#34427,#34428);
#32297=AXIS2_PLACEMENT_3D('',#41255,#34429,#34430);
#32298=AXIS2_PLACEMENT_3D('',#41257,#34431,#34432);
#32299=AXIS2_PLACEMENT_3D('',#41259,#34433,#34434);
#32300=AXIS2_PLACEMENT_3D('',#41261,#34435,#34436);
#32301=AXIS2_PLACEMENT_3D('',#41263,#34437,#34438);
#32302=AXIS2_PLACEMENT_3D('',#41265,#34439,#34440);
#32303=AXIS2_PLACEMENT_3D('',#41267,#34441,#34442);
#32304=AXIS2_PLACEMENT_3D('',#41269,#34443,#34444);
#32305=AXIS2_PLACEMENT_3D('',#41270,#34445,#34446);
#32306=AXIS2_PLACEMENT_3D('',#41273,#34448,#34449);
#32307=AXIS2_PLACEMENT_3D('',#41274,#34450,#34451);
#32308=AXIS2_PLACEMENT_3D('',#41276,#34452,#34453);
#32309=AXIS2_PLACEMENT_3D('',#41278,#34455,#34456);
#32310=AXIS2_PLACEMENT_3D('',#41281,#34458,#34459);
#32311=AXIS2_PLACEMENT_3D('',#41282,#34460,#34461);
#32312=AXIS2_PLACEMENT_3D('',#41284,#34462,#34463);
#32313=AXIS2_PLACEMENT_3D('',#41286,#34465,#34466);
#32314=AXIS2_PLACEMENT_3D('',#41289,#34468,#34469);
#32315=AXIS2_PLACEMENT_3D('',#41290,#34470,#34471);
#32316=AXIS2_PLACEMENT_3D('',#41292,#34472,#34473);
#32317=AXIS2_PLACEMENT_3D('',#41294,#34475,#34476);
#32318=AXIS2_PLACEMENT_3D('',#41297,#34478,#34479);
#32319=AXIS2_PLACEMENT_3D('',#41298,#34480,#34481);
#32320=AXIS2_PLACEMENT_3D('',#41301,#34483,#34484);
#32321=AXIS2_PLACEMENT_3D('',#41304,#34486,#34487);
#32322=AXIS2_PLACEMENT_3D('',#41307,#34489,#34490);
#32323=AXIS2_PLACEMENT_3D('',#41310,#34492,#34493);
#32324=AXIS2_PLACEMENT_3D('',#41312,#34494,#34495);
#32325=AXIS2_PLACEMENT_3D('',#41314,#34497,#34498);
#32326=AXIS2_PLACEMENT_3D('',#41317,#34500,#34501);
#32327=AXIS2_PLACEMENT_3D('',#41318,#34502,#34503);
#32328=AXIS2_PLACEMENT_3D('',#41320,#34504,#34505);
#32329=AXIS2_PLACEMENT_3D('',#41322,#34507,#34508);
#32330=AXIS2_PLACEMENT_3D('',#41325,#34510,#34511);
#32331=AXIS2_PLACEMENT_3D('',#41326,#34512,#34513);
#32332=AXIS2_PLACEMENT_3D('',#41328,#34514,#34515);
#32333=AXIS2_PLACEMENT_3D('',#41330,#34517,#34518);
#32334=AXIS2_PLACEMENT_3D('',#41333,#34520,#34521);
#32335=AXIS2_PLACEMENT_3D('',#41334,#34522,#34523);
#32336=AXIS2_PLACEMENT_3D('',#41336,#34524,#34525);
#32337=AXIS2_PLACEMENT_3D('',#41338,#34527,#34528);
#32338=AXIS2_PLACEMENT_3D('',#41341,#34530,#34531);
#32339=AXIS2_PLACEMENT_3D('',#41342,#34532,#34533);
#32340=AXIS2_PLACEMENT_3D('',#41344,#34534,#34535);
#32341=AXIS2_PLACEMENT_3D('',#41346,#34537,#34538);
#32342=AXIS2_PLACEMENT_3D('',#41349,#34540,#34541);
#32343=AXIS2_PLACEMENT_3D('',#41350,#34542,#34543);
#32344=AXIS2_PLACEMENT_3D('',#41352,#34544,#34545);
#32345=AXIS2_PLACEMENT_3D('',#41354,#34547,#34548);
#32346=AXIS2_PLACEMENT_3D('',#41357,#34550,#34551);
#32347=AXIS2_PLACEMENT_3D('',#41358,#34552,#34553);
#32348=AXIS2_PLACEMENT_3D('',#41361,#34555,#34556);
#32349=AXIS2_PLACEMENT_3D('',#41364,#34558,#34559);
#32350=AXIS2_PLACEMENT_3D('',#41367,#34561,#34562);
#32351=AXIS2_PLACEMENT_3D('',#41370,#34564,#34565);
#32352=AXIS2_PLACEMENT_3D('',#41373,#34567,#34568);
#32353=AXIS2_PLACEMENT_3D('',#41376,#34570,#34571);
#32354=AXIS2_PLACEMENT_3D('',#41381,#34573,#34574);
#32355=AXIS2_PLACEMENT_3D('',#41384,#34576,#34577);
#32356=AXIS2_PLACEMENT_3D('',#41385,#34578,#34579);
#32357=AXIS2_PLACEMENT_3D('',#41392,#34584,#34585);
#32358=AXIS2_PLACEMENT_3D('',#41408,#34594,#34595);
#32359=AXIS2_PLACEMENT_3D('',#41412,#34597,#34598);
#32360=AXIS2_PLACEMENT_3D('',#41413,#34599,#34600);
#32361=AXIS2_PLACEMENT_3D('',#41414,#34601,#34602);
#32362=AXIS2_PLACEMENT_3D('',#41416,#34603,#34604);
#32363=AXIS2_PLACEMENT_3D('',#41418,#34606,#34607);
#32364=AXIS2_PLACEMENT_3D('',#41421,#34609,#34610);
#32365=AXIS2_PLACEMENT_3D('',#41422,#34611,#34612);
#32366=AXIS2_PLACEMENT_3D('',#41424,#34613,#34614);
#32367=AXIS2_PLACEMENT_3D('',#41425,#34615,#34616);
#32368=AXIS2_PLACEMENT_3D('',#41428,#34618,#34619);
#32369=AXIS2_PLACEMENT_3D('',#41429,#34620,#34621);
#32370=AXIS2_PLACEMENT_3D('',#41430,#34622,#34623);
#32371=AXIS2_PLACEMENT_3D('',#41435,#34627,#34628);
#32372=AXIS2_PLACEMENT_3D('',#41438,#34631,#34632);
#32373=AXIS2_PLACEMENT_3D('',#41440,#34634,#34635);
#32374=AXIS2_PLACEMENT_3D('',#41441,#34636,#34637);
#32375=AXIS2_PLACEMENT_3D('',#41444,#34640,#34641);
#32376=AXIS2_PLACEMENT_3D('',#41456,#34648,#34649);
#32377=AXIS2_PLACEMENT_3D('',#41460,#34652,#34653);
#32378=AXIS2_PLACEMENT_3D('',#41464,#34656,#34657);
#32379=AXIS2_PLACEMENT_3D('',#41468,#34660,#34661);
#32380=AXIS2_PLACEMENT_3D('',#41472,#34664,#34665);
#32381=AXIS2_PLACEMENT_3D('',#41476,#34668,#34669);
#32382=AXIS2_PLACEMENT_3D('',#41478,#34671,#34672);
#32383=AXIS2_PLACEMENT_3D('',#41479,#34673,#34674);
#32384=AXIS2_PLACEMENT_3D('',#41480,#34675,#34676);
#32385=AXIS2_PLACEMENT_3D('',#41481,#34677,#34678);
#32386=AXIS2_PLACEMENT_3D('',#41484,#34679,#34680);
#32387=AXIS2_PLACEMENT_3D('',#41487,#34682,#34683);
#32388=AXIS2_PLACEMENT_3D('',#41488,#34684,#34685);
#32389=AXIS2_PLACEMENT_3D('',#41489,#34686,#34687);
#32390=AXIS2_PLACEMENT_3D('',#41493,#34689,#34690);
#32391=AXIS2_PLACEMENT_3D('',#41494,#34691,#34692);
#32392=AXIS2_PLACEMENT_3D('',#41495,#34693,#34694);
#32393=AXIS2_PLACEMENT_3D('',#41497,#34695,#34696);
#32394=AXIS2_PLACEMENT_3D('',#41498,#34697,#34698);
#32395=AXIS2_PLACEMENT_3D('',#41501,#34700,#34701);
#32396=AXIS2_PLACEMENT_3D('',#41502,#34702,#34703);
#32397=AXIS2_PLACEMENT_3D('',#41504,#34704,#34705);
#32398=AXIS2_PLACEMENT_3D('',#41505,#34706,#34707);
#32399=AXIS2_PLACEMENT_3D('',#41507,#34708,#34709);
#32400=AXIS2_PLACEMENT_3D('',#41509,#34711,#34712);
#32401=AXIS2_PLACEMENT_3D('',#41511,#34713,#34714);
#32402=AXIS2_PLACEMENT_3D('',#41513,#34716,#34717);
#32403=AXIS2_PLACEMENT_3D('',#41515,#34719,#34720);
#32404=AXIS2_PLACEMENT_3D('',#41516,#34721,#34722);
#32405=AXIS2_PLACEMENT_3D('',#41520,#34724,#34725);
#32406=AXIS2_PLACEMENT_3D('',#41832,#34728,#34729);
#32407=AXIS2_PLACEMENT_3D('',#42030,#34731,#34732);
#32408=AXIS2_PLACEMENT_3D('',#42130,#34734,#34735);
#32409=AXIS2_PLACEMENT_3D('',#42296,#34737,#34738);
#32410=AXIS2_PLACEMENT_3D('',#42403,#34740,#34741);
#32411=AXIS2_PLACEMENT_3D('',#42498,#34743,#34744);
#32412=AXIS2_PLACEMENT_3D('',#42929,#34746,#34747);
#32413=AXIS2_PLACEMENT_3D('',#43020,#34749,#34750);
#32414=AXIS2_PLACEMENT_3D('',#43116,#34752,#34753);
#32415=AXIS2_PLACEMENT_3D('',#43308,#34755,#34756);
#32416=AXIS2_PLACEMENT_3D('',#43407,#34758,#34759);
#32417=AXIS2_PLACEMENT_3D('',#43583,#34761,#34762);
#32418=AXIS2_PLACEMENT_3D('',#43678,#34764,#34765);
#32419=AXIS2_PLACEMENT_3D('',#43771,#34767,#34768);
#32420=AXIS2_PLACEMENT_3D('',#43865,#34770,#34771);
#32421=AXIS2_PLACEMENT_3D('',#43951,#34773,#34774);
#32422=AXIS2_PLACEMENT_3D('',#44157,#34776,#34777);
#32423=AXIS2_PLACEMENT_3D('',#44313,#34779,#34780);
#32424=AXIS2_PLACEMENT_3D('',#44403,#34782,#34783);
#32425=AXIS2_PLACEMENT_3D('',#44503,#34785,#34786);
#32426=AXIS2_PLACEMENT_3D('',#44606,#34788,#34789);
#32427=AXIS2_PLACEMENT_3D('',#44898,#34791,#34792);
#32428=AXIS2_PLACEMENT_3D('',#45341,#34794,#34795);
#32429=AXIS2_PLACEMENT_3D('',#45429,#34797,#34798);
#32430=AXIS2_PLACEMENT_3D('',#45824,#34800,#34801);
#32431=AXIS2_PLACEMENT_3D('',#45917,#34803,#34804);
#32432=AXIS2_PLACEMENT_3D('',#46003,#34806,#34807);
#32433=AXIS2_PLACEMENT_3D('',#46103,#34809,#34810);
#32434=AXIS2_PLACEMENT_3D('',#46191,#34812,#34813);
#32435=AXIS2_PLACEMENT_3D('',#46511,#34815,#34816);
#32436=AXIS2_PLACEMENT_3D('',#46699,#34818,#34819);
#32437=AXIS2_PLACEMENT_3D('',#46794,#34821,#34822);
#32438=AXIS2_PLACEMENT_3D('',#46881,#34824,#34825);
#32439=AXIS2_PLACEMENT_3D('',#46991,#34827,#34828);
#32440=AXIS2_PLACEMENT_3D('',#47084,#34830,#34831);
#32441=AXIS2_PLACEMENT_3D('',#47184,#34833,#34834);
#32442=AXIS2_PLACEMENT_3D('',#47270,#34836,#34837);
#32443=AXIS2_PLACEMENT_3D('',#47614,#34839,#34840);
#32444=AXIS2_PLACEMENT_3D('',#47703,#34842,#34843);
#32445=AXIS2_PLACEMENT_3D('',#47823,#34845,#34846);
#32446=AXIS2_PLACEMENT_3D('',#47916,#34848,#34849);
#32447=AXIS2_PLACEMENT_3D('',#48050,#34851,#34852);
#32448=AXIS2_PLACEMENT_3D('',#48145,#34854,#34855);
#32449=AXIS2_PLACEMENT_3D('',#48245,#34857,#34858);
#32450=AXIS2_PLACEMENT_3D('',#48331,#34860,#34861);
#32451=AXIS2_PLACEMENT_3D('',#48430,#34863,#34864);
#32452=AXIS2_PLACEMENT_3D('',#48432,#34865,#34866);
#32453=AXIS2_PLACEMENT_3D('',#48581,#34870,#34871);
#32454=AXIS2_PLACEMENT_3D('',#48686,#34872,#34873);
#32455=AXIS2_PLACEMENT_3D('',#48689,#34874,#34875);
#32456=AXIS2_PLACEMENT_3D('',#48691,#34877,#34878);
#32457=AXIS2_PLACEMENT_3D('',#48694,#34879,#34880);
#32458=AXIS2_PLACEMENT_3D('',#48696,#34882,#34883);
#32459=AXIS2_PLACEMENT_3D('',#48699,#34886,#34887);
#32460=AXIS2_PLACEMENT_3D('',#68981,#34894,#34895);
#32461=AXIS2_PLACEMENT_3D('',#68982,#34896,#34897);
#32462=AXIS2_PLACEMENT_3D('',#68984,#34898,#34899);
#32463=AXIS2_PLACEMENT_3D('',#68985,#34900,#34901);
#32464=AXIS2_PLACEMENT_3D('',#68987,#34902,#34903);
#32465=AXIS2_PLACEMENT_3D('',#68989,#34905,#34906);
#32466=AXIS2_PLACEMENT_3D('',#68991,#34907,#34908);
#32467=AXIS2_PLACEMENT_3D('',#68993,#34910,#34911);
#32468=AXIS2_PLACEMENT_3D('',#68994,#34912,#34913);
#32469=AXIS2_PLACEMENT_3D('',#68997,#34915,#34916);
#32470=AXIS2_PLACEMENT_3D('',#68998,#34917,#34918);
#32471=AXIS2_PLACEMENT_3D('',#69000,#34919,#34920);
#32472=AXIS2_PLACEMENT_3D('',#69001,#34921,#34922);
#32473=AXIS2_PLACEMENT_3D('',#69003,#34923,#34924);
#32474=AXIS2_PLACEMENT_3D('',#69005,#34926,#34927);
#32475=AXIS2_PLACEMENT_3D('',#69008,#34929,#34930);
#32476=AXIS2_PLACEMENT_3D('',#69009,#34931,#34932);
#32477=AXIS2_PLACEMENT_3D('',#69010,#34933,#34934);
#32478=AXIS2_PLACEMENT_3D('',#69011,#34935,#34936);
#32479=AXIS2_PLACEMENT_3D('',#69021,#34937,#34938);
#32480=AXIS2_PLACEMENT_3D('',#69023,#34939,#34940);
#32481=AXIS2_PLACEMENT_3D('',#69032,#34941,#34942);
#32482=AXIS2_PLACEMENT_3D('',#69034,#34943,#34944);
#32483=AXIS2_PLACEMENT_3D('',#69043,#34945,#34946);
#32484=AXIS2_PLACEMENT_3D('',#69045,#34947,#34948);
#32485=AXIS2_PLACEMENT_3D('',#69059,#34949,#34950);
#32486=AXIS2_PLACEMENT_3D('',#69061,#34951,#34952);
#32487=AXIS2_PLACEMENT_3D('',#69070,#34953,#34954);
#32488=AXIS2_PLACEMENT_3D('',#69072,#34955,#34956);
#32489=AXIS2_PLACEMENT_3D('',#69081,#34957,#34958);
#32490=AXIS2_PLACEMENT_3D('',#69083,#34959,#34960);
#32491=AXIS2_PLACEMENT_3D('',#69137,#34962,#34963);
#32492=AXIS2_PLACEMENT_3D('',#69143,#34967,#34968);
#32493=AXIS2_PLACEMENT_3D('',#69147,#34971,#34972);
#32494=AXIS2_PLACEMENT_3D('',#69153,#34976,#34977);
#32495=AXIS2_PLACEMENT_3D('',#69159,#34981,#34982);
#32496=AXIS2_PLACEMENT_3D('',#69163,#34985,#34986);
#32497=AXIS2_PLACEMENT_3D('',#69167,#34989,#34990);
#32498=AXIS2_PLACEMENT_3D('',#69173,#34994,#34995);
#32499=AXIS2_PLACEMENT_3D('',#69179,#34999,#35000);
#32500=AXIS2_PLACEMENT_3D('',#69183,#35003,#35004);
#32501=AXIS2_PLACEMENT_3D('',#69187,#35007,#35008);
#32502=AXIS2_PLACEMENT_3D('',#69188,#35009,#35010);
#32503=AXIS2_PLACEMENT_3D('',#69189,#35011,#35012);
#32504=AXIS2_PLACEMENT_3D('',#69190,#35013,#35014);
#32505=AXIS2_PLACEMENT_3D('',#69191,#35015,#35016);
#32506=AXIS2_PLACEMENT_3D('',#69200,#35021,#35022);
#32507=AXIS2_PLACEMENT_3D('',#69202,#35023,#35024);
#32508=AXIS2_PLACEMENT_3D('',#69204,#35026,#35027);
#32509=AXIS2_PLACEMENT_3D('',#69208,#35030,#35031);
#32510=AXIS2_PLACEMENT_3D('',#69209,#35032,#35033);
#32511=AXIS2_PLACEMENT_3D('',#69210,#35034,#35035);
#32512=AXIS2_PLACEMENT_3D('',#69219,#35040,#35041);
#32513=AXIS2_PLACEMENT_3D('',#69221,#35042,#35043);
#32514=AXIS2_PLACEMENT_3D('',#69223,#35045,#35046);
#32515=AXIS2_PLACEMENT_3D('',#69227,#35049,#35050);
#32516=AXIS2_PLACEMENT_3D('',#69228,#35051,#35052);
#32517=AXIS2_PLACEMENT_3D('',#69229,#35053,#35054);
#32518=AXIS2_PLACEMENT_3D('',#69238,#35059,#35060);
#32519=AXIS2_PLACEMENT_3D('',#69240,#35061,#35062);
#32520=AXIS2_PLACEMENT_3D('',#69242,#35064,#35065);
#32521=AXIS2_PLACEMENT_3D('',#69246,#35068,#35069);
#32522=AXIS2_PLACEMENT_3D('',#69247,#35070,#35071);
#32523=AXIS2_PLACEMENT_3D('',#69248,#35072,#35073);
#32524=AXIS2_PLACEMENT_3D('',#69257,#35078,#35079);
#32525=AXIS2_PLACEMENT_3D('',#69259,#35080,#35081);
#32526=AXIS2_PLACEMENT_3D('',#69261,#35083,#35084);
#32527=AXIS2_PLACEMENT_3D('',#69265,#35087,#35088);
#32528=AXIS2_PLACEMENT_3D('',#69266,#35089,#35090);
#32529=AXIS2_PLACEMENT_3D('',#69267,#35091,#35092);
#32530=AXIS2_PLACEMENT_3D('',#69276,#35097,#35098);
#32531=AXIS2_PLACEMENT_3D('',#69278,#35099,#35100);
#32532=AXIS2_PLACEMENT_3D('',#69280,#35102,#35103);
#32533=AXIS2_PLACEMENT_3D('',#69284,#35106,#35107);
#32534=AXIS2_PLACEMENT_3D('',#69285,#35108,#35109);
#32535=AXIS2_PLACEMENT_3D('',#69286,#35110,#35111);
#32536=AXIS2_PLACEMENT_3D('',#69295,#35116,#35117);
#32537=AXIS2_PLACEMENT_3D('',#69297,#35118,#35119);
#32538=AXIS2_PLACEMENT_3D('',#69299,#35121,#35122);
#32539=AXIS2_PLACEMENT_3D('',#69303,#35125,#35126);
#32540=AXIS2_PLACEMENT_3D('',#69304,#35127,#35128);
#32541=AXIS2_PLACEMENT_3D('',#69305,#35129,#35130);
#32542=AXIS2_PLACEMENT_3D('',#69314,#35135,#35136);
#32543=AXIS2_PLACEMENT_3D('',#69316,#35137,#35138);
#32544=AXIS2_PLACEMENT_3D('',#69318,#35140,#35141);
#32545=AXIS2_PLACEMENT_3D('',#69322,#35144,#35145);
#32546=AXIS2_PLACEMENT_3D('',#69323,#35146,#35147);
#32547=AXIS2_PLACEMENT_3D('',#69324,#35148,#35149);
#32548=AXIS2_PLACEMENT_3D('',#69333,#35154,#35155);
#32549=AXIS2_PLACEMENT_3D('',#69335,#35156,#35157);
#32550=AXIS2_PLACEMENT_3D('',#69337,#35159,#35160);
#32551=AXIS2_PLACEMENT_3D('',#69341,#35163,#35164);
#32552=AXIS2_PLACEMENT_3D('',#69342,#35165,#35166);
#32553=AXIS2_PLACEMENT_3D('',#69343,#35167,#35168);
#32554=AXIS2_PLACEMENT_3D('',#69352,#35173,#35174);
#32555=AXIS2_PLACEMENT_3D('',#69354,#35175,#35176);
#32556=AXIS2_PLACEMENT_3D('',#69356,#35178,#35179);
#32557=AXIS2_PLACEMENT_3D('',#69360,#35182,#35183);
#32558=AXIS2_PLACEMENT_3D('',#69361,#35184,#35185);
#32559=AXIS2_PLACEMENT_3D('',#69362,#35186,#35187);
#32560=AXIS2_PLACEMENT_3D('',#69371,#35192,#35193);
#32561=AXIS2_PLACEMENT_3D('',#69373,#35194,#35195);
#32562=AXIS2_PLACEMENT_3D('',#69375,#35197,#35198);
#32563=AXIS2_PLACEMENT_3D('',#69379,#35201,#35202);
#32564=AXIS2_PLACEMENT_3D('',#69380,#35203,#35204);
#32565=AXIS2_PLACEMENT_3D('',#69381,#35205,#35206);
#32566=AXIS2_PLACEMENT_3D('',#69390,#35211,#35212);
#32567=AXIS2_PLACEMENT_3D('',#69392,#35213,#35214);
#32568=AXIS2_PLACEMENT_3D('',#69394,#35216,#35217);
#32569=AXIS2_PLACEMENT_3D('',#69398,#35220,#35221);
#32570=AXIS2_PLACEMENT_3D('',#69399,#35222,#35223);
#32571=AXIS2_PLACEMENT_3D('',#69400,#35224,#35225);
#32572=AXIS2_PLACEMENT_3D('',#69409,#35230,#35231);
#32573=AXIS2_PLACEMENT_3D('',#69411,#35232,#35233);
#32574=AXIS2_PLACEMENT_3D('',#69413,#35235,#35236);
#32575=AXIS2_PLACEMENT_3D('',#69417,#35239,#35240);
#32576=AXIS2_PLACEMENT_3D('',#69418,#35241,#35242);
#32577=AXIS2_PLACEMENT_3D('',#69419,#35243,#35244);
#32578=AXIS2_PLACEMENT_3D('',#69428,#35249,#35250);
#32579=AXIS2_PLACEMENT_3D('',#69430,#35251,#35252);
#32580=AXIS2_PLACEMENT_3D('',#69432,#35254,#35255);
#32581=AXIS2_PLACEMENT_3D('',#69436,#35258,#35259);
#32582=AXIS2_PLACEMENT_3D('',#69437,#35260,#35261);
#32583=AXIS2_PLACEMENT_3D('',#69438,#35262,#35263);
#32584=AXIS2_PLACEMENT_3D('',#69447,#35268,#35269);
#32585=AXIS2_PLACEMENT_3D('',#69449,#35270,#35271);
#32586=AXIS2_PLACEMENT_3D('',#69451,#35273,#35274);
#32587=AXIS2_PLACEMENT_3D('',#69455,#35277,#35278);
#32588=AXIS2_PLACEMENT_3D('',#69456,#35279,#35280);
#32589=AXIS2_PLACEMENT_3D('',#69457,#35281,#35282);
#32590=AXIS2_PLACEMENT_3D('',#69466,#35287,#35288);
#32591=AXIS2_PLACEMENT_3D('',#69468,#35289,#35290);
#32592=AXIS2_PLACEMENT_3D('',#69470,#35292,#35293);
#32593=AXIS2_PLACEMENT_3D('',#69474,#35296,#35297);
#32594=AXIS2_PLACEMENT_3D('',#69475,#35298,#35299);
#32595=AXIS2_PLACEMENT_3D('',#69476,#35300,#35301);
#32596=AXIS2_PLACEMENT_3D('',#69485,#35306,#35307);
#32597=AXIS2_PLACEMENT_3D('',#69487,#35308,#35309);
#32598=AXIS2_PLACEMENT_3D('',#69489,#35311,#35312);
#32599=AXIS2_PLACEMENT_3D('',#69493,#35315,#35316);
#32600=AXIS2_PLACEMENT_3D('',#69494,#35317,#35318);
#32601=AXIS2_PLACEMENT_3D('',#69495,#35319,#35320);
#32602=AXIS2_PLACEMENT_3D('',#69504,#35325,#35326);
#32603=AXIS2_PLACEMENT_3D('',#69506,#35327,#35328);
#32604=AXIS2_PLACEMENT_3D('',#69508,#35330,#35331);
#32605=AXIS2_PLACEMENT_3D('',#69512,#35334,#35335);
#32606=AXIS2_PLACEMENT_3D('',#69513,#35336,#35337);
#32607=AXIS2_PLACEMENT_3D('',#69514,#35338,#35339);
#32608=AXIS2_PLACEMENT_3D('',#69523,#35344,#35345);
#32609=AXIS2_PLACEMENT_3D('',#69525,#35346,#35347);
#32610=AXIS2_PLACEMENT_3D('',#69527,#35349,#35350);
#32611=AXIS2_PLACEMENT_3D('',#69531,#35353,#35354);
#32612=AXIS2_PLACEMENT_3D('',#69532,#35355,#35356);
#32613=AXIS2_PLACEMENT_3D('',#69533,#35357,#35358);
#32614=AXIS2_PLACEMENT_3D('',#69542,#35363,#35364);
#32615=AXIS2_PLACEMENT_3D('',#69544,#35365,#35366);
#32616=AXIS2_PLACEMENT_3D('',#69547,#35368,#35369);
#32617=AXIS2_PLACEMENT_3D('',#69548,#35370,#35371);
#32618=AXIS2_PLACEMENT_3D('',#69552,#35374,#35375);
#32619=AXIS2_PLACEMENT_3D('',#69554,#35376,#35377);
#32620=AXIS2_PLACEMENT_3D('',#69555,#35378,#35379);
#32621=AXIS2_PLACEMENT_3D('',#69556,#35380,#35381);
#32622=AXIS2_PLACEMENT_3D('',#69565,#35386,#35387);
#32623=AXIS2_PLACEMENT_3D('',#69567,#35388,#35389);
#32624=AXIS2_PLACEMENT_3D('',#69569,#35391,#35392);
#32625=AXIS2_PLACEMENT_3D('',#69573,#35395,#35396);
#32626=AXIS2_PLACEMENT_3D('',#69574,#35397,#35398);
#32627=AXIS2_PLACEMENT_3D('',#69575,#35399,#35400);
#32628=AXIS2_PLACEMENT_3D('',#69584,#35405,#35406);
#32629=AXIS2_PLACEMENT_3D('',#69586,#35407,#35408);
#32630=AXIS2_PLACEMENT_3D('',#69588,#35410,#35411);
#32631=AXIS2_PLACEMENT_3D('',#69592,#35414,#35415);
#32632=AXIS2_PLACEMENT_3D('',#69593,#35416,#35417);
#32633=AXIS2_PLACEMENT_3D('',#69594,#35418,#35419);
#32634=AXIS2_PLACEMENT_3D('',#69603,#35424,#35425);
#32635=AXIS2_PLACEMENT_3D('',#69605,#35426,#35427);
#32636=AXIS2_PLACEMENT_3D('',#69607,#35429,#35430);
#32637=AXIS2_PLACEMENT_3D('',#69611,#35433,#35434);
#32638=AXIS2_PLACEMENT_3D('',#69612,#35435,#35436);
#32639=AXIS2_PLACEMENT_3D('',#69613,#35437,#35438);
#32640=AXIS2_PLACEMENT_3D('',#69622,#35443,#35444);
#32641=AXIS2_PLACEMENT_3D('',#69624,#35445,#35446);
#32642=AXIS2_PLACEMENT_3D('',#69626,#35448,#35449);
#32643=AXIS2_PLACEMENT_3D('',#69630,#35452,#35453);
#32644=AXIS2_PLACEMENT_3D('',#69631,#35454,#35455);
#32645=AXIS2_PLACEMENT_3D('',#69632,#35456,#35457);
#32646=AXIS2_PLACEMENT_3D('',#69641,#35462,#35463);
#32647=AXIS2_PLACEMENT_3D('',#69643,#35464,#35465);
#32648=AXIS2_PLACEMENT_3D('',#69645,#35467,#35468);
#32649=AXIS2_PLACEMENT_3D('',#69649,#35471,#35472);
#32650=AXIS2_PLACEMENT_3D('',#69650,#35473,#35474);
#32651=AXIS2_PLACEMENT_3D('',#69651,#35475,#35476);
#32652=AXIS2_PLACEMENT_3D('',#69660,#35481,#35482);
#32653=AXIS2_PLACEMENT_3D('',#69662,#35483,#35484);
#32654=AXIS2_PLACEMENT_3D('',#69664,#35486,#35487);
#32655=AXIS2_PLACEMENT_3D('',#69668,#35490,#35491);
#32656=AXIS2_PLACEMENT_3D('',#69669,#35492,#35493);
#32657=AXIS2_PLACEMENT_3D('',#69670,#35494,#35495);
#32658=AXIS2_PLACEMENT_3D('',#69679,#35500,#35501);
#32659=AXIS2_PLACEMENT_3D('',#69681,#35502,#35503);
#32660=AXIS2_PLACEMENT_3D('',#69683,#35505,#35506);
#32661=AXIS2_PLACEMENT_3D('',#69687,#35509,#35510);
#32662=AXIS2_PLACEMENT_3D('',#69688,#35511,#35512);
#32663=AXIS2_PLACEMENT_3D('',#69689,#35513,#35514);
#32664=AXIS2_PLACEMENT_3D('',#69698,#35519,#35520);
#32665=AXIS2_PLACEMENT_3D('',#69700,#35521,#35522);
#32666=AXIS2_PLACEMENT_3D('',#69702,#35524,#35525);
#32667=AXIS2_PLACEMENT_3D('',#69706,#35528,#35529);
#32668=AXIS2_PLACEMENT_3D('',#69707,#35530,#35531);
#32669=AXIS2_PLACEMENT_3D('',#69708,#35532,#35533);
#32670=AXIS2_PLACEMENT_3D('',#69717,#35538,#35539);
#32671=AXIS2_PLACEMENT_3D('',#69719,#35540,#35541);
#32672=AXIS2_PLACEMENT_3D('',#69721,#35543,#35544);
#32673=AXIS2_PLACEMENT_3D('',#69725,#35547,#35548);
#32674=AXIS2_PLACEMENT_3D('',#69726,#35549,#35550);
#32675=AXIS2_PLACEMENT_3D('',#69727,#35551,#35552);
#32676=AXIS2_PLACEMENT_3D('',#69736,#35557,#35558);
#32677=AXIS2_PLACEMENT_3D('',#69738,#35559,#35560);
#32678=AXIS2_PLACEMENT_3D('',#69740,#35562,#35563);
#32679=AXIS2_PLACEMENT_3D('',#69744,#35566,#35567);
#32680=AXIS2_PLACEMENT_3D('',#69745,#35568,#35569);
#32681=AXIS2_PLACEMENT_3D('',#69746,#35570,#35571);
#32682=AXIS2_PLACEMENT_3D('',#69755,#35576,#35577);
#32683=AXIS2_PLACEMENT_3D('',#69757,#35578,#35579);
#32684=AXIS2_PLACEMENT_3D('',#69759,#35581,#35582);
#32685=AXIS2_PLACEMENT_3D('',#69763,#35585,#35586);
#32686=AXIS2_PLACEMENT_3D('',#69764,#35587,#35588);
#32687=AXIS2_PLACEMENT_3D('',#69765,#35589,#35590);
#32688=AXIS2_PLACEMENT_3D('',#69774,#35595,#35596);
#32689=AXIS2_PLACEMENT_3D('',#69776,#35597,#35598);
#32690=AXIS2_PLACEMENT_3D('',#69778,#35600,#35601);
#32691=AXIS2_PLACEMENT_3D('',#69782,#35604,#35605);
#32692=AXIS2_PLACEMENT_3D('',#69783,#35606,#35607);
#32693=AXIS2_PLACEMENT_3D('',#69784,#35608,#35609);
#32694=AXIS2_PLACEMENT_3D('',#69793,#35614,#35615);
#32695=AXIS2_PLACEMENT_3D('',#69795,#35616,#35617);
#32696=AXIS2_PLACEMENT_3D('',#69797,#35619,#35620);
#32697=AXIS2_PLACEMENT_3D('',#69801,#35623,#35624);
#32698=AXIS2_PLACEMENT_3D('',#69802,#35625,#35626);
#32699=AXIS2_PLACEMENT_3D('',#69803,#35627,#35628);
#32700=AXIS2_PLACEMENT_3D('',#69812,#35633,#35634);
#32701=AXIS2_PLACEMENT_3D('',#69814,#35635,#35636);
#32702=AXIS2_PLACEMENT_3D('',#69816,#35638,#35639);
#32703=AXIS2_PLACEMENT_3D('',#69820,#35642,#35643);
#32704=AXIS2_PLACEMENT_3D('',#69821,#35644,#35645);
#32705=AXIS2_PLACEMENT_3D('',#69822,#35646,#35647);
#32706=AXIS2_PLACEMENT_3D('',#69831,#35652,#35653);
#32707=AXIS2_PLACEMENT_3D('',#69833,#35654,#35655);
#32708=AXIS2_PLACEMENT_3D('',#69835,#35657,#35658);
#32709=AXIS2_PLACEMENT_3D('',#69839,#35661,#35662);
#32710=AXIS2_PLACEMENT_3D('',#69840,#35663,#35664);
#32711=AXIS2_PLACEMENT_3D('',#69841,#35665,#35666);
#32712=AXIS2_PLACEMENT_3D('',#69850,#35671,#35672);
#32713=AXIS2_PLACEMENT_3D('',#69852,#35673,#35674);
#32714=AXIS2_PLACEMENT_3D('',#69854,#35676,#35677);
#32715=AXIS2_PLACEMENT_3D('',#69858,#35680,#35681);
#32716=AXIS2_PLACEMENT_3D('',#69859,#35682,#35683);
#32717=AXIS2_PLACEMENT_3D('',#69860,#35684,#35685);
#32718=AXIS2_PLACEMENT_3D('',#69869,#35690,#35691);
#32719=AXIS2_PLACEMENT_3D('',#69871,#35692,#35693);
#32720=AXIS2_PLACEMENT_3D('',#69873,#35695,#35696);
#32721=AXIS2_PLACEMENT_3D('',#69877,#35699,#35700);
#32722=AXIS2_PLACEMENT_3D('',#69878,#35701,#35702);
#32723=AXIS2_PLACEMENT_3D('',#69879,#35703,#35704);
#32724=AXIS2_PLACEMENT_3D('',#69888,#35709,#35710);
#32725=AXIS2_PLACEMENT_3D('',#69890,#35711,#35712);
#32726=AXIS2_PLACEMENT_3D('',#69892,#35714,#35715);
#32727=AXIS2_PLACEMENT_3D('',#69896,#35718,#35719);
#32728=AXIS2_PLACEMENT_3D('',#69897,#35720,#35721);
#32729=AXIS2_PLACEMENT_3D('',#69898,#35722,#35723);
#32730=AXIS2_PLACEMENT_3D('',#69904,#35727,#35728);
#32731=AXIS2_PLACEMENT_3D('',#69905,#35729,#35730);
#32732=AXIS2_PLACEMENT_3D('',#69906,#35731,#35732);
#32733=AXIS2_PLACEMENT_3D('',#69910,#35735,#35736);
#32734=AXIS2_PLACEMENT_3D('',#69911,#35737,#35738);
#32735=AXIS2_PLACEMENT_3D('',#69912,#35739,#35740);
#32736=AXIS2_PLACEMENT_3D('',#69913,#35741,#35742);
#32737=AXIS2_PLACEMENT_3D('',#69914,#35743,#35744);
#32738=AXIS2_PLACEMENT_3D('',#69915,#35745,#35746);
#32739=AXIS2_PLACEMENT_3D('',#69916,#35747,#35748);
#32740=AXIS2_PLACEMENT_3D('',#69918,#35749,#35750);
#32741=AXIS2_PLACEMENT_3D('',#69921,#35752,#35753);
#32742=AXIS2_PLACEMENT_3D('',#69922,#35754,#35755);
#32743=AXIS2_PLACEMENT_3D('',#69924,#35756,#35757);
#32744=AXIS2_PLACEMENT_3D('',#69925,#35758,#35759);
#32745=AXIS2_PLACEMENT_3D('',#69927,#35760,#35761);
#32746=AXIS2_PLACEMENT_3D('',#69929,#35763,#35764);
#32747=AXIS2_PLACEMENT_3D('',#69931,#35765,#35766);
#32748=AXIS2_PLACEMENT_3D('',#69934,#35769,#35770);
#32749=AXIS2_PLACEMENT_3D('',#69937,#35772,#35773);
#32750=AXIS2_PLACEMENT_3D('',#69938,#35774,#35775);
#32751=AXIS2_PLACEMENT_3D('',#69940,#35776,#35777);
#32752=AXIS2_PLACEMENT_3D('',#69941,#35778,#35779);
#32753=AXIS2_PLACEMENT_3D('',#69943,#35780,#35781);
#32754=AXIS2_PLACEMENT_3D('',#69945,#35783,#35784);
#32755=AXIS2_PLACEMENT_3D('',#69947,#35785,#35786);
#32756=AXIS2_PLACEMENT_3D('',#69948,#35787,#35788);
#32757=AXIS2_PLACEMENT_3D('',#69950,#35790,#35791);
#32758=AXIS2_PLACEMENT_3D('',#70251,#35812,#35813);
#32759=AXIS2_PLACEMENT_3D('',#70252,#35814,#35815);
#32760=AXIS2_PLACEMENT_3D('',#70261,#35820,#35821);
#32761=AXIS2_PLACEMENT_3D('',#70267,#35825,#35826);
#32762=AXIS2_PLACEMENT_3D('',#70270,#35829,#35830);
#32763=AXIS2_PLACEMENT_3D('',#70279,#35835,#35836);
#32764=AXIS2_PLACEMENT_3D('',#70285,#35840,#35841);
#32765=AXIS2_PLACEMENT_3D('',#70291,#35845,#35846);
#32766=AXIS2_PLACEMENT_3D('',#70297,#35850,#35851);
#32767=AXIS2_PLACEMENT_3D('',#70303,#35855,#35856);
#32768=AXIS2_PLACEMENT_3D('',#70309,#35860,#35861);
#32769=AXIS2_PLACEMENT_3D('',#70315,#35865,#35866);
#32770=AXIS2_PLACEMENT_3D('',#70321,#35870,#35871);
#32771=AXIS2_PLACEMENT_3D('',#70327,#35875,#35876);
#32772=AXIS2_PLACEMENT_3D('',#70333,#35880,#35881);
#32773=AXIS2_PLACEMENT_3D('',#70336,#35884,#35885);
#32774=AXIS2_PLACEMENT_3D('',#70337,#35886,#35887);
#32775=AXIS2_PLACEMENT_3D('',#70338,#35888,#35889);
#32776=AXIS2_PLACEMENT_3D('',#70639,#35910,#35911);
#32777=AXIS2_PLACEMENT_3D('',#70823,#35925,#35926);
#32778=AXIS2_PLACEMENT_3D('',#70934,#35937,#35938);
#32779=AXIS2_PLACEMENT_3D('',#71045,#35949,#35950);
#32780=AXIS2_PLACEMENT_3D('',#71063,#35954,#35955);
#32781=AXIS2_PLACEMENT_3D('',#71064,#35956,#35957);
#32782=AXIS2_PLACEMENT_3D('',#71365,#35978,#35979);
#32783=AXIS2_PLACEMENT_3D('',#71504,#35990,#35991);
#32784=AXIS2_PLACEMENT_3D('',#71645,#36004,#36005);
#32785=AXIS2_PLACEMENT_3D('',#71651,#36009,#36010);
#32786=AXIS2_PLACEMENT_3D('',#71657,#36014,#36015);
#32787=AXIS2_PLACEMENT_3D('',#71660,#36018,#36019);
#32788=AXIS2_PLACEMENT_3D('',#71661,#36020,#36021);
#32789=AXIS2_PLACEMENT_3D('',#71962,#36042,#36043);
#32790=AXIS2_PLACEMENT_3D('',#71963,#36044,#36045);
#32791=AXIS2_PLACEMENT_3D('',#72002,#36052,#36053);
#32792=AXIS2_PLACEMENT_3D('',#72038,#36059,#36060);
#32793=AXIS2_PLACEMENT_3D('',#72044,#36064,#36065);
#32794=AXIS2_PLACEMENT_3D('',#72050,#36069,#36070);
#32795=AXIS2_PLACEMENT_3D('',#72053,#36073,#36074);
#32796=AXIS2_PLACEMENT_3D('',#72054,#36075,#36076);
#32797=AXIS2_PLACEMENT_3D('',#72355,#36097,#36098);
#32798=AXIS2_PLACEMENT_3D('',#72356,#36099,#36100);
#32799=AXIS2_PLACEMENT_3D('',#72657,#36121,#36122);
#32800=AXIS2_PLACEMENT_3D('',#72658,#36123,#36124);
#32801=AXIS2_PLACEMENT_3D('',#72697,#36131,#36132);
#32802=AXIS2_PLACEMENT_3D('',#72733,#36138,#36139);
#32803=AXIS2_PLACEMENT_3D('',#72739,#36143,#36144);
#32804=AXIS2_PLACEMENT_3D('',#72745,#36148,#36149);
#32805=AXIS2_PLACEMENT_3D('',#72748,#36152,#36153);
#32806=AXIS2_PLACEMENT_3D('',#72749,#36154,#36155);
#32807=AXIS2_PLACEMENT_3D('',#73050,#36176,#36177);
#32808=AXIS2_PLACEMENT_3D('',#73189,#36188,#36189);
#32809=AXIS2_PLACEMENT_3D('',#73330,#36202,#36203);
#32810=AXIS2_PLACEMENT_3D('',#73336,#36207,#36208);
#32811=AXIS2_PLACEMENT_3D('',#73342,#36212,#36213);
#32812=AXIS2_PLACEMENT_3D('',#73345,#36216,#36217);
#32813=AXIS2_PLACEMENT_3D('',#73346,#36218,#36219);
#32814=AXIS2_PLACEMENT_3D('',#73647,#36240,#36241);
#32815=AXIS2_PLACEMENT_3D('',#73831,#36255,#36256);
#32816=AXIS2_PLACEMENT_3D('',#73942,#36267,#36268);
#32817=AXIS2_PLACEMENT_3D('',#74053,#36279,#36280);
#32818=AXIS2_PLACEMENT_3D('',#74071,#36284,#36285);
#32819=AXIS2_PLACEMENT_3D('',#74072,#36286,#36287);
#32820=AXIS2_PLACEMENT_3D('',#74373,#36308,#36309);
#32821=AXIS2_PLACEMENT_3D('',#74374,#36310,#36311);
#32822=AXIS2_PLACEMENT_3D('',#74383,#36316,#36317);
#32823=AXIS2_PLACEMENT_3D('',#74389,#36321,#36322);
#32824=AXIS2_PLACEMENT_3D('',#74392,#36325,#36326);
#32825=AXIS2_PLACEMENT_3D('',#74401,#36331,#36332);
#32826=AXIS2_PLACEMENT_3D('',#74407,#36336,#36337);
#32827=AXIS2_PLACEMENT_3D('',#74413,#36341,#36342);
#32828=AXIS2_PLACEMENT_3D('',#74419,#36346,#36347);
#32829=AXIS2_PLACEMENT_3D('',#74425,#36351,#36352);
#32830=AXIS2_PLACEMENT_3D('',#74431,#36356,#36357);
#32831=AXIS2_PLACEMENT_3D('',#74437,#36361,#36362);
#32832=AXIS2_PLACEMENT_3D('',#74443,#36366,#36367);
#32833=AXIS2_PLACEMENT_3D('',#74449,#36371,#36372);
#32834=AXIS2_PLACEMENT_3D('',#74455,#36376,#36377);
#32835=AXIS2_PLACEMENT_3D('',#74458,#36380,#36381);
#32836=AXIS2_PLACEMENT_3D('',#74459,#36382,#36383);
#32837=AXIS2_PLACEMENT_3D('',#74460,#36384,#36385);
#32838=AXIS2_PLACEMENT_3D('',#74461,#36386,#36387);
#32839=AXIS2_PLACEMENT_3D('',#74470,#36392,#36393);
#32840=AXIS2_PLACEMENT_3D('',#74476,#36397,#36398);
#32841=AXIS2_PLACEMENT_3D('',#74482,#36402,#36403);
#32842=AXIS2_PLACEMENT_3D('',#74485,#36406,#36407);
#32843=AXIS2_PLACEMENT_3D('',#74486,#36408,#36409);
#32844=AXIS2_PLACEMENT_3D('',#74495,#36414,#36415);
#32845=AXIS2_PLACEMENT_3D('',#74501,#36419,#36420);
#32846=AXIS2_PLACEMENT_3D('',#74507,#36424,#36425);
#32847=AXIS2_PLACEMENT_3D('',#74510,#36428,#36429);
#32848=AXIS2_PLACEMENT_3D('',#74511,#36430,#36431);
#32849=AXIS2_PLACEMENT_3D('',#74520,#36436,#36437);
#32850=AXIS2_PLACEMENT_3D('',#74526,#36441,#36442);
#32851=AXIS2_PLACEMENT_3D('',#74532,#36446,#36447);
#32852=AXIS2_PLACEMENT_3D('',#74535,#36450,#36451);
#32853=AXIS2_PLACEMENT_3D('',#74536,#36452,#36453);
#32854=AXIS2_PLACEMENT_3D('',#74545,#36458,#36459);
#32855=AXIS2_PLACEMENT_3D('',#74551,#36463,#36464);
#32856=AXIS2_PLACEMENT_3D('',#74557,#36468,#36469);
#32857=AXIS2_PLACEMENT_3D('',#74560,#36472,#36473);
#32858=AXIS2_PLACEMENT_3D('',#74561,#36474,#36475);
#32859=AXIS2_PLACEMENT_3D('',#74570,#36480,#36481);
#32860=AXIS2_PLACEMENT_3D('',#74576,#36485,#36486);
#32861=AXIS2_PLACEMENT_3D('',#74582,#36490,#36491);
#32862=AXIS2_PLACEMENT_3D('',#74585,#36494,#36495);
#32863=AXIS2_PLACEMENT_3D('',#74586,#36496,#36497);
#32864=AXIS2_PLACEMENT_3D('',#74595,#36502,#36503);
#32865=AXIS2_PLACEMENT_3D('',#74601,#36507,#36508);
#32866=AXIS2_PLACEMENT_3D('',#74607,#36512,#36513);
#32867=AXIS2_PLACEMENT_3D('',#74610,#36516,#36517);
#32868=AXIS2_PLACEMENT_3D('',#74611,#36518,#36519);
#32869=AXIS2_PLACEMENT_3D('',#74620,#36524,#36525);
#32870=AXIS2_PLACEMENT_3D('',#74626,#36529,#36530);
#32871=AXIS2_PLACEMENT_3D('',#74632,#36534,#36535);
#32872=AXIS2_PLACEMENT_3D('',#74635,#36538,#36539);
#32873=AXIS2_PLACEMENT_3D('',#74636,#36540,#36541);
#32874=AXIS2_PLACEMENT_3D('',#74645,#36546,#36547);
#32875=AXIS2_PLACEMENT_3D('',#74651,#36551,#36552);
#32876=AXIS2_PLACEMENT_3D('',#74657,#36556,#36557);
#32877=AXIS2_PLACEMENT_3D('',#74660,#36560,#36561);
#32878=AXIS2_PLACEMENT_3D('',#74661,#36562,#36563);
#32879=AXIS2_PLACEMENT_3D('',#74670,#36568,#36569);
#32880=AXIS2_PLACEMENT_3D('',#74676,#36573,#36574);
#32881=AXIS2_PLACEMENT_3D('',#74682,#36578,#36579);
#32882=AXIS2_PLACEMENT_3D('',#74685,#36582,#36583);
#32883=AXIS2_PLACEMENT_3D('',#74686,#36584,#36585);
#32884=AXIS2_PLACEMENT_3D('',#74695,#36590,#36591);
#32885=AXIS2_PLACEMENT_3D('',#74701,#36595,#36596);
#32886=AXIS2_PLACEMENT_3D('',#74707,#36600,#36601);
#32887=AXIS2_PLACEMENT_3D('',#74710,#36604,#36605);
#32888=AXIS2_PLACEMENT_3D('',#74711,#36606,#36607);
#32889=AXIS2_PLACEMENT_3D('',#74720,#36612,#36613);
#32890=AXIS2_PLACEMENT_3D('',#74726,#36617,#36618);
#32891=AXIS2_PLACEMENT_3D('',#74732,#36622,#36623);
#32892=AXIS2_PLACEMENT_3D('',#74735,#36626,#36627);
#32893=AXIS2_PLACEMENT_3D('',#74736,#36628,#36629);
#32894=AXIS2_PLACEMENT_3D('',#74745,#36634,#36635);
#32895=AXIS2_PLACEMENT_3D('',#74751,#36639,#36640);
#32896=AXIS2_PLACEMENT_3D('',#74757,#36644,#36645);
#32897=AXIS2_PLACEMENT_3D('',#74760,#36648,#36649);
#32898=AXIS2_PLACEMENT_3D('',#74761,#36650,#36651);
#32899=AXIS2_PLACEMENT_3D('',#74770,#36656,#36657);
#32900=AXIS2_PLACEMENT_3D('',#74776,#36661,#36662);
#32901=AXIS2_PLACEMENT_3D('',#74782,#36666,#36667);
#32902=AXIS2_PLACEMENT_3D('',#74785,#36670,#36671);
#32903=AXIS2_PLACEMENT_3D('',#74786,#36672,#36673);
#32904=AXIS2_PLACEMENT_3D('',#74795,#36678,#36679);
#32905=AXIS2_PLACEMENT_3D('',#74801,#36683,#36684);
#32906=AXIS2_PLACEMENT_3D('',#74807,#36688,#36689);
#32907=AXIS2_PLACEMENT_3D('',#74810,#36692,#36693);
#32908=AXIS2_PLACEMENT_3D('',#74811,#36694,#36695);
#32909=AXIS2_PLACEMENT_3D('',#74820,#36700,#36701);
#32910=AXIS2_PLACEMENT_3D('',#74826,#36705,#36706);
#32911=AXIS2_PLACEMENT_3D('',#74832,#36710,#36711);
#32912=AXIS2_PLACEMENT_3D('',#74835,#36714,#36715);
#32913=AXIS2_PLACEMENT_3D('',#74836,#36716,#36717);
#32914=AXIS2_PLACEMENT_3D('',#74845,#36722,#36723);
#32915=AXIS2_PLACEMENT_3D('',#74851,#36727,#36728);
#32916=AXIS2_PLACEMENT_3D('',#74857,#36732,#36733);
#32917=AXIS2_PLACEMENT_3D('',#74860,#36736,#36737);
#32918=AXIS2_PLACEMENT_3D('',#74861,#36738,#36739);
#32919=AXIS2_PLACEMENT_3D('',#74870,#36744,#36745);
#32920=AXIS2_PLACEMENT_3D('',#74876,#36749,#36750);
#32921=AXIS2_PLACEMENT_3D('',#74882,#36754,#36755);
#32922=AXIS2_PLACEMENT_3D('',#74885,#36758,#36759);
#32923=AXIS2_PLACEMENT_3D('',#74886,#36760,#36761);
#32924=AXIS2_PLACEMENT_3D('',#74895,#36766,#36767);
#32925=AXIS2_PLACEMENT_3D('',#74901,#36771,#36772);
#32926=AXIS2_PLACEMENT_3D('',#74907,#36776,#36777);
#32927=AXIS2_PLACEMENT_3D('',#74910,#36780,#36781);
#32928=AXIS2_PLACEMENT_3D('',#74911,#36782,#36783);
#32929=AXIS2_PLACEMENT_3D('',#74920,#36788,#36789);
#32930=AXIS2_PLACEMENT_3D('',#74926,#36793,#36794);
#32931=AXIS2_PLACEMENT_3D('',#74932,#36798,#36799);
#32932=AXIS2_PLACEMENT_3D('',#74935,#36802,#36803);
#32933=AXIS2_PLACEMENT_3D('',#74936,#36804,#36805);
#32934=AXIS2_PLACEMENT_3D('',#74945,#36810,#36811);
#32935=AXIS2_PLACEMENT_3D('',#74951,#36815,#36816);
#32936=AXIS2_PLACEMENT_3D('',#74957,#36820,#36821);
#32937=AXIS2_PLACEMENT_3D('',#74960,#36824,#36825);
#32938=AXIS2_PLACEMENT_3D('',#74961,#36826,#36827);
#32939=AXIS2_PLACEMENT_3D('',#74970,#36832,#36833);
#32940=AXIS2_PLACEMENT_3D('',#74976,#36837,#36838);
#32941=AXIS2_PLACEMENT_3D('',#74982,#36842,#36843);
#32942=AXIS2_PLACEMENT_3D('',#74985,#36846,#36847);
#32943=AXIS2_PLACEMENT_3D('',#74986,#36848,#36849);
#32944=AXIS2_PLACEMENT_3D('',#74995,#36854,#36855);
#32945=AXIS2_PLACEMENT_3D('',#75001,#36859,#36860);
#32946=AXIS2_PLACEMENT_3D('',#75007,#36864,#36865);
#32947=AXIS2_PLACEMENT_3D('',#75010,#36868,#36869);
#32948=AXIS2_PLACEMENT_3D('',#75011,#36870,#36871);
#32949=AXIS2_PLACEMENT_3D('',#75020,#36876,#36877);
#32950=AXIS2_PLACEMENT_3D('',#75026,#36881,#36882);
#32951=AXIS2_PLACEMENT_3D('',#75032,#36886,#36887);
#32952=AXIS2_PLACEMENT_3D('',#75035,#36890,#36891);
#32953=AXIS2_PLACEMENT_3D('',#75036,#36892,#36893);
#32954=AXIS2_PLACEMENT_3D('',#75045,#36898,#36899);
#32955=AXIS2_PLACEMENT_3D('',#75051,#36903,#36904);
#32956=AXIS2_PLACEMENT_3D('',#75057,#36908,#36909);
#32957=AXIS2_PLACEMENT_3D('',#75060,#36912,#36913);
#32958=AXIS2_PLACEMENT_3D('',#75061,#36914,#36915);
#32959=AXIS2_PLACEMENT_3D('',#75070,#36920,#36921);
#32960=AXIS2_PLACEMENT_3D('',#75076,#36925,#36926);
#32961=AXIS2_PLACEMENT_3D('',#75082,#36930,#36931);
#32962=AXIS2_PLACEMENT_3D('',#75085,#36934,#36935);
#32963=AXIS2_PLACEMENT_3D('',#75086,#36936,#36937);
#32964=AXIS2_PLACEMENT_3D('',#75095,#36942,#36943);
#32965=AXIS2_PLACEMENT_3D('',#75101,#36947,#36948);
#32966=AXIS2_PLACEMENT_3D('',#75107,#36952,#36953);
#32967=AXIS2_PLACEMENT_3D('',#75110,#36956,#36957);
#32968=AXIS2_PLACEMENT_3D('',#75111,#36958,#36959);
#32969=AXIS2_PLACEMENT_3D('',#75120,#36964,#36965);
#32970=AXIS2_PLACEMENT_3D('',#75126,#36969,#36970);
#32971=AXIS2_PLACEMENT_3D('',#75132,#36974,#36975);
#32972=AXIS2_PLACEMENT_3D('',#75135,#36978,#36979);
#32973=AXIS2_PLACEMENT_3D('',#75136,#36980,#36981);
#32974=AXIS2_PLACEMENT_3D('',#75145,#36986,#36987);
#32975=AXIS2_PLACEMENT_3D('',#75151,#36991,#36992);
#32976=AXIS2_PLACEMENT_3D('',#75157,#36996,#36997);
#32977=AXIS2_PLACEMENT_3D('',#75160,#37000,#37001);
#32978=AXIS2_PLACEMENT_3D('',#75161,#37002,#37003);
#32979=AXIS2_PLACEMENT_3D('',#75170,#37008,#37009);
#32980=AXIS2_PLACEMENT_3D('',#75176,#37013,#37014);
#32981=AXIS2_PLACEMENT_3D('',#75182,#37018,#37019);
#32982=AXIS2_PLACEMENT_3D('',#75185,#37022,#37023);
#32983=AXIS2_PLACEMENT_3D('',#75186,#37024,#37025);
#32984=AXIS2_PLACEMENT_3D('',#75195,#37030,#37031);
#32985=AXIS2_PLACEMENT_3D('',#75201,#37035,#37036);
#32986=AXIS2_PLACEMENT_3D('',#75207,#37040,#37041);
#32987=AXIS2_PLACEMENT_3D('',#75210,#37044,#37045);
#32988=AXIS2_PLACEMENT_3D('',#75211,#37046,#37047);
#32989=AXIS2_PLACEMENT_3D('',#75220,#37052,#37053);
#32990=AXIS2_PLACEMENT_3D('',#75226,#37057,#37058);
#32991=AXIS2_PLACEMENT_3D('',#75232,#37062,#37063);
#32992=AXIS2_PLACEMENT_3D('',#75235,#37066,#37067);
#32993=AXIS2_PLACEMENT_3D('',#75236,#37068,#37069);
#32994=AXIS2_PLACEMENT_3D('',#75245,#37074,#37075);
#32995=AXIS2_PLACEMENT_3D('',#75251,#37079,#37080);
#32996=AXIS2_PLACEMENT_3D('',#75257,#37084,#37085);
#32997=AXIS2_PLACEMENT_3D('',#75260,#37088,#37089);
#32998=AXIS2_PLACEMENT_3D('',#75261,#37090,#37091);
#32999=AXIS2_PLACEMENT_3D('',#75270,#37096,#37097);
#33000=AXIS2_PLACEMENT_3D('',#75276,#37101,#37102);
#33001=AXIS2_PLACEMENT_3D('',#75282,#37106,#37107);
#33002=AXIS2_PLACEMENT_3D('',#75285,#37110,#37111);
#33003=AXIS2_PLACEMENT_3D('',#75286,#37112,#37113);
#33004=AXIS2_PLACEMENT_3D('',#75295,#37118,#37119);
#33005=AXIS2_PLACEMENT_3D('',#75301,#37123,#37124);
#33006=AXIS2_PLACEMENT_3D('',#75307,#37128,#37129);
#33007=AXIS2_PLACEMENT_3D('',#75310,#37132,#37133);
#33008=AXIS2_PLACEMENT_3D('',#75311,#37134,#37135);
#33009=AXIS2_PLACEMENT_3D('',#75320,#37140,#37141);
#33010=AXIS2_PLACEMENT_3D('',#75326,#37145,#37146);
#33011=AXIS2_PLACEMENT_3D('',#75332,#37150,#37151);
#33012=AXIS2_PLACEMENT_3D('',#75335,#37154,#37155);
#33013=AXIS2_PLACEMENT_3D('',#75336,#37156,#37157);
#33014=AXIS2_PLACEMENT_3D('',#75345,#37162,#37163);
#33015=AXIS2_PLACEMENT_3D('',#75351,#37167,#37168);
#33016=AXIS2_PLACEMENT_3D('',#75357,#37172,#37173);
#33017=AXIS2_PLACEMENT_3D('',#75360,#37176,#37177);
#33018=AXIS2_PLACEMENT_3D('',#75361,#37178,#37179);
#33019=AXIS2_PLACEMENT_3D('',#75370,#37184,#37185);
#33020=AXIS2_PLACEMENT_3D('',#75376,#37189,#37190);
#33021=AXIS2_PLACEMENT_3D('',#75382,#37194,#37195);
#33022=AXIS2_PLACEMENT_3D('',#75385,#37198,#37199);
#33023=AXIS2_PLACEMENT_3D('',#75386,#37200,#37201);
#33024=AXIS2_PLACEMENT_3D('',#75395,#37206,#37207);
#33025=AXIS2_PLACEMENT_3D('',#75401,#37211,#37212);
#33026=AXIS2_PLACEMENT_3D('',#75407,#37216,#37217);
#33027=AXIS2_PLACEMENT_3D('',#75410,#37220,#37221);
#33028=AXIS2_PLACEMENT_3D('',#75411,#37222,#37223);
#33029=AXIS2_PLACEMENT_3D('',#75420,#37228,#37229);
#33030=AXIS2_PLACEMENT_3D('',#75426,#37233,#37234);
#33031=AXIS2_PLACEMENT_3D('',#75432,#37238,#37239);
#33032=AXIS2_PLACEMENT_3D('',#75435,#37242,#37243);
#33033=AXIS2_PLACEMENT_3D('',#75436,#37244,#37245);
#33034=AXIS2_PLACEMENT_3D('',#75445,#37250,#37251);
#33035=AXIS2_PLACEMENT_3D('',#75451,#37255,#37256);
#33036=AXIS2_PLACEMENT_3D('',#75457,#37260,#37261);
#33037=AXIS2_PLACEMENT_3D('',#75460,#37264,#37265);
#33038=AXIS2_PLACEMENT_3D('',#75461,#37266,#37267);
#33039=AXIS2_PLACEMENT_3D('',#75470,#37272,#37273);
#33040=AXIS2_PLACEMENT_3D('',#75476,#37277,#37278);
#33041=AXIS2_PLACEMENT_3D('',#75482,#37282,#37283);
#33042=AXIS2_PLACEMENT_3D('',#75485,#37286,#37287);
#33043=AXIS2_PLACEMENT_3D('',#75486,#37288,#37289);
#33044=AXIS2_PLACEMENT_3D('',#75495,#37294,#37295);
#33045=AXIS2_PLACEMENT_3D('',#75501,#37299,#37300);
#33046=AXIS2_PLACEMENT_3D('',#75507,#37304,#37305);
#33047=AXIS2_PLACEMENT_3D('',#75510,#37308,#37309);
#33048=AXIS2_PLACEMENT_3D('',#75511,#37310,#37311);
#33049=AXIS2_PLACEMENT_3D('',#75520,#37316,#37317);
#33050=AXIS2_PLACEMENT_3D('',#75526,#37321,#37322);
#33051=AXIS2_PLACEMENT_3D('',#75532,#37326,#37327);
#33052=AXIS2_PLACEMENT_3D('',#75535,#37330,#37331);
#33053=AXIS2_PLACEMENT_3D('',#75536,#37332,#37333);
#33054=AXIS2_PLACEMENT_3D('',#75545,#37338,#37339);
#33055=AXIS2_PLACEMENT_3D('',#75551,#37343,#37344);
#33056=AXIS2_PLACEMENT_3D('',#75557,#37348,#37349);
#33057=AXIS2_PLACEMENT_3D('',#75560,#37352,#37353);
#33058=AXIS2_PLACEMENT_3D('',#75561,#37354,#37355);
#33059=AXIS2_PLACEMENT_3D('',#75570,#37360,#37361);
#33060=AXIS2_PLACEMENT_3D('',#75576,#37365,#37366);
#33061=AXIS2_PLACEMENT_3D('',#75582,#37370,#37371);
#33062=AXIS2_PLACEMENT_3D('',#75585,#37374,#37375);
#33063=AXIS2_PLACEMENT_3D('',#75586,#37376,#37377);
#33064=AXIS2_PLACEMENT_3D('',#75595,#37382,#37383);
#33065=AXIS2_PLACEMENT_3D('',#75601,#37387,#37388);
#33066=AXIS2_PLACEMENT_3D('',#75607,#37392,#37393);
#33067=AXIS2_PLACEMENT_3D('',#75610,#37396,#37397);
#33068=AXIS2_PLACEMENT_3D('',#75611,#37398,#37399);
#33069=AXIS2_PLACEMENT_3D('',#75620,#37404,#37405);
#33070=AXIS2_PLACEMENT_3D('',#75626,#37409,#37410);
#33071=AXIS2_PLACEMENT_3D('',#75632,#37414,#37415);
#33072=AXIS2_PLACEMENT_3D('',#75635,#37418,#37419);
#33073=AXIS2_PLACEMENT_3D('',#75636,#37420,#37421);
#33074=AXIS2_PLACEMENT_3D('',#75645,#37426,#37427);
#33075=AXIS2_PLACEMENT_3D('',#75651,#37431,#37432);
#33076=AXIS2_PLACEMENT_3D('',#75657,#37436,#37437);
#33077=AXIS2_PLACEMENT_3D('',#75660,#37440,#37441);
#33078=AXIS2_PLACEMENT_3D('',#75661,#37442,#37443);
#33079=AXIS2_PLACEMENT_3D('',#75670,#37448,#37449);
#33080=AXIS2_PLACEMENT_3D('',#75676,#37453,#37454);
#33081=AXIS2_PLACEMENT_3D('',#75682,#37458,#37459);
#33082=AXIS2_PLACEMENT_3D('',#75685,#37462,#37463);
#33083=AXIS2_PLACEMENT_3D('',#75686,#37464,#37465);
#33084=AXIS2_PLACEMENT_3D('',#75695,#37470,#37471);
#33085=AXIS2_PLACEMENT_3D('',#75701,#37475,#37476);
#33086=AXIS2_PLACEMENT_3D('',#75707,#37480,#37481);
#33087=AXIS2_PLACEMENT_3D('',#75710,#37484,#37485);
#33088=AXIS2_PLACEMENT_3D('',#75711,#37486,#37487);
#33089=AXIS2_PLACEMENT_3D('',#75720,#37492,#37493);
#33090=AXIS2_PLACEMENT_3D('',#75726,#37497,#37498);
#33091=AXIS2_PLACEMENT_3D('',#75732,#37502,#37503);
#33092=AXIS2_PLACEMENT_3D('',#75735,#37506,#37507);
#33093=AXIS2_PLACEMENT_3D('',#75736,#37508,#37509);
#33094=AXIS2_PLACEMENT_3D('',#75745,#37514,#37515);
#33095=AXIS2_PLACEMENT_3D('',#75751,#37519,#37520);
#33096=AXIS2_PLACEMENT_3D('',#75757,#37524,#37525);
#33097=AXIS2_PLACEMENT_3D('',#75760,#37528,#37529);
#33098=AXIS2_PLACEMENT_3D('',#75761,#37530,#37531);
#33099=AXIS2_PLACEMENT_3D('',#75770,#37536,#37537);
#33100=AXIS2_PLACEMENT_3D('',#75776,#37541,#37542);
#33101=AXIS2_PLACEMENT_3D('',#75782,#37546,#37547);
#33102=AXIS2_PLACEMENT_3D('',#75785,#37550,#37551);
#33103=AXIS2_PLACEMENT_3D('',#75786,#37552,#37553);
#33104=AXIS2_PLACEMENT_3D('',#75795,#37558,#37559);
#33105=AXIS2_PLACEMENT_3D('',#75801,#37563,#37564);
#33106=AXIS2_PLACEMENT_3D('',#75807,#37568,#37569);
#33107=AXIS2_PLACEMENT_3D('',#75810,#37572,#37573);
#33108=AXIS2_PLACEMENT_3D('',#75811,#37574,#37575);
#33109=AXIS2_PLACEMENT_3D('',#75820,#37580,#37581);
#33110=AXIS2_PLACEMENT_3D('',#75826,#37585,#37586);
#33111=AXIS2_PLACEMENT_3D('',#75832,#37590,#37591);
#33112=AXIS2_PLACEMENT_3D('',#75835,#37594,#37595);
#33113=AXIS2_PLACEMENT_3D('',#75836,#37596,#37597);
#33114=AXIS2_PLACEMENT_3D('',#75845,#37602,#37603);
#33115=AXIS2_PLACEMENT_3D('',#75851,#37607,#37608);
#33116=AXIS2_PLACEMENT_3D('',#75857,#37612,#37613);
#33117=AXIS2_PLACEMENT_3D('',#75860,#37616,#37617);
#33118=AXIS2_PLACEMENT_3D('',#75861,#37618,#37619);
#33119=AXIS2_PLACEMENT_3D('',#75870,#37624,#37625);
#33120=AXIS2_PLACEMENT_3D('',#75876,#37629,#37630);
#33121=AXIS2_PLACEMENT_3D('',#75882,#37634,#37635);
#33122=AXIS2_PLACEMENT_3D('',#75885,#37638,#37639);
#33123=AXIS2_PLACEMENT_3D('',#75886,#37640,#37641);
#33124=AXIS2_PLACEMENT_3D('',#75895,#37646,#37647);
#33125=AXIS2_PLACEMENT_3D('',#75901,#37651,#37652);
#33126=AXIS2_PLACEMENT_3D('',#75907,#37656,#37657);
#33127=AXIS2_PLACEMENT_3D('',#75910,#37660,#37661);
#33128=AXIS2_PLACEMENT_3D('',#75911,#37662,#37663);
#33129=AXIS2_PLACEMENT_3D('',#75920,#37668,#37669);
#33130=AXIS2_PLACEMENT_3D('',#75926,#37673,#37674);
#33131=AXIS2_PLACEMENT_3D('',#75932,#37678,#37679);
#33132=AXIS2_PLACEMENT_3D('',#75935,#37682,#37683);
#33133=AXIS2_PLACEMENT_3D('',#75936,#37684,#37685);
#33134=AXIS2_PLACEMENT_3D('',#75945,#37690,#37691);
#33135=AXIS2_PLACEMENT_3D('',#75951,#37695,#37696);
#33136=AXIS2_PLACEMENT_3D('',#75957,#37700,#37701);
#33137=AXIS2_PLACEMENT_3D('',#75960,#37704,#37705);
#33138=AXIS2_PLACEMENT_3D('',#75961,#37706,#37707);
#33139=AXIS2_PLACEMENT_3D('',#75970,#37712,#37713);
#33140=AXIS2_PLACEMENT_3D('',#75976,#37717,#37718);
#33141=AXIS2_PLACEMENT_3D('',#75982,#37722,#37723);
#33142=AXIS2_PLACEMENT_3D('',#75985,#37726,#37727);
#33143=AXIS2_PLACEMENT_3D('',#75986,#37728,#37729);
#33144=AXIS2_PLACEMENT_3D('',#75995,#37734,#37735);
#33145=AXIS2_PLACEMENT_3D('',#76001,#37739,#37740);
#33146=AXIS2_PLACEMENT_3D('',#76007,#37744,#37745);
#33147=AXIS2_PLACEMENT_3D('',#76010,#37748,#37749);
#33148=AXIS2_PLACEMENT_3D('',#76011,#37750,#37751);
#33149=AXIS2_PLACEMENT_3D('',#76020,#37756,#37757);
#33150=AXIS2_PLACEMENT_3D('',#76026,#37761,#37762);
#33151=AXIS2_PLACEMENT_3D('',#76032,#37766,#37767);
#33152=AXIS2_PLACEMENT_3D('',#76035,#37770,#37771);
#33153=AXIS2_PLACEMENT_3D('',#76036,#37772,#37773);
#33154=AXIS2_PLACEMENT_3D('',#76045,#37778,#37779);
#33155=AXIS2_PLACEMENT_3D('',#76051,#37783,#37784);
#33156=AXIS2_PLACEMENT_3D('',#76057,#37788,#37789);
#33157=AXIS2_PLACEMENT_3D('',#76060,#37792,#37793);
#33158=AXIS2_PLACEMENT_3D('',#76061,#37794,#37795);
#33159=AXIS2_PLACEMENT_3D('',#76070,#37800,#37801);
#33160=AXIS2_PLACEMENT_3D('',#76076,#37805,#37806);
#33161=AXIS2_PLACEMENT_3D('',#76082,#37810,#37811);
#33162=AXIS2_PLACEMENT_3D('',#76085,#37814,#37815);
#33163=AXIS2_PLACEMENT_3D('',#76086,#37816,#37817);
#33164=AXIS2_PLACEMENT_3D('',#76095,#37822,#37823);
#33165=AXIS2_PLACEMENT_3D('',#76101,#37827,#37828);
#33166=AXIS2_PLACEMENT_3D('',#76107,#37832,#37833);
#33167=AXIS2_PLACEMENT_3D('',#76110,#37836,#37837);
#33168=AXIS2_PLACEMENT_3D('',#76111,#37838,#37839);
#33169=AXIS2_PLACEMENT_3D('',#76120,#37844,#37845);
#33170=AXIS2_PLACEMENT_3D('',#76126,#37849,#37850);
#33171=AXIS2_PLACEMENT_3D('',#76132,#37854,#37855);
#33172=AXIS2_PLACEMENT_3D('',#76135,#37858,#37859);
#33173=AXIS2_PLACEMENT_3D('',#76136,#37860,#37861);
#33174=AXIS2_PLACEMENT_3D('',#76145,#37866,#37867);
#33175=AXIS2_PLACEMENT_3D('',#76151,#37871,#37872);
#33176=AXIS2_PLACEMENT_3D('',#76157,#37876,#37877);
#33177=AXIS2_PLACEMENT_3D('',#76160,#37880,#37881);
#33178=AXIS2_PLACEMENT_3D('',#76161,#37882,#37883);
#33179=AXIS2_PLACEMENT_3D('',#76170,#37888,#37889);
#33180=AXIS2_PLACEMENT_3D('',#76176,#37893,#37894);
#33181=AXIS2_PLACEMENT_3D('',#76182,#37898,#37899);
#33182=AXIS2_PLACEMENT_3D('',#76185,#37902,#37903);
#33183=AXIS2_PLACEMENT_3D('',#76186,#37904,#37905);
#33184=AXIS2_PLACEMENT_3D('',#76195,#37910,#37911);
#33185=AXIS2_PLACEMENT_3D('',#76201,#37915,#37916);
#33186=AXIS2_PLACEMENT_3D('',#76207,#37920,#37921);
#33187=AXIS2_PLACEMENT_3D('',#76210,#37924,#37925);
#33188=AXIS2_PLACEMENT_3D('',#76211,#37926,#37927);
#33189=AXIS2_PLACEMENT_3D('',#76220,#37932,#37933);
#33190=AXIS2_PLACEMENT_3D('',#76226,#37937,#37938);
#33191=AXIS2_PLACEMENT_3D('',#76232,#37942,#37943);
#33192=AXIS2_PLACEMENT_3D('',#76235,#37946,#37947);
#33193=AXIS2_PLACEMENT_3D('',#76236,#37948,#37949);
#33194=AXIS2_PLACEMENT_3D('',#76245,#37954,#37955);
#33195=AXIS2_PLACEMENT_3D('',#76251,#37959,#37960);
#33196=AXIS2_PLACEMENT_3D('',#76257,#37964,#37965);
#33197=AXIS2_PLACEMENT_3D('',#76260,#37968,#37969);
#33198=AXIS2_PLACEMENT_3D('',#76261,#37970,#37971);
#33199=AXIS2_PLACEMENT_3D('',#76270,#37976,#37977);
#33200=AXIS2_PLACEMENT_3D('',#76276,#37981,#37982);
#33201=AXIS2_PLACEMENT_3D('',#76282,#37986,#37987);
#33202=AXIS2_PLACEMENT_3D('',#76285,#37990,#37991);
#33203=AXIS2_PLACEMENT_3D('',#76286,#37992,#37993);
#33204=AXIS2_PLACEMENT_3D('',#76295,#37998,#37999);
#33205=AXIS2_PLACEMENT_3D('',#76301,#38003,#38004);
#33206=AXIS2_PLACEMENT_3D('',#76307,#38008,#38009);
#33207=AXIS2_PLACEMENT_3D('',#76310,#38012,#38013);
#33208=AXIS2_PLACEMENT_3D('',#76311,#38014,#38015);
#33209=AXIS2_PLACEMENT_3D('',#76320,#38020,#38021);
#33210=AXIS2_PLACEMENT_3D('',#76326,#38025,#38026);
#33211=AXIS2_PLACEMENT_3D('',#76332,#38030,#38031);
#33212=AXIS2_PLACEMENT_3D('',#76335,#38034,#38035);
#33213=AXIS2_PLACEMENT_3D('',#76336,#38036,#38037);
#33214=AXIS2_PLACEMENT_3D('',#76345,#38042,#38043);
#33215=AXIS2_PLACEMENT_3D('',#76351,#38047,#38048);
#33216=AXIS2_PLACEMENT_3D('',#76357,#38052,#38053);
#33217=AXIS2_PLACEMENT_3D('',#76360,#38056,#38057);
#33218=AXIS2_PLACEMENT_3D('',#76361,#38058,#38059);
#33219=AXIS2_PLACEMENT_3D('',#76370,#38064,#38065);
#33220=AXIS2_PLACEMENT_3D('',#76376,#38069,#38070);
#33221=AXIS2_PLACEMENT_3D('',#76382,#38074,#38075);
#33222=AXIS2_PLACEMENT_3D('',#76385,#38078,#38079);
#33223=AXIS2_PLACEMENT_3D('',#76386,#38080,#38081);
#33224=AXIS2_PLACEMENT_3D('',#76395,#38086,#38087);
#33225=AXIS2_PLACEMENT_3D('',#76401,#38091,#38092);
#33226=AXIS2_PLACEMENT_3D('',#76407,#38096,#38097);
#33227=AXIS2_PLACEMENT_3D('',#76410,#38100,#38101);
#33228=AXIS2_PLACEMENT_3D('',#76411,#38102,#38103);
#33229=AXIS2_PLACEMENT_3D('',#76420,#38108,#38109);
#33230=AXIS2_PLACEMENT_3D('',#76426,#38113,#38114);
#33231=AXIS2_PLACEMENT_3D('',#76432,#38118,#38119);
#33232=AXIS2_PLACEMENT_3D('',#76435,#38122,#38123);
#33233=AXIS2_PLACEMENT_3D('',#76436,#38124,#38125);
#33234=AXIS2_PLACEMENT_3D('',#76445,#38130,#38131);
#33235=AXIS2_PLACEMENT_3D('',#76451,#38135,#38136);
#33236=AXIS2_PLACEMENT_3D('',#76457,#38140,#38141);
#33237=AXIS2_PLACEMENT_3D('',#76460,#38144,#38145);
#33238=AXIS2_PLACEMENT_3D('',#76461,#38146,#38147);
#33239=AXIS2_PLACEMENT_3D('',#76470,#38152,#38153);
#33240=AXIS2_PLACEMENT_3D('',#76476,#38157,#38158);
#33241=AXIS2_PLACEMENT_3D('',#76482,#38162,#38163);
#33242=AXIS2_PLACEMENT_3D('',#76485,#38166,#38167);
#33243=AXIS2_PLACEMENT_3D('',#76486,#38168,#38169);
#33244=AXIS2_PLACEMENT_3D('',#76495,#38174,#38175);
#33245=AXIS2_PLACEMENT_3D('',#76501,#38179,#38180);
#33246=AXIS2_PLACEMENT_3D('',#76507,#38184,#38185);
#33247=AXIS2_PLACEMENT_3D('',#76510,#38188,#38189);
#33248=AXIS2_PLACEMENT_3D('',#76511,#38190,#38191);
#33249=AXIS2_PLACEMENT_3D('',#76520,#38196,#38197);
#33250=AXIS2_PLACEMENT_3D('',#76526,#38201,#38202);
#33251=AXIS2_PLACEMENT_3D('',#76532,#38206,#38207);
#33252=AXIS2_PLACEMENT_3D('',#76535,#38210,#38211);
#33253=AXIS2_PLACEMENT_3D('',#76536,#38212,#38213);
#33254=AXIS2_PLACEMENT_3D('',#76545,#38218,#38219);
#33255=AXIS2_PLACEMENT_3D('',#76551,#38223,#38224);
#33256=AXIS2_PLACEMENT_3D('',#76557,#38228,#38229);
#33257=AXIS2_PLACEMENT_3D('',#76560,#38232,#38233);
#33258=AXIS2_PLACEMENT_3D('',#76561,#38234,#38235);
#33259=AXIS2_PLACEMENT_3D('',#76570,#38240,#38241);
#33260=AXIS2_PLACEMENT_3D('',#76576,#38245,#38246);
#33261=AXIS2_PLACEMENT_3D('',#76582,#38250,#38251);
#33262=AXIS2_PLACEMENT_3D('',#76585,#38254,#38255);
#33263=AXIS2_PLACEMENT_3D('',#76586,#38256,#38257);
#33264=AXIS2_PLACEMENT_3D('',#76588,#38258,#38259);
#33265=AXIS2_PLACEMENT_3D('',#76591,#38261,#38262);
#33266=AXIS2_PLACEMENT_3D('',#76592,#38263,#38264);
#33267=AXIS2_PLACEMENT_3D('',#76594,#38265,#38266);
#33268=AXIS2_PLACEMENT_3D('',#76597,#38268,#38269);
#33269=AXIS2_PLACEMENT_3D('',#76598,#38270,#38271);
#33270=AXIS2_PLACEMENT_3D('',#76607,#38276,#38277);
#33271=AXIS2_PLACEMENT_3D('',#76609,#38278,#38279);
#33272=AXIS2_PLACEMENT_3D('',#76611,#38280,#38281);
#33273=AXIS2_PLACEMENT_3D('',#76613,#38283,#38284);
#33274=AXIS2_PLACEMENT_3D('',#76619,#38288,#38289);
#33275=AXIS2_PLACEMENT_3D('',#76621,#38290,#38291);
#33276=AXIS2_PLACEMENT_3D('',#76623,#38292,#38293);
#33277=AXIS2_PLACEMENT_3D('',#76625,#38295,#38296);
#33278=AXIS2_PLACEMENT_3D('',#76631,#38300,#38301);
#33279=AXIS2_PLACEMENT_3D('',#76633,#38302,#38303);
#33280=AXIS2_PLACEMENT_3D('',#76635,#38304,#38305);
#33281=AXIS2_PLACEMENT_3D('',#76637,#38307,#38308);
#33282=AXIS2_PLACEMENT_3D('',#76643,#38312,#38313);
#33283=AXIS2_PLACEMENT_3D('',#76644,#38314,#38315);
#33284=AXIS2_PLACEMENT_3D('',#76645,#38316,#38317);
#33285=AXIS2_PLACEMENT_3D('',#76646,#38318,#38319);
#33286=AXIS2_PLACEMENT_3D('',#76647,#38320,#38321);
#33287=AXIS2_PLACEMENT_3D('',#76648,#38322,#38323);
#33288=AXIS2_PLACEMENT_3D('',#76649,#38324,#38325);
#33289=AXIS2_PLACEMENT_3D('',#76658,#38330,#38331);
#33290=AXIS2_PLACEMENT_3D('',#76664,#38335,#38336);
#33291=AXIS2_PLACEMENT_3D('',#76670,#38340,#38341);
#33292=AXIS2_PLACEMENT_3D('',#76673,#38344,#38345);
#33293=AXIS2_PLACEMENT_3D('',#76674,#38346,#38347);
#33294=AXIS2_PLACEMENT_3D('',#76683,#38352,#38353);
#33295=AXIS2_PLACEMENT_3D('',#76689,#38357,#38358);
#33296=AXIS2_PLACEMENT_3D('',#76695,#38362,#38363);
#33297=AXIS2_PLACEMENT_3D('',#76698,#38366,#38367);
#33298=AXIS2_PLACEMENT_3D('',#76699,#38368,#38369);
#33299=AXIS2_PLACEMENT_3D('',#76708,#38374,#38375);
#33300=AXIS2_PLACEMENT_3D('',#76714,#38379,#38380);
#33301=AXIS2_PLACEMENT_3D('',#76720,#38384,#38385);
#33302=AXIS2_PLACEMENT_3D('',#76723,#38388,#38389);
#33303=AXIS2_PLACEMENT_3D('',#76724,#38390,#38391);
#33304=AXIS2_PLACEMENT_3D('',#76733,#38396,#38397);
#33305=AXIS2_PLACEMENT_3D('',#76739,#38401,#38402);
#33306=AXIS2_PLACEMENT_3D('',#76745,#38406,#38407);
#33307=AXIS2_PLACEMENT_3D('',#76748,#38410,#38411);
#33308=AXIS2_PLACEMENT_3D('',#76749,#38412,#38413);
#33309=AXIS2_PLACEMENT_3D('',#76758,#38418,#38419);
#33310=AXIS2_PLACEMENT_3D('',#76764,#38423,#38424);
#33311=AXIS2_PLACEMENT_3D('',#76770,#38428,#38429);
#33312=AXIS2_PLACEMENT_3D('',#76773,#38432,#38433);
#33313=AXIS2_PLACEMENT_3D('',#76774,#38434,#38435);
#33314=AXIS2_PLACEMENT_3D('',#76783,#38440,#38441);
#33315=AXIS2_PLACEMENT_3D('',#76789,#38445,#38446);
#33316=AXIS2_PLACEMENT_3D('',#76795,#38450,#38451);
#33317=AXIS2_PLACEMENT_3D('',#76798,#38454,#38455);
#33318=AXIS2_PLACEMENT_3D('',#76799,#38456,#38457);
#33319=AXIS2_PLACEMENT_3D('',#76808,#38462,#38463);
#33320=AXIS2_PLACEMENT_3D('',#76814,#38467,#38468);
#33321=AXIS2_PLACEMENT_3D('',#76820,#38472,#38473);
#33322=AXIS2_PLACEMENT_3D('',#76823,#38476,#38477);
#33323=AXIS2_PLACEMENT_3D('',#76824,#38478,#38479);
#33324=AXIS2_PLACEMENT_3D('',#76833,#38484,#38485);
#33325=AXIS2_PLACEMENT_3D('',#76839,#38489,#38490);
#33326=AXIS2_PLACEMENT_3D('',#76845,#38494,#38495);
#33327=AXIS2_PLACEMENT_3D('',#76848,#38498,#38499);
#33328=AXIS2_PLACEMENT_3D('',#76849,#38500,#38501);
#33329=AXIS2_PLACEMENT_3D('',#76858,#38506,#38507);
#33330=AXIS2_PLACEMENT_3D('',#76864,#38511,#38512);
#33331=AXIS2_PLACEMENT_3D('',#76870,#38516,#38517);
#33332=AXIS2_PLACEMENT_3D('',#76873,#38520,#38521);
#33333=AXIS2_PLACEMENT_3D('',#76874,#38522,#38523);
#33334=AXIS2_PLACEMENT_3D('',#76883,#38528,#38529);
#33335=AXIS2_PLACEMENT_3D('',#76889,#38533,#38534);
#33336=AXIS2_PLACEMENT_3D('',#76895,#38538,#38539);
#33337=AXIS2_PLACEMENT_3D('',#76898,#38542,#38543);
#33338=AXIS2_PLACEMENT_3D('',#76899,#38544,#38545);
#33339=AXIS2_PLACEMENT_3D('',#76908,#38550,#38551);
#33340=AXIS2_PLACEMENT_3D('',#76914,#38555,#38556);
#33341=AXIS2_PLACEMENT_3D('',#76920,#38560,#38561);
#33342=AXIS2_PLACEMENT_3D('',#76923,#38564,#38565);
#33343=AXIS2_PLACEMENT_3D('',#76924,#38566,#38567);
#33344=AXIS2_PLACEMENT_3D('',#76926,#38568,#38569);
#33345=AXIS2_PLACEMENT_3D('',#76929,#38571,#38572);
#33346=AXIS2_PLACEMENT_3D('',#76930,#38573,#38574);
#33347=AXIS2_PLACEMENT_3D('',#76932,#38575,#38576);
#33348=AXIS2_PLACEMENT_3D('',#76935,#38578,#38579);
#33349=AXIS2_PLACEMENT_3D('',#76936,#38580,#38581);
#33350=AXIS2_PLACEMENT_3D('',#76945,#38586,#38587);
#33351=AXIS2_PLACEMENT_3D('',#76951,#38591,#38592);
#33352=AXIS2_PLACEMENT_3D('',#76957,#38596,#38597);
#33353=AXIS2_PLACEMENT_3D('',#76963,#38601,#38602);
#33354=AXIS2_PLACEMENT_3D('',#76969,#38606,#38607);
#33355=AXIS2_PLACEMENT_3D('',#76975,#38611,#38612);
#33356=AXIS2_PLACEMENT_3D('',#76981,#38616,#38617);
#33357=AXIS2_PLACEMENT_3D('',#76984,#38620,#38621);
#33358=AXIS2_PLACEMENT_3D('',#76985,#38622,#38623);
#33359=AXIS2_PLACEMENT_3D('',#76986,#38624,#38625);
#33360=AXIS2_PLACEMENT_3D('',#76987,#38626,#38627);
#33361=AXIS2_PLACEMENT_3D('',#76994,#38628,#38629);
#33362=AXIS2_PLACEMENT_3D('',#76999,#38630,#38631);
#33363=AXIS2_PLACEMENT_3D('',#77000,#38632,#38633);
#33364=AXIS2_PLACEMENT_3D('',#77004,#38635,#38636);
#33365=AXIS2_PLACEMENT_3D('',#77018,#38643,#38644);
#33366=AXIS2_PLACEMENT_3D('',#77021,#38646,#38647);
#33367=AXIS2_PLACEMENT_3D('',#77026,#38649,#38650);
#33368=AXIS2_PLACEMENT_3D('',#77029,#38652,#38653);
#33369=AXIS2_PLACEMENT_3D('',#77030,#38654,#38655);
#33370=AXIS2_PLACEMENT_3D('',#77039,#38656,#38657);
#33371=AXIS2_PLACEMENT_3D('',#77040,#38658,#38659);
#33372=AXIS2_PLACEMENT_3D('',#77056,#38669,#38670);
#33373=AXIS2_PLACEMENT_3D('',#77057,#38671,#38672);
#33374=AXIS2_PLACEMENT_3D('',#77058,#38673,#38674);
#33375=AXIS2_PLACEMENT_3D('',#77060,#38675,#38676);
#33376=AXIS2_PLACEMENT_3D('',#77061,#38677,#38678);
#33377=AXIS2_PLACEMENT_3D('',#77062,#38679,#38680);
#33378=AXIS2_PLACEMENT_3D('',#77063,#38681,#38682);
#33379=AXIS2_PLACEMENT_3D('',#77065,#38683,#38684);
#33380=AXIS2_PLACEMENT_3D('',#77066,#38685,#38686);
#33381=AXIS2_PLACEMENT_3D('',#77070,#38688,#38689);
#33382=AXIS2_PLACEMENT_3D('',#77072,#38690,#38691);
#33383=AXIS2_PLACEMENT_3D('',#77073,#38692,#38693);
#33384=AXIS2_PLACEMENT_3D('',#77074,#38694,#38695);
#33385=AXIS2_PLACEMENT_3D('',#77078,#38697,#38698);
#33386=AXIS2_PLACEMENT_3D('',#77080,#38699,#38700);
#33387=AXIS2_PLACEMENT_3D('',#77081,#38701,#38702);
#33388=AXIS2_PLACEMENT_3D('',#77082,#38703,#38704);
#33389=AXIS2_PLACEMENT_3D('',#77090,#38710,#38711);
#33390=AXIS2_PLACEMENT_3D('',#77096,#38715,#38716);
#33391=AXIS2_PLACEMENT_3D('',#77099,#38717,#38718);
#33392=AXIS2_PLACEMENT_3D('',#77101,#38719,#38720);
#33393=AXIS2_PLACEMENT_3D('',#77103,#38722,#38723);
#33394=AXIS2_PLACEMENT_3D('',#77104,#38724,#38725);
#33395=AXIS2_PLACEMENT_3D('',#77108,#38728,#38729);
#33396=AXIS2_PLACEMENT_3D('',#77109,#38730,#38731);
#33397=AXIS2_PLACEMENT_3D('',#77110,#38732,#38733);
#33398=AXIS2_PLACEMENT_3D('',#77116,#38737,#38738);
#33399=AXIS2_PLACEMENT_3D('',#77119,#38739,#38740);
#33400=AXIS2_PLACEMENT_3D('',#77121,#38741,#38742);
#33401=AXIS2_PLACEMENT_3D('',#77123,#38744,#38745);
#33402=AXIS2_PLACEMENT_3D('',#77124,#38746,#38747);
#33403=AXIS2_PLACEMENT_3D('',#77128,#38750,#38751);
#33404=AXIS2_PLACEMENT_3D('',#77129,#38752,#38753);
#33405=AXIS2_PLACEMENT_3D('',#77130,#38754,#38755);
#33406=AXIS2_PLACEMENT_3D('',#77138,#38761,#38762);
#33407=AXIS2_PLACEMENT_3D('',#77142,#38765,#38766);
#33408=AXIS2_PLACEMENT_3D('',#77146,#38769,#38770);
#33409=AXIS2_PLACEMENT_3D('',#77148,#38772,#38773);
#33410=AXIS2_PLACEMENT_3D('',#77151,#38776,#38777);
#33411=AXIS2_PLACEMENT_3D('',#77152,#38778,#38779);
#33412=AXIS2_PLACEMENT_3D('',#77153,#38780,#38781);
#33413=AXIS2_PLACEMENT_3D('',#77154,#38782,#38783);
#33414=AXIS2_PLACEMENT_3D('',#77218,#38785,#38786);
#33415=AXIS2_PLACEMENT_3D('',#77250,#38787,#38788);
#33416=AXIS2_PLACEMENT_3D('',#77640,#38790,#38791);
#33417=AXIS2_PLACEMENT_3D('',#78039,#38793,#38794);
#33418=AXIS2_PLACEMENT_3D('',#78419,#38796,#38797);
#33419=AXIS2_PLACEMENT_3D('',#78774,#38799,#38800);
#33420=AXIS2_PLACEMENT_3D('',#79140,#38802,#38803);
#33421=AXIS2_PLACEMENT_3D('',#79499,#38805,#38806);
#33422=AXIS2_PLACEMENT_3D('',#79883,#38808,#38809);
#33423=AXIS2_PLACEMENT_3D('',#80253,#38811,#38812);
#33424=AXIS2_PLACEMENT_3D('',#80389,#38814,#38815);
#33425=AXIS2_PLACEMENT_3D('',#80486,#38816,#38817);
#33426=AXIS2_PLACEMENT_3D('',#80832,#38819,#38820);
#33427=AXIS2_PLACEMENT_3D('',#81166,#38822,#38823);
#33428=AXIS2_PLACEMENT_3D('',#81503,#38825,#38826);
#33429=AXIS2_PLACEMENT_3D('',#81841,#38828,#38829);
#33430=AXIS2_PLACEMENT_3D('',#82191,#38831,#38832);
#33431=AXIS2_PLACEMENT_3D('',#82540,#38834,#38835);
#33432=AXIS2_PLACEMENT_3D('',#82868,#38837,#38838);
#33433=AXIS2_PLACEMENT_3D('',#83027,#38839,#38840);
#33434=AXIS2_PLACEMENT_3D('',#83150,#38841,#38842);
#33435=AXIS2_PLACEMENT_3D('',#83215,#38843,#38844);
#33436=AXIS2_PLACEMENT_3D('',#83256,#38845,#38846);
#33437=AXIS2_PLACEMENT_3D('',#83259,#38847,#38848);
#33438=AXIS2_PLACEMENT_3D('',#83356,#38849,#38850);
#33439=AXIS2_PLACEMENT_3D('',#83689,#38851,#38852);
#33440=AXIS2_PLACEMENT_3D('',#83691,#38853,#38854);
#33441=AXIS2_PLACEMENT_3D('',#83693,#38855,#38856);
#33442=AXIS2_PLACEMENT_3D('',#84018,#38857,#38858);
#33443=AXIS2_PLACEMENT_3D('',#84025,#38859,#38860);
#33444=AXIS2_PLACEMENT_3D('',#84035,#38861,#38862);
#33445=AXIS2_PLACEMENT_3D('',#84045,#38863,#38864);
#33446=AXIS2_PLACEMENT_3D('',#84055,#38865,#38866);
#33447=AXIS2_PLACEMENT_3D('',#84065,#38867,#38868);
#33448=AXIS2_PLACEMENT_3D('',#84075,#38869,#38870);
#33449=AXIS2_PLACEMENT_3D('',#84081,#38872,#38873);
#33450=AXIS2_PLACEMENT_3D('',#84082,#38874,#38875);
#33451=AXIS2_PLACEMENT_3D('',#84087,#38878,#38879);
#33452=AXIS2_PLACEMENT_3D('',#84088,#38880,#38881);
#33453=AXIS2_PLACEMENT_3D('',#84092,#38883,#38884);
#33454=AXIS2_PLACEMENT_3D('',#84094,#38886,#38887);
#33455=AXIS2_PLACEMENT_3D('',#84099,#38890,#38891);
#33456=AXIS2_PLACEMENT_3D('',#84100,#38892,#38893);
#33457=AXIS2_PLACEMENT_3D('',#84104,#38895,#38896);
#33458=AXIS2_PLACEMENT_3D('',#84106,#38898,#38899);
#33459=AXIS2_PLACEMENT_3D('',#84111,#38902,#38903);
#33460=AXIS2_PLACEMENT_3D('',#84112,#38904,#38905);
#33461=AXIS2_PLACEMENT_3D('',#84116,#38907,#38908);
#33462=AXIS2_PLACEMENT_3D('',#84118,#38910,#38911);
#33463=AXIS2_PLACEMENT_3D('',#84125,#38916,#38917);
#33464=AXIS2_PLACEMENT_3D('',#84130,#38921,#38922);
#33465=AXIS2_PLACEMENT_3D('',#84135,#38926,#38927);
#33466=AXIS2_PLACEMENT_3D('',#84136,#38928,#38929);
#33467=AXIS2_PLACEMENT_3D('',#84137,#38930,#38931);
#33468=AXIS2_PLACEMENT_3D('',#84139,#38933,#38934);
#33469=AXIS2_PLACEMENT_3D('',#84140,#38935,#38936);
#33470=AXIS2_PLACEMENT_3D('',#84142,#38938,#38939);
#33471=AXIS2_PLACEMENT_3D('',#84144,#38941,#38942);
#33472=AXIS2_PLACEMENT_3D('',#84148,#38944,#38945);
#33473=AXIS2_PLACEMENT_3D('',#84149,#38946,#38947);
#33474=AXIS2_PLACEMENT_3D('',#84151,#38949,#38950);
#33475=AXIS2_PLACEMENT_3D('',#84152,#38951,#38952);
#33476=AXIS2_PLACEMENT_3D('',#84153,#38953,#38954);
#33477=AXIS2_PLACEMENT_3D('',#84154,#38955,#38956);
#33478=AXIS2_PLACEMENT_3D('',#84155,#38957,#38958);
#33479=AXIS2_PLACEMENT_3D('',#84156,#38959,#38960);
#33480=AXIS2_PLACEMENT_3D('',#84157,#38961,#38962);
#33481=AXIS2_PLACEMENT_3D('',#84158,#38963,#38964);
#33482=AXIS2_PLACEMENT_3D('',#84160,#38966,#38967);
#33483=AXIS2_PLACEMENT_3D('',#84161,#38968,#38969);
#33484=AXIS2_PLACEMENT_3D('',#84164,#38971,#38972);
#33485=AXIS2_PLACEMENT_3D('',#84167,#38975,#38976);
#33486=AXIS2_PLACEMENT_3D('',#84168,#38977,#38978);
#33487=AXIS2_PLACEMENT_3D('',#84169,#38979,#38980);
#33488=AXIS2_PLACEMENT_3D('',#84171,#38981,#38982);
#33489=AXIS2_PLACEMENT_3D('',#84172,#38983,#38984);
#33490=AXIS2_PLACEMENT_3D('',#84174,#38986,#38987);
#33491=AXIS2_PLACEMENT_3D('',#84177,#38989,#38990);
#33492=AXIS2_PLACEMENT_3D('',#84178,#38991,#38992);
#33493=AXIS2_PLACEMENT_3D('',#84179,#38993,#38994);
#33494=AXIS2_PLACEMENT_3D('',#84180,#38995,#38996);
#33495=AXIS2_PLACEMENT_3D('',#84182,#38997,#38998);
#33496=AXIS2_PLACEMENT_3D('',#84185,#39000,#39001);
#33497=AXIS2_PLACEMENT_3D('',#84186,#39002,#39003);
#33498=AXIS2_PLACEMENT_3D('',#84190,#39005,#39006);
#33499=AXIS2_PLACEMENT_3D('',#84191,#39007,#39008);
#33500=AXIS2_PLACEMENT_3D('',#84192,#39009,#39010);
#33501=AXIS2_PLACEMENT_3D('',#84201,#39015,#39016);
#33502=AXIS2_PLACEMENT_3D('',#84204,#39018,#39019);
#33503=AXIS2_PLACEMENT_3D('',#84206,#39020,#39021);
#33504=AXIS2_PLACEMENT_3D('',#84209,#39023,#39024);
#33505=AXIS2_PLACEMENT_3D('',#84210,#39025,#39026);
#33506=AXIS2_PLACEMENT_3D('',#84214,#39028,#39029);
#33507=AXIS2_PLACEMENT_3D('',#84215,#39030,#39031);
#33508=AXIS2_PLACEMENT_3D('',#84216,#39032,#39033);
#33509=AXIS2_PLACEMENT_3D('',#84225,#39038,#39039);
#33510=AXIS2_PLACEMENT_3D('',#84228,#39041,#39042);
#33511=AXIS2_PLACEMENT_3D('',#84230,#39043,#39044);
#33512=AXIS2_PLACEMENT_3D('',#84233,#39046,#39047);
#33513=AXIS2_PLACEMENT_3D('',#84234,#39048,#39049);
#33514=AXIS2_PLACEMENT_3D('',#84246,#39056,#39057);
#33515=AXIS2_PLACEMENT_3D('',#84248,#39058,#39059);
#33516=AXIS2_PLACEMENT_3D('',#84250,#39060,#39061);
#33517=AXIS2_PLACEMENT_3D('',#84252,#39062,#39063);
#33518=AXIS2_PLACEMENT_3D('',#84253,#39064,#39065);
#33519=AXIS2_PLACEMENT_3D('',#84256,#39067,#39068);
#33520=AXIS2_PLACEMENT_3D('',#84257,#39069,#39070);
#33521=AXIS2_PLACEMENT_3D('',#84259,#39071,#39072);
#33522=AXIS2_PLACEMENT_3D('',#84261,#39074,#39075);
#33523=AXIS2_PLACEMENT_3D('',#84264,#39077,#39078);
#33524=AXIS2_PLACEMENT_3D('',#84265,#39079,#39080);
#33525=AXIS2_PLACEMENT_3D('',#84268,#39082,#39083);
#33526=AXIS2_PLACEMENT_3D('',#84271,#39085,#39086);
#33527=AXIS2_PLACEMENT_3D('',#84273,#39087,#39088);
#33528=AXIS2_PLACEMENT_3D('',#84275,#39090,#39091);
#33529=AXIS2_PLACEMENT_3D('',#84278,#39093,#39094);
#33530=AXIS2_PLACEMENT_3D('',#84279,#39095,#39096);
#33531=AXIS2_PLACEMENT_3D('',#84281,#39097,#39098);
#33532=AXIS2_PLACEMENT_3D('',#84283,#39100,#39101);
#33533=AXIS2_PLACEMENT_3D('',#84286,#39103,#39104);
#33534=AXIS2_PLACEMENT_3D('',#84287,#39105,#39106);
#33535=AXIS2_PLACEMENT_3D('',#84289,#39107,#39108);
#33536=AXIS2_PLACEMENT_3D('',#84290,#39109,#39110);
#33537=AXIS2_PLACEMENT_3D('',#84292,#39111,#39112);
#33538=AXIS2_PLACEMENT_3D('',#84293,#39113,#39114);
#33539=AXIS2_PLACEMENT_3D('',#84296,#39116,#39117);
#33540=AXIS2_PLACEMENT_3D('',#84297,#39118,#39119);
#33541=AXIS2_PLACEMENT_3D('',#84300,#39121,#39122);
#33542=AXIS2_PLACEMENT_3D('',#84301,#39123,#39124);
#33543=AXIS2_PLACEMENT_3D('',#84303,#39125,#39126);
#33544=AXIS2_PLACEMENT_3D('',#84306,#39128,#39129);
#33545=AXIS2_PLACEMENT_3D('',#84307,#39130,#39131);
#33546=AXIS2_PLACEMENT_3D('',#84309,#39132,#39133);
#33547=AXIS2_PLACEMENT_3D('',#84311,#39135,#39136);
#33548=AXIS2_PLACEMENT_3D('',#84322,#39143,#39144);
#33549=AXIS2_PLACEMENT_3D('',#84324,#39146,#39147);
#33550=AXIS2_PLACEMENT_3D('',#84326,#39149,#39150);
#33551=AXIS2_PLACEMENT_3D('',#84328,#39152,#39153);
#33552=AXIS2_PLACEMENT_3D('',#84330,#39155,#39156);
#33553=AXIS2_PLACEMENT_3D('',#84332,#39158,#39159);
#33554=AXIS2_PLACEMENT_3D('',#84333,#39160,#39161);
#33555=AXIS2_PLACEMENT_3D('',#84334,#39162,#39163);
#33556=AXIS2_PLACEMENT_3D('',#84335,#39164,#39165);
#33557=AXIS2_PLACEMENT_3D('',#84411,#39167,#39168);
#33558=AXIS2_PLACEMENT_3D('',#84443,#39169,#39170);
#33559=AXIS2_PLACEMENT_3D('',#84869,#39172,#39173);
#33560=AXIS2_PLACEMENT_3D('',#85329,#39175,#39176);
#33561=AXIS2_PLACEMENT_3D('',#85819,#39178,#39179);
#33562=AXIS2_PLACEMENT_3D('',#86285,#39181,#39182);
#33563=AXIS2_PLACEMENT_3D('',#86745,#39184,#39185);
#33564=AXIS2_PLACEMENT_3D('',#87215,#39187,#39188);
#33565=AXIS2_PLACEMENT_3D('',#87699,#39190,#39191);
#33566=AXIS2_PLACEMENT_3D('',#88163,#39193,#39194);
#33567=AXIS2_PLACEMENT_3D('',#88637,#39196,#39197);
#33568=AXIS2_PLACEMENT_3D('',#89105,#39199,#39200);
#33569=AXIS2_PLACEMENT_3D('',#89563,#39202,#39203);
#33570=AXIS2_PLACEMENT_3D('',#90005,#39205,#39206);
#33571=AXIS2_PLACEMENT_3D('',#90481,#39208,#39209);
#33572=AXIS2_PLACEMENT_3D('',#90945,#39211,#39212);
#33573=AXIS2_PLACEMENT_3D('',#91389,#39214,#39215);
#33574=AXIS2_PLACEMENT_3D('',#91865,#39217,#39218);
#33575=AXIS2_PLACEMENT_3D('',#92309,#39220,#39221);
#33576=AXIS2_PLACEMENT_3D('',#92783,#39223,#39224);
#33577=AXIS2_PLACEMENT_3D('',#93289,#39226,#39227);
#33578=AXIS2_PLACEMENT_3D('',#93759,#39229,#39230);
#33579=AXIS2_PLACEMENT_3D('',#94223,#39232,#39233);
#33580=AXIS2_PLACEMENT_3D('',#94684,#39235,#39236);
#33581=AXIS2_PLACEMENT_3D('',#94804,#39238,#39239);
#33582=AXIS2_PLACEMENT_3D('',#94887,#39240,#39241);
#33583=AXIS2_PLACEMENT_3D('',#95361,#39243,#39244);
#33584=AXIS2_PLACEMENT_3D('',#95791,#39246,#39247);
#33585=AXIS2_PLACEMENT_3D('',#96219,#39249,#39250);
#33586=AXIS2_PLACEMENT_3D('',#96662,#39252,#39253);
#33587=AXIS2_PLACEMENT_3D('',#97103,#39255,#39256);
#33588=AXIS2_PLACEMENT_3D('',#97545,#39258,#39259);
#33589=AXIS2_PLACEMENT_3D('',#97969,#39261,#39262);
#33590=AXIS2_PLACEMENT_3D('',#98395,#39264,#39265);
#33591=AXIS2_PLACEMENT_3D('',#98843,#39267,#39268);
#33592=AXIS2_PLACEMENT_3D('',#99301,#39270,#39271);
#33593=AXIS2_PLACEMENT_3D('',#99727,#39273,#39274);
#33594=AXIS2_PLACEMENT_3D('',#100159,#39276,#39277);
#33595=AXIS2_PLACEMENT_3D('',#100583,#39279,#39280);
#33596=AXIS2_PLACEMENT_3D('',#101040,#39282,#39283);
#33597=AXIS2_PLACEMENT_3D('',#101458,#39285,#39286);
#33598=AXIS2_PLACEMENT_3D('',#101882,#39288,#39289);
#33599=AXIS2_PLACEMENT_3D('',#102318,#39291,#39292);
#33600=AXIS2_PLACEMENT_3D('',#102736,#39294,#39295);
#33601=AXIS2_PLACEMENT_3D('',#103174,#39297,#39298);
#33602=AXIS2_PLACEMENT_3D('',#103633,#39300,#39301);
#33603=AXIS2_PLACEMENT_3D('',#104047,#39303,#39304);
#33604=AXIS2_PLACEMENT_3D('',#104513,#39306,#39307);
#33605=AXIS2_PLACEMENT_3D('',#104702,#39308,#39309);
#33606=AXIS2_PLACEMENT_3D('',#104833,#39310,#39311);
#33607=AXIS2_PLACEMENT_3D('',#105072,#39312,#39313);
#33608=AXIS2_PLACEMENT_3D('',#105239,#39314,#39315);
#33609=AXIS2_PLACEMENT_3D('',#105242,#39316,#39317);
#33610=AXIS2_PLACEMENT_3D('',#105336,#39318,#39319);
#33611=AXIS2_PLACEMENT_3D('',#105961,#39320,#39321);
#33612=AXIS2_PLACEMENT_3D('',#105964,#39322,#39323);
#33613=AXIS2_PLACEMENT_3D('',#106044,#39324,#39325);
#33614=AXIS2_PLACEMENT_3D('',#106655,#39326,#39327);
#33615=AXIS2_PLACEMENT_3D('',#106657,#39328,#39329);
#33616=AXIS2_PLACEMENT_3D('',#106658,#39330,#39331);
#33617=AXIS2_PLACEMENT_3D('',#106659,#39332,#39333);
#33618=AXIS2_PLACEMENT_3D('',#106661,#39334,#39335);
#33619=AXIS2_PLACEMENT_3D('',#106662,#39336,#39337);
#33620=AXIS2_PLACEMENT_3D('',#106665,#39339,#39340);
#33621=AXIS2_PLACEMENT_3D('',#106666,#39341,#39342);
#33622=AXIS2_PLACEMENT_3D('',#106667,#39343,#39344);
#33623=AXIS2_PLACEMENT_3D('',#106670,#39345,#39346);
#33624=AXIS2_PLACEMENT_3D('',#106674,#39349,#39350);
#33625=AXIS2_PLACEMENT_3D('',#106682,#39353,#39354);
#33626=AXIS2_PLACEMENT_3D('',#106688,#39356,#39357);
#33627=AXIS2_PLACEMENT_3D('',#106691,#39358,#39359);
#33628=AXIS2_PLACEMENT_3D('',#106695,#39361,#39362);
#33629=AXIS2_PLACEMENT_3D('',#106696,#39363,#39364);
#33630=AXIS2_PLACEMENT_3D('',#106698,#39365,#39366);
#33631=AXIS2_PLACEMENT_3D('',#106702,#39368,#39369);
#33632=AXIS2_PLACEMENT_3D('',#106706,#39371,#39372);
#33633=AXIS2_PLACEMENT_3D('',#106710,#39374,#39375);
#33634=AXIS2_PLACEMENT_3D('',#106714,#39377,#39378);
#33635=AXIS2_PLACEMENT_3D('',#106718,#39380,#39381);
#33636=AXIS2_PLACEMENT_3D('',#106722,#39383,#39384);
#33637=AXIS2_PLACEMENT_3D('',#106726,#39386,#39387);
#33638=AXIS2_PLACEMENT_3D('',#106730,#39389,#39390);
#33639=AXIS2_PLACEMENT_3D('',#106734,#39392,#39393);
#33640=AXIS2_PLACEMENT_3D('',#106738,#39395,#39396);
#33641=AXIS2_PLACEMENT_3D('',#106742,#39398,#39399);
#33642=AXIS2_PLACEMENT_3D('',#106746,#39401,#39402);
#33643=AXIS2_PLACEMENT_3D('',#106750,#39404,#39405);
#33644=AXIS2_PLACEMENT_3D('',#106754,#39407,#39408);
#33645=AXIS2_PLACEMENT_3D('',#106758,#39410,#39411);
#33646=AXIS2_PLACEMENT_3D('',#106762,#39413,#39414);
#33647=AXIS2_PLACEMENT_3D('',#106766,#39416,#39417);
#33648=AXIS2_PLACEMENT_3D('',#106770,#39419,#39420);
#33649=AXIS2_PLACEMENT_3D('',#106774,#39422,#39423);
#33650=AXIS2_PLACEMENT_3D('',#106778,#39425,#39426);
#33651=AXIS2_PLACEMENT_3D('',#106782,#39428,#39429);
#33652=AXIS2_PLACEMENT_3D('',#106786,#39431,#39432);
#33653=AXIS2_PLACEMENT_3D('',#106790,#39434,#39435);
#33654=AXIS2_PLACEMENT_3D('',#106794,#39437,#39438);
#33655=AXIS2_PLACEMENT_3D('',#106798,#39440,#39441);
#33656=AXIS2_PLACEMENT_3D('',#106802,#39443,#39444);
#33657=AXIS2_PLACEMENT_3D('',#106806,#39446,#39447);
#33658=AXIS2_PLACEMENT_3D('',#106810,#39449,#39450);
#33659=AXIS2_PLACEMENT_3D('',#106814,#39452,#39453);
#33660=AXIS2_PLACEMENT_3D('',#106818,#39455,#39456);
#33661=AXIS2_PLACEMENT_3D('',#106822,#39458,#39459);
#33662=AXIS2_PLACEMENT_3D('',#106826,#39461,#39462);
#33663=AXIS2_PLACEMENT_3D('',#106829,#39464,#39465);
#33664=AXIS2_PLACEMENT_3D('',#106831,#39466,#39467);
#33665=AXIS2_PLACEMENT_3D('',#106835,#39469,#39470);
#33666=AXIS2_PLACEMENT_3D('',#106839,#39472,#39473);
#33667=AXIS2_PLACEMENT_3D('',#106843,#39475,#39476);
#33668=AXIS2_PLACEMENT_3D('',#106847,#39478,#39479);
#33669=AXIS2_PLACEMENT_3D('',#106851,#39481,#39482);
#33670=AXIS2_PLACEMENT_3D('',#106855,#39484,#39485);
#33671=AXIS2_PLACEMENT_3D('',#106859,#39487,#39488);
#33672=AXIS2_PLACEMENT_3D('',#106863,#39490,#39491);
#33673=AXIS2_PLACEMENT_3D('',#106867,#39493,#39494);
#33674=AXIS2_PLACEMENT_3D('',#106871,#39496,#39497);
#33675=AXIS2_PLACEMENT_3D('',#106875,#39499,#39500);
#33676=AXIS2_PLACEMENT_3D('',#106879,#39502,#39503);
#33677=AXIS2_PLACEMENT_3D('',#106883,#39505,#39506);
#33678=AXIS2_PLACEMENT_3D('',#106887,#39508,#39509);
#33679=AXIS2_PLACEMENT_3D('',#106891,#39511,#39512);
#33680=AXIS2_PLACEMENT_3D('',#106895,#39514,#39515);
#33681=AXIS2_PLACEMENT_3D('',#106899,#39517,#39518);
#33682=AXIS2_PLACEMENT_3D('',#106903,#39520,#39521);
#33683=AXIS2_PLACEMENT_3D('',#106907,#39523,#39524);
#33684=AXIS2_PLACEMENT_3D('',#106911,#39526,#39527);
#33685=AXIS2_PLACEMENT_3D('',#106915,#39529,#39530);
#33686=AXIS2_PLACEMENT_3D('',#106919,#39532,#39533);
#33687=AXIS2_PLACEMENT_3D('',#106923,#39535,#39536);
#33688=AXIS2_PLACEMENT_3D('',#106927,#39538,#39539);
#33689=AXIS2_PLACEMENT_3D('',#106931,#39541,#39542);
#33690=AXIS2_PLACEMENT_3D('',#106935,#39544,#39545);
#33691=AXIS2_PLACEMENT_3D('',#106939,#39547,#39548);
#33692=AXIS2_PLACEMENT_3D('',#106943,#39550,#39551);
#33693=AXIS2_PLACEMENT_3D('',#106947,#39553,#39554);
#33694=AXIS2_PLACEMENT_3D('',#106951,#39556,#39557);
#33695=AXIS2_PLACEMENT_3D('',#106955,#39559,#39560);
#33696=AXIS2_PLACEMENT_3D('',#106959,#39562,#39563);
#33697=AXIS2_PLACEMENT_3D('',#106963,#39565,#39566);
#33698=AXIS2_PLACEMENT_3D('',#106967,#39568,#39569);
#33699=AXIS2_PLACEMENT_3D('',#106971,#39571,#39572);
#33700=AXIS2_PLACEMENT_3D('',#106975,#39574,#39575);
#33701=AXIS2_PLACEMENT_3D('',#106977,#39577,#39578);
#33702=AXIS2_PLACEMENT_3D('',#106985,#39581,#39582);
#33703=AXIS2_PLACEMENT_3D('',#106990,#39584,#39585);
#33704=AXIS2_PLACEMENT_3D('',#106991,#39586,#39587);
#33705=AXIS2_PLACEMENT_3D('',#107232,#39589,#39590);
#33706=AXIS2_PLACEMENT_3D('',#107233,#39591,#39592);
#33707=AXIS2_PLACEMENT_3D('',#107237,#39595,#39596);
#33708=AXIS2_PLACEMENT_3D('',#107239,#39598,#39599);
#33709=AXIS2_PLACEMENT_3D('',#107240,#39600,#39601);
#33710=AXIS2_PLACEMENT_3D('',#107244,#39604,#39605);
#33711=AXIS2_PLACEMENT_3D('',#107246,#39607,#39608);
#33712=AXIS2_PLACEMENT_3D('',#107247,#39609,#39610);
#33713=AXIS2_PLACEMENT_3D('',#107251,#39613,#39614);
#33714=AXIS2_PLACEMENT_3D('',#107253,#39616,#39617);
#33715=AXIS2_PLACEMENT_3D('',#107254,#39618,#39619);
#33716=AXIS2_PLACEMENT_3D('',#107258,#39622,#39623);
#33717=AXIS2_PLACEMENT_3D('',#107260,#39625,#39626);
#33718=AXIS2_PLACEMENT_3D('',#107261,#39627,#39628);
#33719=AXIS2_PLACEMENT_3D('',#107265,#39631,#39632);
#33720=AXIS2_PLACEMENT_3D('',#107267,#39634,#39635);
#33721=AXIS2_PLACEMENT_3D('',#107268,#39636,#39637);
#33722=AXIS2_PLACEMENT_3D('',#107272,#39640,#39641);
#33723=AXIS2_PLACEMENT_3D('',#107274,#39643,#39644);
#33724=AXIS2_PLACEMENT_3D('',#107275,#39645,#39646);
#33725=AXIS2_PLACEMENT_3D('',#107279,#39649,#39650);
#33726=AXIS2_PLACEMENT_3D('',#107281,#39652,#39653);
#33727=AXIS2_PLACEMENT_3D('',#107282,#39654,#39655);
#33728=AXIS2_PLACEMENT_3D('',#107286,#39658,#39659);
#33729=AXIS2_PLACEMENT_3D('',#107288,#39661,#39662);
#33730=AXIS2_PLACEMENT_3D('',#107289,#39663,#39664);
#33731=AXIS2_PLACEMENT_3D('',#107293,#39667,#39668);
#33732=AXIS2_PLACEMENT_3D('',#107295,#39670,#39671);
#33733=AXIS2_PLACEMENT_3D('',#107296,#39672,#39673);
#33734=AXIS2_PLACEMENT_3D('',#107300,#39676,#39677);
#33735=AXIS2_PLACEMENT_3D('',#107302,#39679,#39680);
#33736=AXIS2_PLACEMENT_3D('',#107303,#39681,#39682);
#33737=AXIS2_PLACEMENT_3D('',#107307,#39685,#39686);
#33738=AXIS2_PLACEMENT_3D('',#107309,#39688,#39689);
#33739=AXIS2_PLACEMENT_3D('',#107310,#39690,#39691);
#33740=AXIS2_PLACEMENT_3D('',#107314,#39694,#39695);
#33741=AXIS2_PLACEMENT_3D('',#107316,#39697,#39698);
#33742=AXIS2_PLACEMENT_3D('',#107317,#39699,#39700);
#33743=AXIS2_PLACEMENT_3D('',#107321,#39703,#39704);
#33744=AXIS2_PLACEMENT_3D('',#107323,#39706,#39707);
#33745=AXIS2_PLACEMENT_3D('',#107324,#39708,#39709);
#33746=AXIS2_PLACEMENT_3D('',#107328,#39712,#39713);
#33747=AXIS2_PLACEMENT_3D('',#107330,#39715,#39716);
#33748=AXIS2_PLACEMENT_3D('',#107331,#39717,#39718);
#33749=AXIS2_PLACEMENT_3D('',#107335,#39721,#39722);
#33750=AXIS2_PLACEMENT_3D('',#107337,#39724,#39725);
#33751=AXIS2_PLACEMENT_3D('',#107338,#39726,#39727);
#33752=AXIS2_PLACEMENT_3D('',#107342,#39730,#39731);
#33753=AXIS2_PLACEMENT_3D('',#107344,#39733,#39734);
#33754=AXIS2_PLACEMENT_3D('',#107345,#39735,#39736);
#33755=AXIS2_PLACEMENT_3D('',#107349,#39739,#39740);
#33756=AXIS2_PLACEMENT_3D('',#107351,#39742,#39743);
#33757=AXIS2_PLACEMENT_3D('',#107352,#39744,#39745);
#33758=AXIS2_PLACEMENT_3D('',#107356,#39748,#39749);
#33759=AXIS2_PLACEMENT_3D('',#107358,#39751,#39752);
#33760=AXIS2_PLACEMENT_3D('',#107359,#39753,#39754);
#33761=AXIS2_PLACEMENT_3D('',#107363,#39757,#39758);
#33762=AXIS2_PLACEMENT_3D('',#107365,#39760,#39761);
#33763=AXIS2_PLACEMENT_3D('',#107366,#39762,#39763);
#33764=AXIS2_PLACEMENT_3D('',#107370,#39766,#39767);
#33765=AXIS2_PLACEMENT_3D('',#107372,#39769,#39770);
#33766=AXIS2_PLACEMENT_3D('',#107373,#39771,#39772);
#33767=AXIS2_PLACEMENT_3D('',#107377,#39775,#39776);
#33768=AXIS2_PLACEMENT_3D('',#107379,#39778,#39779);
#33769=AXIS2_PLACEMENT_3D('',#107380,#39780,#39781);
#33770=AXIS2_PLACEMENT_3D('',#107384,#39784,#39785);
#33771=AXIS2_PLACEMENT_3D('',#107386,#39787,#39788);
#33772=AXIS2_PLACEMENT_3D('',#107387,#39789,#39790);
#33773=AXIS2_PLACEMENT_3D('',#107391,#39793,#39794);
#33774=AXIS2_PLACEMENT_3D('',#107393,#39796,#39797);
#33775=AXIS2_PLACEMENT_3D('',#107394,#39798,#39799);
#33776=AXIS2_PLACEMENT_3D('',#107398,#39802,#39803);
#33777=AXIS2_PLACEMENT_3D('',#107400,#39805,#39806);
#33778=AXIS2_PLACEMENT_3D('',#107401,#39807,#39808);
#33779=AXIS2_PLACEMENT_3D('',#107405,#39811,#39812);
#33780=AXIS2_PLACEMENT_3D('',#107407,#39814,#39815);
#33781=AXIS2_PLACEMENT_3D('',#107408,#39816,#39817);
#33782=AXIS2_PLACEMENT_3D('',#107412,#39820,#39821);
#33783=AXIS2_PLACEMENT_3D('',#107414,#39823,#39824);
#33784=AXIS2_PLACEMENT_3D('',#107415,#39825,#39826);
#33785=AXIS2_PLACEMENT_3D('',#107419,#39829,#39830);
#33786=AXIS2_PLACEMENT_3D('',#107421,#39832,#39833);
#33787=AXIS2_PLACEMENT_3D('',#107422,#39834,#39835);
#33788=AXIS2_PLACEMENT_3D('',#107426,#39838,#39839);
#33789=AXIS2_PLACEMENT_3D('',#107428,#39841,#39842);
#33790=AXIS2_PLACEMENT_3D('',#107429,#39843,#39844);
#33791=AXIS2_PLACEMENT_3D('',#107433,#39847,#39848);
#33792=AXIS2_PLACEMENT_3D('',#107435,#39850,#39851);
#33793=AXIS2_PLACEMENT_3D('',#107436,#39852,#39853);
#33794=AXIS2_PLACEMENT_3D('',#107440,#39856,#39857);
#33795=AXIS2_PLACEMENT_3D('',#107442,#39859,#39860);
#33796=AXIS2_PLACEMENT_3D('',#107443,#39861,#39862);
#33797=AXIS2_PLACEMENT_3D('',#107447,#39865,#39866);
#33798=AXIS2_PLACEMENT_3D('',#107449,#39868,#39869);
#33799=AXIS2_PLACEMENT_3D('',#107450,#39870,#39871);
#33800=AXIS2_PLACEMENT_3D('',#107454,#39874,#39875);
#33801=AXIS2_PLACEMENT_3D('',#107456,#39877,#39878);
#33802=AXIS2_PLACEMENT_3D('',#107457,#39879,#39880);
#33803=AXIS2_PLACEMENT_3D('',#107461,#39883,#39884);
#33804=AXIS2_PLACEMENT_3D('',#107463,#39886,#39887);
#33805=AXIS2_PLACEMENT_3D('',#107464,#39888,#39889);
#33806=AXIS2_PLACEMENT_3D('',#107468,#39892,#39893);
#33807=AXIS2_PLACEMENT_3D('',#107470,#39895,#39896);
#33808=AXIS2_PLACEMENT_3D('',#107471,#39897,#39898);
#33809=AXIS2_PLACEMENT_3D('',#107472,#39899,#39900);
#33810=AXIS2_PLACEMENT_3D('',#107473,#39901,#39902);
#33811=AXIS2_PLACEMENT_3D('',#107475,#39903,#39904);
#33812=AXIS2_PLACEMENT_3D('',#107476,#39905,#39906);
#33813=AXIS2_PLACEMENT_3D('',#107483,#39907,#39908);
#33814=AXIS2_PLACEMENT_3D('',#107493,#39909,#39910);
#33815=AXIS2_PLACEMENT_3D('',#107503,#39911,#39912);
#33816=AXIS2_PLACEMENT_3D('',#107513,#39913,#39914);
#33817=AXIS2_PLACEMENT_3D('',#107523,#39915,#39916);
#33818=AXIS2_PLACEMENT_3D('',#107533,#39917,#39918);
#33819=AXIS2_PLACEMENT_3D('',#107538,#39920,#39921);
#33820=AXIS2_PLACEMENT_3D('',#107543,#39924,#39925);
#33821=AXIS2_PLACEMENT_3D('',#107544,#39926,#39927);
#33822=AXIS2_PLACEMENT_3D('',#107548,#39929,#39930);
#33823=AXIS2_PLACEMENT_3D('',#107550,#39932,#39933);
#33824=AXIS2_PLACEMENT_3D('',#107555,#39936,#39937);
#33825=AXIS2_PLACEMENT_3D('',#107556,#39938,#39939);
#33826=AXIS2_PLACEMENT_3D('',#107560,#39941,#39942);
#33827=AXIS2_PLACEMENT_3D('',#107562,#39944,#39945);
#33828=AXIS2_PLACEMENT_3D('',#107567,#39948,#39949);
#33829=AXIS2_PLACEMENT_3D('',#107568,#39950,#39951);
#33830=AXIS2_PLACEMENT_3D('',#107572,#39953,#39954);
#33831=AXIS2_PLACEMENT_3D('',#107574,#39956,#39957);
#33832=AXIS2_PLACEMENT_3D('',#107581,#39962,#39963);
#33833=AXIS2_PLACEMENT_3D('',#107586,#39967,#39968);
#33834=AXIS2_PLACEMENT_3D('',#107591,#39972,#39973);
#33835=AXIS2_PLACEMENT_3D('',#107592,#39974,#39975);
#33836=AXIS2_PLACEMENT_3D('',#107593,#39976,#39977);
#33837=AXIS2_PLACEMENT_3D('',#107595,#39979,#39980);
#33838=AXIS2_PLACEMENT_3D('',#107596,#39981,#39982);
#33839=AXIS2_PLACEMENT_3D('',#107598,#39984,#39985);
#33840=AXIS2_PLACEMENT_3D('',#107600,#39987,#39988);
#33841=AXIS2_PLACEMENT_3D('',#107604,#39990,#39991);
#33842=AXIS2_PLACEMENT_3D('',#107605,#39992,#39993);
#33843=AXIS2_PLACEMENT_3D('',#107607,#39995,#39996);
#33844=AXIS2_PLACEMENT_3D('',#107608,#39997,#39998);
#33845=AXIS2_PLACEMENT_3D('',#107609,#39999,#40000);
#33846=AXIS2_PLACEMENT_3D('',#107610,#40001,#40002);
#33847=AXIS2_PLACEMENT_3D('',#107611,#40003,#40004);
#33848=AXIS2_PLACEMENT_3D('',#107612,#40005,#40006);
#33849=AXIS2_PLACEMENT_3D('',#107613,#40007,#40008);
#33850=AXIS2_PLACEMENT_3D('',#107614,#40009,#40010);
#33851=AXIS2_PLACEMENT_3D('',#107616,#40012,#40013);
#33852=AXIS2_PLACEMENT_3D('',#107617,#40014,#40015);
#33853=AXIS2_PLACEMENT_3D('',#107620,#40017,#40018);
#33854=AXIS2_PLACEMENT_3D('',#107623,#40021,#40022);
#33855=AXIS2_PLACEMENT_3D('',#107624,#40023,#40024);
#33856=AXIS2_PLACEMENT_3D('',#107625,#40025,#40026);
#33857=AXIS2_PLACEMENT_3D('',#107626,#40027,#40028);
#33858=AXIS2_PLACEMENT_3D('',#107758,#40030,#40031);
#33859=AXIS2_PLACEMENT_3D('',#107790,#40032,#40033);
#33860=AXIS2_PLACEMENT_3D('',#108210,#40035,#40036);
#33861=AXIS2_PLACEMENT_3D('',#108662,#40038,#40039);
#33862=AXIS2_PLACEMENT_3D('',#109116,#40041,#40042);
#33863=AXIS2_PLACEMENT_3D('',#109550,#40044,#40045);
#33864=AXIS2_PLACEMENT_3D('',#109986,#40047,#40048);
#33865=AXIS2_PLACEMENT_3D('',#110495,#40050,#40051);
#33866=AXIS2_PLACEMENT_3D('',#110943,#40053,#40054);
#33867=AXIS2_PLACEMENT_3D('',#111389,#40056,#40057);
#33868=AXIS2_PLACEMENT_3D('',#111846,#40059,#40060);
#33869=AXIS2_PLACEMENT_3D('',#112306,#40062,#40063);
#33870=AXIS2_PLACEMENT_3D('',#112758,#40065,#40066);
#33871=AXIS2_PLACEMENT_3D('',#113254,#40068,#40069);
#33872=AXIS2_PLACEMENT_3D('',#113688,#40071,#40072);
#33873=AXIS2_PLACEMENT_3D('',#114148,#40074,#40075);
#33874=AXIS2_PLACEMENT_3D('',#114545,#40077,#40078);
#33875=AXIS2_PLACEMENT_3D('',#114987,#40080,#40081);
#33876=AXIS2_PLACEMENT_3D('',#115429,#40083,#40084);
#33877=AXIS2_PLACEMENT_3D('',#115829,#40086,#40087);
#33878=AXIS2_PLACEMENT_3D('',#115963,#40089,#40090);
#33879=AXIS2_PLACEMENT_3D('',#116049,#40091,#40092);
#33880=AXIS2_PLACEMENT_3D('',#116526,#40094,#40095);
#33881=AXIS2_PLACEMENT_3D('',#116944,#40097,#40098);
#33882=AXIS2_PLACEMENT_3D('',#117358,#40100,#40101);
#33883=AXIS2_PLACEMENT_3D('',#117832,#40103,#40104);
#33884=AXIS2_PLACEMENT_3D('',#118267,#40106,#40107);
#33885=AXIS2_PLACEMENT_3D('',#118697,#40109,#40110);
#33886=AXIS2_PLACEMENT_3D('',#119137,#40112,#40113);
#33887=AXIS2_PLACEMENT_3D('',#119567,#40115,#40116);
#33888=AXIS2_PLACEMENT_3D('',#120077,#40118,#40119);
#33889=AXIS2_PLACEMENT_3D('',#120509,#40121,#40122);
#33890=AXIS2_PLACEMENT_3D('',#120927,#40124,#40125);
#33891=AXIS2_PLACEMENT_3D('',#121373,#40127,#40128);
#33892=AXIS2_PLACEMENT_3D('',#121839,#40130,#40131);
#33893=AXIS2_PLACEMENT_3D('',#122266,#40133,#40134);
#33894=AXIS2_PLACEMENT_3D('',#122690,#40136,#40137);
#33895=AXIS2_PLACEMENT_3D('',#123118,#40139,#40140);
#33896=AXIS2_PLACEMENT_3D('',#123559,#40142,#40143);
#33897=AXIS2_PLACEMENT_3D('',#123981,#40145,#40146);
#33898=AXIS2_PLACEMENT_3D('',#124174,#40147,#40148);
#33899=AXIS2_PLACEMENT_3D('',#124301,#40149,#40150);
#33900=AXIS2_PLACEMENT_3D('',#124500,#40151,#40152);
#33901=AXIS2_PLACEMENT_3D('',#124637,#40153,#40154);
#33902=AXIS2_PLACEMENT_3D('',#124640,#40155,#40156);
#33903=AXIS2_PLACEMENT_3D('',#124737,#40157,#40158);
#33904=AXIS2_PLACEMENT_3D('',#125338,#40159,#40160);
#33905=AXIS2_PLACEMENT_3D('',#125341,#40161,#40162);
#33906=AXIS2_PLACEMENT_3D('',#125424,#40163,#40164);
#33907=AXIS2_PLACEMENT_3D('',#125935,#40165,#40166);
#33908=AXIS2_PLACEMENT_3D('',#125937,#40167,#40168);
#33909=AXIS2_PLACEMENT_3D('',#125938,#40169,#40170);
#33910=AXIS2_PLACEMENT_3D('',#125939,#40171,#40172);
#33911=AXIS2_PLACEMENT_3D('',#125941,#40173,#40174);
#33912=AXIS2_PLACEMENT_3D('',#125942,#40175,#40176);
#33913=AXIS2_PLACEMENT_3D('',#125945,#40178,#40179);
#33914=AXIS2_PLACEMENT_3D('',#125946,#40180,#40181);
#33915=AXIS2_PLACEMENT_3D('',#125947,#40182,#40183);
#33916=AXIS2_PLACEMENT_3D('',#125950,#40184,#40185);
#33917=AXIS2_PLACEMENT_3D('',#125954,#40188,#40189);
#33918=AXIS2_PLACEMENT_3D('',#125962,#40192,#40193);
#33919=AXIS2_PLACEMENT_3D('',#125968,#40195,#40196);
#33920=AXIS2_PLACEMENT_3D('',#125971,#40197,#40198);
#33921=AXIS2_PLACEMENT_3D('',#125975,#40200,#40201);
#33922=AXIS2_PLACEMENT_3D('',#125976,#40202,#40203);
#33923=AXIS2_PLACEMENT_3D('',#125978,#40204,#40205);
#33924=AXIS2_PLACEMENT_3D('',#125982,#40207,#40208);
#33925=AXIS2_PLACEMENT_3D('',#125986,#40210,#40211);
#33926=AXIS2_PLACEMENT_3D('',#125990,#40213,#40214);
#33927=AXIS2_PLACEMENT_3D('',#125994,#40216,#40217);
#33928=AXIS2_PLACEMENT_3D('',#125998,#40219,#40220);
#33929=AXIS2_PLACEMENT_3D('',#126002,#40222,#40223);
#33930=AXIS2_PLACEMENT_3D('',#126006,#40225,#40226);
#33931=AXIS2_PLACEMENT_3D('',#126010,#40228,#40229);
#33932=AXIS2_PLACEMENT_3D('',#126014,#40231,#40232);
#33933=AXIS2_PLACEMENT_3D('',#126018,#40234,#40235);
#33934=AXIS2_PLACEMENT_3D('',#126022,#40237,#40238);
#33935=AXIS2_PLACEMENT_3D('',#126026,#40240,#40241);
#33936=AXIS2_PLACEMENT_3D('',#126030,#40243,#40244);
#33937=AXIS2_PLACEMENT_3D('',#126034,#40246,#40247);
#33938=AXIS2_PLACEMENT_3D('',#126038,#40249,#40250);
#33939=AXIS2_PLACEMENT_3D('',#126042,#40252,#40253);
#33940=AXIS2_PLACEMENT_3D('',#126046,#40255,#40256);
#33941=AXIS2_PLACEMENT_3D('',#126050,#40258,#40259);
#33942=AXIS2_PLACEMENT_3D('',#126054,#40261,#40262);
#33943=AXIS2_PLACEMENT_3D('',#126058,#40264,#40265);
#33944=AXIS2_PLACEMENT_3D('',#126062,#40267,#40268);
#33945=AXIS2_PLACEMENT_3D('',#126066,#40270,#40271);
#33946=AXIS2_PLACEMENT_3D('',#126070,#40273,#40274);
#33947=AXIS2_PLACEMENT_3D('',#126074,#40276,#40277);
#33948=AXIS2_PLACEMENT_3D('',#126078,#40279,#40280);
#33949=AXIS2_PLACEMENT_3D('',#126082,#40282,#40283);
#33950=AXIS2_PLACEMENT_3D('',#126086,#40285,#40286);
#33951=AXIS2_PLACEMENT_3D('',#126090,#40288,#40289);
#33952=AXIS2_PLACEMENT_3D('',#126094,#40291,#40292);
#33953=AXIS2_PLACEMENT_3D('',#126098,#40294,#40295);
#33954=AXIS2_PLACEMENT_3D('',#126102,#40297,#40298);
#33955=AXIS2_PLACEMENT_3D('',#126106,#40300,#40301);
#33956=AXIS2_PLACEMENT_3D('',#126109,#40303,#40304);
#33957=AXIS2_PLACEMENT_3D('',#126111,#40305,#40306);
#33958=AXIS2_PLACEMENT_3D('',#126115,#40308,#40309);
#33959=AXIS2_PLACEMENT_3D('',#126119,#40311,#40312);
#33960=AXIS2_PLACEMENT_3D('',#126123,#40314,#40315);
#33961=AXIS2_PLACEMENT_3D('',#126127,#40317,#40318);
#33962=AXIS2_PLACEMENT_3D('',#126131,#40320,#40321);
#33963=AXIS2_PLACEMENT_3D('',#126135,#40323,#40324);
#33964=AXIS2_PLACEMENT_3D('',#126139,#40326,#40327);
#33965=AXIS2_PLACEMENT_3D('',#126143,#40329,#40330);
#33966=AXIS2_PLACEMENT_3D('',#126147,#40332,#40333);
#33967=AXIS2_PLACEMENT_3D('',#126151,#40335,#40336);
#33968=AXIS2_PLACEMENT_3D('',#126155,#40338,#40339);
#33969=AXIS2_PLACEMENT_3D('',#126159,#40341,#40342);
#33970=AXIS2_PLACEMENT_3D('',#126163,#40344,#40345);
#33971=AXIS2_PLACEMENT_3D('',#126167,#40347,#40348);
#33972=AXIS2_PLACEMENT_3D('',#126171,#40350,#40351);
#33973=AXIS2_PLACEMENT_3D('',#126175,#40353,#40354);
#33974=AXIS2_PLACEMENT_3D('',#126179,#40356,#40357);
#33975=AXIS2_PLACEMENT_3D('',#126183,#40359,#40360);
#33976=AXIS2_PLACEMENT_3D('',#126187,#40362,#40363);
#33977=AXIS2_PLACEMENT_3D('',#126191,#40365,#40366);
#33978=AXIS2_PLACEMENT_3D('',#126195,#40368,#40369);
#33979=AXIS2_PLACEMENT_3D('',#126199,#40371,#40372);
#33980=AXIS2_PLACEMENT_3D('',#126203,#40374,#40375);
#33981=AXIS2_PLACEMENT_3D('',#126207,#40377,#40378);
#33982=AXIS2_PLACEMENT_3D('',#126211,#40380,#40381);
#33983=AXIS2_PLACEMENT_3D('',#126215,#40383,#40384);
#33984=AXIS2_PLACEMENT_3D('',#126219,#40386,#40387);
#33985=AXIS2_PLACEMENT_3D('',#126223,#40389,#40390);
#33986=AXIS2_PLACEMENT_3D('',#126227,#40392,#40393);
#33987=AXIS2_PLACEMENT_3D('',#126231,#40395,#40396);
#33988=AXIS2_PLACEMENT_3D('',#126235,#40398,#40399);
#33989=AXIS2_PLACEMENT_3D('',#126239,#40401,#40402);
#33990=AXIS2_PLACEMENT_3D('',#126243,#40404,#40405);
#33991=AXIS2_PLACEMENT_3D('',#126247,#40407,#40408);
#33992=AXIS2_PLACEMENT_3D('',#126251,#40410,#40411);
#33993=AXIS2_PLACEMENT_3D('',#126255,#40413,#40414);
#33994=AXIS2_PLACEMENT_3D('',#126257,#40416,#40417);
#33995=AXIS2_PLACEMENT_3D('',#126265,#40420,#40421);
#33996=AXIS2_PLACEMENT_3D('',#126270,#40423,#40424);
#33997=AXIS2_PLACEMENT_3D('',#126271,#40425,#40426);
#33998=AXIS2_PLACEMENT_3D('',#126512,#40428,#40429);
#33999=AXIS2_PLACEMENT_3D('',#126513,#40430,#40431);
#34000=AXIS2_PLACEMENT_3D('',#126517,#40434,#40435);
#34001=AXIS2_PLACEMENT_3D('',#126519,#40437,#40438);
#34002=AXIS2_PLACEMENT_3D('',#126520,#40439,#40440);
#34003=AXIS2_PLACEMENT_3D('',#126524,#40443,#40444);
#34004=AXIS2_PLACEMENT_3D('',#126526,#40446,#40447);
#34005=AXIS2_PLACEMENT_3D('',#126527,#40448,#40449);
#34006=AXIS2_PLACEMENT_3D('',#126531,#40452,#40453);
#34007=AXIS2_PLACEMENT_3D('',#126533,#40455,#40456);
#34008=AXIS2_PLACEMENT_3D('',#126534,#40457,#40458);
#34009=AXIS2_PLACEMENT_3D('',#126538,#40461,#40462);
#34010=AXIS2_PLACEMENT_3D('',#126540,#40464,#40465);
#34011=AXIS2_PLACEMENT_3D('',#126541,#40466,#40467);
#34012=AXIS2_PLACEMENT_3D('',#126545,#40470,#40471);
#34013=AXIS2_PLACEMENT_3D('',#126547,#40473,#40474);
#34014=AXIS2_PLACEMENT_3D('',#126548,#40475,#40476);
#34015=AXIS2_PLACEMENT_3D('',#126552,#40479,#40480);
#34016=AXIS2_PLACEMENT_3D('',#126554,#40482,#40483);
#34017=AXIS2_PLACEMENT_3D('',#126555,#40484,#40485);
#34018=AXIS2_PLACEMENT_3D('',#126559,#40488,#40489);
#34019=AXIS2_PLACEMENT_3D('',#126561,#40491,#40492);
#34020=AXIS2_PLACEMENT_3D('',#126562,#40493,#40494);
#34021=AXIS2_PLACEMENT_3D('',#126566,#40497,#40498);
#34022=AXIS2_PLACEMENT_3D('',#126568,#40500,#40501);
#34023=AXIS2_PLACEMENT_3D('',#126569,#40502,#40503);
#34024=AXIS2_PLACEMENT_3D('',#126573,#40506,#40507);
#34025=AXIS2_PLACEMENT_3D('',#126575,#40509,#40510);
#34026=AXIS2_PLACEMENT_3D('',#126576,#40511,#40512);
#34027=AXIS2_PLACEMENT_3D('',#126580,#40515,#40516);
#34028=AXIS2_PLACEMENT_3D('',#126582,#40518,#40519);
#34029=AXIS2_PLACEMENT_3D('',#126583,#40520,#40521);
#34030=AXIS2_PLACEMENT_3D('',#126587,#40524,#40525);
#34031=AXIS2_PLACEMENT_3D('',#126589,#40527,#40528);
#34032=AXIS2_PLACEMENT_3D('',#126590,#40529,#40530);
#34033=AXIS2_PLACEMENT_3D('',#126594,#40533,#40534);
#34034=AXIS2_PLACEMENT_3D('',#126596,#40536,#40537);
#34035=AXIS2_PLACEMENT_3D('',#126597,#40538,#40539);
#34036=AXIS2_PLACEMENT_3D('',#126601,#40542,#40543);
#34037=AXIS2_PLACEMENT_3D('',#126603,#40545,#40546);
#34038=AXIS2_PLACEMENT_3D('',#126604,#40547,#40548);
#34039=AXIS2_PLACEMENT_3D('',#126608,#40551,#40552);
#34040=AXIS2_PLACEMENT_3D('',#126610,#40554,#40555);
#34041=AXIS2_PLACEMENT_3D('',#126611,#40556,#40557);
#34042=AXIS2_PLACEMENT_3D('',#126615,#40560,#40561);
#34043=AXIS2_PLACEMENT_3D('',#126617,#40563,#40564);
#34044=AXIS2_PLACEMENT_3D('',#126618,#40565,#40566);
#34045=AXIS2_PLACEMENT_3D('',#126622,#40569,#40570);
#34046=AXIS2_PLACEMENT_3D('',#126624,#40572,#40573);
#34047=AXIS2_PLACEMENT_3D('',#126625,#40574,#40575);
#34048=AXIS2_PLACEMENT_3D('',#126629,#40578,#40579);
#34049=AXIS2_PLACEMENT_3D('',#126631,#40581,#40582);
#34050=AXIS2_PLACEMENT_3D('',#126632,#40583,#40584);
#34051=AXIS2_PLACEMENT_3D('',#126636,#40587,#40588);
#34052=AXIS2_PLACEMENT_3D('',#126638,#40590,#40591);
#34053=AXIS2_PLACEMENT_3D('',#126639,#40592,#40593);
#34054=AXIS2_PLACEMENT_3D('',#126643,#40596,#40597);
#34055=AXIS2_PLACEMENT_3D('',#126645,#40599,#40600);
#34056=AXIS2_PLACEMENT_3D('',#126646,#40601,#40602);
#34057=AXIS2_PLACEMENT_3D('',#126650,#40605,#40606);
#34058=AXIS2_PLACEMENT_3D('',#126652,#40608,#40609);
#34059=AXIS2_PLACEMENT_3D('',#126653,#40610,#40611);
#34060=AXIS2_PLACEMENT_3D('',#126657,#40614,#40615);
#34061=AXIS2_PLACEMENT_3D('',#126659,#40617,#40618);
#34062=AXIS2_PLACEMENT_3D('',#126660,#40619,#40620);
#34063=AXIS2_PLACEMENT_3D('',#126664,#40623,#40624);
#34064=AXIS2_PLACEMENT_3D('',#126666,#40626,#40627);
#34065=AXIS2_PLACEMENT_3D('',#126667,#40628,#40629);
#34066=AXIS2_PLACEMENT_3D('',#126671,#40632,#40633);
#34067=AXIS2_PLACEMENT_3D('',#126673,#40635,#40636);
#34068=AXIS2_PLACEMENT_3D('',#126674,#40637,#40638);
#34069=AXIS2_PLACEMENT_3D('',#126678,#40641,#40642);
#34070=AXIS2_PLACEMENT_3D('',#126680,#40644,#40645);
#34071=AXIS2_PLACEMENT_3D('',#126681,#40646,#40647);
#34072=AXIS2_PLACEMENT_3D('',#126685,#40650,#40651);
#34073=AXIS2_PLACEMENT_3D('',#126687,#40653,#40654);
#34074=AXIS2_PLACEMENT_3D('',#126688,#40655,#40656);
#34075=AXIS2_PLACEMENT_3D('',#126692,#40659,#40660);
#34076=AXIS2_PLACEMENT_3D('',#126694,#40662,#40663);
#34077=AXIS2_PLACEMENT_3D('',#126695,#40664,#40665);
#34078=AXIS2_PLACEMENT_3D('',#126699,#40668,#40669);
#34079=AXIS2_PLACEMENT_3D('',#126701,#40671,#40672);
#34080=AXIS2_PLACEMENT_3D('',#126702,#40673,#40674);
#34081=AXIS2_PLACEMENT_3D('',#126706,#40677,#40678);
#34082=AXIS2_PLACEMENT_3D('',#126708,#40680,#40681);
#34083=AXIS2_PLACEMENT_3D('',#126709,#40682,#40683);
#34084=AXIS2_PLACEMENT_3D('',#126713,#40686,#40687);
#34085=AXIS2_PLACEMENT_3D('',#126715,#40689,#40690);
#34086=AXIS2_PLACEMENT_3D('',#126716,#40691,#40692);
#34087=AXIS2_PLACEMENT_3D('',#126720,#40695,#40696);
#34088=AXIS2_PLACEMENT_3D('',#126722,#40698,#40699);
#34089=AXIS2_PLACEMENT_3D('',#126723,#40700,#40701);
#34090=AXIS2_PLACEMENT_3D('',#126727,#40704,#40705);
#34091=AXIS2_PLACEMENT_3D('',#126729,#40707,#40708);
#34092=AXIS2_PLACEMENT_3D('',#126730,#40709,#40710);
#34093=AXIS2_PLACEMENT_3D('',#126734,#40713,#40714);
#34094=AXIS2_PLACEMENT_3D('',#126736,#40716,#40717);
#34095=AXIS2_PLACEMENT_3D('',#126737,#40718,#40719);
#34096=AXIS2_PLACEMENT_3D('',#126741,#40722,#40723);
#34097=AXIS2_PLACEMENT_3D('',#126743,#40725,#40726);
#34098=AXIS2_PLACEMENT_3D('',#126744,#40727,#40728);
#34099=AXIS2_PLACEMENT_3D('',#126748,#40731,#40732);
#34100=AXIS2_PLACEMENT_3D('',#126750,#40734,#40735);
#34101=AXIS2_PLACEMENT_3D('',#126751,#40736,#40737);
#34102=AXIS2_PLACEMENT_3D('',#126752,#40738,#40739);
#34103=AXIS2_PLACEMENT_3D('',#126753,#40740,#40741);
#34104=AXIS2_PLACEMENT_3D('',#126755,#40742,#40743);
#34105=AXIS2_PLACEMENT_3D('',#126756,#40744,#40745);
#34106=AXIS2_PLACEMENT_3D('',#126763,#40746,#40747);
#34107=AXIS2_PLACEMENT_3D('',#126773,#40748,#40749);
#34108=AXIS2_PLACEMENT_3D('',#126783,#40750,#40751);
#34109=AXIS2_PLACEMENT_3D('',#126793,#40752,#40753);
#34110=AXIS2_PLACEMENT_3D('',#126803,#40754,#40755);
#34111=AXIS2_PLACEMENT_3D('',#126813,#40756,#40757);
#34112=AXIS2_PLACEMENT_3D('',#126818,#40759,#40760);
#34113=AXIS2_PLACEMENT_3D('',#126823,#40763,#40764);
#34114=AXIS2_PLACEMENT_3D('',#126824,#40765,#40766);
#34115=AXIS2_PLACEMENT_3D('',#126828,#40768,#40769);
#34116=AXIS2_PLACEMENT_3D('',#126830,#40771,#40772);
#34117=AXIS2_PLACEMENT_3D('',#126835,#40775,#40776);
#34118=AXIS2_PLACEMENT_3D('',#126836,#40777,#40778);
#34119=AXIS2_PLACEMENT_3D('',#126840,#40780,#40781);
#34120=AXIS2_PLACEMENT_3D('',#126842,#40783,#40784);
#34121=AXIS2_PLACEMENT_3D('',#126847,#40787,#40788);
#34122=AXIS2_PLACEMENT_3D('',#126848,#40789,#40790);
#34123=AXIS2_PLACEMENT_3D('',#126852,#40792,#40793);
#34124=AXIS2_PLACEMENT_3D('',#126854,#40795,#40796);
#34125=AXIS2_PLACEMENT_3D('',#126861,#40801,#40802);
#34126=AXIS2_PLACEMENT_3D('',#126866,#40806,#40807);
#34127=AXIS2_PLACEMENT_3D('',#126871,#40811,#40812);
#34128=AXIS2_PLACEMENT_3D('',#126872,#40813,#40814);
#34129=AXIS2_PLACEMENT_3D('',#126873,#40815,#40816);
#34130=AXIS2_PLACEMENT_3D('',#126875,#40818,#40819);
#34131=AXIS2_PLACEMENT_3D('',#126876,#40820,#40821);
#34132=AXIS2_PLACEMENT_3D('',#126878,#40823,#40824);
#34133=AXIS2_PLACEMENT_3D('',#126880,#40826,#40827);
#34134=AXIS2_PLACEMENT_3D('',#126884,#40829,#40830);
#34135=AXIS2_PLACEMENT_3D('',#126885,#40831,#40832);
#34136=AXIS2_PLACEMENT_3D('',#126887,#40834,#40835);
#34137=AXIS2_PLACEMENT_3D('',#126888,#40836,#40837);
#34138=AXIS2_PLACEMENT_3D('',#126889,#40838,#40839);
#34139=AXIS2_PLACEMENT_3D('',#126890,#40840,#40841);
#34140=AXIS2_PLACEMENT_3D('',#126891,#40842,#40843);
#34141=AXIS2_PLACEMENT_3D('',#126892,#40844,#40845);
#34142=AXIS2_PLACEMENT_3D('',#126893,#40846,#40847);
#34143=AXIS2_PLACEMENT_3D('',#126894,#40848,#40849);
#34144=AXIS2_PLACEMENT_3D('',#126896,#40851,#40852);
#34145=AXIS2_PLACEMENT_3D('',#126897,#40853,#40854);
#34146=AXIS2_PLACEMENT_3D('',#126900,#40856,#40857);
#34147=AXIS2_PLACEMENT_3D('',#126903,#40860,#40861);
#34148=AXIS2_PLACEMENT_3D('',#126904,#40862,#40863);
#34149=AXIS2_PLACEMENT_3D('',#126905,#40864,#40865);
#34150=AXIS2_PLACEMENT_3D('',#126906,#40866,#40867);
#34151=AXIS2_PLACEMENT_3D('',#126964,#40869,#40870);
#34152=AXIS2_PLACEMENT_3D('',#126993,#40871,#40872);
#34153=AXIS2_PLACEMENT_3D('',#127366,#40874,#40875);
#34154=AXIS2_PLACEMENT_3D('',#127728,#40877,#40878);
#34155=AXIS2_PLACEMENT_3D('',#128100,#40880,#40881);
#34156=AXIS2_PLACEMENT_3D('',#128436,#40883,#40884);
#34157=AXIS2_PLACEMENT_3D('',#128792,#40886,#40887);
#34158=AXIS2_PLACEMENT_3D('',#129160,#40889,#40890);
#34159=AXIS2_PLACEMENT_3D('',#129516,#40892,#40893);
#34160=AXIS2_PLACEMENT_3D('',#129868,#40895,#40896);
#34161=AXIS2_PLACEMENT_3D('',#130208,#40898,#40899);
#34162=AXIS2_PLACEMENT_3D('',#130584,#40901,#40902);
#34163=AXIS2_PLACEMENT_3D('',#130630,#40904,#40905);
#34164=AXIS2_PLACEMENT_3D('',#130639,#40906,#40907);
#34165=AXIS2_PLACEMENT_3D('',#131004,#40909,#40910);
#34166=AXIS2_PLACEMENT_3D('',#131373,#40912,#40913);
#34167=AXIS2_PLACEMENT_3D('',#131742,#40915,#40916);
#34168=AXIS2_PLACEMENT_3D('',#132097,#40918,#40919);
#34169=AXIS2_PLACEMENT_3D('',#132461,#40921,#40922);
#34170=AXIS2_PLACEMENT_3D('',#132840,#40924,#40925);
#34171=AXIS2_PLACEMENT_3D('',#133213,#40927,#40928);
#34172=AXIS2_PLACEMENT_3D('',#133576,#40930,#40931);
#34173=AXIS2_PLACEMENT_3D('',#133944,#40933,#40934);
#34174=AXIS2_PLACEMENT_3D('',#134130,#40935,#40936);
#34175=AXIS2_PLACEMENT_3D('',#134288,#40937,#40938);
#34176=AXIS2_PLACEMENT_3D('',#134349,#40939,#40940);
#34177=AXIS2_PLACEMENT_3D('',#134794,#40941,#40942);
#34178=AXIS2_PLACEMENT_3D('',#134796,#40943,#40944);
#34179=AXIS2_PLACEMENT_3D('',#134878,#40945,#40946);
#34180=AXIS2_PLACEMENT_3D('',#135171,#40947,#40948);
#34181=AXIS2_PLACEMENT_3D('',#135173,#40949,#40950);
#34182=AXIS2_PLACEMENT_3D('',#135174,#40951,#40952);
#34183=AXIS2_PLACEMENT_3D('',#135175,#40953,#40954);
#34184=AXIS2_PLACEMENT_3D('',#135177,#40955,#40956);
#34185=AXIS2_PLACEMENT_3D('',#135178,#40957,#40958);
#34186=AXIS2_PLACEMENT_3D('',#135181,#40959,#40960);
#34187=AXIS2_PLACEMENT_3D('',#135185,#40962,#40963);
#34188=AXIS2_PLACEMENT_3D('',#135188,#40965,#40966);
#34189=AXIS2_PLACEMENT_3D('',#135189,#40967,#40968);
#34190=AXIS2_PLACEMENT_3D('',#135203,#40972,#40973);
#34191=AXIS2_PLACEMENT_3D('',#135217,#40977,#40978);
#34192=AXIS2_PLACEMENT_3D('',#135219,#40980,#40981);
#34193=AXIS2_PLACEMENT_3D('',#135220,#40982,#40983);
#34194=AXIS2_PLACEMENT_3D('',#135221,#40984,#40985);
#34195=AXIS2_PLACEMENT_3D('',#135222,#40986,#40987);
#34196=AXIS2_PLACEMENT_3D('',#135223,#40988,#40989);
#34197=AXIS2_PLACEMENT_3D('',#135224,#40990,#40991);
#34198=AXIS2_PLACEMENT_3D('',#135225,#40992,#40993);
#34199=AXIS2_PLACEMENT_3D('',#135226,#40994,#40995);
#34200=AXIS2_PLACEMENT_3D('',#135228,#40996,#40997);
#34201=AXIS2_PLACEMENT_3D('',#135229,#40998,#40999);
#34202=AXIS2_PLACEMENT_3D('',#135231,#41001,#41002);
#34203=AXIS2_PLACEMENT_3D('',#135232,#41003,#41004);
#34204=AXIS2_PLACEMENT_3D('',#135233,#41005,#41006);
#34205=AXIS2_PLACEMENT_3D('',#135234,#41007,#41008);
#34206=AXIS2_PLACEMENT_3D('',#135235,#41009,#41010);
#34207=AXIS2_PLACEMENT_3D('',#135236,#41011,#41012);
#34208=AXIS2_PLACEMENT_3D('',#135237,#41013,#41014);
#34209=AXIS2_PLACEMENT_3D('',#135238,#41015,#41016);
#34210=AXIS2_PLACEMENT_3D('',#135239,#41017,#41018);
#34211=AXIS2_PLACEMENT_3D('',#135240,#41019,#41020);
#34212=AXIS2_PLACEMENT_3D('',#135241,#41021,#41022);
#34213=AXIS2_PLACEMENT_3D('',#135242,#41023,#41024);
#34214=AXIS2_PLACEMENT_3D('',#135243,#41025,#41026);
#34215=AXIS2_PLACEMENT_3D('',#135244,#41027,#41028);
#34216=AXIS2_PLACEMENT_3D('',#135245,#41029,#41030);
#34217=AXIS2_PLACEMENT_3D('',#135246,#41031,#41032);
#34218=AXIS2_PLACEMENT_3D('',#135247,#41033,#41034);
#34219=AXIS2_PLACEMENT_3D('',#135248,#41035,#41036);
#34220=AXIS2_PLACEMENT_3D('',#135249,#41037,#41038);
#34221=AXIS2_PLACEMENT_3D('',#135250,#41039,#41040);
#34222=AXIS2_PLACEMENT_3D('',#135251,#41041,#41042);
#34223=AXIS2_PLACEMENT_3D('',#135252,#41043,#41044);
#34224=DIRECTION('axis',(0.,0.,1.));
#34225=DIRECTION('refdir',(1.,0.,0.));
#34226=DIRECTION('axis',(0.,0.,1.));
#34227=DIRECTION('refdir',(1.,0.,0.));
#34228=DIRECTION('center_axis',(0.,1.,0.));
#34229=DIRECTION('ref_axis',(1.,0.,0.));
#34230=DIRECTION('center_axis',(0.,-1.,0.));
#34231=DIRECTION('ref_axis',(1.,0.,0.));
#34232=DIRECTION('',(-0.707106781186555,0.70710678118654,8.65956056235503E-17));
#34233=DIRECTION('center_axis',(0.,1.,0.));
#34234=DIRECTION('ref_axis',(1.,0.,0.));
#34235=DIRECTION('center_axis',(0.,1.,0.));
#34236=DIRECTION('ref_axis',(0.,0.,1.));
#34237=DIRECTION('',(-0.499999999999999,0.,0.866025403784439));
#34238=DIRECTION('',(-0.5,0.,-0.866025403784439));
#34239=DIRECTION('',(0.,0.,-1.));
#34240=DIRECTION('',(1.,0.,0.));
#34241=DIRECTION('',(0.,0.,1.));
#34242=DIRECTION('',(-0.5,0.,0.866025403784439));
#34243=DIRECTION('',(-0.500000000000003,0.,-0.866025403784437));
#34244=DIRECTION('',(1.,0.,0.));
#34245=DIRECTION('',(-0.707106781186548,0.,0.707106781186548));
#34246=DIRECTION('',(0.,0.,-1.));
#34247=DIRECTION('',(0.707106781186548,0.,0.707106781186548));
#34248=DIRECTION('',(-1.,0.,0.));
#34249=DIRECTION('',(0.707106781186548,0.,-0.707106781186547));
#34250=DIRECTION('',(0.,0.,1.));
#34251=DIRECTION('',(-0.707106781186548,0.,-0.707106781186548));
#34252=DIRECTION('',(1.,0.,0.));
#34253=DIRECTION('center_axis',(0.,1.,0.));
#34254=DIRECTION('ref_axis',(1.,0.,0.));
#34255=DIRECTION('center_axis',(0.,-1.,0.));
#34256=DIRECTION('ref_axis',(1.,0.,0.));
#34257=DIRECTION('',(0.,-1.,0.));
#34258=DIRECTION('center_axis',(0.,-1.,0.));
#34259=DIRECTION('ref_axis',(1.,0.,0.));
#34260=DIRECTION('center_axis',(0.,1.,0.));
#34261=DIRECTION('ref_axis',(1.,0.,0.));
#34262=DIRECTION('center_axis',(0.,-1.,0.));
#34263=DIRECTION('ref_axis',(1.,0.,0.));
#34264=DIRECTION('',(-0.707106781186555,0.70710678118654,8.65956056235503E-17));
#34265=DIRECTION('center_axis',(0.,-1.,0.));
#34266=DIRECTION('ref_axis',(1.,0.,0.));
#34267=DIRECTION('',(0.,-1.,0.));
#34268=DIRECTION('center_axis',(0.,-1.,0.));
#34269=DIRECTION('ref_axis',(1.,0.,0.));
#34270=DIRECTION('center_axis',(0.,1.,0.));
#34271=DIRECTION('ref_axis',(1.,0.,0.));
#34272=DIRECTION('',(-0.857167300702115,0.515038074910049,1.04972719113862E-16));
#34273=DIRECTION('center_axis',(0.,1.,0.));
#34274=DIRECTION('ref_axis',(1.,0.,0.));
#34275=DIRECTION('',(-0.857167300702115,0.515038074910049,1.04972719113862E-16));
#34276=DIRECTION('center_axis',(0.,-1.,0.));
#34277=DIRECTION('ref_axis',(1.,0.,0.));
#34278=DIRECTION('center_axis',(0.,1.,0.));
#34279=DIRECTION('ref_axis',(1.,0.,0.));
#34280=DIRECTION('',(-0.707106781186547,-0.707106781186548,-8.65956056235493E-17));
#34281=DIRECTION('center_axis',(0.,-1.,0.));
#34282=DIRECTION('ref_axis',(1.,0.,0.));
#34283=DIRECTION('center_axis',(0.,1.,0.));
#34284=DIRECTION('ref_axis',(1.,0.,0.));
#34285=DIRECTION('',(0.499999999999999,0.,-0.866025403784439));
#34286=DIRECTION('',(-1.,0.,0.));
#34287=DIRECTION('',(0.707106781186548,0.,0.707106781186548));
#34288=DIRECTION('',(0.,0.,-1.));
#34289=DIRECTION('',(-0.707106781186548,0.,0.707106781186547));
#34290=DIRECTION('',(1.,0.,0.));
#34291=DIRECTION('',(-0.707106781186548,0.,-0.707106781186548));
#34292=DIRECTION('',(0.,0.,1.));
#34293=DIRECTION('',(0.707106781186548,0.,-0.707106781186548));
#34294=DIRECTION('',(-1.,0.,0.));
#34295=DIRECTION('',(0.500000000000003,0.,0.866025403784437));
#34296=DIRECTION('',(0.5,0.,-0.866025403784439));
#34297=DIRECTION('',(0.,0.,-1.));
#34298=DIRECTION('',(-1.,0.,0.));
#34299=DIRECTION('',(0.,0.,1.));
#34300=DIRECTION('',(0.5,0.,0.866025403784439));
#34301=DIRECTION('center_axis',(0.,-1.,0.));
#34302=DIRECTION('ref_axis',(1.,0.,0.));
#34303=DIRECTION('center_axis',(0.,1.,0.));
#34304=DIRECTION('ref_axis',(1.,0.,0.));
#34305=DIRECTION('',(0.,1.,0.));
#34306=DIRECTION('center_axis',(0.,1.,0.));
#34307=DIRECTION('ref_axis',(1.,0.,0.));
#34308=DIRECTION('center_axis',(0.,-1.,0.));
#34309=DIRECTION('ref_axis',(1.,0.,0.));
#34310=DIRECTION('center_axis',(0.,1.,0.));
#34311=DIRECTION('ref_axis',(1.,0.,0.));
#34312=DIRECTION('',(-0.707106781186547,-0.707106781186548,-8.65956056235493E-17));
#34313=DIRECTION('center_axis',(0.,1.,0.));
#34314=DIRECTION('ref_axis',(1.,0.,0.));
#34315=DIRECTION('',(0.,1.,0.));
#34316=DIRECTION('center_axis',(0.,1.,0.));
#34317=DIRECTION('ref_axis',(1.,0.,0.));
#34318=DIRECTION('center_axis',(0.,-1.,0.));
#34319=DIRECTION('ref_axis',(1.,0.,0.));
#34320=DIRECTION('',(-0.85716730070211,-0.515038074910058,-1.04972719113862E-16));
#34321=DIRECTION('center_axis',(0.,-1.,0.));
#34322=DIRECTION('ref_axis',(1.,0.,0.));
#34323=DIRECTION('',(-0.85716730070211,-0.515038074910058,-1.04972719113862E-16));
#34324=DIRECTION('center_axis',(0.866025403784439,0.,0.499999999999999));
#34325=DIRECTION('ref_axis',(0.499999999999999,0.,-0.866025403784439));
#34326=DIRECTION('',(0.,-1.,0.));
#34327=DIRECTION('',(0.,1.,0.));
#34328=DIRECTION('center_axis',(0.,0.,1.));
#34329=DIRECTION('ref_axis',(1.,0.,0.));
#34330=DIRECTION('',(0.,1.,0.));
#34331=DIRECTION('center_axis',(-0.866025403784437,0.,0.500000000000003));
#34332=DIRECTION('ref_axis',(0.500000000000003,0.,0.866025403784437));
#34333=DIRECTION('',(0.,-1.,0.));
#34334=DIRECTION('',(0.,1.,0.));
#34335=DIRECTION('center_axis',(0.,0.,1.));
#34336=DIRECTION('ref_axis',(1.,0.,0.));
#34337=DIRECTION('',(0.,-1.,0.));
#34338=DIRECTION('center_axis',(0.707106781186548,0.,0.707106781186548));
#34339=DIRECTION('ref_axis',(0.707106781186548,0.,-0.707106781186548));
#34340=DIRECTION('',(0.,1.,0.));
#34341=DIRECTION('center_axis',(0.707106781186548,0.,-0.707106781186548));
#34342=DIRECTION('ref_axis',(-0.707106781186548,0.,-0.707106781186548));
#34343=DIRECTION('',(0.,-1.,0.));
#34344=DIRECTION('',(0.,1.,0.));
#34345=DIRECTION('center_axis',(0.,0.,-1.));
#34346=DIRECTION('ref_axis',(-1.,0.,0.));
#34347=DIRECTION('',(0.,-1.,0.));
#34348=DIRECTION('center_axis',(-0.707106781186547,0.,-0.707106781186548));
#34349=DIRECTION('ref_axis',(-0.707106781186548,0.,0.707106781186547));
#34350=DIRECTION('',(0.,1.,0.));
#34351=DIRECTION('center_axis',(-0.707106781186548,0.,0.707106781186548));
#34352=DIRECTION('ref_axis',(0.707106781186548,0.,0.707106781186548));
#34353=DIRECTION('',(0.,-1.,0.));
#34354=DIRECTION('center_axis',(-1.,0.,0.));
#34355=DIRECTION('ref_axis',(0.,0.,1.));
#34356=DIRECTION('center_axis',(1.,0.,0.));
#34357=DIRECTION('ref_axis',(0.,0.,-1.));
#34358=DIRECTION('center_axis',(-0.866025403784439,0.,-0.5));
#34359=DIRECTION('ref_axis',(-0.5,0.,0.866025403784439));
#34360=DIRECTION('',(0.,1.,0.));
#34361=DIRECTION('center_axis',(-1.,0.,0.));
#34362=DIRECTION('ref_axis',(0.,0.,1.));
#34363=DIRECTION('',(0.,1.,0.));
#34364=DIRECTION('center_axis',(0.,0.,1.));
#34365=DIRECTION('ref_axis',(1.,0.,0.));
#34366=DIRECTION('',(0.,1.,0.));
#34367=DIRECTION('center_axis',(1.,0.,0.));
#34368=DIRECTION('ref_axis',(0.,0.,-1.));
#34369=DIRECTION('',(0.,1.,0.));
#34370=DIRECTION('center_axis',(0.866025403784439,0.,-0.5));
#34371=DIRECTION('ref_axis',(-0.5,0.,-0.866025403784439));
#34372=DIRECTION('axis',(0.,0.,1.));
#34373=DIRECTION('refdir',(1.,0.,0.));
#34374=DIRECTION('center_axis',(1.,0.,0.));
#34375=DIRECTION('ref_axis',(0.,0.,-1.));
#34376=DIRECTION('center_axis',(-1.,0.,0.));
#34377=DIRECTION('ref_axis',(0.,0.,-1.));
#34378=DIRECTION('',(0.707106781186542,-8.659560562355E-17,0.707106781186553));
#34379=DIRECTION('center_axis',(1.,0.,0.));
#34380=DIRECTION('ref_axis',(0.,0.,-1.));
#34381=DIRECTION('center_axis',(1.,0.,0.));
#34382=DIRECTION('ref_axis',(0.,0.,-1.));
#34383=DIRECTION('',(0.,1.,0.));
#34384=DIRECTION('',(0.,0.,1.));
#34385=DIRECTION('',(0.,1.,0.));
#34386=DIRECTION('',(0.,0.,-1.));
#34387=DIRECTION('center_axis',(1.,0.,0.));
#34388=DIRECTION('ref_axis',(0.,0.,-1.));
#34389=DIRECTION('center_axis',(-1.,0.,0.));
#34390=DIRECTION('ref_axis',(0.,0.,-1.));
#34391=DIRECTION('',(-1.,0.,0.));
#34392=DIRECTION('center_axis',(-1.,0.,0.));
#34393=DIRECTION('ref_axis',(0.,0.,-1.));
#34394=DIRECTION('center_axis',(-1.,0.,0.));
#34395=DIRECTION('ref_axis',(0.,0.,-1.));
#34396=DIRECTION('center_axis',(1.,0.,0.));
#34397=DIRECTION('ref_axis',(0.,0.,-1.));
#34398=DIRECTION('center_axis',(-1.,0.,0.));
#34399=DIRECTION('ref_axis',(0.,0.,-1.));
#34400=DIRECTION('',(0.707106781186542,-8.659560562355E-17,0.707106781186553));
#34401=DIRECTION('center_axis',(-1.,0.,0.));
#34402=DIRECTION('ref_axis',(0.,0.,-1.));
#34403=DIRECTION('',(-1.,0.,0.));
#34404=DIRECTION('center_axis',(-1.,0.,0.));
#34405=DIRECTION('ref_axis',(0.,0.,-1.));
#34406=DIRECTION('center_axis',(-1.,0.,0.));
#34407=DIRECTION('ref_axis',(0.,0.,-1.));
#34408=DIRECTION('center_axis',(1.,0.,0.));
#34409=DIRECTION('ref_axis',(0.,1.,0.));
#34410=DIRECTION('',(0.515038074910058,-0.85716730070211,-1.04972719113862E-16));
#34411=DIRECTION('center_axis',(1.,0.,0.));
#34412=DIRECTION('ref_axis',(0.,1.,0.));
#34413=DIRECTION('',(0.515038074910058,-0.85716730070211,-1.04972719113862E-16));
#34414=DIRECTION('center_axis',(0.,0.,1.));
#34415=DIRECTION('ref_axis',(1.,0.,0.));
#34416=DIRECTION('center_axis',(0.,0.,-1.));
#34417=DIRECTION('ref_axis',(1.,0.,0.));
#34418=DIRECTION('',(-0.707106781186545,-8.6595605623549E-17,0.70710678118655));
#34419=DIRECTION('center_axis',(0.,0.,1.));
#34420=DIRECTION('ref_axis',(1.,0.,0.));
#34421=DIRECTION('center_axis',(0.,0.,1.));
#34422=DIRECTION('ref_axis',(1.,0.,0.));
#34423=DIRECTION('',(-1.,0.,0.));
#34424=DIRECTION('',(0.,-1.,0.));
#34425=DIRECTION('',(1.,0.,0.));
#34426=DIRECTION('',(0.,1.,0.));
#34427=DIRECTION('center_axis',(0.,0.,1.));
#34428=DIRECTION('ref_axis',(1.,0.,0.));
#34429=DIRECTION('center_axis',(0.,0.,1.));
#34430=DIRECTION('ref_axis',(1.,0.,0.));
#34431=DIRECTION('center_axis',(0.,0.,1.));
#34432=DIRECTION('ref_axis',(1.,0.,0.));
#34433=DIRECTION('center_axis',(0.,0.,1.));
#34434=DIRECTION('ref_axis',(1.,0.,0.));
#34435=DIRECTION('center_axis',(0.,0.,1.));
#34436=DIRECTION('ref_axis',(1.,0.,0.));
#34437=DIRECTION('center_axis',(0.,0.,1.));
#34438=DIRECTION('ref_axis',(1.,0.,0.));
#34439=DIRECTION('center_axis',(0.,0.,1.));
#34440=DIRECTION('ref_axis',(1.,0.,0.));
#34441=DIRECTION('center_axis',(0.,0.,1.));
#34442=DIRECTION('ref_axis',(1.,0.,0.));
#34443=DIRECTION('center_axis',(0.,0.,1.));
#34444=DIRECTION('ref_axis',(1.,0.,0.));
#34445=DIRECTION('center_axis',(0.,0.,-1.));
#34446=DIRECTION('ref_axis',(1.,0.,0.));
#34447=DIRECTION('',(0.,0.,-1.));
#34448=DIRECTION('center_axis',(0.,0.,-1.));
#34449=DIRECTION('ref_axis',(1.,0.,0.));
#34450=DIRECTION('center_axis',(0.,0.,1.));
#34451=DIRECTION('ref_axis',(1.,0.,0.));
#34452=DIRECTION('center_axis',(0.,0.,-1.));
#34453=DIRECTION('ref_axis',(1.,0.,0.));
#34454=DIRECTION('',(-0.707106781186545,-8.6595605623549E-17,0.70710678118655));
#34455=DIRECTION('center_axis',(0.,0.,-1.));
#34456=DIRECTION('ref_axis',(1.,0.,0.));
#34457=DIRECTION('',(0.,0.,-1.));
#34458=DIRECTION('center_axis',(0.,0.,-1.));
#34459=DIRECTION('ref_axis',(1.,0.,0.));
#34460=DIRECTION('center_axis',(0.,0.,1.));
#34461=DIRECTION('ref_axis',(1.,0.,0.));
#34462=DIRECTION('center_axis',(0.,0.,-1.));
#34463=DIRECTION('ref_axis',(1.,0.,0.));
#34464=DIRECTION('',(-0.707106781186545,-8.6595605623549E-17,0.70710678118655));
#34465=DIRECTION('center_axis',(0.,0.,-1.));
#34466=DIRECTION('ref_axis',(1.,0.,0.));
#34467=DIRECTION('',(0.,0.,-1.));
#34468=DIRECTION('center_axis',(0.,0.,-1.));
#34469=DIRECTION('ref_axis',(1.,0.,0.));
#34470=DIRECTION('center_axis',(0.,0.,1.));
#34471=DIRECTION('ref_axis',(1.,0.,0.));
#34472=DIRECTION('center_axis',(0.,0.,-1.));
#34473=DIRECTION('ref_axis',(1.,0.,0.));
#34474=DIRECTION('',(-0.707106781186545,-8.6595605623549E-17,0.70710678118655));
#34475=DIRECTION('center_axis',(0.,0.,-1.));
#34476=DIRECTION('ref_axis',(1.,0.,0.));
#34477=DIRECTION('',(0.,0.,-1.));
#34478=DIRECTION('center_axis',(0.,0.,-1.));
#34479=DIRECTION('ref_axis',(1.,0.,0.));
#34480=DIRECTION('center_axis',(0.,0.,1.));
#34481=DIRECTION('ref_axis',(1.,0.,0.));
#34482=DIRECTION('',(-0.85716730070211,-1.04972719113862E-16,0.515038074910058));
#34483=DIRECTION('center_axis',(0.,0.,1.));
#34484=DIRECTION('ref_axis',(1.,0.,0.));
#34485=DIRECTION('',(-0.85716730070211,-1.04972719113862E-16,0.515038074910058));
#34486=DIRECTION('center_axis',(0.,0.,1.));
#34487=DIRECTION('ref_axis',(1.,0.,0.));
#34488=DIRECTION('',(-0.85716730070211,-1.04972719113862E-16,0.515038074910058));
#34489=DIRECTION('center_axis',(0.,0.,1.));
#34490=DIRECTION('ref_axis',(1.,0.,0.));
#34491=DIRECTION('',(-0.85716730070211,-1.04972719113862E-16,0.515038074910058));
#34492=DIRECTION('center_axis',(0.,0.,1.));
#34493=DIRECTION('ref_axis',(1.,0.,0.));
#34494=DIRECTION('center_axis',(0.,0.,-1.));
#34495=DIRECTION('ref_axis',(1.,0.,0.));
#34496=DIRECTION('',(-0.707106781186549,-8.65956056235496E-17,0.707106781186546));
#34497=DIRECTION('center_axis',(0.,0.,-1.));
#34498=DIRECTION('ref_axis',(1.,0.,0.));
#34499=DIRECTION('',(0.,0.,-1.));
#34500=DIRECTION('center_axis',(0.,0.,-1.));
#34501=DIRECTION('ref_axis',(1.,0.,0.));
#34502=DIRECTION('center_axis',(0.,0.,1.));
#34503=DIRECTION('ref_axis',(1.,0.,0.));
#34504=DIRECTION('center_axis',(0.,0.,-1.));
#34505=DIRECTION('ref_axis',(1.,0.,0.));
#34506=DIRECTION('',(-0.70710678118655,-8.65956056235496E-17,0.707106781186545));
#34507=DIRECTION('center_axis',(0.,0.,-1.));
#34508=DIRECTION('ref_axis',(1.,0.,0.));
#34509=DIRECTION('',(0.,0.,-1.));
#34510=DIRECTION('center_axis',(0.,0.,-1.));
#34511=DIRECTION('ref_axis',(1.,0.,0.));
#34512=DIRECTION('center_axis',(0.,0.,1.));
#34513=DIRECTION('ref_axis',(1.,0.,0.));
#34514=DIRECTION('center_axis',(0.,0.,-1.));
#34515=DIRECTION('ref_axis',(1.,0.,0.));
#34516=DIRECTION('',(-0.70710678118655,-8.65956056235496E-17,0.707106781186545));
#34517=DIRECTION('center_axis',(0.,0.,-1.));
#34518=DIRECTION('ref_axis',(1.,0.,0.));
#34519=DIRECTION('',(0.,0.,-1.));
#34520=DIRECTION('center_axis',(0.,0.,-1.));
#34521=DIRECTION('ref_axis',(1.,0.,0.));
#34522=DIRECTION('center_axis',(0.,0.,1.));
#34523=DIRECTION('ref_axis',(1.,0.,0.));
#34524=DIRECTION('center_axis',(0.,0.,-1.));
#34525=DIRECTION('ref_axis',(1.,0.,0.));
#34526=DIRECTION('',(-0.70710678118655,-8.65956056235496E-17,0.707106781186545));
#34527=DIRECTION('center_axis',(0.,0.,-1.));
#34528=DIRECTION('ref_axis',(1.,0.,0.));
#34529=DIRECTION('',(0.,0.,-1.));
#34530=DIRECTION('center_axis',(0.,0.,-1.));
#34531=DIRECTION('ref_axis',(1.,0.,0.));
#34532=DIRECTION('center_axis',(0.,0.,1.));
#34533=DIRECTION('ref_axis',(1.,0.,0.));
#34534=DIRECTION('center_axis',(0.,0.,-1.));
#34535=DIRECTION('ref_axis',(1.,0.,0.));
#34536=DIRECTION('',(-0.70710678118655,-8.65956056235496E-17,0.707106781186545));
#34537=DIRECTION('center_axis',(0.,0.,-1.));
#34538=DIRECTION('ref_axis',(1.,0.,0.));
#34539=DIRECTION('',(0.,0.,-1.));
#34540=DIRECTION('center_axis',(0.,0.,-1.));
#34541=DIRECTION('ref_axis',(1.,0.,0.));
#34542=DIRECTION('center_axis',(0.,0.,1.));
#34543=DIRECTION('ref_axis',(1.,0.,0.));
#34544=DIRECTION('center_axis',(0.,0.,-1.));
#34545=DIRECTION('ref_axis',(1.,0.,0.));
#34546=DIRECTION('',(-0.707106781186549,-8.65956056235496E-17,0.707106781186546));
#34547=DIRECTION('center_axis',(0.,0.,-1.));
#34548=DIRECTION('ref_axis',(1.,0.,0.));
#34549=DIRECTION('',(0.,0.,-1.));
#34550=DIRECTION('center_axis',(0.,0.,-1.));
#34551=DIRECTION('ref_axis',(1.,0.,0.));
#34552=DIRECTION('center_axis',(0.,0.,1.));
#34553=DIRECTION('ref_axis',(1.,0.,0.));
#34554=DIRECTION('',(-0.857167300702115,-1.04972719113862E-16,0.515038074910049));
#34555=DIRECTION('center_axis',(0.,0.,1.));
#34556=DIRECTION('ref_axis',(1.,0.,0.));
#34557=DIRECTION('',(-0.857167300702115,-1.04972719113862E-16,0.515038074910049));
#34558=DIRECTION('center_axis',(0.,0.,1.));
#34559=DIRECTION('ref_axis',(1.,0.,0.));
#34560=DIRECTION('',(-0.857167300702115,-1.04972719113862E-16,0.515038074910049));
#34561=DIRECTION('center_axis',(0.,0.,1.));
#34562=DIRECTION('ref_axis',(1.,0.,0.));
#34563=DIRECTION('',(-0.857167300702115,-1.04972719113862E-16,0.515038074910049));
#34564=DIRECTION('center_axis',(0.,0.,1.));
#34565=DIRECTION('ref_axis',(1.,0.,0.));
#34566=DIRECTION('',(-0.857167300702115,-1.04972719113862E-16,0.515038074910049));
#34567=DIRECTION('center_axis',(0.,0.,1.));
#34568=DIRECTION('ref_axis',(1.,0.,0.));
#34569=DIRECTION('',(-0.857167300702115,-1.04972719113862E-16,0.515038074910049));
#34570=DIRECTION('center_axis',(0.,-1.,0.));
#34571=DIRECTION('ref_axis',(1.,0.,0.));
#34572=DIRECTION('',(0.,1.,0.));
#34573=DIRECTION('center_axis',(0.,1.,0.));
#34574=DIRECTION('ref_axis',(1.,0.,0.));
#34575=DIRECTION('',(0.,-1.,0.));
#34576=DIRECTION('center_axis',(0.,-1.,0.));
#34577=DIRECTION('ref_axis',(1.,0.,0.));
#34578=DIRECTION('center_axis',(0.,1.,0.));
#34579=DIRECTION('ref_axis',(0.,0.,1.));
#34580=DIRECTION('',(-1.,0.,0.));
#34581=DIRECTION('',(0.,0.,1.));
#34582=DIRECTION('',(-1.,0.,0.));
#34583=DIRECTION('',(-1.,0.,0.));
#34584=DIRECTION('center_axis',(0.,0.,-1.));
#34585=DIRECTION('ref_axis',(-1.,0.,0.));
#34586=DIRECTION('',(-1.,0.,0.));
#34587=DIRECTION('',(-1.,0.,0.));
#34588=DIRECTION('',(0.,-1.,0.));
#34589=DIRECTION('',(1.,0.,0.));
#34590=DIRECTION('',(1.,0.,0.));
#34591=DIRECTION('',(0.,-1.,0.));
#34592=DIRECTION('',(1.,0.,0.));
#34593=DIRECTION('',(0.,1.,0.));
#34594=DIRECTION('center_axis',(0.,1.,0.));
#34595=DIRECTION('ref_axis',(1.,0.,0.));
#34596=DIRECTION('',(0.,1.,0.));
#34597=DIRECTION('center_axis',(0.,1.,0.));
#34598=DIRECTION('ref_axis',(1.,0.,0.));
#34599=DIRECTION('center_axis',(0.,-1.,0.));
#34600=DIRECTION('ref_axis',(1.,0.,0.));
#34601=DIRECTION('center_axis',(0.,1.,0.));
#34602=DIRECTION('ref_axis',(1.,0.,0.));
#34603=DIRECTION('center_axis',(0.,1.,0.));
#34604=DIRECTION('ref_axis',(1.,0.,0.));
#34605=DIRECTION('',(1.,0.,0.));
#34606=DIRECTION('center_axis',(0.,1.,0.));
#34607=DIRECTION('ref_axis',(1.,0.,0.));
#34608=DIRECTION('',(-1.,0.,0.));
#34609=DIRECTION('center_axis',(0.,1.,0.));
#34610=DIRECTION('ref_axis',(1.,0.,0.));
#34611=DIRECTION('center_axis',(0.,1.,0.));
#34612=DIRECTION('ref_axis',(1.,0.,0.));
#34613=DIRECTION('center_axis',(0.,1.,0.));
#34614=DIRECTION('ref_axis',(1.,0.,0.));
#34615=DIRECTION('center_axis',(0.,1.,0.));
#34616=DIRECTION('ref_axis',(1.,0.,0.));
#34617=DIRECTION('',(0.,1.,0.));
#34618=DIRECTION('center_axis',(0.,-1.,0.));
#34619=DIRECTION('ref_axis',(1.,0.,0.));
#34620=DIRECTION('center_axis',(0.,-1.,0.));
#34621=DIRECTION('ref_axis',(1.,0.,0.));
#34622=DIRECTION('center_axis',(0.,-0.707106781186541,0.707106781186554));
#34623=DIRECTION('ref_axis',(1.,0.,0.));
#34624=DIRECTION('',(-0.577350269189622,-0.577350269189633,-0.577350269189622));
#34625=DIRECTION('',(1.,0.,0.));
#34626=DIRECTION('',(-0.577350269189622,0.577350269189633,0.577350269189622));
#34627=DIRECTION('center_axis',(-0.707106781186548,0.,0.707106781186548));
#34628=DIRECTION('ref_axis',(0.707106781186548,0.,0.707106781186548));
#34629=DIRECTION('',(0.,-1.,0.));
#34630=DIRECTION('',(-0.577350269189622,0.577350269189633,-0.577350269189622));
#34631=DIRECTION('center_axis',(0.,0.707106781186541,0.707106781186554));
#34632=DIRECTION('ref_axis',(1.,0.,0.));
#34633=DIRECTION('',(-0.577350269189622,-0.577350269189633,0.577350269189622));
#34634=DIRECTION('center_axis',(0.707106781186548,0.,0.707106781186548));
#34635=DIRECTION('ref_axis',(0.707106781186548,0.,-0.707106781186548));
#34636=DIRECTION('center_axis',(0.,1.,0.));
#34637=DIRECTION('ref_axis',(1.,0.,0.));
#34638=DIRECTION('',(1.,0.,0.));
#34639=DIRECTION('',(0.,0.,-1.));
#34640=DIRECTION('center_axis',(0.,1.,0.));
#34641=DIRECTION('ref_axis',(0.,0.,1.));
#34642=DIRECTION('',(-1.,0.,0.));
#34643=DIRECTION('',(0.5,0.,-0.866025403784439));
#34644=DIRECTION('',(0.,0.,-1.));
#34645=DIRECTION('',(-1.,0.,0.));
#34646=DIRECTION('',(0.,0.,1.));
#34647=DIRECTION('',(0.5,0.,0.866025403784439));
#34648=DIRECTION('center_axis',(-0.866025403784439,0.,0.5));
#34649=DIRECTION('ref_axis',(0.5,0.,0.866025403784439));
#34650=DIRECTION('',(-0.5,0.,-0.866025403784439));
#34651=DIRECTION('',(0.,1.,0.));
#34652=DIRECTION('center_axis',(-1.,0.,0.));
#34653=DIRECTION('ref_axis',(0.,0.,1.));
#34654=DIRECTION('',(0.,0.,-1.));
#34655=DIRECTION('',(0.,1.,0.));
#34656=DIRECTION('center_axis',(0.,0.,-1.));
#34657=DIRECTION('ref_axis',(-1.,0.,0.));
#34658=DIRECTION('',(1.,0.,0.));
#34659=DIRECTION('',(0.,1.,0.));
#34660=DIRECTION('center_axis',(1.,0.,0.));
#34661=DIRECTION('ref_axis',(0.,0.,-1.));
#34662=DIRECTION('',(0.,0.,1.));
#34663=DIRECTION('',(0.,1.,0.));
#34664=DIRECTION('center_axis',(0.866025403784439,0.,0.5));
#34665=DIRECTION('ref_axis',(0.5,0.,-0.866025403784439));
#34666=DIRECTION('',(-0.5,0.,0.866025403784439));
#34667=DIRECTION('',(0.,1.,0.));
#34668=DIRECTION('center_axis',(0.,1.,0.));
#34669=DIRECTION('ref_axis',(1.,0.,0.));
#34670=DIRECTION('',(1.,0.,0.));
#34671=DIRECTION('center_axis',(-1.,0.,0.));
#34672=DIRECTION('ref_axis',(0.,0.,1.));
#34673=DIRECTION('center_axis',(0.,0.,-1.));
#34674=DIRECTION('ref_axis',(-1.,0.,0.));
#34675=DIRECTION('axis',(0.,0.,1.));
#34676=DIRECTION('refdir',(1.,0.,0.));
#34677=DIRECTION('center_axis',(0.,1.,0.));
#34678=DIRECTION('ref_axis',(-1.,0.,0.));
#34679=DIRECTION('center_axis',(0.,-1.,0.));
#34680=DIRECTION('ref_axis',(-1.,0.,0.));
#34681=DIRECTION('',(0.707106781186544,0.707106781186551,-8.6595605623549E-17));
#34682=DIRECTION('center_axis',(0.,1.,0.));
#34683=DIRECTION('ref_axis',(-1.,0.,0.));
#34684=DIRECTION('center_axis',(0.,-1.,0.));
#34685=DIRECTION('ref_axis',(-1.,0.,0.));
#34686=DIRECTION('center_axis',(0.,-1.,0.));
#34687=DIRECTION('ref_axis',(1.,0.,0.));
#34688=DIRECTION('',(0.,-1.,0.));
#34689=DIRECTION('center_axis',(0.,1.,0.));
#34690=DIRECTION('ref_axis',(-1.,0.,0.));
#34691=DIRECTION('center_axis',(0.,1.,0.));
#34692=DIRECTION('ref_axis',(-1.,0.,0.));
#34693=DIRECTION('center_axis',(0.,1.,0.));
#34694=DIRECTION('ref_axis',(0.,0.,1.));
#34695=DIRECTION('center_axis',(0.,-1.,0.));
#34696=DIRECTION('ref_axis',(1.,0.,0.));
#34697=DIRECTION('center_axis',(0.,-1.,0.));
#34698=DIRECTION('ref_axis',(-1.,0.,0.));
#34699=DIRECTION('',(0.707106781186544,-0.707106781186551,8.6595605623549E-17));
#34700=DIRECTION('center_axis',(0.,-1.,0.));
#34701=DIRECTION('ref_axis',(-1.,0.,0.));
#34702=DIRECTION('center_axis',(0.,-1.,0.));
#34703=DIRECTION('ref_axis',(0.,0.,-1.));
#34704=DIRECTION('center_axis',(0.,-1.,0.));
#34705=DIRECTION('ref_axis',(1.,0.,0.));
#34706=DIRECTION('center_axis',(0.,-1.,0.));
#34707=DIRECTION('ref_axis',(1.,0.,0.));
#34708=DIRECTION('center_axis',(0.,-1.,0.));
#34709=DIRECTION('ref_axis',(1.,0.,0.));
#34710=DIRECTION('',(0.707106781186555,0.70710678118654,8.65956056235503E-17));
#34711=DIRECTION('center_axis',(0.,-1.,0.));
#34712=DIRECTION('ref_axis',(1.,0.,0.));
#34713=DIRECTION('center_axis',(0.,-1.,0.));
#34714=DIRECTION('ref_axis',(1.,0.,0.));
#34715=DIRECTION('',(0.,1.,0.));
#34716=DIRECTION('center_axis',(0.,1.,0.));
#34717=DIRECTION('ref_axis',(1.,0.,0.));
#34718=DIRECTION('',(0.707106781186555,-0.70710678118654,-8.65956056235503E-17));
#34719=DIRECTION('axis',(0.,0.,1.));
#34720=DIRECTION('refdir',(1.,0.,0.));
#34721=DIRECTION('center_axis',(0.,-1.,0.));
#34722=DIRECTION('ref_axis',(1.,0.,0.));
#34723=DIRECTION('',(0.,1.,0.));
#34724=DIRECTION('center_axis',(0.,-1.,0.));
#34725=DIRECTION('ref_axis',(1.,0.,0.));
#34726=DIRECTION('',(0.,1.,0.));
#34727=DIRECTION('',(-0.0016684081382487,0.99998546068423,-0.00512784890894562));
#34728=DIRECTION('center_axis',(0.,-1.,0.));
#34729=DIRECTION('ref_axis',(1.,0.,0.));
#34730=DIRECTION('',(0.,1.,0.));
#34731=DIRECTION('center_axis',(0.,-1.,0.));
#34732=DIRECTION('ref_axis',(1.,0.,0.));
#34733=DIRECTION('',(0.,1.,0.));
#34734=DIRECTION('center_axis',(0.,-1.,0.));
#34735=DIRECTION('ref_axis',(1.,0.,0.));
#34736=DIRECTION('',(0.,1.,0.));
#34737=DIRECTION('center_axis',(0.,-1.,0.));
#34738=DIRECTION('ref_axis',(1.,0.,0.));
#34739=DIRECTION('',(0.,1.,0.));
#34740=DIRECTION('center_axis',(0.,-1.,0.));
#34741=DIRECTION('ref_axis',(1.,0.,0.));
#34742=DIRECTION('',(0.,1.,0.));
#34743=DIRECTION('center_axis',(0.,-1.,0.));
#34744=DIRECTION('ref_axis',(1.,0.,0.));
#34745=DIRECTION('',(0.,1.,0.));
#34746=DIRECTION('center_axis',(0.,-1.,0.));
#34747=DIRECTION('ref_axis',(1.,0.,0.));
#34748=DIRECTION('',(0.,1.,0.));
#34749=DIRECTION('center_axis',(0.,-1.,0.));
#34750=DIRECTION('ref_axis',(1.,0.,0.));
#34751=DIRECTION('',(0.,1.,0.));
#34752=DIRECTION('center_axis',(0.,-1.,0.));
#34753=DIRECTION('ref_axis',(1.,0.,0.));
#34754=DIRECTION('',(0.,1.,0.));
#34755=DIRECTION('center_axis',(0.,-1.,0.));
#34756=DIRECTION('ref_axis',(1.,0.,0.));
#34757=DIRECTION('',(0.,1.,0.));
#34758=DIRECTION('center_axis',(0.,-1.,0.));
#34759=DIRECTION('ref_axis',(1.,0.,0.));
#34760=DIRECTION('',(0.,1.,0.));
#34761=DIRECTION('center_axis',(0.,-1.,0.));
#34762=DIRECTION('ref_axis',(1.,0.,0.));
#34763=DIRECTION('',(0.,1.,0.));
#34764=DIRECTION('center_axis',(0.,-1.,0.));
#34765=DIRECTION('ref_axis',(1.,0.,0.));
#34766=DIRECTION('',(0.,1.,0.));
#34767=DIRECTION('center_axis',(0.,-1.,0.));
#34768=DIRECTION('ref_axis',(1.,0.,0.));
#34769=DIRECTION('',(0.,1.,0.));
#34770=DIRECTION('center_axis',(0.,-1.,0.));
#34771=DIRECTION('ref_axis',(1.,0.,0.));
#34772=DIRECTION('',(0.,1.,0.));
#34773=DIRECTION('center_axis',(0.,-1.,0.));
#34774=DIRECTION('ref_axis',(1.,0.,0.));
#34775=DIRECTION('',(0.,1.,0.));
#34776=DIRECTION('center_axis',(0.,-1.,0.));
#34777=DIRECTION('ref_axis',(1.,0.,0.));
#34778=DIRECTION('',(0.,1.,0.));
#34779=DIRECTION('center_axis',(0.,-1.,0.));
#34780=DIRECTION('ref_axis',(1.,0.,0.));
#34781=DIRECTION('',(0.,1.,0.));
#34782=DIRECTION('center_axis',(0.,-1.,0.));
#34783=DIRECTION('ref_axis',(1.,0.,0.));
#34784=DIRECTION('',(0.,1.,0.));
#34785=DIRECTION('center_axis',(0.,-1.,0.));
#34786=DIRECTION('ref_axis',(1.,0.,0.));
#34787=DIRECTION('',(0.,1.,0.));
#34788=DIRECTION('center_axis',(0.,-1.,0.));
#34789=DIRECTION('ref_axis',(1.,0.,0.));
#34790=DIRECTION('',(0.,1.,0.));
#34791=DIRECTION('center_axis',(0.,-1.,0.));
#34792=DIRECTION('ref_axis',(1.,0.,0.));
#34793=DIRECTION('',(0.,1.,0.));
#34794=DIRECTION('center_axis',(0.,-1.,0.));
#34795=DIRECTION('ref_axis',(1.,0.,0.));
#34796=DIRECTION('',(0.,1.,0.));
#34797=DIRECTION('center_axis',(0.,-1.,0.));
#34798=DIRECTION('ref_axis',(1.,0.,0.));
#34799=DIRECTION('',(0.,1.,0.));
#34800=DIRECTION('center_axis',(0.,-1.,0.));
#34801=DIRECTION('ref_axis',(1.,0.,0.));
#34802=DIRECTION('',(0.,1.,0.));
#34803=DIRECTION('center_axis',(0.,-1.,0.));
#34804=DIRECTION('ref_axis',(1.,0.,0.));
#34805=DIRECTION('',(0.,1.,0.));
#34806=DIRECTION('center_axis',(0.,-1.,0.));
#34807=DIRECTION('ref_axis',(1.,0.,0.));
#34808=DIRECTION('',(0.,1.,0.));
#34809=DIRECTION('center_axis',(0.,-1.,0.));
#34810=DIRECTION('ref_axis',(1.,0.,0.));
#34811=DIRECTION('',(0.,1.,0.));
#34812=DIRECTION('center_axis',(0.,-1.,0.));
#34813=DIRECTION('ref_axis',(1.,0.,0.));
#34814=DIRECTION('',(0.,1.,0.));
#34815=DIRECTION('center_axis',(0.,-1.,0.));
#34816=DIRECTION('ref_axis',(1.,0.,0.));
#34817=DIRECTION('',(0.,1.,0.));
#34818=DIRECTION('center_axis',(0.,-1.,0.));
#34819=DIRECTION('ref_axis',(1.,0.,0.));
#34820=DIRECTION('',(0.,1.,0.));
#34821=DIRECTION('center_axis',(0.,-1.,0.));
#34822=DIRECTION('ref_axis',(1.,0.,0.));
#34823=DIRECTION('',(0.,1.,0.));
#34824=DIRECTION('center_axis',(0.,-1.,0.));
#34825=DIRECTION('ref_axis',(1.,0.,0.));
#34826=DIRECTION('',(0.,1.,0.));
#34827=DIRECTION('center_axis',(0.,-1.,0.));
#34828=DIRECTION('ref_axis',(1.,0.,0.));
#34829=DIRECTION('',(0.,1.,0.));
#34830=DIRECTION('center_axis',(0.,-1.,0.));
#34831=DIRECTION('ref_axis',(1.,0.,0.));
#34832=DIRECTION('',(0.,1.,0.));
#34833=DIRECTION('center_axis',(0.,-1.,0.));
#34834=DIRECTION('ref_axis',(1.,0.,0.));
#34835=DIRECTION('',(0.,1.,0.));
#34836=DIRECTION('center_axis',(0.,-1.,0.));
#34837=DIRECTION('ref_axis',(1.,0.,0.));
#34838=DIRECTION('',(0.,1.,0.));
#34839=DIRECTION('center_axis',(0.,-1.,0.));
#34840=DIRECTION('ref_axis',(1.,0.,0.));
#34841=DIRECTION('',(0.,1.,0.));
#34842=DIRECTION('center_axis',(0.,-1.,0.));
#34843=DIRECTION('ref_axis',(1.,0.,0.));
#34844=DIRECTION('',(0.,1.,0.));
#34845=DIRECTION('center_axis',(0.,-1.,0.));
#34846=DIRECTION('ref_axis',(1.,0.,0.));
#34847=DIRECTION('',(0.,1.,0.));
#34848=DIRECTION('center_axis',(0.,-1.,0.));
#34849=DIRECTION('ref_axis',(1.,0.,0.));
#34850=DIRECTION('',(0.,1.,0.));
#34851=DIRECTION('center_axis',(0.,-1.,0.));
#34852=DIRECTION('ref_axis',(1.,0.,0.));
#34853=DIRECTION('',(0.,1.,0.));
#34854=DIRECTION('center_axis',(0.,-1.,0.));
#34855=DIRECTION('ref_axis',(1.,0.,0.));
#34856=DIRECTION('',(0.,1.,0.));
#34857=DIRECTION('center_axis',(0.,-1.,0.));
#34858=DIRECTION('ref_axis',(1.,0.,0.));
#34859=DIRECTION('',(0.,1.,0.));
#34860=DIRECTION('center_axis',(0.,-1.,0.));
#34861=DIRECTION('ref_axis',(1.,0.,0.));
#34862=DIRECTION('',(0.,1.,0.));
#34863=DIRECTION('center_axis',(0.,-1.,0.));
#34864=DIRECTION('ref_axis',(1.,0.,0.));
#34865=DIRECTION('center_axis',(0.,-1.,0.));
#34866=DIRECTION('ref_axis',(1.,0.,0.));
#34867=DIRECTION('',(0.,1.,0.));
#34868=DIRECTION('',(0.,1.,0.));
#34869=DIRECTION('',(0.,-1.,0.));
#34870=DIRECTION('center_axis',(0.,-1.,0.));
#34871=DIRECTION('ref_axis',(1.,0.,0.));
#34872=DIRECTION('center_axis',(0.,1.,0.));
#34873=DIRECTION('ref_axis',(0.,0.,1.));
#34874=DIRECTION('center_axis',(0.,1.,0.));
#34875=DIRECTION('ref_axis',(1.,0.,0.));
#34876=DIRECTION('',(0.,0.,1.));
#34877=DIRECTION('center_axis',(0.,-1.,0.));
#34878=DIRECTION('ref_axis',(0.,0.,-1.));
#34879=DIRECTION('center_axis',(0.,-1.,0.));
#34880=DIRECTION('ref_axis',(1.,0.,0.));
#34881=DIRECTION('',(0.,0.,-1.));
#34882=DIRECTION('center_axis',(1.,0.,0.));
#34883=DIRECTION('ref_axis',(0.,0.,-1.));
#34884=DIRECTION('',(0.,1.,0.));
#34885=DIRECTION('',(0.,-1.,0.));
#34886=DIRECTION('center_axis',(0.282244511485419,0.0053902631593721,0.959327358517117));
#34887=DIRECTION('ref_axis',(0.891452264496529,-0.370963252076271,-0.260190556579225));
#34888=DIRECTION('',(0.743330576824897,-0.633384321745291,-0.215137059858184));
#34889=DIRECTION('',(-0.354472701149703,-0.928631902678381,0.109507504160964));
#34890=DIRECTION('',(-0.956816275612035,0.0741039314181457,0.281089348912921));
#34891=DIRECTION('',(0.,-1.,0.));
#34892=DIRECTION('',(0.953582665134141,-0.3011313679371,0.));
#34893=DIRECTION('',(-0.953582665134141,-0.3011313679371,0.));
#34894=DIRECTION('center_axis',(0.,0.,1.));
#34895=DIRECTION('ref_axis',(1.,0.,0.));
#34896=DIRECTION('center_axis',(0.,1.,0.));
#34897=DIRECTION('ref_axis',(0.,0.,1.));
#34898=DIRECTION('center_axis',(0.,-1.,0.));
#34899=DIRECTION('ref_axis',(1.,0.,0.));
#34900=DIRECTION('center_axis',(0.,-1.,0.));
#34901=DIRECTION('ref_axis',(1.,0.,0.));
#34902=DIRECTION('center_axis',(0.,-1.,0.));
#34903=DIRECTION('ref_axis',(1.,0.,0.));
#34904=DIRECTION('',(0.707106781186534,0.707106781186561,8.65956056235478E-17));
#34905=DIRECTION('center_axis',(0.,-1.,0.));
#34906=DIRECTION('ref_axis',(1.,0.,0.));
#34907=DIRECTION('center_axis',(0.,-1.,0.));
#34908=DIRECTION('ref_axis',(1.,0.,0.));
#34909=DIRECTION('',(0.,1.,0.));
#34910=DIRECTION('center_axis',(0.,1.,0.));
#34911=DIRECTION('ref_axis',(0.,0.,1.));
#34912=DIRECTION('center_axis',(0.,1.,0.));
#34913=DIRECTION('ref_axis',(1.,0.,0.));
#34914=DIRECTION('',(0.707106781186549,-0.707106781186546,-8.65956056235496E-17));
#34915=DIRECTION('center_axis',(0.,-1.,0.));
#34916=DIRECTION('ref_axis',(1.,0.,0.));
#34917=DIRECTION('center_axis',(0.,-1.,0.));
#34918=DIRECTION('ref_axis',(0.,0.,-1.));
#34919=DIRECTION('center_axis',(0.,-1.,0.));
#34920=DIRECTION('ref_axis',(1.,0.,0.));
#34921=DIRECTION('center_axis',(0.,-1.,0.));
#34922=DIRECTION('ref_axis',(1.,0.,0.));
#34923=DIRECTION('center_axis',(0.,-1.,0.));
#34924=DIRECTION('ref_axis',(1.,0.,0.));
#34925=DIRECTION('',(0.,1.,0.));
#34926=DIRECTION('center_axis',(0.,1.,0.));
#34927=DIRECTION('ref_axis',(1.,0.,0.));
#34928=DIRECTION('',(0.707106781186547,-0.707106781186548,-8.65956056235493E-17));
#34929=DIRECTION('center_axis',(0.,-1.,0.));
#34930=DIRECTION('ref_axis',(1.,0.,0.));
#34931=DIRECTION('center_axis',(0.,-1.,0.));
#34932=DIRECTION('ref_axis',(0.,0.,-1.));
#34933=DIRECTION('axis',(0.,0.,1.));
#34934=DIRECTION('refdir',(1.,0.,0.));
#34935=DIRECTION('center_axis',(-1.,0.,0.));
#34936=DIRECTION('ref_axis',(0.,0.,-1.));
#34937=DIRECTION('center_axis',(-0.559437318248335,0.,0.828872660274852));
#34938=DIRECTION('ref_axis',(-0.828872660274852,0.,-0.559437318248335));
#34939=DIRECTION('center_axis',(-0.275920768781063,0.,-0.961180383359579));
#34940=DIRECTION('ref_axis',(0.961180383359579,0.,-0.275920768781063));
#34941=DIRECTION('center_axis',(-0.422885465331123,0.,0.906183139995266));
#34942=DIRECTION('ref_axis',(-0.906183139995266,0.,-0.422885465331123));
#34943=DIRECTION('center_axis',(-0.422885465331123,0.,-0.906183139995266));
#34944=DIRECTION('ref_axis',(0.906183139995266,0.,-0.422885465331123));
#34945=DIRECTION('center_axis',(-0.275920768781063,0.,0.961180383359579));
#34946=DIRECTION('ref_axis',(-0.961180383359579,0.,-0.275920768781063));
#34947=DIRECTION('center_axis',(-0.559437318248336,0.,-0.828872660274852));
#34948=DIRECTION('ref_axis',(0.828872660274852,0.,-0.559437318248336));
#34949=DIRECTION('center_axis',(-0.559437318248336,0.,-0.828872660274852));
#34950=DIRECTION('ref_axis',(0.828872660274852,0.,-0.559437318248336));
#34951=DIRECTION('center_axis',(-0.275920768781063,0.,0.961180383359579));
#34952=DIRECTION('ref_axis',(-0.961180383359579,0.,-0.275920768781063));
#34953=DIRECTION('center_axis',(-0.422885465331123,0.,-0.906183139995266));
#34954=DIRECTION('ref_axis',(0.906183139995266,0.,-0.422885465331123));
#34955=DIRECTION('center_axis',(-0.422885465331123,0.,0.906183139995266));
#34956=DIRECTION('ref_axis',(-0.906183139995266,0.,-0.422885465331123));
#34957=DIRECTION('center_axis',(-0.275920768781063,0.,-0.961180383359579));
#34958=DIRECTION('ref_axis',(0.961180383359579,0.,-0.275920768781063));
#34959=DIRECTION('center_axis',(-0.559437318248335,0.,0.828872660274852));
#34960=DIRECTION('ref_axis',(-0.828872660274852,0.,-0.559437318248335));
#34961=DIRECTION('',(-1.,0.,0.));
#34962=DIRECTION('center_axis',(-0.559437318248335,0.,0.828872660274852));
#34963=DIRECTION('ref_axis',(0.828872660274852,0.,0.559437318248335));
#34964=DIRECTION('',(0.,1.,0.));
#34965=DIRECTION('',(-0.828872660274852,0.,-0.559437318248335));
#34966=DIRECTION('',(0.,1.,0.));
#34967=DIRECTION('center_axis',(-0.275920768781063,0.,-0.961180383359579));
#34968=DIRECTION('ref_axis',(-0.961180383359579,0.,0.275920768781063));
#34969=DIRECTION('',(0.961180383359579,0.,-0.275920768781063));
#34970=DIRECTION('',(0.,-1.,0.));
#34971=DIRECTION('center_axis',(-0.559437318248336,0.,-0.828872660274852));
#34972=DIRECTION('ref_axis',(-0.828872660274852,0.,0.559437318248336));
#34973=DIRECTION('',(0.,1.,0.));
#34974=DIRECTION('',(0.828872660274852,0.,-0.559437318248336));
#34975=DIRECTION('',(0.,-1.,0.));
#34976=DIRECTION('center_axis',(-0.559437318248336,0.,-0.828872660274852));
#34977=DIRECTION('ref_axis',(-0.828872660274852,0.,0.559437318248336));
#34978=DIRECTION('',(0.,-1.,0.));
#34979=DIRECTION('',(-0.828872660274852,0.,0.559437318248336));
#34980=DIRECTION('',(0.,1.,0.));
#34981=DIRECTION('center_axis',(-0.275920768781063,0.,0.961180383359579));
#34982=DIRECTION('ref_axis',(0.961180383359579,0.,0.275920768781063));
#34983=DIRECTION('',(0.,1.,0.));
#34984=DIRECTION('',(-0.961180383359579,0.,-0.275920768781063));
#34985=DIRECTION('center_axis',(-0.275920768781063,0.,0.961180383359579));
#34986=DIRECTION('ref_axis',(0.961180383359579,0.,0.275920768781063));
#34987=DIRECTION('',(0.961180383359579,0.,0.275920768781063));
#34988=DIRECTION('',(0.,1.,0.));
#34989=DIRECTION('center_axis',(-0.422885465331123,0.,0.906183139995266));
#34990=DIRECTION('ref_axis',(0.906183139995266,0.,0.422885465331123));
#34991=DIRECTION('',(0.,1.,0.));
#34992=DIRECTION('',(-0.906183139995266,0.,-0.422885465331123));
#34993=DIRECTION('',(0.,1.,0.));
#34994=DIRECTION('center_axis',(-0.422885465331123,0.,0.906183139995266));
#34995=DIRECTION('ref_axis',(0.906183139995266,0.,0.422885465331123));
#34996=DIRECTION('',(0.,1.,0.));
#34997=DIRECTION('',(0.906183139995266,0.,0.422885465331123));
#34998=DIRECTION('',(0.,1.,0.));
#34999=DIRECTION('center_axis',(-0.422885465331123,0.,-0.906183139995266));
#35000=DIRECTION('ref_axis',(-0.906183139995266,0.,0.422885465331123));
#35001=DIRECTION('',(0.906183139995266,0.,-0.422885465331123));
#35002=DIRECTION('',(0.,-1.,0.));
#35003=DIRECTION('center_axis',(-0.422885465331123,0.,-0.906183139995266));
#35004=DIRECTION('ref_axis',(-0.906183139995266,0.,0.422885465331123));
#35005=DIRECTION('',(0.,-1.,0.));
#35006=DIRECTION('',(-0.906183139995266,0.,0.422885465331123));
#35007=DIRECTION('center_axis',(0.,1.,0.));
#35008=DIRECTION('ref_axis',(0.987688340595138,0.,-0.156434465040231));
#35009=DIRECTION('center_axis',(0.,-1.,0.));
#35010=DIRECTION('ref_axis',(1.,0.,0.));
#35011=DIRECTION('center_axis',(0.,1.,0.));
#35012=DIRECTION('ref_axis',(0.156434465040231,0.,0.987688340595138));
#35013=DIRECTION('center_axis',(0.,1.,0.));
#35014=DIRECTION('ref_axis',(1.,0.,0.));
#35015=DIRECTION('center_axis',(-0.682213967724262,0.,-0.731152584787826));
#35016=DIRECTION('ref_axis',(-0.731152584787826,0.,0.682213967724262));
#35017=DIRECTION('',(0.,-1.,0.));
#35018=DIRECTION('',(-0.731152584787826,0.,0.682213967724262));
#35019=DIRECTION('',(0.,1.,0.));
#35020=DIRECTION('',(0.731152584787826,0.,-0.682213967724262));
#35021=DIRECTION('center_axis',(0.,1.,0.));
#35022=DIRECTION('ref_axis',(0.951056516295153,0.,-0.309016994374948));
#35023=DIRECTION('center_axis',(0.,-1.,0.));
#35024=DIRECTION('ref_axis',(1.,0.,0.));
#35025=DIRECTION('',(-0.992510175710776,0.,-0.122161987175083));
#35026=DIRECTION('center_axis',(-0.122161987175083,0.,0.992510175710776));
#35027=DIRECTION('ref_axis',(0.992510175710776,0.,0.122161987175083));
#35028=DIRECTION('',(0.,1.,0.));
#35029=DIRECTION('',(0.992510175710776,0.,0.122161987175083));
#35030=DIRECTION('center_axis',(0.,1.,0.));
#35031=DIRECTION('ref_axis',(0.309016994374948,0.,0.951056516295153));
#35032=DIRECTION('center_axis',(0.,1.,0.));
#35033=DIRECTION('ref_axis',(1.,0.,0.));
#35034=DIRECTION('center_axis',(-0.788192245176467,0.,-0.615429106107016));
#35035=DIRECTION('ref_axis',(-0.615429106107016,0.,0.788192245176467));
#35036=DIRECTION('',(0.,-1.,0.));
#35037=DIRECTION('',(-0.615429106107016,0.,0.788192245176467));
#35038=DIRECTION('',(0.,1.,0.));
#35039=DIRECTION('',(0.615429106107016,0.,-0.788192245176467));
#35040=DIRECTION('center_axis',(0.,1.,0.));
#35041=DIRECTION('ref_axis',(0.891006524188368,0.,-0.453990499739547));
#35042=DIRECTION('center_axis',(0.,-1.,0.));
#35043=DIRECTION('ref_axis',(1.,0.,0.));
#35044=DIRECTION('',(-0.99940107358355,0.,0.0346048279875384));
#35045=DIRECTION('center_axis',(0.0346048279875384,0.,0.99940107358355));
#35046=DIRECTION('ref_axis',(0.99940107358355,0.,-0.0346048279875384));
#35047=DIRECTION('',(0.,1.,0.));
#35048=DIRECTION('',(0.99940107358355,0.,-0.0346048279875384));
#35049=DIRECTION('center_axis',(0.,1.,0.));
#35050=DIRECTION('ref_axis',(0.453990499739547,0.,0.891006524188368));
#35051=DIRECTION('center_axis',(0.,1.,0.));
#35052=DIRECTION('ref_axis',(1.,0.,0.));
#35053=DIRECTION('center_axis',(-0.874762613692339,0.,-0.484551720341748));
#35054=DIRECTION('ref_axis',(-0.484551720341748,0.,0.874762613692339));
#35055=DIRECTION('',(0.,-1.,0.));
#35056=DIRECTION('',(-0.484551720341748,0.,0.874762613692339));
#35057=DIRECTION('',(0.,1.,0.));
#35058=DIRECTION('',(0.484551720341748,0.,-0.874762613692339));
#35059=DIRECTION('center_axis',(0.,1.,0.));
#35060=DIRECTION('ref_axis',(0.809016994374947,0.,-0.587785252292473));
#35061=DIRECTION('center_axis',(0.,-1.,0.));
#35062=DIRECTION('ref_axis',(1.,0.,0.));
#35063=DIRECTION('',(-0.981683400202696,0.,0.190519557438267));
#35064=DIRECTION('center_axis',(0.190519557438267,0.,0.981683400202696));
#35065=DIRECTION('ref_axis',(0.981683400202696,0.,-0.190519557438267));
#35066=DIRECTION('',(0.,1.,0.));
#35067=DIRECTION('',(0.981683400202696,0.,-0.190519557438267));
#35068=DIRECTION('center_axis',(0.,1.,0.));
#35069=DIRECTION('ref_axis',(0.587785252292473,0.,0.809016994374947));
#35070=DIRECTION('center_axis',(0.,1.,0.));
#35071=DIRECTION('ref_axis',(1.,0.,0.));
#35072=DIRECTION('center_axis',(-0.939793423488437,0.,-0.341743063086705));
#35073=DIRECTION('ref_axis',(-0.341743063086705,0.,0.939793423488437));
#35074=DIRECTION('',(0.,-1.,0.));
#35075=DIRECTION('',(-0.341743063086705,0.,0.939793423488437));
#35076=DIRECTION('',(0.,1.,0.));
#35077=DIRECTION('',(0.341743063086705,0.,-0.939793423488437));
#35078=DIRECTION('center_axis',(0.,1.,0.));
#35079=DIRECTION('ref_axis',(0.707106781186547,0.,-0.707106781186548));
#35080=DIRECTION('center_axis',(0.,-1.,0.));
#35081=DIRECTION('ref_axis',(1.,0.,0.));
#35082=DIRECTION('',(-0.939793423488437,0.,0.341743063086706));
#35083=DIRECTION('center_axis',(0.341743063086706,0.,0.939793423488437));
#35084=DIRECTION('ref_axis',(0.939793423488437,0.,-0.341743063086706));
#35085=DIRECTION('',(0.,1.,0.));
#35086=DIRECTION('',(0.939793423488437,0.,-0.341743063086706));
#35087=DIRECTION('center_axis',(0.,1.,0.));
#35088=DIRECTION('ref_axis',(0.707106781186548,0.,0.707106781186547));
#35089=DIRECTION('center_axis',(0.,1.,0.));
#35090=DIRECTION('ref_axis',(1.,0.,0.));
#35091=DIRECTION('center_axis',(-0.981683400202696,0.,-0.190519557438267));
#35092=DIRECTION('ref_axis',(-0.190519557438267,0.,0.981683400202696));
#35093=DIRECTION('',(0.,-1.,0.));
#35094=DIRECTION('',(-0.190519557438267,0.,0.981683400202696));
#35095=DIRECTION('',(0.,1.,0.));
#35096=DIRECTION('',(0.190519557438267,0.,-0.981683400202696));
#35097=DIRECTION('center_axis',(0.,1.,0.));
#35098=DIRECTION('ref_axis',(0.587785252292473,0.,-0.809016994374948));
#35099=DIRECTION('center_axis',(0.,-1.,0.));
#35100=DIRECTION('ref_axis',(1.,0.,0.));
#35101=DIRECTION('',(-0.874762613692339,0.,0.484551720341749));
#35102=DIRECTION('center_axis',(0.484551720341749,0.,0.874762613692339));
#35103=DIRECTION('ref_axis',(0.874762613692339,0.,-0.484551720341749));
#35104=DIRECTION('',(0.,1.,0.));
#35105=DIRECTION('',(0.874762613692339,0.,-0.484551720341749));
#35106=DIRECTION('center_axis',(0.,1.,0.));
#35107=DIRECTION('ref_axis',(0.809016994374948,0.,0.587785252292473));
#35108=DIRECTION('center_axis',(0.,1.,0.));
#35109=DIRECTION('ref_axis',(1.,0.,0.));
#35110=DIRECTION('center_axis',(-0.99940107358355,0.,-0.0346048279875381));
#35111=DIRECTION('ref_axis',(-0.0346048279875381,0.,0.99940107358355));
#35112=DIRECTION('',(0.,-1.,0.));
#35113=DIRECTION('',(-0.0346048279875381,0.,0.99940107358355));
#35114=DIRECTION('',(0.,1.,0.));
#35115=DIRECTION('',(0.0346048279875381,0.,-0.99940107358355));
#35116=DIRECTION('center_axis',(0.,1.,0.));
#35117=DIRECTION('ref_axis',(0.453990499739547,0.,-0.891006524188368));
#35118=DIRECTION('center_axis',(0.,-1.,0.));
#35119=DIRECTION('ref_axis',(1.,0.,0.));
#35120=DIRECTION('',(-0.788192245176467,0.,0.615429106107016));
#35121=DIRECTION('center_axis',(0.615429106107016,0.,0.788192245176467));
#35122=DIRECTION('ref_axis',(0.788192245176467,0.,-0.615429106107016));
#35123=DIRECTION('',(0.,1.,0.));
#35124=DIRECTION('',(0.788192245176467,0.,-0.615429106107016));
#35125=DIRECTION('center_axis',(0.,1.,0.));
#35126=DIRECTION('ref_axis',(0.891006524188368,0.,0.453990499739547));
#35127=DIRECTION('center_axis',(0.,1.,0.));
#35128=DIRECTION('ref_axis',(1.,0.,0.));
#35129=DIRECTION('center_axis',(-0.992510175710776,0.,0.122161987175083));
#35130=DIRECTION('ref_axis',(0.122161987175083,0.,0.992510175710776));
#35131=DIRECTION('',(0.,-1.,0.));
#35132=DIRECTION('',(0.122161987175083,0.,0.992510175710776));
#35133=DIRECTION('',(0.,1.,0.));
#35134=DIRECTION('',(-0.122161987175083,0.,-0.992510175710776));
#35135=DIRECTION('center_axis',(0.,1.,0.));
#35136=DIRECTION('ref_axis',(0.309016994374947,0.,-0.951056516295154));
#35137=DIRECTION('center_axis',(0.,-1.,0.));
#35138=DIRECTION('ref_axis',(1.,0.,0.));
#35139=DIRECTION('',(-0.682213967724262,0.,0.731152584787827));
#35140=DIRECTION('center_axis',(0.731152584787827,0.,0.682213967724262));
#35141=DIRECTION('ref_axis',(0.682213967724262,0.,-0.731152584787827));
#35142=DIRECTION('',(0.,1.,0.));
#35143=DIRECTION('',(0.682213967724262,0.,-0.731152584787827));
#35144=DIRECTION('center_axis',(0.,1.,0.));
#35145=DIRECTION('ref_axis',(0.951056516295154,0.,0.309016994374947));
#35146=DIRECTION('center_axis',(0.,1.,0.));
#35147=DIRECTION('ref_axis',(1.,0.,0.));
#35148=DIRECTION('center_axis',(-0.961180383359579,0.,0.275920768781063));
#35149=DIRECTION('ref_axis',(0.275920768781063,0.,0.961180383359579));
#35150=DIRECTION('',(0.,-1.,0.));
#35151=DIRECTION('',(0.275920768781063,0.,0.961180383359579));
#35152=DIRECTION('',(0.,1.,0.));
#35153=DIRECTION('',(-0.275920768781063,0.,-0.961180383359579));
#35154=DIRECTION('center_axis',(0.,1.,0.));
#35155=DIRECTION('ref_axis',(0.156434465040231,0.,-0.987688340595138));
#35156=DIRECTION('center_axis',(0.,-1.,0.));
#35157=DIRECTION('ref_axis',(1.,0.,0.));
#35158=DIRECTION('',(-0.559437318248335,0.,0.828872660274852));
#35159=DIRECTION('center_axis',(0.828872660274853,0.,0.559437318248335));
#35160=DIRECTION('ref_axis',(0.559437318248335,0.,-0.828872660274853));
#35161=DIRECTION('',(0.,1.,0.));
#35162=DIRECTION('',(0.559437318248335,0.,-0.828872660274852));
#35163=DIRECTION('center_axis',(0.,1.,0.));
#35164=DIRECTION('ref_axis',(0.987688340595138,0.,0.156434465040231));
#35165=DIRECTION('center_axis',(0.,1.,0.));
#35166=DIRECTION('ref_axis',(1.,0.,0.));
#35167=DIRECTION('center_axis',(-0.906183139995266,0.,0.422885465331123));
#35168=DIRECTION('ref_axis',(0.422885465331123,0.,0.906183139995266));
#35169=DIRECTION('',(0.,-1.,0.));
#35170=DIRECTION('',(0.422885465331123,0.,0.906183139995266));
#35171=DIRECTION('',(0.,1.,0.));
#35172=DIRECTION('',(-0.422885465331123,0.,-0.906183139995266));
#35173=DIRECTION('center_axis',(0.,1.,0.));
#35174=DIRECTION('ref_axis',(-1.83697019872103E-16,0.,-1.));
#35175=DIRECTION('center_axis',(0.,-1.,0.));
#35176=DIRECTION('ref_axis',(1.,0.,0.));
#35177=DIRECTION('',(-0.422885465331123,0.,0.906183139995266));
#35178=DIRECTION('center_axis',(0.906183139995266,0.,0.422885465331123));
#35179=DIRECTION('ref_axis',(0.422885465331123,0.,-0.906183139995266));
#35180=DIRECTION('',(0.,1.,0.));
#35181=DIRECTION('',(0.422885465331123,0.,-0.906183139995266));
#35182=DIRECTION('center_axis',(0.,1.,0.));
#35183=DIRECTION('ref_axis',(1.,0.,-1.83697019872103E-16));
#35184=DIRECTION('center_axis',(0.,1.,0.));
#35185=DIRECTION('ref_axis',(1.,0.,0.));
#35186=DIRECTION('center_axis',(-0.828872660274852,0.,0.559437318248335));
#35187=DIRECTION('ref_axis',(0.559437318248335,0.,0.828872660274853));
#35188=DIRECTION('',(0.,-1.,0.));
#35189=DIRECTION('',(0.559437318248335,0.,0.828872660274852));
#35190=DIRECTION('',(0.,1.,0.));
#35191=DIRECTION('',(-0.559437318248335,0.,-0.828872660274852));
#35192=DIRECTION('center_axis',(0.,1.,0.));
#35193=DIRECTION('ref_axis',(-0.156434465040231,0.,-0.987688340595138));
#35194=DIRECTION('center_axis',(0.,-1.,0.));
#35195=DIRECTION('ref_axis',(1.,0.,0.));
#35196=DIRECTION('',(-0.275920768781063,0.,0.961180383359579));
#35197=DIRECTION('center_axis',(0.961180383359579,0.,0.275920768781063));
#35198=DIRECTION('ref_axis',(0.275920768781063,0.,-0.961180383359579));
#35199=DIRECTION('',(0.,1.,0.));
#35200=DIRECTION('',(0.275920768781063,0.,-0.961180383359579));
#35201=DIRECTION('center_axis',(0.,1.,0.));
#35202=DIRECTION('ref_axis',(0.987688340595138,0.,-0.156434465040231));
#35203=DIRECTION('center_axis',(0.,1.,0.));
#35204=DIRECTION('ref_axis',(1.,0.,0.));
#35205=DIRECTION('center_axis',(-0.731152584787826,0.,0.682213967724262));
#35206=DIRECTION('ref_axis',(0.682213967724262,0.,0.731152584787826));
#35207=DIRECTION('',(0.,-1.,0.));
#35208=DIRECTION('',(0.682213967724262,0.,0.731152584787826));
#35209=DIRECTION('',(0.,1.,0.));
#35210=DIRECTION('',(-0.682213967724262,0.,-0.731152584787826));
#35211=DIRECTION('center_axis',(0.,1.,0.));
#35212=DIRECTION('ref_axis',(-0.309016994374948,0.,-0.951056516295153));
#35213=DIRECTION('center_axis',(0.,-1.,0.));
#35214=DIRECTION('ref_axis',(1.,0.,0.));
#35215=DIRECTION('',(-0.122161987175083,0.,0.992510175710776));
#35216=DIRECTION('center_axis',(0.992510175710776,0.,0.122161987175083));
#35217=DIRECTION('ref_axis',(0.122161987175083,0.,-0.992510175710776));
#35218=DIRECTION('',(0.,1.,0.));
#35219=DIRECTION('',(0.122161987175083,0.,-0.992510175710776));
#35220=DIRECTION('center_axis',(0.,1.,0.));
#35221=DIRECTION('ref_axis',(0.951056516295153,0.,-0.309016994374948));
#35222=DIRECTION('center_axis',(0.,1.,0.));
#35223=DIRECTION('ref_axis',(1.,0.,0.));
#35224=DIRECTION('center_axis',(-0.615429106107016,0.,0.788192245176467));
#35225=DIRECTION('ref_axis',(0.788192245176467,0.,0.615429106107016));
#35226=DIRECTION('',(0.,-1.,0.));
#35227=DIRECTION('',(0.788192245176467,0.,0.615429106107016));
#35228=DIRECTION('',(0.,1.,0.));
#35229=DIRECTION('',(-0.788192245176467,0.,-0.615429106107016));
#35230=DIRECTION('center_axis',(0.,1.,0.));
#35231=DIRECTION('ref_axis',(-0.453990499739547,0.,-0.891006524188368));
#35232=DIRECTION('center_axis',(0.,-1.,0.));
#35233=DIRECTION('ref_axis',(1.,0.,0.));
#35234=DIRECTION('',(0.0346048279875384,0.,0.99940107358355));
#35235=DIRECTION('center_axis',(0.99940107358355,0.,-0.0346048279875384));
#35236=DIRECTION('ref_axis',(-0.0346048279875384,0.,-0.99940107358355));
#35237=DIRECTION('',(0.,1.,0.));
#35238=DIRECTION('',(-0.0346048279875384,0.,-0.99940107358355));
#35239=DIRECTION('center_axis',(0.,1.,0.));
#35240=DIRECTION('ref_axis',(0.891006524188368,0.,-0.453990499739547));
#35241=DIRECTION('center_axis',(0.,1.,0.));
#35242=DIRECTION('ref_axis',(1.,0.,0.));
#35243=DIRECTION('center_axis',(-0.484551720341748,0.,0.874762613692339));
#35244=DIRECTION('ref_axis',(0.874762613692339,0.,0.484551720341748));
#35245=DIRECTION('',(0.,-1.,0.));
#35246=DIRECTION('',(0.874762613692339,0.,0.484551720341748));
#35247=DIRECTION('',(0.,1.,0.));
#35248=DIRECTION('',(-0.874762613692339,0.,-0.484551720341748));
#35249=DIRECTION('center_axis',(0.,1.,0.));
#35250=DIRECTION('ref_axis',(-0.587785252292473,0.,-0.809016994374947));
#35251=DIRECTION('center_axis',(0.,-1.,0.));
#35252=DIRECTION('ref_axis',(1.,0.,0.));
#35253=DIRECTION('',(0.190519557438267,0.,0.981683400202696));
#35254=DIRECTION('center_axis',(0.981683400202696,0.,-0.190519557438267));
#35255=DIRECTION('ref_axis',(-0.190519557438267,0.,-0.981683400202696));
#35256=DIRECTION('',(0.,1.,0.));
#35257=DIRECTION('',(-0.190519557438267,0.,-0.981683400202696));
#35258=DIRECTION('center_axis',(0.,1.,0.));
#35259=DIRECTION('ref_axis',(0.809016994374947,0.,-0.587785252292473));
#35260=DIRECTION('center_axis',(0.,1.,0.));
#35261=DIRECTION('ref_axis',(1.,0.,0.));
#35262=DIRECTION('center_axis',(-0.341743063086705,0.,0.939793423488437));
#35263=DIRECTION('ref_axis',(0.939793423488437,0.,0.341743063086705));
#35264=DIRECTION('',(0.,-1.,0.));
#35265=DIRECTION('',(0.939793423488437,0.,0.341743063086705));
#35266=DIRECTION('',(0.,1.,0.));
#35267=DIRECTION('',(-0.939793423488437,0.,-0.341743063086705));
#35268=DIRECTION('center_axis',(0.,1.,0.));
#35269=DIRECTION('ref_axis',(-0.707106781186548,0.,-0.707106781186547));
#35270=DIRECTION('center_axis',(0.,-1.,0.));
#35271=DIRECTION('ref_axis',(1.,0.,0.));
#35272=DIRECTION('',(0.341743063086706,0.,0.939793423488437));
#35273=DIRECTION('center_axis',(0.939793423488437,0.,-0.341743063086706));
#35274=DIRECTION('ref_axis',(-0.341743063086706,0.,-0.939793423488437));
#35275=DIRECTION('',(0.,1.,0.));
#35276=DIRECTION('',(-0.341743063086706,0.,-0.939793423488437));
#35277=DIRECTION('center_axis',(0.,1.,0.));
#35278=DIRECTION('ref_axis',(0.707106781186547,0.,-0.707106781186548));
#35279=DIRECTION('center_axis',(0.,1.,0.));
#35280=DIRECTION('ref_axis',(1.,0.,0.));
#35281=DIRECTION('center_axis',(-0.190519557438267,0.,0.981683400202696));
#35282=DIRECTION('ref_axis',(0.981683400202696,0.,0.190519557438267));
#35283=DIRECTION('',(0.,-1.,0.));
#35284=DIRECTION('',(0.981683400202696,0.,0.190519557438267));
#35285=DIRECTION('',(0.,1.,0.));
#35286=DIRECTION('',(-0.981683400202696,0.,-0.190519557438267));
#35287=DIRECTION('center_axis',(0.,1.,0.));
#35288=DIRECTION('ref_axis',(-0.809016994374947,0.,-0.587785252292473));
#35289=DIRECTION('center_axis',(0.,-1.,0.));
#35290=DIRECTION('ref_axis',(1.,0.,0.));
#35291=DIRECTION('',(0.484551720341748,0.,0.874762613692339));
#35292=DIRECTION('center_axis',(0.874762613692339,0.,-0.484551720341748));
#35293=DIRECTION('ref_axis',(-0.484551720341748,0.,-0.874762613692339));
#35294=DIRECTION('',(0.,1.,0.));
#35295=DIRECTION('',(-0.484551720341748,0.,-0.874762613692339));
#35296=DIRECTION('center_axis',(0.,1.,0.));
#35297=DIRECTION('ref_axis',(0.587785252292473,0.,-0.809016994374947));
#35298=DIRECTION('center_axis',(0.,1.,0.));
#35299=DIRECTION('ref_axis',(1.,0.,0.));
#35300=DIRECTION('center_axis',(-0.0346048279875381,0.,0.99940107358355));
#35301=DIRECTION('ref_axis',(0.99940107358355,0.,0.0346048279875381));
#35302=DIRECTION('',(0.,-1.,0.));
#35303=DIRECTION('',(0.99940107358355,0.,0.0346048279875381));
#35304=DIRECTION('',(0.,1.,0.));
#35305=DIRECTION('',(-0.99940107358355,0.,-0.0346048279875381));
#35306=DIRECTION('center_axis',(0.,1.,0.));
#35307=DIRECTION('ref_axis',(-0.891006524188368,0.,-0.453990499739547));
#35308=DIRECTION('center_axis',(0.,-1.,0.));
#35309=DIRECTION('ref_axis',(1.,0.,0.));
#35310=DIRECTION('',(0.615429106107016,0.,0.788192245176467));
#35311=DIRECTION('center_axis',(0.788192245176467,0.,-0.615429106107016));
#35312=DIRECTION('ref_axis',(-0.615429106107016,0.,-0.788192245176467));
#35313=DIRECTION('',(0.,1.,0.));
#35314=DIRECTION('',(-0.615429106107016,0.,-0.788192245176467));
#35315=DIRECTION('center_axis',(0.,1.,0.));
#35316=DIRECTION('ref_axis',(0.453990499739547,0.,-0.891006524188368));
#35317=DIRECTION('center_axis',(0.,1.,0.));
#35318=DIRECTION('ref_axis',(1.,0.,0.));
#35319=DIRECTION('center_axis',(0.122161987175083,0.,0.992510175710776));
#35320=DIRECTION('ref_axis',(0.992510175710776,0.,-0.122161987175083));
#35321=DIRECTION('',(0.,-1.,0.));
#35322=DIRECTION('',(0.992510175710776,0.,-0.122161987175083));
#35323=DIRECTION('',(0.,1.,0.));
#35324=DIRECTION('',(-0.992510175710776,0.,0.122161987175083));
#35325=DIRECTION('center_axis',(0.,1.,0.));
#35326=DIRECTION('ref_axis',(-0.951056516295154,0.,-0.309016994374947));
#35327=DIRECTION('center_axis',(0.,-1.,0.));
#35328=DIRECTION('ref_axis',(1.,0.,0.));
#35329=DIRECTION('',(0.731152584787827,0.,0.682213967724262));
#35330=DIRECTION('center_axis',(0.682213967724262,0.,-0.731152584787827));
#35331=DIRECTION('ref_axis',(-0.731152584787827,0.,-0.682213967724262));
#35332=DIRECTION('',(0.,1.,0.));
#35333=DIRECTION('',(-0.731152584787827,0.,-0.682213967724262));
#35334=DIRECTION('center_axis',(0.,1.,0.));
#35335=DIRECTION('ref_axis',(0.309016994374947,0.,-0.951056516295154));
#35336=DIRECTION('center_axis',(0.,1.,0.));
#35337=DIRECTION('ref_axis',(1.,0.,0.));
#35338=DIRECTION('center_axis',(0.275920768781063,0.,0.961180383359579));
#35339=DIRECTION('ref_axis',(0.961180383359579,0.,-0.275920768781063));
#35340=DIRECTION('',(0.,-1.,0.));
#35341=DIRECTION('',(0.961180383359579,0.,-0.275920768781063));
#35342=DIRECTION('',(0.,1.,0.));
#35343=DIRECTION('',(-0.961180383359579,0.,0.275920768781063));
#35344=DIRECTION('center_axis',(0.,1.,0.));
#35345=DIRECTION('ref_axis',(-0.987688340595138,0.,-0.156434465040231));
#35346=DIRECTION('center_axis',(0.,-1.,0.));
#35347=DIRECTION('ref_axis',(1.,0.,0.));
#35348=DIRECTION('',(0.828872660274852,0.,0.559437318248335));
#35349=DIRECTION('center_axis',(0.559437318248335,0.,-0.828872660274853));
#35350=DIRECTION('ref_axis',(-0.828872660274853,0.,-0.559437318248335));
#35351=DIRECTION('',(0.,1.,0.));
#35352=DIRECTION('',(-0.828872660274852,0.,-0.559437318248335));
#35353=DIRECTION('center_axis',(0.,1.,0.));
#35354=DIRECTION('ref_axis',(0.156434465040231,0.,-0.987688340595138));
#35355=DIRECTION('center_axis',(0.,1.,0.));
#35356=DIRECTION('ref_axis',(1.,0.,0.));
#35357=DIRECTION('center_axis',(0.422885465331123,0.,0.906183139995266));
#35358=DIRECTION('ref_axis',(0.906183139995266,0.,-0.422885465331123));
#35359=DIRECTION('',(0.,-1.,0.));
#35360=DIRECTION('',(0.906183139995266,0.,-0.422885465331123));
#35361=DIRECTION('',(0.,1.,0.));
#35362=DIRECTION('',(-0.906183139995266,0.,0.422885465331123));
#35363=DIRECTION('center_axis',(0.,1.,0.));
#35364=DIRECTION('ref_axis',(-1.,0.,1.22464679914735E-16));
#35365=DIRECTION('center_axis',(0.,-1.,0.));
#35366=DIRECTION('ref_axis',(1.,0.,0.));
#35367=DIRECTION('',(0.906183139995266,0.,0.422885465331123));
#35368=DIRECTION('center_axis',(0.,-1.,0.));
#35369=DIRECTION('ref_axis',(1.,0.,0.));
#35370=DIRECTION('center_axis',(0.422885465331123,0.,-0.906183139995266));
#35371=DIRECTION('ref_axis',(-0.906183139995266,0.,-0.422885465331123));
#35372=DIRECTION('',(0.,1.,0.));
#35373=DIRECTION('',(-0.906183139995266,0.,-0.422885465331123));
#35374=DIRECTION('center_axis',(0.,1.,0.));
#35375=DIRECTION('ref_axis',(-1.22464679914735E-16,0.,-1.));
#35376=DIRECTION('center_axis',(0.,1.,0.));
#35377=DIRECTION('ref_axis',(1.,0.,0.));
#35378=DIRECTION('center_axis',(0.,1.,0.));
#35379=DIRECTION('ref_axis',(1.,0.,0.));
#35380=DIRECTION('center_axis',(0.559437318248335,0.,0.828872660274852));
#35381=DIRECTION('ref_axis',(0.828872660274852,0.,-0.559437318248335));
#35382=DIRECTION('',(0.,-1.,0.));
#35383=DIRECTION('',(0.828872660274852,0.,-0.559437318248335));
#35384=DIRECTION('',(0.,1.,0.));
#35385=DIRECTION('',(-0.828872660274852,0.,0.559437318248335));
#35386=DIRECTION('center_axis',(0.,1.,0.));
#35387=DIRECTION('ref_axis',(-0.987688340595138,0.,0.156434465040231));
#35388=DIRECTION('center_axis',(0.,-1.,0.));
#35389=DIRECTION('ref_axis',(1.,0.,0.));
#35390=DIRECTION('',(0.961180383359579,0.,0.275920768781063));
#35391=DIRECTION('center_axis',(0.275920768781063,0.,-0.961180383359579));
#35392=DIRECTION('ref_axis',(-0.961180383359579,0.,-0.275920768781063));
#35393=DIRECTION('',(0.,1.,0.));
#35394=DIRECTION('',(-0.961180383359579,0.,-0.275920768781063));
#35395=DIRECTION('center_axis',(0.,1.,0.));
#35396=DIRECTION('ref_axis',(-0.156434465040231,0.,-0.987688340595138));
#35397=DIRECTION('center_axis',(0.,1.,0.));
#35398=DIRECTION('ref_axis',(1.,0.,0.));
#35399=DIRECTION('center_axis',(0.682213967724262,0.,0.731152584787826));
#35400=DIRECTION('ref_axis',(0.731152584787826,0.,-0.682213967724262));
#35401=DIRECTION('',(0.,-1.,0.));
#35402=DIRECTION('',(0.731152584787826,0.,-0.682213967724262));
#35403=DIRECTION('',(0.,1.,0.));
#35404=DIRECTION('',(-0.731152584787826,0.,0.682213967724262));
#35405=DIRECTION('center_axis',(0.,1.,0.));
#35406=DIRECTION('ref_axis',(-0.951056516295153,0.,0.309016994374948));
#35407=DIRECTION('center_axis',(0.,-1.,0.));
#35408=DIRECTION('ref_axis',(1.,0.,0.));
#35409=DIRECTION('',(0.992510175710776,0.,0.122161987175083));
#35410=DIRECTION('center_axis',(0.122161987175083,0.,-0.992510175710776));
#35411=DIRECTION('ref_axis',(-0.992510175710776,0.,-0.122161987175083));
#35412=DIRECTION('',(0.,1.,0.));
#35413=DIRECTION('',(-0.992510175710776,0.,-0.122161987175083));
#35414=DIRECTION('center_axis',(0.,1.,0.));
#35415=DIRECTION('ref_axis',(-0.309016994374948,0.,-0.951056516295153));
#35416=DIRECTION('center_axis',(0.,1.,0.));
#35417=DIRECTION('ref_axis',(1.,0.,0.));
#35418=DIRECTION('center_axis',(0.788192245176467,0.,0.615429106107016));
#35419=DIRECTION('ref_axis',(0.615429106107016,0.,-0.788192245176467));
#35420=DIRECTION('',(0.,-1.,0.));
#35421=DIRECTION('',(0.615429106107016,0.,-0.788192245176467));
#35422=DIRECTION('',(0.,1.,0.));
#35423=DIRECTION('',(-0.615429106107016,0.,0.788192245176467));
#35424=DIRECTION('center_axis',(0.,1.,0.));
#35425=DIRECTION('ref_axis',(-0.891006524188368,0.,0.453990499739547));
#35426=DIRECTION('center_axis',(0.,-1.,0.));
#35427=DIRECTION('ref_axis',(1.,0.,0.));
#35428=DIRECTION('',(0.99940107358355,0.,-0.0346048279875384));
#35429=DIRECTION('center_axis',(-0.0346048279875384,0.,-0.99940107358355));
#35430=DIRECTION('ref_axis',(-0.99940107358355,0.,0.0346048279875384));
#35431=DIRECTION('',(0.,1.,0.));
#35432=DIRECTION('',(-0.99940107358355,0.,0.0346048279875384));
#35433=DIRECTION('center_axis',(0.,1.,0.));
#35434=DIRECTION('ref_axis',(-0.453990499739547,0.,-0.891006524188368));
#35435=DIRECTION('center_axis',(0.,1.,0.));
#35436=DIRECTION('ref_axis',(1.,0.,0.));
#35437=DIRECTION('center_axis',(0.874762613692339,0.,0.484551720341748));
#35438=DIRECTION('ref_axis',(0.484551720341748,0.,-0.874762613692339));
#35439=DIRECTION('',(0.,-1.,0.));
#35440=DIRECTION('',(0.484551720341748,0.,-0.874762613692339));
#35441=DIRECTION('',(0.,1.,0.));
#35442=DIRECTION('',(-0.484551720341748,0.,0.874762613692339));
#35443=DIRECTION('center_axis',(0.,1.,0.));
#35444=DIRECTION('ref_axis',(-0.809016994374947,0.,0.587785252292473));
#35445=DIRECTION('center_axis',(0.,-1.,0.));
#35446=DIRECTION('ref_axis',(1.,0.,0.));
#35447=DIRECTION('',(0.981683400202696,0.,-0.190519557438267));
#35448=DIRECTION('center_axis',(-0.190519557438267,0.,-0.981683400202696));
#35449=DIRECTION('ref_axis',(-0.981683400202696,0.,0.190519557438267));
#35450=DIRECTION('',(0.,1.,0.));
#35451=DIRECTION('',(-0.981683400202696,0.,0.190519557438267));
#35452=DIRECTION('center_axis',(0.,1.,0.));
#35453=DIRECTION('ref_axis',(-0.587785252292473,0.,-0.809016994374947));
#35454=DIRECTION('center_axis',(0.,1.,0.));
#35455=DIRECTION('ref_axis',(1.,0.,0.));
#35456=DIRECTION('center_axis',(0.939793423488437,0.,0.341743063086706));
#35457=DIRECTION('ref_axis',(0.341743063086706,0.,-0.939793423488437));
#35458=DIRECTION('',(0.,-1.,0.));
#35459=DIRECTION('',(0.341743063086706,0.,-0.939793423488437));
#35460=DIRECTION('',(0.,1.,0.));
#35461=DIRECTION('',(-0.341743063086706,0.,0.939793423488437));
#35462=DIRECTION('center_axis',(0.,1.,0.));
#35463=DIRECTION('ref_axis',(-0.707106781186547,0.,0.707106781186548));
#35464=DIRECTION('center_axis',(0.,-1.,0.));
#35465=DIRECTION('ref_axis',(1.,0.,0.));
#35466=DIRECTION('',(0.939793423488437,0.,-0.341743063086706));
#35467=DIRECTION('center_axis',(-0.341743063086706,0.,-0.939793423488437));
#35468=DIRECTION('ref_axis',(-0.939793423488437,0.,0.341743063086706));
#35469=DIRECTION('',(0.,1.,0.));
#35470=DIRECTION('',(-0.939793423488437,0.,0.341743063086706));
#35471=DIRECTION('center_axis',(0.,1.,0.));
#35472=DIRECTION('ref_axis',(-0.707106781186548,0.,-0.707106781186547));
#35473=DIRECTION('center_axis',(0.,1.,0.));
#35474=DIRECTION('ref_axis',(1.,0.,0.));
#35475=DIRECTION('center_axis',(0.981683400202696,0.,0.190519557438267));
#35476=DIRECTION('ref_axis',(0.190519557438267,0.,-0.981683400202696));
#35477=DIRECTION('',(0.,-1.,0.));
#35478=DIRECTION('',(0.190519557438267,0.,-0.981683400202696));
#35479=DIRECTION('',(0.,1.,0.));
#35480=DIRECTION('',(-0.190519557438267,0.,0.981683400202696));
#35481=DIRECTION('center_axis',(0.,1.,0.));
#35482=DIRECTION('ref_axis',(-0.587785252292473,0.,0.809016994374947));
#35483=DIRECTION('center_axis',(0.,-1.,0.));
#35484=DIRECTION('ref_axis',(1.,0.,0.));
#35485=DIRECTION('',(0.874762613692339,0.,-0.484551720341748));
#35486=DIRECTION('center_axis',(-0.484551720341748,0.,-0.874762613692339));
#35487=DIRECTION('ref_axis',(-0.874762613692339,0.,0.484551720341748));
#35488=DIRECTION('',(0.,1.,0.));
#35489=DIRECTION('',(-0.874762613692339,0.,0.484551720341748));
#35490=DIRECTION('center_axis',(0.,1.,0.));
#35491=DIRECTION('ref_axis',(-0.809016994374947,0.,-0.587785252292473));
#35492=DIRECTION('center_axis',(0.,1.,0.));
#35493=DIRECTION('ref_axis',(1.,0.,0.));
#35494=DIRECTION('center_axis',(0.99940107358355,0.,0.0346048279875382));
#35495=DIRECTION('ref_axis',(0.0346048279875382,0.,-0.99940107358355));
#35496=DIRECTION('',(0.,-1.,0.));
#35497=DIRECTION('',(0.0346048279875382,0.,-0.99940107358355));
#35498=DIRECTION('',(0.,1.,0.));
#35499=DIRECTION('',(-0.0346048279875382,0.,0.99940107358355));
#35500=DIRECTION('center_axis',(0.,1.,0.));
#35501=DIRECTION('ref_axis',(-0.453990499739547,0.,0.891006524188368));
#35502=DIRECTION('center_axis',(0.,-1.,0.));
#35503=DIRECTION('ref_axis',(1.,0.,0.));
#35504=DIRECTION('',(0.788192245176467,0.,-0.615429106107016));
#35505=DIRECTION('center_axis',(-0.615429106107016,0.,-0.788192245176467));
#35506=DIRECTION('ref_axis',(-0.788192245176467,0.,0.615429106107016));
#35507=DIRECTION('',(0.,1.,0.));
#35508=DIRECTION('',(-0.788192245176467,0.,0.615429106107016));
#35509=DIRECTION('center_axis',(0.,1.,0.));
#35510=DIRECTION('ref_axis',(-0.891006524188368,0.,-0.453990499739547));
#35511=DIRECTION('center_axis',(0.,1.,0.));
#35512=DIRECTION('ref_axis',(1.,0.,0.));
#35513=DIRECTION('center_axis',(0.992510175710776,0.,-0.122161987175083));
#35514=DIRECTION('ref_axis',(-0.122161987175083,0.,-0.992510175710776));
#35515=DIRECTION('',(0.,-1.,0.));
#35516=DIRECTION('',(-0.122161987175083,0.,-0.992510175710776));
#35517=DIRECTION('',(0.,1.,0.));
#35518=DIRECTION('',(0.122161987175083,0.,0.992510175710776));
#35519=DIRECTION('center_axis',(0.,1.,0.));
#35520=DIRECTION('ref_axis',(-0.309016994374947,0.,0.951056516295154));
#35521=DIRECTION('center_axis',(0.,-1.,0.));
#35522=DIRECTION('ref_axis',(1.,0.,0.));
#35523=DIRECTION('',(0.682213967724262,0.,-0.731152584787827));
#35524=DIRECTION('center_axis',(-0.731152584787827,0.,-0.682213967724262));
#35525=DIRECTION('ref_axis',(-0.682213967724262,0.,0.731152584787827));
#35526=DIRECTION('',(0.,1.,0.));
#35527=DIRECTION('',(-0.682213967724262,0.,0.731152584787827));
#35528=DIRECTION('center_axis',(0.,1.,0.));
#35529=DIRECTION('ref_axis',(-0.951056516295154,0.,-0.309016994374947));
#35530=DIRECTION('center_axis',(0.,1.,0.));
#35531=DIRECTION('ref_axis',(1.,0.,0.));
#35532=DIRECTION('center_axis',(0.961180383359579,0.,-0.275920768781063));
#35533=DIRECTION('ref_axis',(-0.275920768781063,0.,-0.961180383359579));
#35534=DIRECTION('',(0.,-1.,0.));
#35535=DIRECTION('',(-0.275920768781063,0.,-0.961180383359579));
#35536=DIRECTION('',(0.,1.,0.));
#35537=DIRECTION('',(0.275920768781063,0.,0.961180383359579));
#35538=DIRECTION('center_axis',(0.,1.,0.));
#35539=DIRECTION('ref_axis',(-0.156434465040231,0.,0.987688340595138));
#35540=DIRECTION('center_axis',(0.,-1.,0.));
#35541=DIRECTION('ref_axis',(1.,0.,0.));
#35542=DIRECTION('',(0.559437318248335,0.,-0.828872660274852));
#35543=DIRECTION('center_axis',(-0.828872660274852,0.,-0.559437318248335));
#35544=DIRECTION('ref_axis',(-0.559437318248335,0.,0.828872660274853));
#35545=DIRECTION('',(0.,1.,0.));
#35546=DIRECTION('',(-0.559437318248335,0.,0.828872660274852));
#35547=DIRECTION('center_axis',(0.,1.,0.));
#35548=DIRECTION('ref_axis',(-0.987688340595138,0.,-0.156434465040231));
#35549=DIRECTION('center_axis',(0.,1.,0.));
#35550=DIRECTION('ref_axis',(1.,0.,0.));
#35551=DIRECTION('center_axis',(0.906183139995266,0.,-0.422885465331123));
#35552=DIRECTION('ref_axis',(-0.422885465331123,0.,-0.906183139995266));
#35553=DIRECTION('',(0.,-1.,0.));
#35554=DIRECTION('',(-0.422885465331123,0.,-0.906183139995266));
#35555=DIRECTION('',(0.,1.,0.));
#35556=DIRECTION('',(0.422885465331123,0.,0.906183139995266));
#35557=DIRECTION('center_axis',(0.,1.,0.));
#35558=DIRECTION('ref_axis',(6.12323399573677E-17,0.,1.));
#35559=DIRECTION('center_axis',(0.,-1.,0.));
#35560=DIRECTION('ref_axis',(1.,0.,0.));
#35561=DIRECTION('',(0.422885465331123,0.,-0.906183139995266));
#35562=DIRECTION('center_axis',(-0.906183139995266,0.,-0.422885465331123));
#35563=DIRECTION('ref_axis',(-0.422885465331123,0.,0.906183139995266));
#35564=DIRECTION('',(0.,1.,0.));
#35565=DIRECTION('',(-0.422885465331123,0.,0.906183139995266));
#35566=DIRECTION('center_axis',(0.,1.,0.));
#35567=DIRECTION('ref_axis',(-1.,0.,6.12323399573677E-17));
#35568=DIRECTION('center_axis',(0.,1.,0.));
#35569=DIRECTION('ref_axis',(1.,0.,0.));
#35570=DIRECTION('center_axis',(0.828872660274852,0.,-0.559437318248335));
#35571=DIRECTION('ref_axis',(-0.559437318248335,0.,-0.828872660274853));
#35572=DIRECTION('',(0.,-1.,0.));
#35573=DIRECTION('',(-0.559437318248335,0.,-0.828872660274852));
#35574=DIRECTION('',(0.,1.,0.));
#35575=DIRECTION('',(0.559437318248335,0.,0.828872660274852));
#35576=DIRECTION('center_axis',(0.,1.,0.));
#35577=DIRECTION('ref_axis',(0.156434465040231,0.,0.987688340595138));
#35578=DIRECTION('center_axis',(0.,-1.,0.));
#35579=DIRECTION('ref_axis',(1.,0.,0.));
#35580=DIRECTION('',(0.275920768781063,0.,-0.961180383359579));
#35581=DIRECTION('center_axis',(-0.961180383359579,0.,-0.275920768781063));
#35582=DIRECTION('ref_axis',(-0.275920768781063,0.,0.961180383359579));
#35583=DIRECTION('',(0.,1.,0.));
#35584=DIRECTION('',(-0.275920768781063,0.,0.961180383359579));
#35585=DIRECTION('center_axis',(0.,1.,0.));
#35586=DIRECTION('ref_axis',(-0.987688340595138,0.,0.156434465040231));
#35587=DIRECTION('center_axis',(0.,1.,0.));
#35588=DIRECTION('ref_axis',(1.,0.,0.));
#35589=DIRECTION('center_axis',(0.731152584787827,0.,-0.682213967724262));
#35590=DIRECTION('ref_axis',(-0.682213967724262,0.,-0.731152584787827));
#35591=DIRECTION('',(0.,-1.,0.));
#35592=DIRECTION('',(-0.682213967724262,0.,-0.731152584787826));
#35593=DIRECTION('',(0.,1.,0.));
#35594=DIRECTION('',(0.682213967724262,0.,0.731152584787826));
#35595=DIRECTION('center_axis',(0.,1.,0.));
#35596=DIRECTION('ref_axis',(0.309016994374948,0.,0.951056516295154));
#35597=DIRECTION('center_axis',(0.,-1.,0.));
#35598=DIRECTION('ref_axis',(1.,0.,0.));
#35599=DIRECTION('',(0.122161987175083,0.,-0.992510175710776));
#35600=DIRECTION('center_axis',(-0.992510175710776,0.,-0.122161987175083));
#35601=DIRECTION('ref_axis',(-0.122161987175083,0.,0.992510175710776));
#35602=DIRECTION('',(0.,1.,0.));
#35603=DIRECTION('',(-0.122161987175083,0.,0.992510175710776));
#35604=DIRECTION('center_axis',(0.,1.,0.));
#35605=DIRECTION('ref_axis',(-0.951056516295154,0.,0.309016994374948));
#35606=DIRECTION('center_axis',(0.,1.,0.));
#35607=DIRECTION('ref_axis',(1.,0.,0.));
#35608=DIRECTION('center_axis',(0.615429106107016,0.,-0.788192245176467));
#35609=DIRECTION('ref_axis',(-0.788192245176467,0.,-0.615429106107016));
#35610=DIRECTION('',(0.,-1.,0.));
#35611=DIRECTION('',(-0.788192245176467,0.,-0.615429106107016));
#35612=DIRECTION('',(0.,1.,0.));
#35613=DIRECTION('',(0.788192245176467,0.,0.615429106107016));
#35614=DIRECTION('center_axis',(0.,1.,0.));
#35615=DIRECTION('ref_axis',(0.453990499739547,0.,0.891006524188368));
#35616=DIRECTION('center_axis',(0.,-1.,0.));
#35617=DIRECTION('ref_axis',(1.,0.,0.));
#35618=DIRECTION('',(-0.0346048279875384,0.,-0.99940107358355));
#35619=DIRECTION('center_axis',(-0.99940107358355,0.,0.0346048279875384));
#35620=DIRECTION('ref_axis',(0.0346048279875384,0.,0.99940107358355));
#35621=DIRECTION('',(0.,1.,0.));
#35622=DIRECTION('',(0.0346048279875384,0.,0.99940107358355));
#35623=DIRECTION('center_axis',(0.,1.,0.));
#35624=DIRECTION('ref_axis',(-0.891006524188368,0.,0.453990499739547));
#35625=DIRECTION('center_axis',(0.,1.,0.));
#35626=DIRECTION('ref_axis',(1.,0.,0.));
#35627=DIRECTION('center_axis',(0.484551720341748,0.,-0.874762613692339));
#35628=DIRECTION('ref_axis',(-0.874762613692339,0.,-0.484551720341748));
#35629=DIRECTION('',(0.,-1.,0.));
#35630=DIRECTION('',(-0.874762613692339,0.,-0.484551720341748));
#35631=DIRECTION('',(0.,1.,0.));
#35632=DIRECTION('',(0.874762613692339,0.,0.484551720341748));
#35633=DIRECTION('center_axis',(0.,1.,0.));
#35634=DIRECTION('ref_axis',(0.587785252292473,0.,0.809016994374947));
#35635=DIRECTION('center_axis',(0.,-1.,0.));
#35636=DIRECTION('ref_axis',(1.,0.,0.));
#35637=DIRECTION('',(-0.190519557438267,0.,-0.981683400202696));
#35638=DIRECTION('center_axis',(-0.981683400202696,0.,0.190519557438267));
#35639=DIRECTION('ref_axis',(0.190519557438267,0.,0.981683400202696));
#35640=DIRECTION('',(0.,1.,0.));
#35641=DIRECTION('',(0.190519557438267,0.,0.981683400202696));
#35642=DIRECTION('center_axis',(0.,1.,0.));
#35643=DIRECTION('ref_axis',(-0.809016994374947,0.,0.587785252292473));
#35644=DIRECTION('center_axis',(0.,1.,0.));
#35645=DIRECTION('ref_axis',(1.,0.,0.));
#35646=DIRECTION('center_axis',(0.341743063086706,0.,-0.939793423488437));
#35647=DIRECTION('ref_axis',(-0.939793423488437,0.,-0.341743063086706));
#35648=DIRECTION('',(0.,-1.,0.));
#35649=DIRECTION('',(-0.939793423488437,0.,-0.341743063086706));
#35650=DIRECTION('',(0.,1.,0.));
#35651=DIRECTION('',(0.939793423488437,0.,0.341743063086706));
#35652=DIRECTION('center_axis',(0.,1.,0.));
#35653=DIRECTION('ref_axis',(0.707106781186548,0.,0.707106781186548));
#35654=DIRECTION('center_axis',(0.,-1.,0.));
#35655=DIRECTION('ref_axis',(1.,0.,0.));
#35656=DIRECTION('',(-0.341743063086706,0.,-0.939793423488437));
#35657=DIRECTION('center_axis',(-0.939793423488437,0.,0.341743063086706));
#35658=DIRECTION('ref_axis',(0.341743063086706,0.,0.939793423488437));
#35659=DIRECTION('',(0.,1.,0.));
#35660=DIRECTION('',(0.341743063086706,0.,0.939793423488437));
#35661=DIRECTION('center_axis',(0.,1.,0.));
#35662=DIRECTION('ref_axis',(-0.707106781186548,0.,0.707106781186548));
#35663=DIRECTION('center_axis',(0.,1.,0.));
#35664=DIRECTION('ref_axis',(1.,0.,0.));
#35665=DIRECTION('center_axis',(0.190519557438267,0.,-0.981683400202696));
#35666=DIRECTION('ref_axis',(-0.981683400202696,0.,-0.190519557438267));
#35667=DIRECTION('',(0.,-1.,0.));
#35668=DIRECTION('',(-0.981683400202696,0.,-0.190519557438267));
#35669=DIRECTION('',(0.,1.,0.));
#35670=DIRECTION('',(0.981683400202696,0.,0.190519557438267));
#35671=DIRECTION('center_axis',(0.,1.,0.));
#35672=DIRECTION('ref_axis',(0.809016994374947,0.,0.587785252292473));
#35673=DIRECTION('center_axis',(0.,-1.,0.));
#35674=DIRECTION('ref_axis',(1.,0.,0.));
#35675=DIRECTION('',(-0.484551720341748,0.,-0.874762613692339));
#35676=DIRECTION('center_axis',(-0.874762613692339,0.,0.484551720341748));
#35677=DIRECTION('ref_axis',(0.484551720341748,0.,0.874762613692339));
#35678=DIRECTION('',(0.,1.,0.));
#35679=DIRECTION('',(0.484551720341748,0.,0.874762613692339));
#35680=DIRECTION('center_axis',(0.,1.,0.));
#35681=DIRECTION('ref_axis',(-0.587785252292473,0.,0.809016994374947));
#35682=DIRECTION('center_axis',(0.,1.,0.));
#35683=DIRECTION('ref_axis',(1.,0.,0.));
#35684=DIRECTION('center_axis',(0.0346048279875382,0.,-0.99940107358355));
#35685=DIRECTION('ref_axis',(-0.99940107358355,0.,-0.0346048279875382));
#35686=DIRECTION('',(0.,-1.,0.));
#35687=DIRECTION('',(-0.99940107358355,0.,-0.0346048279875382));
#35688=DIRECTION('',(0.,1.,0.));
#35689=DIRECTION('',(0.99940107358355,0.,0.0346048279875382));
#35690=DIRECTION('center_axis',(0.,1.,0.));
#35691=DIRECTION('ref_axis',(0.891006524188368,0.,0.453990499739547));
#35692=DIRECTION('center_axis',(0.,-1.,0.));
#35693=DIRECTION('ref_axis',(1.,0.,0.));
#35694=DIRECTION('',(-0.615429106107016,0.,-0.788192245176467));
#35695=DIRECTION('center_axis',(-0.788192245176467,0.,0.615429106107016));
#35696=DIRECTION('ref_axis',(0.615429106107016,0.,0.788192245176467));
#35697=DIRECTION('',(0.,1.,0.));
#35698=DIRECTION('',(0.615429106107016,0.,0.788192245176467));
#35699=DIRECTION('center_axis',(0.,1.,0.));
#35700=DIRECTION('ref_axis',(-0.453990499739547,0.,0.891006524188368));
#35701=DIRECTION('center_axis',(0.,1.,0.));
#35702=DIRECTION('ref_axis',(1.,0.,0.));
#35703=DIRECTION('center_axis',(-0.122161987175083,0.,-0.992510175710776));
#35704=DIRECTION('ref_axis',(-0.992510175710776,0.,0.122161987175083));
#35705=DIRECTION('',(0.,-1.,0.));
#35706=DIRECTION('',(-0.992510175710776,0.,0.122161987175083));
#35707=DIRECTION('',(0.,1.,0.));
#35708=DIRECTION('',(0.992510175710776,0.,-0.122161987175083));
#35709=DIRECTION('center_axis',(0.,1.,0.));
#35710=DIRECTION('ref_axis',(0.951056516295154,0.,0.309016994374947));
#35711=DIRECTION('center_axis',(0.,-1.,0.));
#35712=DIRECTION('ref_axis',(1.,0.,0.));
#35713=DIRECTION('',(-0.731152584787826,0.,-0.682213967724262));
#35714=DIRECTION('center_axis',(-0.682213967724262,0.,0.731152584787827));
#35715=DIRECTION('ref_axis',(0.731152584787827,0.,0.682213967724262));
#35716=DIRECTION('',(0.,1.,0.));
#35717=DIRECTION('',(0.731152584787826,0.,0.682213967724262));
#35718=DIRECTION('center_axis',(0.,1.,0.));
#35719=DIRECTION('ref_axis',(-0.309016994374947,0.,0.951056516295154));
#35720=DIRECTION('center_axis',(0.,1.,0.));
#35721=DIRECTION('ref_axis',(1.,0.,0.));
#35722=DIRECTION('center_axis',(-0.275920768781063,0.,-0.961180383359579));
#35723=DIRECTION('ref_axis',(-0.961180383359579,0.,0.275920768781063));
#35724=DIRECTION('',(0.,-1.,0.));
#35725=DIRECTION('',(-0.961180383359579,0.,0.275920768781063));
#35726=DIRECTION('',(0.,1.,0.));
#35727=DIRECTION('center_axis',(0.,1.,0.));
#35728=DIRECTION('ref_axis',(0.987688340595138,0.,0.156434465040231));
#35729=DIRECTION('center_axis',(0.,-1.,0.));
#35730=DIRECTION('ref_axis',(1.,0.,0.));
#35731=DIRECTION('center_axis',(-0.559437318248335,0.,0.828872660274852));
#35732=DIRECTION('ref_axis',(0.828872660274852,0.,0.559437318248335));
#35733=DIRECTION('',(0.828872660274852,0.,0.559437318248335));
#35734=DIRECTION('',(0.,1.,0.));
#35735=DIRECTION('center_axis',(0.,1.,0.));
#35736=DIRECTION('ref_axis',(-0.156434465040231,0.,0.987688340595138));
#35737=DIRECTION('center_axis',(0.,1.,0.));
#35738=DIRECTION('ref_axis',(1.,0.,0.));
#35739=DIRECTION('center_axis',(0.,1.,0.));
#35740=DIRECTION('ref_axis',(1.,0.,0.));
#35741=DIRECTION('center_axis',(0.,-1.,0.));
#35742=DIRECTION('ref_axis',(1.,0.,0.));
#35743=DIRECTION('center_axis',(0.,1.,0.));
#35744=DIRECTION('ref_axis',(0.,0.,1.));
#35745=DIRECTION('center_axis',(0.,1.,0.));
#35746=DIRECTION('ref_axis',(1.,0.,0.));
#35747=DIRECTION('center_axis',(0.,1.,0.));
#35748=DIRECTION('ref_axis',(1.,0.,0.));
#35749=DIRECTION('center_axis',(0.,1.,0.));
#35750=DIRECTION('ref_axis',(1.,0.,0.));
#35751=DIRECTION('',(-0.991409720169891,0.130792839072551,1.21412674044963E-16));
#35752=DIRECTION('center_axis',(0.,-1.,0.));
#35753=DIRECTION('ref_axis',(1.,0.,0.));
#35754=DIRECTION('center_axis',(0.,1.,0.));
#35755=DIRECTION('ref_axis',(0.,0.,1.));
#35756=DIRECTION('center_axis',(0.,-1.,0.));
#35757=DIRECTION('ref_axis',(1.,0.,0.));
#35758=DIRECTION('center_axis',(0.,-1.,0.));
#35759=DIRECTION('ref_axis',(1.,0.,0.));
#35760=DIRECTION('center_axis',(0.,-1.,0.));
#35761=DIRECTION('ref_axis',(1.,0.,0.));
#35762=DIRECTION('',(0.707106781186544,0.707106781186551,8.6595605623549E-17));
#35763=DIRECTION('center_axis',(0.,-1.,0.));
#35764=DIRECTION('ref_axis',(1.,0.,0.));
#35765=DIRECTION('center_axis',(0.,-1.,0.));
#35766=DIRECTION('ref_axis',(1.,0.,0.));
#35767=DIRECTION('',(0.,1.,0.));
#35768=DIRECTION('',(0.,1.,0.));
#35769=DIRECTION('center_axis',(0.,1.,0.));
#35770=DIRECTION('ref_axis',(1.,0.,0.));
#35771=DIRECTION('',(0.707106781186539,-0.707106781186556,-8.65956056235483E-17));
#35772=DIRECTION('center_axis',(0.,-1.,0.));
#35773=DIRECTION('ref_axis',(1.,0.,0.));
#35774=DIRECTION('center_axis',(0.,-1.,0.));
#35775=DIRECTION('ref_axis',(0.,0.,-1.));
#35776=DIRECTION('center_axis',(0.,-1.,0.));
#35777=DIRECTION('ref_axis',(1.,0.,0.));
#35778=DIRECTION('center_axis',(0.,-1.,0.));
#35779=DIRECTION('ref_axis',(1.,0.,0.));
#35780=DIRECTION('center_axis',(0.,-1.,0.));
#35781=DIRECTION('ref_axis',(1.,0.,0.));
#35782=DIRECTION('',(0.,1.,0.));
#35783=DIRECTION('center_axis',(0.,-1.,0.));
#35784=DIRECTION('ref_axis',(0.,0.,-1.));
#35785=DIRECTION('center_axis',(0.,-1.,0.));
#35786=DIRECTION('ref_axis',(1.,0.,0.));
#35787=DIRECTION('center_axis',(0.,-1.,0.));
#35788=DIRECTION('ref_axis',(1.,0.,0.));
#35789=DIRECTION('',(0.,-1.,0.));
#35790=DIRECTION('axis',(0.,0.,1.));
#35791=DIRECTION('refdir',(1.,0.,0.));
#35792=DIRECTION('',(-1.,0.,0.));
#35793=DIRECTION('',(-1.,0.,0.));
#35794=DIRECTION('',(-1.,0.,0.));
#35795=DIRECTION('',(-1.,0.,0.));
#35796=DIRECTION('',(-1.,0.,0.));
#35797=DIRECTION('',(-1.,0.,0.));
#35798=DIRECTION('',(-1.,0.,0.));
#35799=DIRECTION('',(-1.,0.,0.));
#35800=DIRECTION('',(-1.,0.,0.));
#35801=DIRECTION('',(-1.,0.,0.));
#35802=DIRECTION('',(-1.,0.,0.));
#35803=DIRECTION('',(-1.,0.,0.));
#35804=DIRECTION('',(-1.,0.,0.));
#35805=DIRECTION('',(-1.,0.,0.));
#35806=DIRECTION('',(-1.,0.,0.));
#35807=DIRECTION('',(-1.,0.,0.));
#35808=DIRECTION('',(-1.,0.,0.));
#35809=DIRECTION('',(-1.,0.,0.));
#35810=DIRECTION('',(-1.,0.,0.));
#35811=DIRECTION('',(-1.,0.,0.));
#35812=DIRECTION('center_axis',(1.,0.,0.));
#35813=DIRECTION('ref_axis',(0.,0.,-1.));
#35814=DIRECTION('center_axis',(0.,-0.570372452855479,-0.821386185069864));
#35815=DIRECTION('ref_axis',(0.,-0.821386185069864,0.570372452855479));
#35816=DIRECTION('',(0.,-0.821386185069864,0.570372452855479));
#35817=DIRECTION('',(-1.,0.,0.));
#35818=DIRECTION('',(0.,-0.821386185069864,0.570372452855479));
#35819=DIRECTION('',(-1.,0.,0.));
#35820=DIRECTION('center_axis',(0.,0.,1.));
#35821=DIRECTION('ref_axis',(0.,1.,0.));
#35822=DIRECTION('',(0.,1.,0.));
#35823=DIRECTION('',(-1.,0.,0.));
#35824=DIRECTION('',(0.,1.,0.));
#35825=DIRECTION('center_axis',(0.,1.,0.));
#35826=DIRECTION('ref_axis',(0.,0.,-1.));
#35827=DIRECTION('',(0.,0.,-1.));
#35828=DIRECTION('',(0.,0.,-1.));
#35829=DIRECTION('center_axis',(0.,0.,-1.));
#35830=DIRECTION('ref_axis',(0.,-1.,0.));
#35831=DIRECTION('',(0.,-1.,0.));
#35832=DIRECTION('',(-1.,0.,0.));
#35833=DIRECTION('',(0.,-1.,0.));
#35834=DIRECTION('',(-1.,0.,0.));
#35835=DIRECTION('center_axis',(0.,-1.,0.));
#35836=DIRECTION('ref_axis',(0.,0.,1.));
#35837=DIRECTION('',(0.,0.,1.));
#35838=DIRECTION('',(-1.,0.,0.));
#35839=DIRECTION('',(0.,0.,1.));
#35840=DIRECTION('center_axis',(0.,0.,-1.));
#35841=DIRECTION('ref_axis',(0.,-1.,0.));
#35842=DIRECTION('',(0.,-1.,0.));
#35843=DIRECTION('',(-1.,0.,0.));
#35844=DIRECTION('',(0.,-1.,0.));
#35845=DIRECTION('center_axis',(0.,1.,0.));
#35846=DIRECTION('ref_axis',(0.,0.,-1.));
#35847=DIRECTION('',(0.,0.,-1.));
#35848=DIRECTION('',(-1.,0.,0.));
#35849=DIRECTION('',(0.,0.,-1.));
#35850=DIRECTION('center_axis',(0.,0.,-1.));
#35851=DIRECTION('ref_axis',(0.,-1.,0.));
#35852=DIRECTION('',(0.,-1.,0.));
#35853=DIRECTION('',(-1.,0.,0.));
#35854=DIRECTION('',(0.,-1.,0.));
#35855=DIRECTION('center_axis',(0.,1.,0.));
#35856=DIRECTION('ref_axis',(0.,0.,-1.));
#35857=DIRECTION('',(0.,0.,-1.));
#35858=DIRECTION('',(-1.,0.,0.));
#35859=DIRECTION('',(0.,0.,-1.));
#35860=DIRECTION('center_axis',(0.,0.575770455267793,0.817611388644213));
#35861=DIRECTION('ref_axis',(0.,0.817611388644213,-0.575770455267793));
#35862=DIRECTION('',(0.,0.817611388644214,-0.575770455267792));
#35863=DIRECTION('',(-1.,0.,0.));
#35864=DIRECTION('',(0.,0.817611388644214,-0.575770455267792));
#35865=DIRECTION('center_axis',(0.,0.,1.));
#35866=DIRECTION('ref_axis',(0.,1.,0.));
#35867=DIRECTION('',(0.,1.,0.));
#35868=DIRECTION('',(-1.,0.,0.));
#35869=DIRECTION('',(0.,1.,0.));
#35870=DIRECTION('center_axis',(0.,-1.,0.));
#35871=DIRECTION('ref_axis',(0.,0.,1.));
#35872=DIRECTION('',(0.,0.,1.));
#35873=DIRECTION('',(-1.,0.,0.));
#35874=DIRECTION('',(0.,0.,1.));
#35875=DIRECTION('center_axis',(0.,0.,1.));
#35876=DIRECTION('ref_axis',(0.,1.,0.));
#35877=DIRECTION('',(0.,1.,0.));
#35878=DIRECTION('',(-1.,0.,0.));
#35879=DIRECTION('',(0.,1.,0.));
#35880=DIRECTION('center_axis',(0.,-1.,0.));
#35881=DIRECTION('ref_axis',(0.,0.,1.));
#35882=DIRECTION('',(0.,0.,1.));
#35883=DIRECTION('',(0.,0.,1.));
#35884=DIRECTION('center_axis',(-1.,0.,0.));
#35885=DIRECTION('ref_axis',(0.,0.,1.));
#35886=DIRECTION('center_axis',(1.,0.,0.));
#35887=DIRECTION('ref_axis',(0.,0.,-1.));
#35888=DIRECTION('center_axis',(1.,0.,0.));
#35889=DIRECTION('ref_axis',(0.,0.,-1.));
#35890=DIRECTION('',(-1.,0.,0.));
#35891=DIRECTION('',(-1.,0.,0.));
#35892=DIRECTION('',(-1.,0.,0.));
#35893=DIRECTION('',(-1.,0.,0.));
#35894=DIRECTION('',(-1.,0.,0.));
#35895=DIRECTION('',(-1.,0.,0.));
#35896=DIRECTION('',(-1.,0.,0.));
#35897=DIRECTION('',(-1.,0.,0.));
#35898=DIRECTION('',(-1.,0.,0.));
#35899=DIRECTION('',(-1.,0.,0.));
#35900=DIRECTION('',(-1.,0.,0.));
#35901=DIRECTION('',(-1.,0.,0.));
#35902=DIRECTION('',(-1.,0.,0.));
#35903=DIRECTION('',(-1.,0.,0.));
#35904=DIRECTION('',(-1.,0.,0.));
#35905=DIRECTION('',(-1.,0.,0.));
#35906=DIRECTION('',(-1.,0.,0.));
#35907=DIRECTION('',(-1.,0.,0.));
#35908=DIRECTION('',(-1.,0.,0.));
#35909=DIRECTION('',(-1.,0.,0.));
#35910=DIRECTION('center_axis',(1.,0.,0.));
#35911=DIRECTION('ref_axis',(0.,0.,-1.));
#35912=DIRECTION('',(-1.,0.,0.));
#35913=DIRECTION('',(-1.,0.,0.));
#35914=DIRECTION('',(-1.,0.,0.));
#35915=DIRECTION('',(-1.,0.,0.));
#35916=DIRECTION('',(-1.,0.,0.));
#35917=DIRECTION('',(-1.,0.,0.));
#35918=DIRECTION('',(-1.,0.,0.));
#35919=DIRECTION('',(-1.,0.,0.));
#35920=DIRECTION('',(-1.,0.,0.));
#35921=DIRECTION('',(-1.,0.,0.));
#35922=DIRECTION('',(-1.,0.,0.));
#35923=DIRECTION('',(-1.,0.,0.));
#35924=DIRECTION('',(-1.,0.,0.));
#35925=DIRECTION('center_axis',(0.,-0.984562439147349,0.175033720808942));
#35926=DIRECTION('ref_axis',(0.,0.175033720808942,0.984562439147349));
#35927=DIRECTION('',(0.,0.175033720808942,0.984562439147349));
#35928=DIRECTION('',(-1.,0.,0.));
#35929=DIRECTION('',(0.,0.175033720808942,0.984562439147349));
#35930=DIRECTION('',(-1.,0.,0.));
#35931=DIRECTION('',(-1.,0.,0.));
#35932=DIRECTION('',(-1.,0.,0.));
#35933=DIRECTION('',(-1.,0.,0.));
#35934=DIRECTION('',(-1.,0.,0.));
#35935=DIRECTION('',(-1.,0.,0.));
#35936=DIRECTION('',(-1.,0.,0.));
#35937=DIRECTION('center_axis',(0.,0.125580335944265,0.992083453759877));
#35938=DIRECTION('ref_axis',(0.,0.992083453759877,-0.125580335944265));
#35939=DIRECTION('',(0.,0.992083453759877,-0.125580335944265));
#35940=DIRECTION('',(-1.,0.,0.));
#35941=DIRECTION('',(0.,0.992083453759877,-0.125580335944265));
#35942=DIRECTION('',(-1.,0.,0.));
#35943=DIRECTION('',(-1.,0.,0.));
#35944=DIRECTION('',(-1.,0.,0.));
#35945=DIRECTION('',(-1.,0.,0.));
#35946=DIRECTION('',(-1.,0.,0.));
#35947=DIRECTION('',(-1.,0.,0.));
#35948=DIRECTION('',(-1.,0.,0.));
#35949=DIRECTION('center_axis',(0.,0.991227812035547,0.132164384942471));
#35950=DIRECTION('ref_axis',(0.,0.132164384942471,-0.991227812035547));
#35951=DIRECTION('',(0.,0.132164384942471,-0.991227812035547));
#35952=DIRECTION('',(-1.,0.,0.));
#35953=DIRECTION('',(0.,0.132164384942471,-0.991227812035547));
#35954=DIRECTION('center_axis',(1.,0.,0.));
#35955=DIRECTION('ref_axis',(0.,0.,-1.));
#35956=DIRECTION('center_axis',(1.,0.,0.));
#35957=DIRECTION('ref_axis',(0.,0.,-1.));
#35958=DIRECTION('',(-1.,0.,0.));
#35959=DIRECTION('',(-1.,0.,0.));
#35960=DIRECTION('',(-1.,0.,0.));
#35961=DIRECTION('',(-1.,0.,0.));
#35962=DIRECTION('',(-1.,0.,0.));
#35963=DIRECTION('',(-1.,0.,0.));
#35964=DIRECTION('',(-1.,0.,0.));
#35965=DIRECTION('',(-1.,0.,0.));
#35966=DIRECTION('',(-1.,0.,0.));
#35967=DIRECTION('',(-1.,0.,0.));
#35968=DIRECTION('',(-1.,0.,0.));
#35969=DIRECTION('',(-1.,0.,0.));
#35970=DIRECTION('',(-1.,0.,0.));
#35971=DIRECTION('',(-1.,0.,0.));
#35972=DIRECTION('',(-1.,0.,0.));
#35973=DIRECTION('',(-1.,0.,0.));
#35974=DIRECTION('',(-1.,0.,0.));
#35975=DIRECTION('',(-1.,0.,0.));
#35976=DIRECTION('',(-1.,0.,0.));
#35977=DIRECTION('',(-1.,0.,0.));
#35978=DIRECTION('center_axis',(1.,0.,0.));
#35979=DIRECTION('ref_axis',(0.,0.,-1.));
#35980=DIRECTION('',(-1.,0.,0.));
#35981=DIRECTION('',(-1.,0.,0.));
#35982=DIRECTION('',(-1.,0.,0.));
#35983=DIRECTION('',(-1.,0.,0.));
#35984=DIRECTION('',(-1.,0.,0.));
#35985=DIRECTION('',(-1.,0.,0.));
#35986=DIRECTION('',(-1.,0.,0.));
#35987=DIRECTION('',(-1.,0.,0.));
#35988=DIRECTION('',(-1.,0.,0.));
#35989=DIRECTION('',(-1.,0.,0.));
#35990=DIRECTION('center_axis',(0.,-0.994767480968245,0.10216486092631));
#35991=DIRECTION('ref_axis',(0.,0.10216486092631,0.994767480968245));
#35992=DIRECTION('',(0.,0.10216486092631,0.994767480968245));
#35993=DIRECTION('',(-1.,0.,0.));
#35994=DIRECTION('',(0.,0.10216486092631,0.994767480968245));
#35995=DIRECTION('',(-1.,0.,0.));
#35996=DIRECTION('',(-1.,0.,0.));
#35997=DIRECTION('',(-1.,0.,0.));
#35998=DIRECTION('',(-1.,0.,0.));
#35999=DIRECTION('',(-1.,0.,0.));
#36000=DIRECTION('',(-1.,0.,0.));
#36001=DIRECTION('',(-1.,0.,0.));
#36002=DIRECTION('',(-1.,0.,0.));
#36003=DIRECTION('',(-1.,0.,0.));
#36004=DIRECTION('center_axis',(0.,-1.,0.));
#36005=DIRECTION('ref_axis',(0.,0.,1.));
#36006=DIRECTION('',(0.,0.,1.));
#36007=DIRECTION('',(-1.,0.,0.));
#36008=DIRECTION('',(0.,0.,1.));
#36009=DIRECTION('center_axis',(0.,0.,-1.));
#36010=DIRECTION('ref_axis',(0.,-1.,0.));
#36011=DIRECTION('',(0.,-1.,0.));
#36012=DIRECTION('',(-1.,0.,0.));
#36013=DIRECTION('',(0.,-1.,0.));
#36014=DIRECTION('center_axis',(0.,1.,0.));
#36015=DIRECTION('ref_axis',(0.,0.,-1.));
#36016=DIRECTION('',(0.,0.,-1.));
#36017=DIRECTION('',(0.,0.,-1.));
#36018=DIRECTION('center_axis',(1.,0.,0.));
#36019=DIRECTION('ref_axis',(0.,0.,-1.));
#36020=DIRECTION('center_axis',(1.,0.,0.));
#36021=DIRECTION('ref_axis',(0.,0.,-1.));
#36022=DIRECTION('',(-1.,0.,0.));
#36023=DIRECTION('',(-1.,0.,0.));
#36024=DIRECTION('',(-1.,0.,0.));
#36025=DIRECTION('',(-1.,0.,0.));
#36026=DIRECTION('',(-1.,0.,0.));
#36027=DIRECTION('',(-1.,0.,0.));
#36028=DIRECTION('',(-1.,0.,0.));
#36029=DIRECTION('',(-1.,0.,0.));
#36030=DIRECTION('',(-1.,0.,0.));
#36031=DIRECTION('',(-1.,0.,0.));
#36032=DIRECTION('',(-1.,0.,0.));
#36033=DIRECTION('',(-1.,0.,0.));
#36034=DIRECTION('',(-1.,0.,0.));
#36035=DIRECTION('',(-1.,0.,0.));
#36036=DIRECTION('',(-1.,0.,0.));
#36037=DIRECTION('',(-1.,0.,0.));
#36038=DIRECTION('',(-1.,0.,0.));
#36039=DIRECTION('',(-1.,0.,0.));
#36040=DIRECTION('',(-1.,0.,0.));
#36041=DIRECTION('',(-1.,0.,0.));
#36042=DIRECTION('center_axis',(1.,0.,0.));
#36043=DIRECTION('ref_axis',(0.,0.,-1.));
#36044=DIRECTION('center_axis',(0.,1.,0.));
#36045=DIRECTION('ref_axis',(0.,0.,-1.));
#36046=DIRECTION('',(0.,0.,-1.));
#36047=DIRECTION('',(-1.,0.,0.));
#36048=DIRECTION('',(0.,0.,-1.));
#36049=DIRECTION('',(-1.,0.,0.));
#36050=DIRECTION('',(-1.,0.,0.));
#36051=DIRECTION('',(-1.,0.,0.));
#36052=DIRECTION('center_axis',(0.,0.,1.));
#36053=DIRECTION('ref_axis',(0.,1.,0.));
#36054=DIRECTION('',(0.,1.,0.));
#36055=DIRECTION('',(-1.,0.,0.));
#36056=DIRECTION('',(0.,1.,0.));
#36057=DIRECTION('',(-1.,0.,0.));
#36058=DIRECTION('',(-1.,0.,0.));
#36059=DIRECTION('center_axis',(0.,0.,1.));
#36060=DIRECTION('ref_axis',(0.,1.,0.));
#36061=DIRECTION('',(0.,1.,0.));
#36062=DIRECTION('',(-1.,0.,0.));
#36063=DIRECTION('',(0.,1.,0.));
#36064=DIRECTION('center_axis',(0.,-1.,0.));
#36065=DIRECTION('ref_axis',(0.,0.,1.));
#36066=DIRECTION('',(0.,0.,1.));
#36067=DIRECTION('',(-1.,0.,0.));
#36068=DIRECTION('',(0.,0.,1.));
#36069=DIRECTION('center_axis',(0.,0.,-1.));
#36070=DIRECTION('ref_axis',(0.,-1.,0.));
#36071=DIRECTION('',(0.,-1.,0.));
#36072=DIRECTION('',(0.,-1.,0.));
#36073=DIRECTION('center_axis',(1.,0.,0.));
#36074=DIRECTION('ref_axis',(0.,0.,-1.));
#36075=DIRECTION('center_axis',(1.,0.,0.));
#36076=DIRECTION('ref_axis',(0.,0.,-1.));
#36077=DIRECTION('',(-1.,0.,0.));
#36078=DIRECTION('',(-1.,0.,0.));
#36079=DIRECTION('',(-1.,0.,0.));
#36080=DIRECTION('',(-1.,0.,0.));
#36081=DIRECTION('',(-1.,0.,0.));
#36082=DIRECTION('',(-1.,0.,0.));
#36083=DIRECTION('',(-1.,0.,0.));
#36084=DIRECTION('',(-1.,0.,0.));
#36085=DIRECTION('',(-1.,0.,0.));
#36086=DIRECTION('',(-1.,0.,0.));
#36087=DIRECTION('',(-1.,0.,0.));
#36088=DIRECTION('',(-1.,0.,0.));
#36089=DIRECTION('',(-1.,0.,0.));
#36090=DIRECTION('',(-1.,0.,0.));
#36091=DIRECTION('',(-1.,0.,0.));
#36092=DIRECTION('',(-1.,0.,0.));
#36093=DIRECTION('',(-1.,0.,0.));
#36094=DIRECTION('',(-1.,0.,0.));
#36095=DIRECTION('',(-1.,0.,0.));
#36096=DIRECTION('',(-1.,0.,0.));
#36097=DIRECTION('center_axis',(1.,0.,0.));
#36098=DIRECTION('ref_axis',(0.,0.,-1.));
#36099=DIRECTION('center_axis',(1.,0.,0.));
#36100=DIRECTION('ref_axis',(0.,0.,-1.));
#36101=DIRECTION('',(-1.,0.,0.));
#36102=DIRECTION('',(-1.,0.,0.));
#36103=DIRECTION('',(-1.,0.,0.));
#36104=DIRECTION('',(-1.,0.,0.));
#36105=DIRECTION('',(-1.,0.,0.));
#36106=DIRECTION('',(-1.,0.,0.));
#36107=DIRECTION('',(-1.,0.,0.));
#36108=DIRECTION('',(-1.,0.,0.));
#36109=DIRECTION('',(-1.,0.,0.));
#36110=DIRECTION('',(-1.,0.,0.));
#36111=DIRECTION('',(-1.,0.,0.));
#36112=DIRECTION('',(-1.,0.,0.));
#36113=DIRECTION('',(-1.,0.,0.));
#36114=DIRECTION('',(-1.,0.,0.));
#36115=DIRECTION('',(-1.,0.,0.));
#36116=DIRECTION('',(-1.,0.,0.));
#36117=DIRECTION('',(-1.,0.,0.));
#36118=DIRECTION('',(-1.,0.,0.));
#36119=DIRECTION('',(-1.,0.,0.));
#36120=DIRECTION('',(-1.,0.,0.));
#36121=DIRECTION('center_axis',(1.,0.,0.));
#36122=DIRECTION('ref_axis',(0.,0.,-1.));
#36123=DIRECTION('center_axis',(0.,1.,0.));
#36124=DIRECTION('ref_axis',(0.,0.,-1.));
#36125=DIRECTION('',(0.,0.,-1.));
#36126=DIRECTION('',(-1.,0.,0.));
#36127=DIRECTION('',(0.,0.,-1.));
#36128=DIRECTION('',(-1.,0.,0.));
#36129=DIRECTION('',(-1.,0.,0.));
#36130=DIRECTION('',(-1.,0.,0.));
#36131=DIRECTION('center_axis',(0.,0.,1.));
#36132=DIRECTION('ref_axis',(0.,1.,0.));
#36133=DIRECTION('',(0.,1.,0.));
#36134=DIRECTION('',(-1.,0.,0.));
#36135=DIRECTION('',(0.,1.,0.));
#36136=DIRECTION('',(-1.,0.,0.));
#36137=DIRECTION('',(-1.,0.,0.));
#36138=DIRECTION('center_axis',(0.,0.,1.));
#36139=DIRECTION('ref_axis',(0.,1.,0.));
#36140=DIRECTION('',(0.,1.,0.));
#36141=DIRECTION('',(-1.,0.,0.));
#36142=DIRECTION('',(0.,1.,0.));
#36143=DIRECTION('center_axis',(0.,-1.,0.));
#36144=DIRECTION('ref_axis',(0.,0.,1.));
#36145=DIRECTION('',(0.,0.,1.));
#36146=DIRECTION('',(-1.,0.,0.));
#36147=DIRECTION('',(0.,0.,1.));
#36148=DIRECTION('center_axis',(0.,0.,-1.));
#36149=DIRECTION('ref_axis',(0.,-1.,0.));
#36150=DIRECTION('',(0.,-1.,0.));
#36151=DIRECTION('',(0.,-1.,0.));
#36152=DIRECTION('center_axis',(1.,0.,0.));
#36153=DIRECTION('ref_axis',(0.,0.,-1.));
#36154=DIRECTION('center_axis',(1.,0.,0.));
#36155=DIRECTION('ref_axis',(0.,0.,-1.));
#36156=DIRECTION('',(-1.,0.,0.));
#36157=DIRECTION('',(-1.,0.,0.));
#36158=DIRECTION('',(-1.,0.,0.));
#36159=DIRECTION('',(-1.,0.,0.));
#36160=DIRECTION('',(-1.,0.,0.));
#36161=DIRECTION('',(-1.,0.,0.));
#36162=DIRECTION('',(-1.,0.,0.));
#36163=DIRECTION('',(-1.,0.,0.));
#36164=DIRECTION('',(-1.,0.,0.));
#36165=DIRECTION('',(-1.,0.,0.));
#36166=DIRECTION('',(-1.,0.,0.));
#36167=DIRECTION('',(-1.,0.,0.));
#36168=DIRECTION('',(-1.,0.,0.));
#36169=DIRECTION('',(-1.,0.,0.));
#36170=DIRECTION('',(-1.,0.,0.));
#36171=DIRECTION('',(-1.,0.,0.));
#36172=DIRECTION('',(-1.,0.,0.));
#36173=DIRECTION('',(-1.,0.,0.));
#36174=DIRECTION('',(-1.,0.,0.));
#36175=DIRECTION('',(-1.,0.,0.));
#36176=DIRECTION('center_axis',(1.,0.,0.));
#36177=DIRECTION('ref_axis',(0.,0.,-1.));
#36178=DIRECTION('',(-1.,0.,0.));
#36179=DIRECTION('',(-1.,0.,0.));
#36180=DIRECTION('',(-1.,0.,0.));
#36181=DIRECTION('',(-1.,0.,0.));
#36182=DIRECTION('',(-1.,0.,0.));
#36183=DIRECTION('',(-1.,0.,0.));
#36184=DIRECTION('',(-1.,0.,0.));
#36185=DIRECTION('',(-1.,0.,0.));
#36186=DIRECTION('',(-1.,0.,0.));
#36187=DIRECTION('',(-1.,0.,0.));
#36188=DIRECTION('center_axis',(0.,-0.994767480968245,0.10216486092631));
#36189=DIRECTION('ref_axis',(0.,0.10216486092631,0.994767480968245));
#36190=DIRECTION('',(0.,0.10216486092631,0.994767480968245));
#36191=DIRECTION('',(-1.,0.,0.));
#36192=DIRECTION('',(0.,0.10216486092631,0.994767480968245));
#36193=DIRECTION('',(-1.,0.,0.));
#36194=DIRECTION('',(-1.,0.,0.));
#36195=DIRECTION('',(-1.,0.,0.));
#36196=DIRECTION('',(-1.,0.,0.));
#36197=DIRECTION('',(-1.,0.,0.));
#36198=DIRECTION('',(-1.,0.,0.));
#36199=DIRECTION('',(-1.,0.,0.));
#36200=DIRECTION('',(-1.,0.,0.));
#36201=DIRECTION('',(-1.,0.,0.));
#36202=DIRECTION('center_axis',(0.,-1.,0.));
#36203=DIRECTION('ref_axis',(0.,0.,1.));
#36204=DIRECTION('',(0.,0.,1.));
#36205=DIRECTION('',(-1.,0.,0.));
#36206=DIRECTION('',(0.,0.,1.));
#36207=DIRECTION('center_axis',(0.,0.,-1.));
#36208=DIRECTION('ref_axis',(0.,-1.,0.));
#36209=DIRECTION('',(0.,-1.,0.));
#36210=DIRECTION('',(-1.,0.,0.));
#36211=DIRECTION('',(0.,-1.,0.));
#36212=DIRECTION('center_axis',(0.,1.,0.));
#36213=DIRECTION('ref_axis',(0.,0.,-1.));
#36214=DIRECTION('',(0.,0.,-1.));
#36215=DIRECTION('',(0.,0.,-1.));
#36216=DIRECTION('center_axis',(1.,0.,0.));
#36217=DIRECTION('ref_axis',(0.,0.,-1.));
#36218=DIRECTION('center_axis',(1.,0.,0.));
#36219=DIRECTION('ref_axis',(0.,0.,-1.));
#36220=DIRECTION('',(-1.,0.,0.));
#36221=DIRECTION('',(-1.,0.,0.));
#36222=DIRECTION('',(-1.,0.,0.));
#36223=DIRECTION('',(-1.,0.,0.));
#36224=DIRECTION('',(-1.,0.,0.));
#36225=DIRECTION('',(-1.,0.,0.));
#36226=DIRECTION('',(-1.,0.,0.));
#36227=DIRECTION('',(-1.,0.,0.));
#36228=DIRECTION('',(-1.,0.,0.));
#36229=DIRECTION('',(-1.,0.,0.));
#36230=DIRECTION('',(-1.,0.,0.));
#36231=DIRECTION('',(-1.,0.,0.));
#36232=DIRECTION('',(-1.,0.,0.));
#36233=DIRECTION('',(-1.,0.,0.));
#36234=DIRECTION('',(-1.,0.,0.));
#36235=DIRECTION('',(-1.,0.,0.));
#36236=DIRECTION('',(-1.,0.,0.));
#36237=DIRECTION('',(-1.,0.,0.));
#36238=DIRECTION('',(-1.,0.,0.));
#36239=DIRECTION('',(-1.,0.,0.));
#36240=DIRECTION('center_axis',(1.,0.,0.));
#36241=DIRECTION('ref_axis',(0.,0.,-1.));
#36242=DIRECTION('',(-1.,0.,0.));
#36243=DIRECTION('',(-1.,0.,0.));
#36244=DIRECTION('',(-1.,0.,0.));
#36245=DIRECTION('',(-1.,0.,0.));
#36246=DIRECTION('',(-1.,0.,0.));
#36247=DIRECTION('',(-1.,0.,0.));
#36248=DIRECTION('',(-1.,0.,0.));
#36249=DIRECTION('',(-1.,0.,0.));
#36250=DIRECTION('',(-1.,0.,0.));
#36251=DIRECTION('',(-1.,0.,0.));
#36252=DIRECTION('',(-1.,0.,0.));
#36253=DIRECTION('',(-1.,0.,0.));
#36254=DIRECTION('',(-1.,0.,0.));
#36255=DIRECTION('center_axis',(0.,-0.984562439147349,0.175033720808942));
#36256=DIRECTION('ref_axis',(0.,0.175033720808942,0.984562439147349));
#36257=DIRECTION('',(0.,0.175033720808942,0.984562439147349));
#36258=DIRECTION('',(-1.,0.,0.));
#36259=DIRECTION('',(0.,0.175033720808942,0.984562439147349));
#36260=DIRECTION('',(-1.,0.,0.));
#36261=DIRECTION('',(-1.,0.,0.));
#36262=DIRECTION('',(-1.,0.,0.));
#36263=DIRECTION('',(-1.,0.,0.));
#36264=DIRECTION('',(-1.,0.,0.));
#36265=DIRECTION('',(-1.,0.,0.));
#36266=DIRECTION('',(-1.,0.,0.));
#36267=DIRECTION('center_axis',(0.,0.125580335944265,0.992083453759877));
#36268=DIRECTION('ref_axis',(0.,0.992083453759877,-0.125580335944265));
#36269=DIRECTION('',(0.,0.992083453759877,-0.125580335944265));
#36270=DIRECTION('',(-1.,0.,0.));
#36271=DIRECTION('',(0.,0.992083453759877,-0.125580335944265));
#36272=DIRECTION('',(-1.,0.,0.));
#36273=DIRECTION('',(-1.,0.,0.));
#36274=DIRECTION('',(-1.,0.,0.));
#36275=DIRECTION('',(-1.,0.,0.));
#36276=DIRECTION('',(-1.,0.,0.));
#36277=DIRECTION('',(-1.,0.,0.));
#36278=DIRECTION('',(-1.,0.,0.));
#36279=DIRECTION('center_axis',(0.,0.991227812035547,0.132164384942471));
#36280=DIRECTION('ref_axis',(0.,0.132164384942471,-0.991227812035547));
#36281=DIRECTION('',(0.,0.132164384942471,-0.991227812035547));
#36282=DIRECTION('',(-1.,0.,0.));
#36283=DIRECTION('',(0.,0.132164384942471,-0.991227812035547));
#36284=DIRECTION('center_axis',(1.,0.,0.));
#36285=DIRECTION('ref_axis',(0.,0.,-1.));
#36286=DIRECTION('center_axis',(1.,0.,0.));
#36287=DIRECTION('ref_axis',(0.,0.,-1.));
#36288=DIRECTION('',(-1.,0.,0.));
#36289=DIRECTION('',(-1.,0.,0.));
#36290=DIRECTION('',(-1.,0.,0.));
#36291=DIRECTION('',(-1.,0.,0.));
#36292=DIRECTION('',(-1.,0.,0.));
#36293=DIRECTION('',(-1.,0.,0.));
#36294=DIRECTION('',(-1.,0.,0.));
#36295=DIRECTION('',(-1.,0.,0.));
#36296=DIRECTION('',(-1.,0.,0.));
#36297=DIRECTION('',(-1.,0.,0.));
#36298=DIRECTION('',(-1.,0.,0.));
#36299=DIRECTION('',(-1.,0.,0.));
#36300=DIRECTION('',(-1.,0.,0.));
#36301=DIRECTION('',(-1.,0.,0.));
#36302=DIRECTION('',(-1.,0.,0.));
#36303=DIRECTION('',(-1.,0.,0.));
#36304=DIRECTION('',(-1.,0.,0.));
#36305=DIRECTION('',(-1.,0.,0.));
#36306=DIRECTION('',(-1.,0.,0.));
#36307=DIRECTION('',(-1.,0.,0.));
#36308=DIRECTION('center_axis',(1.,0.,0.));
#36309=DIRECTION('ref_axis',(0.,0.,-1.));
#36310=DIRECTION('center_axis',(0.,-0.570372452855479,-0.821386185069864));
#36311=DIRECTION('ref_axis',(0.,-0.821386185069864,0.570372452855479));
#36312=DIRECTION('',(0.,-0.821386185069864,0.570372452855479));
#36313=DIRECTION('',(-1.,0.,0.));
#36314=DIRECTION('',(0.,-0.821386185069864,0.570372452855479));
#36315=DIRECTION('',(-1.,0.,0.));
#36316=DIRECTION('center_axis',(0.,0.,1.));
#36317=DIRECTION('ref_axis',(0.,1.,0.));
#36318=DIRECTION('',(0.,1.,0.));
#36319=DIRECTION('',(-1.,0.,0.));
#36320=DIRECTION('',(0.,1.,0.));
#36321=DIRECTION('center_axis',(0.,1.,0.));
#36322=DIRECTION('ref_axis',(0.,0.,-1.));
#36323=DIRECTION('',(0.,0.,-1.));
#36324=DIRECTION('',(0.,0.,-1.));
#36325=DIRECTION('center_axis',(0.,0.,-1.));
#36326=DIRECTION('ref_axis',(0.,-1.,0.));
#36327=DIRECTION('',(0.,-1.,0.));
#36328=DIRECTION('',(-1.,0.,0.));
#36329=DIRECTION('',(0.,-1.,0.));
#36330=DIRECTION('',(-1.,0.,0.));
#36331=DIRECTION('center_axis',(0.,-1.,0.));
#36332=DIRECTION('ref_axis',(0.,0.,1.));
#36333=DIRECTION('',(0.,0.,1.));
#36334=DIRECTION('',(-1.,0.,0.));
#36335=DIRECTION('',(0.,0.,1.));
#36336=DIRECTION('center_axis',(0.,0.,-1.));
#36337=DIRECTION('ref_axis',(0.,-1.,0.));
#36338=DIRECTION('',(0.,-1.,0.));
#36339=DIRECTION('',(-1.,0.,0.));
#36340=DIRECTION('',(0.,-1.,0.));
#36341=DIRECTION('center_axis',(0.,1.,0.));
#36342=DIRECTION('ref_axis',(0.,0.,-1.));
#36343=DIRECTION('',(0.,0.,-1.));
#36344=DIRECTION('',(-1.,0.,0.));
#36345=DIRECTION('',(0.,0.,-1.));
#36346=DIRECTION('center_axis',(0.,0.,-1.));
#36347=DIRECTION('ref_axis',(0.,-1.,0.));
#36348=DIRECTION('',(0.,-1.,0.));
#36349=DIRECTION('',(-1.,0.,0.));
#36350=DIRECTION('',(0.,-1.,0.));
#36351=DIRECTION('center_axis',(0.,1.,0.));
#36352=DIRECTION('ref_axis',(0.,0.,-1.));
#36353=DIRECTION('',(0.,0.,-1.));
#36354=DIRECTION('',(-1.,0.,0.));
#36355=DIRECTION('',(0.,0.,-1.));
#36356=DIRECTION('center_axis',(0.,0.575770455267793,0.817611388644213));
#36357=DIRECTION('ref_axis',(0.,0.817611388644213,-0.575770455267793));
#36358=DIRECTION('',(0.,0.817611388644214,-0.575770455267792));
#36359=DIRECTION('',(-1.,0.,0.));
#36360=DIRECTION('',(0.,0.817611388644214,-0.575770455267792));
#36361=DIRECTION('center_axis',(0.,0.,1.));
#36362=DIRECTION('ref_axis',(0.,1.,0.));
#36363=DIRECTION('',(0.,1.,0.));
#36364=DIRECTION('',(-1.,0.,0.));
#36365=DIRECTION('',(0.,1.,0.));
#36366=DIRECTION('center_axis',(0.,-1.,0.));
#36367=DIRECTION('ref_axis',(0.,0.,1.));
#36368=DIRECTION('',(0.,0.,1.));
#36369=DIRECTION('',(-1.,0.,0.));
#36370=DIRECTION('',(0.,0.,1.));
#36371=DIRECTION('center_axis',(0.,0.,1.));
#36372=DIRECTION('ref_axis',(0.,1.,0.));
#36373=DIRECTION('',(0.,1.,0.));
#36374=DIRECTION('',(-1.,0.,0.));
#36375=DIRECTION('',(0.,1.,0.));
#36376=DIRECTION('center_axis',(0.,-1.,0.));
#36377=DIRECTION('ref_axis',(0.,0.,1.));
#36378=DIRECTION('',(0.,0.,1.));
#36379=DIRECTION('',(0.,0.,1.));
#36380=DIRECTION('center_axis',(-1.,0.,0.));
#36381=DIRECTION('ref_axis',(0.,0.,1.));
#36382=DIRECTION('center_axis',(1.,0.,0.));
#36383=DIRECTION('ref_axis',(0.,0.,-1.));
#36384=DIRECTION('center_axis',(1.,0.,0.));
#36385=DIRECTION('ref_axis',(0.,0.,-1.));
#36386=DIRECTION('center_axis',(0.,0.,-1.));
#36387=DIRECTION('ref_axis',(0.,-1.,0.));
#36388=DIRECTION('',(0.,-1.,0.));
#36389=DIRECTION('',(-1.,0.,0.));
#36390=DIRECTION('',(0.,-1.,0.));
#36391=DIRECTION('',(-1.,0.,0.));
#36392=DIRECTION('center_axis',(0.,1.,0.));
#36393=DIRECTION('ref_axis',(0.,0.,-1.));
#36394=DIRECTION('',(0.,0.,-1.));
#36395=DIRECTION('',(-1.,0.,0.));
#36396=DIRECTION('',(0.,0.,-1.));
#36397=DIRECTION('center_axis',(0.,0.,1.));
#36398=DIRECTION('ref_axis',(0.,1.,0.));
#36399=DIRECTION('',(0.,1.,0.));
#36400=DIRECTION('',(-1.,0.,0.));
#36401=DIRECTION('',(0.,1.,0.));
#36402=DIRECTION('center_axis',(0.,-1.,0.));
#36403=DIRECTION('ref_axis',(0.,0.,1.));
#36404=DIRECTION('',(0.,0.,1.));
#36405=DIRECTION('',(0.,0.,1.));
#36406=DIRECTION('center_axis',(-1.,0.,0.));
#36407=DIRECTION('ref_axis',(0.,0.,1.));
#36408=DIRECTION('center_axis',(0.,0.,-1.));
#36409=DIRECTION('ref_axis',(0.,-1.,0.));
#36410=DIRECTION('',(0.,-1.,0.));
#36411=DIRECTION('',(-1.,0.,0.));
#36412=DIRECTION('',(0.,-1.,0.));
#36413=DIRECTION('',(-1.,0.,0.));
#36414=DIRECTION('center_axis',(0.,1.,0.));
#36415=DIRECTION('ref_axis',(0.,0.,-1.));
#36416=DIRECTION('',(0.,0.,-1.));
#36417=DIRECTION('',(-1.,0.,0.));
#36418=DIRECTION('',(0.,0.,-1.));
#36419=DIRECTION('center_axis',(0.,0.,1.));
#36420=DIRECTION('ref_axis',(0.,1.,0.));
#36421=DIRECTION('',(0.,1.,0.));
#36422=DIRECTION('',(-1.,0.,0.));
#36423=DIRECTION('',(0.,1.,0.));
#36424=DIRECTION('center_axis',(0.,-1.,0.));
#36425=DIRECTION('ref_axis',(0.,0.,1.));
#36426=DIRECTION('',(0.,0.,1.));
#36427=DIRECTION('',(0.,0.,1.));
#36428=DIRECTION('center_axis',(-1.,0.,0.));
#36429=DIRECTION('ref_axis',(0.,0.,1.));
#36430=DIRECTION('center_axis',(0.,0.,-1.));
#36431=DIRECTION('ref_axis',(0.,-1.,0.));
#36432=DIRECTION('',(0.,-1.,0.));
#36433=DIRECTION('',(-1.,0.,0.));
#36434=DIRECTION('',(0.,-1.,0.));
#36435=DIRECTION('',(-1.,0.,0.));
#36436=DIRECTION('center_axis',(0.,1.,0.));
#36437=DIRECTION('ref_axis',(0.,0.,-1.));
#36438=DIRECTION('',(0.,0.,-1.));
#36439=DIRECTION('',(-1.,0.,0.));
#36440=DIRECTION('',(0.,0.,-1.));
#36441=DIRECTION('center_axis',(0.,0.,1.));
#36442=DIRECTION('ref_axis',(0.,1.,0.));
#36443=DIRECTION('',(0.,1.,0.));
#36444=DIRECTION('',(-1.,0.,0.));
#36445=DIRECTION('',(0.,1.,0.));
#36446=DIRECTION('center_axis',(0.,-1.,0.));
#36447=DIRECTION('ref_axis',(0.,0.,1.));
#36448=DIRECTION('',(0.,0.,1.));
#36449=DIRECTION('',(0.,0.,1.));
#36450=DIRECTION('center_axis',(-1.,0.,0.));
#36451=DIRECTION('ref_axis',(0.,0.,1.));
#36452=DIRECTION('center_axis',(0.,0.,-1.));
#36453=DIRECTION('ref_axis',(0.,-1.,0.));
#36454=DIRECTION('',(0.,-1.,0.));
#36455=DIRECTION('',(-1.,0.,0.));
#36456=DIRECTION('',(0.,-1.,0.));
#36457=DIRECTION('',(-1.,0.,0.));
#36458=DIRECTION('center_axis',(0.,1.,0.));
#36459=DIRECTION('ref_axis',(0.,0.,-1.));
#36460=DIRECTION('',(0.,0.,-1.));
#36461=DIRECTION('',(-1.,0.,0.));
#36462=DIRECTION('',(0.,0.,-1.));
#36463=DIRECTION('center_axis',(0.,0.,1.));
#36464=DIRECTION('ref_axis',(0.,1.,0.));
#36465=DIRECTION('',(0.,1.,0.));
#36466=DIRECTION('',(-1.,0.,0.));
#36467=DIRECTION('',(0.,1.,0.));
#36468=DIRECTION('center_axis',(0.,-1.,0.));
#36469=DIRECTION('ref_axis',(0.,0.,1.));
#36470=DIRECTION('',(0.,0.,1.));
#36471=DIRECTION('',(0.,0.,1.));
#36472=DIRECTION('center_axis',(-1.,0.,0.));
#36473=DIRECTION('ref_axis',(0.,0.,1.));
#36474=DIRECTION('center_axis',(0.,0.,-1.));
#36475=DIRECTION('ref_axis',(0.,-1.,0.));
#36476=DIRECTION('',(0.,-1.,0.));
#36477=DIRECTION('',(-1.,0.,0.));
#36478=DIRECTION('',(0.,-1.,0.));
#36479=DIRECTION('',(-1.,0.,0.));
#36480=DIRECTION('center_axis',(0.,1.,0.));
#36481=DIRECTION('ref_axis',(0.,0.,-1.));
#36482=DIRECTION('',(0.,0.,-1.));
#36483=DIRECTION('',(-1.,0.,0.));
#36484=DIRECTION('',(0.,0.,-1.));
#36485=DIRECTION('center_axis',(0.,0.,1.));
#36486=DIRECTION('ref_axis',(0.,1.,0.));
#36487=DIRECTION('',(0.,1.,0.));
#36488=DIRECTION('',(-1.,0.,0.));
#36489=DIRECTION('',(0.,1.,0.));
#36490=DIRECTION('center_axis',(0.,-1.,0.));
#36491=DIRECTION('ref_axis',(0.,0.,1.));
#36492=DIRECTION('',(0.,0.,1.));
#36493=DIRECTION('',(0.,0.,1.));
#36494=DIRECTION('center_axis',(-1.,0.,0.));
#36495=DIRECTION('ref_axis',(0.,0.,1.));
#36496=DIRECTION('center_axis',(0.,0.,-1.));
#36497=DIRECTION('ref_axis',(0.,-1.,0.));
#36498=DIRECTION('',(0.,-1.,0.));
#36499=DIRECTION('',(-1.,0.,0.));
#36500=DIRECTION('',(0.,-1.,0.));
#36501=DIRECTION('',(-1.,0.,0.));
#36502=DIRECTION('center_axis',(0.,1.,0.));
#36503=DIRECTION('ref_axis',(0.,0.,-1.));
#36504=DIRECTION('',(0.,0.,-1.));
#36505=DIRECTION('',(-1.,0.,0.));
#36506=DIRECTION('',(0.,0.,-1.));
#36507=DIRECTION('center_axis',(0.,0.,1.));
#36508=DIRECTION('ref_axis',(0.,1.,0.));
#36509=DIRECTION('',(0.,1.,0.));
#36510=DIRECTION('',(-1.,0.,0.));
#36511=DIRECTION('',(0.,1.,0.));
#36512=DIRECTION('center_axis',(0.,-1.,0.));
#36513=DIRECTION('ref_axis',(0.,0.,1.));
#36514=DIRECTION('',(0.,0.,1.));
#36515=DIRECTION('',(0.,0.,1.));
#36516=DIRECTION('center_axis',(-1.,0.,0.));
#36517=DIRECTION('ref_axis',(0.,0.,1.));
#36518=DIRECTION('center_axis',(0.,0.,-1.));
#36519=DIRECTION('ref_axis',(0.,-1.,0.));
#36520=DIRECTION('',(0.,-1.,0.));
#36521=DIRECTION('',(-1.,0.,0.));
#36522=DIRECTION('',(0.,-1.,0.));
#36523=DIRECTION('',(-1.,0.,0.));
#36524=DIRECTION('center_axis',(0.,1.,0.));
#36525=DIRECTION('ref_axis',(0.,0.,-1.));
#36526=DIRECTION('',(0.,0.,-1.));
#36527=DIRECTION('',(-1.,0.,0.));
#36528=DIRECTION('',(0.,0.,-1.));
#36529=DIRECTION('center_axis',(0.,0.,1.));
#36530=DIRECTION('ref_axis',(0.,1.,0.));
#36531=DIRECTION('',(0.,1.,0.));
#36532=DIRECTION('',(-1.,0.,0.));
#36533=DIRECTION('',(0.,1.,0.));
#36534=DIRECTION('center_axis',(0.,-1.,0.));
#36535=DIRECTION('ref_axis',(0.,0.,1.));
#36536=DIRECTION('',(0.,0.,1.));
#36537=DIRECTION('',(0.,0.,1.));
#36538=DIRECTION('center_axis',(-1.,0.,0.));
#36539=DIRECTION('ref_axis',(0.,0.,1.));
#36540=DIRECTION('center_axis',(0.,0.,-1.));
#36541=DIRECTION('ref_axis',(0.,-1.,0.));
#36542=DIRECTION('',(0.,-1.,0.));
#36543=DIRECTION('',(-1.,0.,0.));
#36544=DIRECTION('',(0.,-1.,0.));
#36545=DIRECTION('',(-1.,0.,0.));
#36546=DIRECTION('center_axis',(0.,1.,0.));
#36547=DIRECTION('ref_axis',(0.,0.,-1.));
#36548=DIRECTION('',(0.,0.,-1.));
#36549=DIRECTION('',(-1.,0.,0.));
#36550=DIRECTION('',(0.,0.,-1.));
#36551=DIRECTION('center_axis',(0.,0.,1.));
#36552=DIRECTION('ref_axis',(0.,1.,0.));
#36553=DIRECTION('',(0.,1.,0.));
#36554=DIRECTION('',(-1.,0.,0.));
#36555=DIRECTION('',(0.,1.,0.));
#36556=DIRECTION('center_axis',(0.,-1.,0.));
#36557=DIRECTION('ref_axis',(0.,0.,1.));
#36558=DIRECTION('',(0.,0.,1.));
#36559=DIRECTION('',(0.,0.,1.));
#36560=DIRECTION('center_axis',(-1.,0.,0.));
#36561=DIRECTION('ref_axis',(0.,0.,1.));
#36562=DIRECTION('center_axis',(0.,0.,-1.));
#36563=DIRECTION('ref_axis',(0.,-1.,0.));
#36564=DIRECTION('',(0.,-1.,0.));
#36565=DIRECTION('',(-1.,0.,0.));
#36566=DIRECTION('',(0.,-1.,0.));
#36567=DIRECTION('',(-1.,0.,0.));
#36568=DIRECTION('center_axis',(0.,1.,0.));
#36569=DIRECTION('ref_axis',(0.,0.,-1.));
#36570=DIRECTION('',(0.,0.,-1.));
#36571=DIRECTION('',(-1.,0.,0.));
#36572=DIRECTION('',(0.,0.,-1.));
#36573=DIRECTION('center_axis',(0.,0.,1.));
#36574=DIRECTION('ref_axis',(0.,1.,0.));
#36575=DIRECTION('',(0.,1.,0.));
#36576=DIRECTION('',(-1.,0.,0.));
#36577=DIRECTION('',(0.,1.,0.));
#36578=DIRECTION('center_axis',(0.,-1.,0.));
#36579=DIRECTION('ref_axis',(0.,0.,1.));
#36580=DIRECTION('',(0.,0.,1.));
#36581=DIRECTION('',(0.,0.,1.));
#36582=DIRECTION('center_axis',(-1.,0.,0.));
#36583=DIRECTION('ref_axis',(0.,0.,1.));
#36584=DIRECTION('center_axis',(0.,0.,-1.));
#36585=DIRECTION('ref_axis',(0.,-1.,0.));
#36586=DIRECTION('',(0.,-1.,0.));
#36587=DIRECTION('',(-1.,0.,0.));
#36588=DIRECTION('',(0.,-1.,0.));
#36589=DIRECTION('',(-1.,0.,0.));
#36590=DIRECTION('center_axis',(0.,1.,0.));
#36591=DIRECTION('ref_axis',(0.,0.,-1.));
#36592=DIRECTION('',(0.,0.,-1.));
#36593=DIRECTION('',(-1.,0.,0.));
#36594=DIRECTION('',(0.,0.,-1.));
#36595=DIRECTION('center_axis',(0.,0.,1.));
#36596=DIRECTION('ref_axis',(0.,1.,0.));
#36597=DIRECTION('',(0.,1.,0.));
#36598=DIRECTION('',(-1.,0.,0.));
#36599=DIRECTION('',(0.,1.,0.));
#36600=DIRECTION('center_axis',(0.,-1.,0.));
#36601=DIRECTION('ref_axis',(0.,0.,1.));
#36602=DIRECTION('',(0.,0.,1.));
#36603=DIRECTION('',(0.,0.,1.));
#36604=DIRECTION('center_axis',(-1.,0.,0.));
#36605=DIRECTION('ref_axis',(0.,0.,1.));
#36606=DIRECTION('center_axis',(0.,0.,-1.));
#36607=DIRECTION('ref_axis',(0.,-1.,0.));
#36608=DIRECTION('',(0.,-1.,0.));
#36609=DIRECTION('',(-1.,0.,0.));
#36610=DIRECTION('',(0.,-1.,0.));
#36611=DIRECTION('',(-1.,0.,0.));
#36612=DIRECTION('center_axis',(0.,1.,0.));
#36613=DIRECTION('ref_axis',(0.,0.,-1.));
#36614=DIRECTION('',(0.,0.,-1.));
#36615=DIRECTION('',(-1.,0.,0.));
#36616=DIRECTION('',(0.,0.,-1.));
#36617=DIRECTION('center_axis',(0.,0.,1.));
#36618=DIRECTION('ref_axis',(0.,1.,0.));
#36619=DIRECTION('',(0.,1.,0.));
#36620=DIRECTION('',(-1.,0.,0.));
#36621=DIRECTION('',(0.,1.,0.));
#36622=DIRECTION('center_axis',(0.,-1.,0.));
#36623=DIRECTION('ref_axis',(0.,0.,1.));
#36624=DIRECTION('',(0.,0.,1.));
#36625=DIRECTION('',(0.,0.,1.));
#36626=DIRECTION('center_axis',(-1.,0.,0.));
#36627=DIRECTION('ref_axis',(0.,0.,1.));
#36628=DIRECTION('center_axis',(0.,0.,-1.));
#36629=DIRECTION('ref_axis',(0.,-1.,0.));
#36630=DIRECTION('',(0.,-1.,0.));
#36631=DIRECTION('',(-1.,0.,0.));
#36632=DIRECTION('',(0.,-1.,0.));
#36633=DIRECTION('',(-1.,0.,0.));
#36634=DIRECTION('center_axis',(0.,1.,0.));
#36635=DIRECTION('ref_axis',(0.,0.,-1.));
#36636=DIRECTION('',(0.,0.,-1.));
#36637=DIRECTION('',(-1.,0.,0.));
#36638=DIRECTION('',(0.,0.,-1.));
#36639=DIRECTION('center_axis',(0.,0.,1.));
#36640=DIRECTION('ref_axis',(0.,1.,0.));
#36641=DIRECTION('',(0.,1.,0.));
#36642=DIRECTION('',(-1.,0.,0.));
#36643=DIRECTION('',(0.,1.,0.));
#36644=DIRECTION('center_axis',(0.,-1.,0.));
#36645=DIRECTION('ref_axis',(0.,0.,1.));
#36646=DIRECTION('',(0.,0.,1.));
#36647=DIRECTION('',(0.,0.,1.));
#36648=DIRECTION('center_axis',(-1.,0.,0.));
#36649=DIRECTION('ref_axis',(0.,0.,1.));
#36650=DIRECTION('center_axis',(0.,0.,-1.));
#36651=DIRECTION('ref_axis',(0.,-1.,0.));
#36652=DIRECTION('',(0.,-1.,0.));
#36653=DIRECTION('',(-1.,0.,0.));
#36654=DIRECTION('',(0.,-1.,0.));
#36655=DIRECTION('',(-1.,0.,0.));
#36656=DIRECTION('center_axis',(0.,1.,0.));
#36657=DIRECTION('ref_axis',(0.,0.,-1.));
#36658=DIRECTION('',(0.,0.,-1.));
#36659=DIRECTION('',(-1.,0.,0.));
#36660=DIRECTION('',(0.,0.,-1.));
#36661=DIRECTION('center_axis',(0.,0.,1.));
#36662=DIRECTION('ref_axis',(0.,1.,0.));
#36663=DIRECTION('',(0.,1.,0.));
#36664=DIRECTION('',(-1.,0.,0.));
#36665=DIRECTION('',(0.,1.,0.));
#36666=DIRECTION('center_axis',(0.,-1.,0.));
#36667=DIRECTION('ref_axis',(0.,0.,1.));
#36668=DIRECTION('',(0.,0.,1.));
#36669=DIRECTION('',(0.,0.,1.));
#36670=DIRECTION('center_axis',(-1.,0.,0.));
#36671=DIRECTION('ref_axis',(0.,0.,1.));
#36672=DIRECTION('center_axis',(0.,0.,-1.));
#36673=DIRECTION('ref_axis',(0.,-1.,0.));
#36674=DIRECTION('',(0.,-1.,0.));
#36675=DIRECTION('',(-1.,0.,0.));
#36676=DIRECTION('',(0.,-1.,0.));
#36677=DIRECTION('',(-1.,0.,0.));
#36678=DIRECTION('center_axis',(0.,1.,0.));
#36679=DIRECTION('ref_axis',(0.,0.,-1.));
#36680=DIRECTION('',(0.,0.,-1.));
#36681=DIRECTION('',(-1.,0.,0.));
#36682=DIRECTION('',(0.,0.,-1.));
#36683=DIRECTION('center_axis',(0.,0.,1.));
#36684=DIRECTION('ref_axis',(0.,1.,0.));
#36685=DIRECTION('',(0.,1.,0.));
#36686=DIRECTION('',(-1.,0.,0.));
#36687=DIRECTION('',(0.,1.,0.));
#36688=DIRECTION('center_axis',(0.,-1.,0.));
#36689=DIRECTION('ref_axis',(0.,0.,1.));
#36690=DIRECTION('',(0.,0.,1.));
#36691=DIRECTION('',(0.,0.,1.));
#36692=DIRECTION('center_axis',(-1.,0.,0.));
#36693=DIRECTION('ref_axis',(0.,0.,1.));
#36694=DIRECTION('center_axis',(0.,0.,-1.));
#36695=DIRECTION('ref_axis',(0.,-1.,0.));
#36696=DIRECTION('',(0.,-1.,0.));
#36697=DIRECTION('',(-1.,0.,0.));
#36698=DIRECTION('',(0.,-1.,0.));
#36699=DIRECTION('',(-1.,0.,0.));
#36700=DIRECTION('center_axis',(0.,1.,0.));
#36701=DIRECTION('ref_axis',(0.,0.,-1.));
#36702=DIRECTION('',(0.,0.,-1.));
#36703=DIRECTION('',(-1.,0.,0.));
#36704=DIRECTION('',(0.,0.,-1.));
#36705=DIRECTION('center_axis',(0.,0.,1.));
#36706=DIRECTION('ref_axis',(0.,1.,0.));
#36707=DIRECTION('',(0.,1.,0.));
#36708=DIRECTION('',(-1.,0.,0.));
#36709=DIRECTION('',(0.,1.,0.));
#36710=DIRECTION('center_axis',(0.,-1.,0.));
#36711=DIRECTION('ref_axis',(0.,0.,1.));
#36712=DIRECTION('',(0.,0.,1.));
#36713=DIRECTION('',(0.,0.,1.));
#36714=DIRECTION('center_axis',(-1.,0.,0.));
#36715=DIRECTION('ref_axis',(0.,0.,1.));
#36716=DIRECTION('center_axis',(0.,0.,-1.));
#36717=DIRECTION('ref_axis',(0.,-1.,0.));
#36718=DIRECTION('',(0.,-1.,0.));
#36719=DIRECTION('',(-1.,0.,0.));
#36720=DIRECTION('',(0.,-1.,0.));
#36721=DIRECTION('',(-1.,0.,0.));
#36722=DIRECTION('center_axis',(0.,1.,0.));
#36723=DIRECTION('ref_axis',(0.,0.,-1.));
#36724=DIRECTION('',(0.,0.,-1.));
#36725=DIRECTION('',(-1.,0.,0.));
#36726=DIRECTION('',(0.,0.,-1.));
#36727=DIRECTION('center_axis',(0.,0.,1.));
#36728=DIRECTION('ref_axis',(0.,1.,0.));
#36729=DIRECTION('',(0.,1.,0.));
#36730=DIRECTION('',(-1.,0.,0.));
#36731=DIRECTION('',(0.,1.,0.));
#36732=DIRECTION('center_axis',(0.,-1.,0.));
#36733=DIRECTION('ref_axis',(0.,0.,1.));
#36734=DIRECTION('',(0.,0.,1.));
#36735=DIRECTION('',(0.,0.,1.));
#36736=DIRECTION('center_axis',(-1.,0.,0.));
#36737=DIRECTION('ref_axis',(0.,0.,1.));
#36738=DIRECTION('center_axis',(0.,0.,-1.));
#36739=DIRECTION('ref_axis',(0.,-1.,0.));
#36740=DIRECTION('',(0.,-1.,0.));
#36741=DIRECTION('',(-1.,0.,0.));
#36742=DIRECTION('',(0.,-1.,0.));
#36743=DIRECTION('',(-1.,0.,0.));
#36744=DIRECTION('center_axis',(0.,1.,0.));
#36745=DIRECTION('ref_axis',(0.,0.,-1.));
#36746=DIRECTION('',(0.,0.,-1.));
#36747=DIRECTION('',(-1.,0.,0.));
#36748=DIRECTION('',(0.,0.,-1.));
#36749=DIRECTION('center_axis',(0.,0.,1.));
#36750=DIRECTION('ref_axis',(0.,1.,0.));
#36751=DIRECTION('',(0.,1.,0.));
#36752=DIRECTION('',(-1.,0.,0.));
#36753=DIRECTION('',(0.,1.,0.));
#36754=DIRECTION('center_axis',(0.,-1.,0.));
#36755=DIRECTION('ref_axis',(0.,0.,1.));
#36756=DIRECTION('',(0.,0.,1.));
#36757=DIRECTION('',(0.,0.,1.));
#36758=DIRECTION('center_axis',(-1.,0.,0.));
#36759=DIRECTION('ref_axis',(0.,0.,1.));
#36760=DIRECTION('center_axis',(0.,0.,-1.));
#36761=DIRECTION('ref_axis',(0.,-1.,0.));
#36762=DIRECTION('',(0.,-1.,0.));
#36763=DIRECTION('',(-1.,0.,0.));
#36764=DIRECTION('',(0.,-1.,0.));
#36765=DIRECTION('',(-1.,0.,0.));
#36766=DIRECTION('center_axis',(0.,1.,0.));
#36767=DIRECTION('ref_axis',(0.,0.,-1.));
#36768=DIRECTION('',(0.,0.,-1.));
#36769=DIRECTION('',(-1.,0.,0.));
#36770=DIRECTION('',(0.,0.,-1.));
#36771=DIRECTION('center_axis',(0.,0.,1.));
#36772=DIRECTION('ref_axis',(0.,1.,0.));
#36773=DIRECTION('',(0.,1.,0.));
#36774=DIRECTION('',(-1.,0.,0.));
#36775=DIRECTION('',(0.,1.,0.));
#36776=DIRECTION('center_axis',(0.,-1.,0.));
#36777=DIRECTION('ref_axis',(0.,0.,1.));
#36778=DIRECTION('',(0.,0.,1.));
#36779=DIRECTION('',(0.,0.,1.));
#36780=DIRECTION('center_axis',(-1.,0.,0.));
#36781=DIRECTION('ref_axis',(0.,0.,1.));
#36782=DIRECTION('center_axis',(0.,0.,-1.));
#36783=DIRECTION('ref_axis',(0.,-1.,0.));
#36784=DIRECTION('',(0.,-1.,0.));
#36785=DIRECTION('',(-1.,0.,0.));
#36786=DIRECTION('',(0.,-1.,0.));
#36787=DIRECTION('',(-1.,0.,0.));
#36788=DIRECTION('center_axis',(0.,1.,0.));
#36789=DIRECTION('ref_axis',(0.,0.,-1.));
#36790=DIRECTION('',(0.,0.,-1.));
#36791=DIRECTION('',(-1.,0.,0.));
#36792=DIRECTION('',(0.,0.,-1.));
#36793=DIRECTION('center_axis',(0.,0.,1.));
#36794=DIRECTION('ref_axis',(0.,1.,0.));
#36795=DIRECTION('',(0.,1.,0.));
#36796=DIRECTION('',(-1.,0.,0.));
#36797=DIRECTION('',(0.,1.,0.));
#36798=DIRECTION('center_axis',(0.,-1.,0.));
#36799=DIRECTION('ref_axis',(0.,0.,1.));
#36800=DIRECTION('',(0.,0.,1.));
#36801=DIRECTION('',(0.,0.,1.));
#36802=DIRECTION('center_axis',(-1.,0.,0.));
#36803=DIRECTION('ref_axis',(0.,0.,1.));
#36804=DIRECTION('center_axis',(0.,0.,-1.));
#36805=DIRECTION('ref_axis',(0.,-1.,0.));
#36806=DIRECTION('',(0.,-1.,0.));
#36807=DIRECTION('',(-1.,0.,0.));
#36808=DIRECTION('',(0.,-1.,0.));
#36809=DIRECTION('',(-1.,0.,0.));
#36810=DIRECTION('center_axis',(0.,1.,0.));
#36811=DIRECTION('ref_axis',(0.,0.,-1.));
#36812=DIRECTION('',(0.,0.,-1.));
#36813=DIRECTION('',(-1.,0.,0.));
#36814=DIRECTION('',(0.,0.,-1.));
#36815=DIRECTION('center_axis',(0.,0.,1.));
#36816=DIRECTION('ref_axis',(0.,1.,0.));
#36817=DIRECTION('',(0.,1.,0.));
#36818=DIRECTION('',(-1.,0.,0.));
#36819=DIRECTION('',(0.,1.,0.));
#36820=DIRECTION('center_axis',(0.,-1.,0.));
#36821=DIRECTION('ref_axis',(0.,0.,1.));
#36822=DIRECTION('',(0.,0.,1.));
#36823=DIRECTION('',(0.,0.,1.));
#36824=DIRECTION('center_axis',(-1.,0.,0.));
#36825=DIRECTION('ref_axis',(0.,0.,1.));
#36826=DIRECTION('center_axis',(0.,0.,-1.));
#36827=DIRECTION('ref_axis',(0.,-1.,0.));
#36828=DIRECTION('',(0.,-1.,0.));
#36829=DIRECTION('',(-1.,0.,0.));
#36830=DIRECTION('',(0.,-1.,0.));
#36831=DIRECTION('',(-1.,0.,0.));
#36832=DIRECTION('center_axis',(0.,1.,0.));
#36833=DIRECTION('ref_axis',(0.,0.,-1.));
#36834=DIRECTION('',(0.,0.,-1.));
#36835=DIRECTION('',(-1.,0.,0.));
#36836=DIRECTION('',(0.,0.,-1.));
#36837=DIRECTION('center_axis',(0.,0.,1.));
#36838=DIRECTION('ref_axis',(0.,1.,0.));
#36839=DIRECTION('',(0.,1.,0.));
#36840=DIRECTION('',(-1.,0.,0.));
#36841=DIRECTION('',(0.,1.,0.));
#36842=DIRECTION('center_axis',(0.,-1.,0.));
#36843=DIRECTION('ref_axis',(0.,0.,1.));
#36844=DIRECTION('',(0.,0.,1.));
#36845=DIRECTION('',(0.,0.,1.));
#36846=DIRECTION('center_axis',(-1.,0.,0.));
#36847=DIRECTION('ref_axis',(0.,0.,1.));
#36848=DIRECTION('center_axis',(0.,0.,-1.));
#36849=DIRECTION('ref_axis',(0.,-1.,0.));
#36850=DIRECTION('',(0.,-1.,0.));
#36851=DIRECTION('',(-1.,0.,0.));
#36852=DIRECTION('',(0.,-1.,0.));
#36853=DIRECTION('',(-1.,0.,0.));
#36854=DIRECTION('center_axis',(0.,1.,0.));
#36855=DIRECTION('ref_axis',(0.,0.,-1.));
#36856=DIRECTION('',(0.,0.,-1.));
#36857=DIRECTION('',(-1.,0.,0.));
#36858=DIRECTION('',(0.,0.,-1.));
#36859=DIRECTION('center_axis',(0.,0.,1.));
#36860=DIRECTION('ref_axis',(0.,1.,0.));
#36861=DIRECTION('',(0.,1.,0.));
#36862=DIRECTION('',(-1.,0.,0.));
#36863=DIRECTION('',(0.,1.,0.));
#36864=DIRECTION('center_axis',(0.,-1.,0.));
#36865=DIRECTION('ref_axis',(0.,0.,1.));
#36866=DIRECTION('',(0.,0.,1.));
#36867=DIRECTION('',(0.,0.,1.));
#36868=DIRECTION('center_axis',(-1.,0.,0.));
#36869=DIRECTION('ref_axis',(0.,0.,1.));
#36870=DIRECTION('center_axis',(0.,0.,-1.));
#36871=DIRECTION('ref_axis',(0.,-1.,0.));
#36872=DIRECTION('',(0.,-1.,0.));
#36873=DIRECTION('',(-1.,0.,0.));
#36874=DIRECTION('',(0.,-1.,0.));
#36875=DIRECTION('',(-1.,0.,0.));
#36876=DIRECTION('center_axis',(0.,1.,0.));
#36877=DIRECTION('ref_axis',(0.,0.,-1.));
#36878=DIRECTION('',(0.,0.,-1.));
#36879=DIRECTION('',(-1.,0.,0.));
#36880=DIRECTION('',(0.,0.,-1.));
#36881=DIRECTION('center_axis',(0.,0.,1.));
#36882=DIRECTION('ref_axis',(0.,1.,0.));
#36883=DIRECTION('',(0.,1.,0.));
#36884=DIRECTION('',(-1.,0.,0.));
#36885=DIRECTION('',(0.,1.,0.));
#36886=DIRECTION('center_axis',(0.,-1.,0.));
#36887=DIRECTION('ref_axis',(0.,0.,1.));
#36888=DIRECTION('',(0.,0.,1.));
#36889=DIRECTION('',(0.,0.,1.));
#36890=DIRECTION('center_axis',(-1.,0.,0.));
#36891=DIRECTION('ref_axis',(0.,0.,1.));
#36892=DIRECTION('center_axis',(0.,0.,-1.));
#36893=DIRECTION('ref_axis',(0.,-1.,0.));
#36894=DIRECTION('',(0.,-1.,0.));
#36895=DIRECTION('',(-1.,0.,0.));
#36896=DIRECTION('',(0.,-1.,0.));
#36897=DIRECTION('',(-1.,0.,0.));
#36898=DIRECTION('center_axis',(0.,1.,0.));
#36899=DIRECTION('ref_axis',(0.,0.,-1.));
#36900=DIRECTION('',(0.,0.,-1.));
#36901=DIRECTION('',(-1.,0.,0.));
#36902=DIRECTION('',(0.,0.,-1.));
#36903=DIRECTION('center_axis',(0.,0.,1.));
#36904=DIRECTION('ref_axis',(0.,1.,0.));
#36905=DIRECTION('',(0.,1.,0.));
#36906=DIRECTION('',(-1.,0.,0.));
#36907=DIRECTION('',(0.,1.,0.));
#36908=DIRECTION('center_axis',(0.,-1.,0.));
#36909=DIRECTION('ref_axis',(0.,0.,1.));
#36910=DIRECTION('',(0.,0.,1.));
#36911=DIRECTION('',(0.,0.,1.));
#36912=DIRECTION('center_axis',(-1.,0.,0.));
#36913=DIRECTION('ref_axis',(0.,0.,1.));
#36914=DIRECTION('center_axis',(0.,0.,-1.));
#36915=DIRECTION('ref_axis',(0.,-1.,0.));
#36916=DIRECTION('',(0.,-1.,0.));
#36917=DIRECTION('',(-1.,0.,0.));
#36918=DIRECTION('',(0.,-1.,0.));
#36919=DIRECTION('',(-1.,0.,0.));
#36920=DIRECTION('center_axis',(0.,1.,0.));
#36921=DIRECTION('ref_axis',(0.,0.,-1.));
#36922=DIRECTION('',(0.,0.,-1.));
#36923=DIRECTION('',(-1.,0.,0.));
#36924=DIRECTION('',(0.,0.,-1.));
#36925=DIRECTION('center_axis',(0.,0.,1.));
#36926=DIRECTION('ref_axis',(0.,1.,0.));
#36927=DIRECTION('',(0.,1.,0.));
#36928=DIRECTION('',(-1.,0.,0.));
#36929=DIRECTION('',(0.,1.,0.));
#36930=DIRECTION('center_axis',(0.,-1.,0.));
#36931=DIRECTION('ref_axis',(0.,0.,1.));
#36932=DIRECTION('',(0.,0.,1.));
#36933=DIRECTION('',(0.,0.,1.));
#36934=DIRECTION('center_axis',(-1.,0.,0.));
#36935=DIRECTION('ref_axis',(0.,0.,1.));
#36936=DIRECTION('center_axis',(0.,0.,-1.));
#36937=DIRECTION('ref_axis',(0.,-1.,0.));
#36938=DIRECTION('',(0.,-1.,0.));
#36939=DIRECTION('',(-1.,0.,0.));
#36940=DIRECTION('',(0.,-1.,0.));
#36941=DIRECTION('',(-1.,0.,0.));
#36942=DIRECTION('center_axis',(0.,1.,0.));
#36943=DIRECTION('ref_axis',(0.,0.,-1.));
#36944=DIRECTION('',(0.,0.,-1.));
#36945=DIRECTION('',(-1.,0.,0.));
#36946=DIRECTION('',(0.,0.,-1.));
#36947=DIRECTION('center_axis',(0.,0.,1.));
#36948=DIRECTION('ref_axis',(0.,1.,0.));
#36949=DIRECTION('',(0.,1.,0.));
#36950=DIRECTION('',(-1.,0.,0.));
#36951=DIRECTION('',(0.,1.,0.));
#36952=DIRECTION('center_axis',(0.,-1.,0.));
#36953=DIRECTION('ref_axis',(0.,0.,1.));
#36954=DIRECTION('',(0.,0.,1.));
#36955=DIRECTION('',(0.,0.,1.));
#36956=DIRECTION('center_axis',(-1.,0.,0.));
#36957=DIRECTION('ref_axis',(0.,0.,1.));
#36958=DIRECTION('center_axis',(0.,0.,-1.));
#36959=DIRECTION('ref_axis',(0.,-1.,0.));
#36960=DIRECTION('',(0.,-1.,0.));
#36961=DIRECTION('',(-1.,0.,0.));
#36962=DIRECTION('',(0.,-1.,0.));
#36963=DIRECTION('',(-1.,0.,0.));
#36964=DIRECTION('center_axis',(0.,1.,0.));
#36965=DIRECTION('ref_axis',(0.,0.,-1.));
#36966=DIRECTION('',(0.,0.,-1.));
#36967=DIRECTION('',(-1.,0.,0.));
#36968=DIRECTION('',(0.,0.,-1.));
#36969=DIRECTION('center_axis',(0.,0.,1.));
#36970=DIRECTION('ref_axis',(0.,1.,0.));
#36971=DIRECTION('',(0.,1.,0.));
#36972=DIRECTION('',(-1.,0.,0.));
#36973=DIRECTION('',(0.,1.,0.));
#36974=DIRECTION('center_axis',(0.,-1.,0.));
#36975=DIRECTION('ref_axis',(0.,0.,1.));
#36976=DIRECTION('',(0.,0.,1.));
#36977=DIRECTION('',(0.,0.,1.));
#36978=DIRECTION('center_axis',(-1.,0.,0.));
#36979=DIRECTION('ref_axis',(0.,0.,1.));
#36980=DIRECTION('center_axis',(0.,0.,-1.));
#36981=DIRECTION('ref_axis',(0.,-1.,0.));
#36982=DIRECTION('',(0.,-1.,0.));
#36983=DIRECTION('',(-1.,0.,0.));
#36984=DIRECTION('',(0.,-1.,0.));
#36985=DIRECTION('',(-1.,0.,0.));
#36986=DIRECTION('center_axis',(0.,1.,0.));
#36987=DIRECTION('ref_axis',(0.,0.,-1.));
#36988=DIRECTION('',(0.,0.,-1.));
#36989=DIRECTION('',(-1.,0.,0.));
#36990=DIRECTION('',(0.,0.,-1.));
#36991=DIRECTION('center_axis',(0.,0.,1.));
#36992=DIRECTION('ref_axis',(0.,1.,0.));
#36993=DIRECTION('',(0.,1.,0.));
#36994=DIRECTION('',(-1.,0.,0.));
#36995=DIRECTION('',(0.,1.,0.));
#36996=DIRECTION('center_axis',(0.,-1.,0.));
#36997=DIRECTION('ref_axis',(0.,0.,1.));
#36998=DIRECTION('',(0.,0.,1.));
#36999=DIRECTION('',(0.,0.,1.));
#37000=DIRECTION('center_axis',(-1.,0.,0.));
#37001=DIRECTION('ref_axis',(0.,0.,1.));
#37002=DIRECTION('center_axis',(0.,0.,-1.));
#37003=DIRECTION('ref_axis',(0.,-1.,0.));
#37004=DIRECTION('',(0.,-1.,0.));
#37005=DIRECTION('',(-1.,0.,0.));
#37006=DIRECTION('',(0.,-1.,0.));
#37007=DIRECTION('',(-1.,0.,0.));
#37008=DIRECTION('center_axis',(0.,1.,0.));
#37009=DIRECTION('ref_axis',(0.,0.,-1.));
#37010=DIRECTION('',(0.,0.,-1.));
#37011=DIRECTION('',(-1.,0.,0.));
#37012=DIRECTION('',(0.,0.,-1.));
#37013=DIRECTION('center_axis',(0.,0.,1.));
#37014=DIRECTION('ref_axis',(0.,1.,0.));
#37015=DIRECTION('',(0.,1.,0.));
#37016=DIRECTION('',(-1.,0.,0.));
#37017=DIRECTION('',(0.,1.,0.));
#37018=DIRECTION('center_axis',(0.,-1.,0.));
#37019=DIRECTION('ref_axis',(0.,0.,1.));
#37020=DIRECTION('',(0.,0.,1.));
#37021=DIRECTION('',(0.,0.,1.));
#37022=DIRECTION('center_axis',(-1.,0.,0.));
#37023=DIRECTION('ref_axis',(0.,0.,1.));
#37024=DIRECTION('center_axis',(0.,0.,-1.));
#37025=DIRECTION('ref_axis',(0.,-1.,0.));
#37026=DIRECTION('',(0.,-1.,0.));
#37027=DIRECTION('',(-1.,0.,0.));
#37028=DIRECTION('',(0.,-1.,0.));
#37029=DIRECTION('',(-1.,0.,0.));
#37030=DIRECTION('center_axis',(0.,1.,0.));
#37031=DIRECTION('ref_axis',(0.,0.,-1.));
#37032=DIRECTION('',(0.,0.,-1.));
#37033=DIRECTION('',(-1.,0.,0.));
#37034=DIRECTION('',(0.,0.,-1.));
#37035=DIRECTION('center_axis',(0.,0.,1.));
#37036=DIRECTION('ref_axis',(0.,1.,0.));
#37037=DIRECTION('',(0.,1.,0.));
#37038=DIRECTION('',(-1.,0.,0.));
#37039=DIRECTION('',(0.,1.,0.));
#37040=DIRECTION('center_axis',(0.,-1.,0.));
#37041=DIRECTION('ref_axis',(0.,0.,1.));
#37042=DIRECTION('',(0.,0.,1.));
#37043=DIRECTION('',(0.,0.,1.));
#37044=DIRECTION('center_axis',(-1.,0.,0.));
#37045=DIRECTION('ref_axis',(0.,0.,1.));
#37046=DIRECTION('center_axis',(0.,0.,-1.));
#37047=DIRECTION('ref_axis',(0.,-1.,0.));
#37048=DIRECTION('',(0.,-1.,0.));
#37049=DIRECTION('',(-1.,0.,0.));
#37050=DIRECTION('',(0.,-1.,0.));
#37051=DIRECTION('',(-1.,0.,0.));
#37052=DIRECTION('center_axis',(0.,1.,0.));
#37053=DIRECTION('ref_axis',(0.,0.,-1.));
#37054=DIRECTION('',(0.,0.,-1.));
#37055=DIRECTION('',(-1.,0.,0.));
#37056=DIRECTION('',(0.,0.,-1.));
#37057=DIRECTION('center_axis',(0.,0.,1.));
#37058=DIRECTION('ref_axis',(0.,1.,0.));
#37059=DIRECTION('',(0.,1.,0.));
#37060=DIRECTION('',(-1.,0.,0.));
#37061=DIRECTION('',(0.,1.,0.));
#37062=DIRECTION('center_axis',(0.,-1.,0.));
#37063=DIRECTION('ref_axis',(0.,0.,1.));
#37064=DIRECTION('',(0.,0.,1.));
#37065=DIRECTION('',(0.,0.,1.));
#37066=DIRECTION('center_axis',(-1.,0.,0.));
#37067=DIRECTION('ref_axis',(0.,0.,1.));
#37068=DIRECTION('center_axis',(0.,0.,-1.));
#37069=DIRECTION('ref_axis',(0.,-1.,0.));
#37070=DIRECTION('',(0.,-1.,0.));
#37071=DIRECTION('',(-1.,0.,0.));
#37072=DIRECTION('',(0.,-1.,0.));
#37073=DIRECTION('',(-1.,0.,0.));
#37074=DIRECTION('center_axis',(0.,1.,0.));
#37075=DIRECTION('ref_axis',(0.,0.,-1.));
#37076=DIRECTION('',(0.,0.,-1.));
#37077=DIRECTION('',(-1.,0.,0.));
#37078=DIRECTION('',(0.,0.,-1.));
#37079=DIRECTION('center_axis',(0.,0.,1.));
#37080=DIRECTION('ref_axis',(0.,1.,0.));
#37081=DIRECTION('',(0.,1.,0.));
#37082=DIRECTION('',(-1.,0.,0.));
#37083=DIRECTION('',(0.,1.,0.));
#37084=DIRECTION('center_axis',(0.,-1.,0.));
#37085=DIRECTION('ref_axis',(0.,0.,1.));
#37086=DIRECTION('',(0.,0.,1.));
#37087=DIRECTION('',(0.,0.,1.));
#37088=DIRECTION('center_axis',(-1.,0.,0.));
#37089=DIRECTION('ref_axis',(0.,0.,1.));
#37090=DIRECTION('center_axis',(0.,0.,-1.));
#37091=DIRECTION('ref_axis',(0.,-1.,0.));
#37092=DIRECTION('',(0.,-1.,0.));
#37093=DIRECTION('',(-1.,0.,0.));
#37094=DIRECTION('',(0.,-1.,0.));
#37095=DIRECTION('',(-1.,0.,0.));
#37096=DIRECTION('center_axis',(0.,1.,0.));
#37097=DIRECTION('ref_axis',(0.,0.,-1.));
#37098=DIRECTION('',(0.,0.,-1.));
#37099=DIRECTION('',(-1.,0.,0.));
#37100=DIRECTION('',(0.,0.,-1.));
#37101=DIRECTION('center_axis',(0.,0.,1.));
#37102=DIRECTION('ref_axis',(0.,1.,0.));
#37103=DIRECTION('',(0.,1.,0.));
#37104=DIRECTION('',(-1.,0.,0.));
#37105=DIRECTION('',(0.,1.,0.));
#37106=DIRECTION('center_axis',(0.,-1.,0.));
#37107=DIRECTION('ref_axis',(0.,0.,1.));
#37108=DIRECTION('',(0.,0.,1.));
#37109=DIRECTION('',(0.,0.,1.));
#37110=DIRECTION('center_axis',(-1.,0.,0.));
#37111=DIRECTION('ref_axis',(0.,0.,1.));
#37112=DIRECTION('center_axis',(0.,0.,-1.));
#37113=DIRECTION('ref_axis',(0.,-1.,0.));
#37114=DIRECTION('',(0.,-1.,0.));
#37115=DIRECTION('',(-1.,0.,0.));
#37116=DIRECTION('',(0.,-1.,0.));
#37117=DIRECTION('',(-1.,0.,0.));
#37118=DIRECTION('center_axis',(0.,1.,0.));
#37119=DIRECTION('ref_axis',(0.,0.,-1.));
#37120=DIRECTION('',(0.,0.,-1.));
#37121=DIRECTION('',(-1.,0.,0.));
#37122=DIRECTION('',(0.,0.,-1.));
#37123=DIRECTION('center_axis',(0.,0.,1.));
#37124=DIRECTION('ref_axis',(0.,1.,0.));
#37125=DIRECTION('',(0.,1.,0.));
#37126=DIRECTION('',(-1.,0.,0.));
#37127=DIRECTION('',(0.,1.,0.));
#37128=DIRECTION('center_axis',(0.,-1.,0.));
#37129=DIRECTION('ref_axis',(0.,0.,1.));
#37130=DIRECTION('',(0.,0.,1.));
#37131=DIRECTION('',(0.,0.,1.));
#37132=DIRECTION('center_axis',(-1.,0.,0.));
#37133=DIRECTION('ref_axis',(0.,0.,1.));
#37134=DIRECTION('center_axis',(0.,0.,-1.));
#37135=DIRECTION('ref_axis',(0.,-1.,0.));
#37136=DIRECTION('',(0.,-1.,0.));
#37137=DIRECTION('',(-1.,0.,0.));
#37138=DIRECTION('',(0.,-1.,0.));
#37139=DIRECTION('',(-1.,0.,0.));
#37140=DIRECTION('center_axis',(0.,1.,0.));
#37141=DIRECTION('ref_axis',(0.,0.,-1.));
#37142=DIRECTION('',(0.,0.,-1.));
#37143=DIRECTION('',(-1.,0.,0.));
#37144=DIRECTION('',(0.,0.,-1.));
#37145=DIRECTION('center_axis',(0.,0.,1.));
#37146=DIRECTION('ref_axis',(0.,1.,0.));
#37147=DIRECTION('',(0.,1.,0.));
#37148=DIRECTION('',(-1.,0.,0.));
#37149=DIRECTION('',(0.,1.,0.));
#37150=DIRECTION('center_axis',(0.,-1.,0.));
#37151=DIRECTION('ref_axis',(0.,0.,1.));
#37152=DIRECTION('',(0.,0.,1.));
#37153=DIRECTION('',(0.,0.,1.));
#37154=DIRECTION('center_axis',(-1.,0.,0.));
#37155=DIRECTION('ref_axis',(0.,0.,1.));
#37156=DIRECTION('center_axis',(0.,0.,-1.));
#37157=DIRECTION('ref_axis',(0.,-1.,0.));
#37158=DIRECTION('',(0.,-1.,0.));
#37159=DIRECTION('',(-1.,0.,0.));
#37160=DIRECTION('',(0.,-1.,0.));
#37161=DIRECTION('',(-1.,0.,0.));
#37162=DIRECTION('center_axis',(0.,1.,0.));
#37163=DIRECTION('ref_axis',(0.,0.,-1.));
#37164=DIRECTION('',(0.,0.,-1.));
#37165=DIRECTION('',(-1.,0.,0.));
#37166=DIRECTION('',(0.,0.,-1.));
#37167=DIRECTION('center_axis',(0.,0.,1.));
#37168=DIRECTION('ref_axis',(0.,1.,0.));
#37169=DIRECTION('',(0.,1.,0.));
#37170=DIRECTION('',(-1.,0.,0.));
#37171=DIRECTION('',(0.,1.,0.));
#37172=DIRECTION('center_axis',(0.,-1.,0.));
#37173=DIRECTION('ref_axis',(0.,0.,1.));
#37174=DIRECTION('',(0.,0.,1.));
#37175=DIRECTION('',(0.,0.,1.));
#37176=DIRECTION('center_axis',(-1.,0.,0.));
#37177=DIRECTION('ref_axis',(0.,0.,1.));
#37178=DIRECTION('center_axis',(0.,0.,-1.));
#37179=DIRECTION('ref_axis',(0.,-1.,0.));
#37180=DIRECTION('',(0.,-1.,0.));
#37181=DIRECTION('',(-1.,0.,0.));
#37182=DIRECTION('',(0.,-1.,0.));
#37183=DIRECTION('',(-1.,0.,0.));
#37184=DIRECTION('center_axis',(0.,1.,0.));
#37185=DIRECTION('ref_axis',(0.,0.,-1.));
#37186=DIRECTION('',(0.,0.,-1.));
#37187=DIRECTION('',(-1.,0.,0.));
#37188=DIRECTION('',(0.,0.,-1.));
#37189=DIRECTION('center_axis',(0.,0.,1.));
#37190=DIRECTION('ref_axis',(0.,1.,0.));
#37191=DIRECTION('',(0.,1.,0.));
#37192=DIRECTION('',(-1.,0.,0.));
#37193=DIRECTION('',(0.,1.,0.));
#37194=DIRECTION('center_axis',(0.,-1.,0.));
#37195=DIRECTION('ref_axis',(0.,0.,1.));
#37196=DIRECTION('',(0.,0.,1.));
#37197=DIRECTION('',(0.,0.,1.));
#37198=DIRECTION('center_axis',(-1.,0.,0.));
#37199=DIRECTION('ref_axis',(0.,0.,1.));
#37200=DIRECTION('center_axis',(0.,0.,-1.));
#37201=DIRECTION('ref_axis',(0.,-1.,0.));
#37202=DIRECTION('',(0.,-1.,0.));
#37203=DIRECTION('',(-1.,0.,0.));
#37204=DIRECTION('',(0.,-1.,0.));
#37205=DIRECTION('',(-1.,0.,0.));
#37206=DIRECTION('center_axis',(0.,1.,0.));
#37207=DIRECTION('ref_axis',(0.,0.,-1.));
#37208=DIRECTION('',(0.,0.,-1.));
#37209=DIRECTION('',(-1.,0.,0.));
#37210=DIRECTION('',(0.,0.,-1.));
#37211=DIRECTION('center_axis',(0.,0.,1.));
#37212=DIRECTION('ref_axis',(0.,1.,0.));
#37213=DIRECTION('',(0.,1.,0.));
#37214=DIRECTION('',(-1.,0.,0.));
#37215=DIRECTION('',(0.,1.,0.));
#37216=DIRECTION('center_axis',(0.,-1.,0.));
#37217=DIRECTION('ref_axis',(0.,0.,1.));
#37218=DIRECTION('',(0.,0.,1.));
#37219=DIRECTION('',(0.,0.,1.));
#37220=DIRECTION('center_axis',(-1.,0.,0.));
#37221=DIRECTION('ref_axis',(0.,0.,1.));
#37222=DIRECTION('center_axis',(0.,0.,-1.));
#37223=DIRECTION('ref_axis',(0.,-1.,0.));
#37224=DIRECTION('',(0.,-1.,0.));
#37225=DIRECTION('',(-1.,0.,0.));
#37226=DIRECTION('',(0.,-1.,0.));
#37227=DIRECTION('',(-1.,0.,0.));
#37228=DIRECTION('center_axis',(0.,1.,0.));
#37229=DIRECTION('ref_axis',(0.,0.,-1.));
#37230=DIRECTION('',(0.,0.,-1.));
#37231=DIRECTION('',(-1.,0.,0.));
#37232=DIRECTION('',(0.,0.,-1.));
#37233=DIRECTION('center_axis',(0.,0.,1.));
#37234=DIRECTION('ref_axis',(0.,1.,0.));
#37235=DIRECTION('',(0.,1.,0.));
#37236=DIRECTION('',(-1.,0.,0.));
#37237=DIRECTION('',(0.,1.,0.));
#37238=DIRECTION('center_axis',(0.,-1.,0.));
#37239=DIRECTION('ref_axis',(0.,0.,1.));
#37240=DIRECTION('',(0.,0.,1.));
#37241=DIRECTION('',(0.,0.,1.));
#37242=DIRECTION('center_axis',(-1.,0.,0.));
#37243=DIRECTION('ref_axis',(0.,0.,1.));
#37244=DIRECTION('center_axis',(0.,0.,-1.));
#37245=DIRECTION('ref_axis',(0.,-1.,0.));
#37246=DIRECTION('',(0.,-1.,0.));
#37247=DIRECTION('',(-1.,0.,0.));
#37248=DIRECTION('',(0.,-1.,0.));
#37249=DIRECTION('',(-1.,0.,0.));
#37250=DIRECTION('center_axis',(0.,1.,0.));
#37251=DIRECTION('ref_axis',(0.,0.,-1.));
#37252=DIRECTION('',(0.,0.,-1.));
#37253=DIRECTION('',(-1.,0.,0.));
#37254=DIRECTION('',(0.,0.,-1.));
#37255=DIRECTION('center_axis',(0.,0.,1.));
#37256=DIRECTION('ref_axis',(0.,1.,0.));
#37257=DIRECTION('',(0.,1.,0.));
#37258=DIRECTION('',(-1.,0.,0.));
#37259=DIRECTION('',(0.,1.,0.));
#37260=DIRECTION('center_axis',(0.,-1.,0.));
#37261=DIRECTION('ref_axis',(0.,0.,1.));
#37262=DIRECTION('',(0.,0.,1.));
#37263=DIRECTION('',(0.,0.,1.));
#37264=DIRECTION('center_axis',(-1.,0.,0.));
#37265=DIRECTION('ref_axis',(0.,0.,1.));
#37266=DIRECTION('center_axis',(0.,0.,-1.));
#37267=DIRECTION('ref_axis',(0.,-1.,0.));
#37268=DIRECTION('',(0.,-1.,0.));
#37269=DIRECTION('',(-1.,0.,0.));
#37270=DIRECTION('',(0.,-1.,0.));
#37271=DIRECTION('',(-1.,0.,0.));
#37272=DIRECTION('center_axis',(0.,1.,0.));
#37273=DIRECTION('ref_axis',(0.,0.,-1.));
#37274=DIRECTION('',(0.,0.,-1.));
#37275=DIRECTION('',(-1.,0.,0.));
#37276=DIRECTION('',(0.,0.,-1.));
#37277=DIRECTION('center_axis',(0.,0.,1.));
#37278=DIRECTION('ref_axis',(0.,1.,0.));
#37279=DIRECTION('',(0.,1.,0.));
#37280=DIRECTION('',(-1.,0.,0.));
#37281=DIRECTION('',(0.,1.,0.));
#37282=DIRECTION('center_axis',(0.,-1.,0.));
#37283=DIRECTION('ref_axis',(0.,0.,1.));
#37284=DIRECTION('',(0.,0.,1.));
#37285=DIRECTION('',(0.,0.,1.));
#37286=DIRECTION('center_axis',(-1.,0.,0.));
#37287=DIRECTION('ref_axis',(0.,0.,1.));
#37288=DIRECTION('center_axis',(0.,0.,-1.));
#37289=DIRECTION('ref_axis',(0.,-1.,0.));
#37290=DIRECTION('',(0.,-1.,0.));
#37291=DIRECTION('',(-1.,0.,0.));
#37292=DIRECTION('',(0.,-1.,0.));
#37293=DIRECTION('',(-1.,0.,0.));
#37294=DIRECTION('center_axis',(0.,1.,0.));
#37295=DIRECTION('ref_axis',(0.,0.,-1.));
#37296=DIRECTION('',(0.,0.,-1.));
#37297=DIRECTION('',(-1.,0.,0.));
#37298=DIRECTION('',(0.,0.,-1.));
#37299=DIRECTION('center_axis',(0.,0.,1.));
#37300=DIRECTION('ref_axis',(0.,1.,0.));
#37301=DIRECTION('',(0.,1.,0.));
#37302=DIRECTION('',(-1.,0.,0.));
#37303=DIRECTION('',(0.,1.,0.));
#37304=DIRECTION('center_axis',(0.,-1.,0.));
#37305=DIRECTION('ref_axis',(0.,0.,1.));
#37306=DIRECTION('',(0.,0.,1.));
#37307=DIRECTION('',(0.,0.,1.));
#37308=DIRECTION('center_axis',(-1.,0.,0.));
#37309=DIRECTION('ref_axis',(0.,0.,1.));
#37310=DIRECTION('center_axis',(0.,0.,-1.));
#37311=DIRECTION('ref_axis',(0.,-1.,0.));
#37312=DIRECTION('',(0.,-1.,0.));
#37313=DIRECTION('',(-1.,0.,0.));
#37314=DIRECTION('',(0.,-1.,0.));
#37315=DIRECTION('',(-1.,0.,0.));
#37316=DIRECTION('center_axis',(0.,1.,0.));
#37317=DIRECTION('ref_axis',(0.,0.,-1.));
#37318=DIRECTION('',(0.,0.,-1.));
#37319=DIRECTION('',(-1.,0.,0.));
#37320=DIRECTION('',(0.,0.,-1.));
#37321=DIRECTION('center_axis',(0.,0.,1.));
#37322=DIRECTION('ref_axis',(0.,1.,0.));
#37323=DIRECTION('',(0.,1.,0.));
#37324=DIRECTION('',(-1.,0.,0.));
#37325=DIRECTION('',(0.,1.,0.));
#37326=DIRECTION('center_axis',(0.,-1.,0.));
#37327=DIRECTION('ref_axis',(0.,0.,1.));
#37328=DIRECTION('',(0.,0.,1.));
#37329=DIRECTION('',(0.,0.,1.));
#37330=DIRECTION('center_axis',(-1.,0.,0.));
#37331=DIRECTION('ref_axis',(0.,0.,1.));
#37332=DIRECTION('center_axis',(0.,0.,-1.));
#37333=DIRECTION('ref_axis',(0.,-1.,0.));
#37334=DIRECTION('',(0.,-1.,0.));
#37335=DIRECTION('',(-1.,0.,0.));
#37336=DIRECTION('',(0.,-1.,0.));
#37337=DIRECTION('',(-1.,0.,0.));
#37338=DIRECTION('center_axis',(0.,1.,0.));
#37339=DIRECTION('ref_axis',(0.,0.,-1.));
#37340=DIRECTION('',(0.,0.,-1.));
#37341=DIRECTION('',(-1.,0.,0.));
#37342=DIRECTION('',(0.,0.,-1.));
#37343=DIRECTION('center_axis',(0.,0.,1.));
#37344=DIRECTION('ref_axis',(0.,1.,0.));
#37345=DIRECTION('',(0.,1.,0.));
#37346=DIRECTION('',(-1.,0.,0.));
#37347=DIRECTION('',(0.,1.,0.));
#37348=DIRECTION('center_axis',(0.,-1.,0.));
#37349=DIRECTION('ref_axis',(0.,0.,1.));
#37350=DIRECTION('',(0.,0.,1.));
#37351=DIRECTION('',(0.,0.,1.));
#37352=DIRECTION('center_axis',(-1.,0.,0.));
#37353=DIRECTION('ref_axis',(0.,0.,1.));
#37354=DIRECTION('center_axis',(0.,0.,-1.));
#37355=DIRECTION('ref_axis',(0.,-1.,0.));
#37356=DIRECTION('',(0.,-1.,0.));
#37357=DIRECTION('',(-1.,0.,0.));
#37358=DIRECTION('',(0.,-1.,0.));
#37359=DIRECTION('',(-1.,0.,0.));
#37360=DIRECTION('center_axis',(0.,1.,0.));
#37361=DIRECTION('ref_axis',(0.,0.,-1.));
#37362=DIRECTION('',(0.,0.,-1.));
#37363=DIRECTION('',(-1.,0.,0.));
#37364=DIRECTION('',(0.,0.,-1.));
#37365=DIRECTION('center_axis',(0.,0.,1.));
#37366=DIRECTION('ref_axis',(0.,1.,0.));
#37367=DIRECTION('',(0.,1.,0.));
#37368=DIRECTION('',(-1.,0.,0.));
#37369=DIRECTION('',(0.,1.,0.));
#37370=DIRECTION('center_axis',(0.,-1.,0.));
#37371=DIRECTION('ref_axis',(0.,0.,1.));
#37372=DIRECTION('',(0.,0.,1.));
#37373=DIRECTION('',(0.,0.,1.));
#37374=DIRECTION('center_axis',(-1.,0.,0.));
#37375=DIRECTION('ref_axis',(0.,0.,1.));
#37376=DIRECTION('center_axis',(0.,0.,-1.));
#37377=DIRECTION('ref_axis',(0.,-1.,0.));
#37378=DIRECTION('',(0.,-1.,0.));
#37379=DIRECTION('',(-1.,0.,0.));
#37380=DIRECTION('',(0.,-1.,0.));
#37381=DIRECTION('',(-1.,0.,0.));
#37382=DIRECTION('center_axis',(0.,1.,0.));
#37383=DIRECTION('ref_axis',(0.,0.,-1.));
#37384=DIRECTION('',(0.,0.,-1.));
#37385=DIRECTION('',(-1.,0.,0.));
#37386=DIRECTION('',(0.,0.,-1.));
#37387=DIRECTION('center_axis',(0.,0.,1.));
#37388=DIRECTION('ref_axis',(0.,1.,0.));
#37389=DIRECTION('',(0.,1.,0.));
#37390=DIRECTION('',(-1.,0.,0.));
#37391=DIRECTION('',(0.,1.,0.));
#37392=DIRECTION('center_axis',(0.,-1.,0.));
#37393=DIRECTION('ref_axis',(0.,0.,1.));
#37394=DIRECTION('',(0.,0.,1.));
#37395=DIRECTION('',(0.,0.,1.));
#37396=DIRECTION('center_axis',(-1.,0.,0.));
#37397=DIRECTION('ref_axis',(0.,0.,1.));
#37398=DIRECTION('center_axis',(0.,0.,-1.));
#37399=DIRECTION('ref_axis',(0.,-1.,0.));
#37400=DIRECTION('',(0.,-1.,0.));
#37401=DIRECTION('',(-1.,0.,0.));
#37402=DIRECTION('',(0.,-1.,0.));
#37403=DIRECTION('',(-1.,0.,0.));
#37404=DIRECTION('center_axis',(0.,1.,0.));
#37405=DIRECTION('ref_axis',(0.,0.,-1.));
#37406=DIRECTION('',(0.,0.,-1.));
#37407=DIRECTION('',(-1.,0.,0.));
#37408=DIRECTION('',(0.,0.,-1.));
#37409=DIRECTION('center_axis',(0.,0.,1.));
#37410=DIRECTION('ref_axis',(0.,1.,0.));
#37411=DIRECTION('',(0.,1.,0.));
#37412=DIRECTION('',(-1.,0.,0.));
#37413=DIRECTION('',(0.,1.,0.));
#37414=DIRECTION('center_axis',(0.,-1.,0.));
#37415=DIRECTION('ref_axis',(0.,0.,1.));
#37416=DIRECTION('',(0.,0.,1.));
#37417=DIRECTION('',(0.,0.,1.));
#37418=DIRECTION('center_axis',(-1.,0.,0.));
#37419=DIRECTION('ref_axis',(0.,0.,1.));
#37420=DIRECTION('center_axis',(0.,0.,-1.));
#37421=DIRECTION('ref_axis',(0.,-1.,0.));
#37422=DIRECTION('',(0.,-1.,0.));
#37423=DIRECTION('',(-1.,0.,0.));
#37424=DIRECTION('',(0.,-1.,0.));
#37425=DIRECTION('',(-1.,0.,0.));
#37426=DIRECTION('center_axis',(0.,1.,0.));
#37427=DIRECTION('ref_axis',(0.,0.,-1.));
#37428=DIRECTION('',(0.,0.,-1.));
#37429=DIRECTION('',(-1.,0.,0.));
#37430=DIRECTION('',(0.,0.,-1.));
#37431=DIRECTION('center_axis',(0.,0.,1.));
#37432=DIRECTION('ref_axis',(0.,1.,0.));
#37433=DIRECTION('',(0.,1.,0.));
#37434=DIRECTION('',(-1.,0.,0.));
#37435=DIRECTION('',(0.,1.,0.));
#37436=DIRECTION('center_axis',(0.,-1.,0.));
#37437=DIRECTION('ref_axis',(0.,0.,1.));
#37438=DIRECTION('',(0.,0.,1.));
#37439=DIRECTION('',(0.,0.,1.));
#37440=DIRECTION('center_axis',(-1.,0.,0.));
#37441=DIRECTION('ref_axis',(0.,0.,1.));
#37442=DIRECTION('center_axis',(0.,0.,-1.));
#37443=DIRECTION('ref_axis',(0.,-1.,0.));
#37444=DIRECTION('',(0.,-1.,0.));
#37445=DIRECTION('',(-1.,0.,0.));
#37446=DIRECTION('',(0.,-1.,0.));
#37447=DIRECTION('',(-1.,0.,0.));
#37448=DIRECTION('center_axis',(0.,1.,0.));
#37449=DIRECTION('ref_axis',(0.,0.,-1.));
#37450=DIRECTION('',(0.,0.,-1.));
#37451=DIRECTION('',(-1.,0.,0.));
#37452=DIRECTION('',(0.,0.,-1.));
#37453=DIRECTION('center_axis',(0.,0.,1.));
#37454=DIRECTION('ref_axis',(0.,1.,0.));
#37455=DIRECTION('',(0.,1.,0.));
#37456=DIRECTION('',(-1.,0.,0.));
#37457=DIRECTION('',(0.,1.,0.));
#37458=DIRECTION('center_axis',(0.,-1.,0.));
#37459=DIRECTION('ref_axis',(0.,0.,1.));
#37460=DIRECTION('',(0.,0.,1.));
#37461=DIRECTION('',(0.,0.,1.));
#37462=DIRECTION('center_axis',(-1.,0.,0.));
#37463=DIRECTION('ref_axis',(0.,0.,1.));
#37464=DIRECTION('center_axis',(0.,0.,-1.));
#37465=DIRECTION('ref_axis',(0.,-1.,0.));
#37466=DIRECTION('',(0.,-1.,0.));
#37467=DIRECTION('',(-1.,0.,0.));
#37468=DIRECTION('',(0.,-1.,0.));
#37469=DIRECTION('',(-1.,0.,0.));
#37470=DIRECTION('center_axis',(0.,1.,0.));
#37471=DIRECTION('ref_axis',(0.,0.,-1.));
#37472=DIRECTION('',(0.,0.,-1.));
#37473=DIRECTION('',(-1.,0.,0.));
#37474=DIRECTION('',(0.,0.,-1.));
#37475=DIRECTION('center_axis',(0.,0.,1.));
#37476=DIRECTION('ref_axis',(0.,1.,0.));
#37477=DIRECTION('',(0.,1.,0.));
#37478=DIRECTION('',(-1.,0.,0.));
#37479=DIRECTION('',(0.,1.,0.));
#37480=DIRECTION('center_axis',(0.,-1.,0.));
#37481=DIRECTION('ref_axis',(0.,0.,1.));
#37482=DIRECTION('',(0.,0.,1.));
#37483=DIRECTION('',(0.,0.,1.));
#37484=DIRECTION('center_axis',(-1.,0.,0.));
#37485=DIRECTION('ref_axis',(0.,0.,1.));
#37486=DIRECTION('center_axis',(0.,0.,-1.));
#37487=DIRECTION('ref_axis',(0.,-1.,0.));
#37488=DIRECTION('',(0.,-1.,0.));
#37489=DIRECTION('',(-1.,0.,0.));
#37490=DIRECTION('',(0.,-1.,0.));
#37491=DIRECTION('',(-1.,0.,0.));
#37492=DIRECTION('center_axis',(0.,1.,0.));
#37493=DIRECTION('ref_axis',(0.,0.,-1.));
#37494=DIRECTION('',(0.,0.,-1.));
#37495=DIRECTION('',(-1.,0.,0.));
#37496=DIRECTION('',(0.,0.,-1.));
#37497=DIRECTION('center_axis',(0.,0.,1.));
#37498=DIRECTION('ref_axis',(0.,1.,0.));
#37499=DIRECTION('',(0.,1.,0.));
#37500=DIRECTION('',(-1.,0.,0.));
#37501=DIRECTION('',(0.,1.,0.));
#37502=DIRECTION('center_axis',(0.,-1.,0.));
#37503=DIRECTION('ref_axis',(0.,0.,1.));
#37504=DIRECTION('',(0.,0.,1.));
#37505=DIRECTION('',(0.,0.,1.));
#37506=DIRECTION('center_axis',(-1.,0.,0.));
#37507=DIRECTION('ref_axis',(0.,0.,1.));
#37508=DIRECTION('center_axis',(0.,0.,-1.));
#37509=DIRECTION('ref_axis',(0.,-1.,0.));
#37510=DIRECTION('',(0.,-1.,0.));
#37511=DIRECTION('',(-1.,0.,0.));
#37512=DIRECTION('',(0.,-1.,0.));
#37513=DIRECTION('',(-1.,0.,0.));
#37514=DIRECTION('center_axis',(0.,1.,0.));
#37515=DIRECTION('ref_axis',(0.,0.,-1.));
#37516=DIRECTION('',(0.,0.,-1.));
#37517=DIRECTION('',(-1.,0.,0.));
#37518=DIRECTION('',(0.,0.,-1.));
#37519=DIRECTION('center_axis',(0.,0.,1.));
#37520=DIRECTION('ref_axis',(0.,1.,0.));
#37521=DIRECTION('',(0.,1.,0.));
#37522=DIRECTION('',(-1.,0.,0.));
#37523=DIRECTION('',(0.,1.,0.));
#37524=DIRECTION('center_axis',(0.,-1.,0.));
#37525=DIRECTION('ref_axis',(0.,0.,1.));
#37526=DIRECTION('',(0.,0.,1.));
#37527=DIRECTION('',(0.,0.,1.));
#37528=DIRECTION('center_axis',(-1.,0.,0.));
#37529=DIRECTION('ref_axis',(0.,0.,1.));
#37530=DIRECTION('center_axis',(0.,0.,-1.));
#37531=DIRECTION('ref_axis',(0.,-1.,0.));
#37532=DIRECTION('',(0.,-1.,0.));
#37533=DIRECTION('',(-1.,0.,0.));
#37534=DIRECTION('',(0.,-1.,0.));
#37535=DIRECTION('',(-1.,0.,0.));
#37536=DIRECTION('center_axis',(0.,1.,0.));
#37537=DIRECTION('ref_axis',(0.,0.,-1.));
#37538=DIRECTION('',(0.,0.,-1.));
#37539=DIRECTION('',(-1.,0.,0.));
#37540=DIRECTION('',(0.,0.,-1.));
#37541=DIRECTION('center_axis',(0.,0.,1.));
#37542=DIRECTION('ref_axis',(0.,1.,0.));
#37543=DIRECTION('',(0.,1.,0.));
#37544=DIRECTION('',(-1.,0.,0.));
#37545=DIRECTION('',(0.,1.,0.));
#37546=DIRECTION('center_axis',(0.,-1.,0.));
#37547=DIRECTION('ref_axis',(0.,0.,1.));
#37548=DIRECTION('',(0.,0.,1.));
#37549=DIRECTION('',(0.,0.,1.));
#37550=DIRECTION('center_axis',(-1.,0.,0.));
#37551=DIRECTION('ref_axis',(0.,0.,1.));
#37552=DIRECTION('center_axis',(0.,0.,-1.));
#37553=DIRECTION('ref_axis',(0.,-1.,0.));
#37554=DIRECTION('',(0.,-1.,0.));
#37555=DIRECTION('',(-1.,0.,0.));
#37556=DIRECTION('',(0.,-1.,0.));
#37557=DIRECTION('',(-1.,0.,0.));
#37558=DIRECTION('center_axis',(0.,1.,0.));
#37559=DIRECTION('ref_axis',(0.,0.,-1.));
#37560=DIRECTION('',(0.,0.,-1.));
#37561=DIRECTION('',(-1.,0.,0.));
#37562=DIRECTION('',(0.,0.,-1.));
#37563=DIRECTION('center_axis',(0.,0.,1.));
#37564=DIRECTION('ref_axis',(0.,1.,0.));
#37565=DIRECTION('',(0.,1.,0.));
#37566=DIRECTION('',(-1.,0.,0.));
#37567=DIRECTION('',(0.,1.,0.));
#37568=DIRECTION('center_axis',(0.,-1.,0.));
#37569=DIRECTION('ref_axis',(0.,0.,1.));
#37570=DIRECTION('',(0.,0.,1.));
#37571=DIRECTION('',(0.,0.,1.));
#37572=DIRECTION('center_axis',(-1.,0.,0.));
#37573=DIRECTION('ref_axis',(0.,0.,1.));
#37574=DIRECTION('center_axis',(0.,0.,-1.));
#37575=DIRECTION('ref_axis',(0.,-1.,0.));
#37576=DIRECTION('',(0.,-1.,0.));
#37577=DIRECTION('',(-1.,0.,0.));
#37578=DIRECTION('',(0.,-1.,0.));
#37579=DIRECTION('',(-1.,0.,0.));
#37580=DIRECTION('center_axis',(0.,1.,0.));
#37581=DIRECTION('ref_axis',(0.,0.,-1.));
#37582=DIRECTION('',(0.,0.,-1.));
#37583=DIRECTION('',(-1.,0.,0.));
#37584=DIRECTION('',(0.,0.,-1.));
#37585=DIRECTION('center_axis',(0.,0.,1.));
#37586=DIRECTION('ref_axis',(0.,1.,0.));
#37587=DIRECTION('',(0.,1.,0.));
#37588=DIRECTION('',(-1.,0.,0.));
#37589=DIRECTION('',(0.,1.,0.));
#37590=DIRECTION('center_axis',(0.,-1.,0.));
#37591=DIRECTION('ref_axis',(0.,0.,1.));
#37592=DIRECTION('',(0.,0.,1.));
#37593=DIRECTION('',(0.,0.,1.));
#37594=DIRECTION('center_axis',(-1.,0.,0.));
#37595=DIRECTION('ref_axis',(0.,0.,1.));
#37596=DIRECTION('center_axis',(0.,0.,-1.));
#37597=DIRECTION('ref_axis',(0.,-1.,0.));
#37598=DIRECTION('',(0.,-1.,0.));
#37599=DIRECTION('',(-1.,0.,0.));
#37600=DIRECTION('',(0.,-1.,0.));
#37601=DIRECTION('',(-1.,0.,0.));
#37602=DIRECTION('center_axis',(0.,1.,0.));
#37603=DIRECTION('ref_axis',(0.,0.,-1.));
#37604=DIRECTION('',(0.,0.,-1.));
#37605=DIRECTION('',(-1.,0.,0.));
#37606=DIRECTION('',(0.,0.,-1.));
#37607=DIRECTION('center_axis',(0.,0.,1.));
#37608=DIRECTION('ref_axis',(0.,1.,0.));
#37609=DIRECTION('',(0.,1.,0.));
#37610=DIRECTION('',(-1.,0.,0.));
#37611=DIRECTION('',(0.,1.,0.));
#37612=DIRECTION('center_axis',(0.,-1.,0.));
#37613=DIRECTION('ref_axis',(0.,0.,1.));
#37614=DIRECTION('',(0.,0.,1.));
#37615=DIRECTION('',(0.,0.,1.));
#37616=DIRECTION('center_axis',(-1.,0.,0.));
#37617=DIRECTION('ref_axis',(0.,0.,1.));
#37618=DIRECTION('center_axis',(0.,0.,-1.));
#37619=DIRECTION('ref_axis',(0.,-1.,0.));
#37620=DIRECTION('',(0.,-1.,0.));
#37621=DIRECTION('',(-1.,0.,0.));
#37622=DIRECTION('',(0.,-1.,0.));
#37623=DIRECTION('',(-1.,0.,0.));
#37624=DIRECTION('center_axis',(0.,1.,0.));
#37625=DIRECTION('ref_axis',(0.,0.,-1.));
#37626=DIRECTION('',(0.,0.,-1.));
#37627=DIRECTION('',(-1.,0.,0.));
#37628=DIRECTION('',(0.,0.,-1.));
#37629=DIRECTION('center_axis',(0.,0.,1.));
#37630=DIRECTION('ref_axis',(0.,1.,0.));
#37631=DIRECTION('',(0.,1.,0.));
#37632=DIRECTION('',(-1.,0.,0.));
#37633=DIRECTION('',(0.,1.,0.));
#37634=DIRECTION('center_axis',(0.,-1.,0.));
#37635=DIRECTION('ref_axis',(0.,0.,1.));
#37636=DIRECTION('',(0.,0.,1.));
#37637=DIRECTION('',(0.,0.,1.));
#37638=DIRECTION('center_axis',(-1.,0.,0.));
#37639=DIRECTION('ref_axis',(0.,0.,1.));
#37640=DIRECTION('center_axis',(0.,0.,-1.));
#37641=DIRECTION('ref_axis',(0.,-1.,0.));
#37642=DIRECTION('',(0.,-1.,0.));
#37643=DIRECTION('',(-1.,0.,0.));
#37644=DIRECTION('',(0.,-1.,0.));
#37645=DIRECTION('',(-1.,0.,0.));
#37646=DIRECTION('center_axis',(0.,1.,0.));
#37647=DIRECTION('ref_axis',(0.,0.,-1.));
#37648=DIRECTION('',(0.,0.,-1.));
#37649=DIRECTION('',(-1.,0.,0.));
#37650=DIRECTION('',(0.,0.,-1.));
#37651=DIRECTION('center_axis',(0.,0.,1.));
#37652=DIRECTION('ref_axis',(0.,1.,0.));
#37653=DIRECTION('',(0.,1.,0.));
#37654=DIRECTION('',(-1.,0.,0.));
#37655=DIRECTION('',(0.,1.,0.));
#37656=DIRECTION('center_axis',(0.,-1.,0.));
#37657=DIRECTION('ref_axis',(0.,0.,1.));
#37658=DIRECTION('',(0.,0.,1.));
#37659=DIRECTION('',(0.,0.,1.));
#37660=DIRECTION('center_axis',(-1.,0.,0.));
#37661=DIRECTION('ref_axis',(0.,0.,1.));
#37662=DIRECTION('center_axis',(0.,0.,-1.));
#37663=DIRECTION('ref_axis',(0.,-1.,0.));
#37664=DIRECTION('',(0.,-1.,0.));
#37665=DIRECTION('',(-1.,0.,0.));
#37666=DIRECTION('',(0.,-1.,0.));
#37667=DIRECTION('',(-1.,0.,0.));
#37668=DIRECTION('center_axis',(0.,1.,0.));
#37669=DIRECTION('ref_axis',(0.,0.,-1.));
#37670=DIRECTION('',(0.,0.,-1.));
#37671=DIRECTION('',(-1.,0.,0.));
#37672=DIRECTION('',(0.,0.,-1.));
#37673=DIRECTION('center_axis',(0.,0.,1.));
#37674=DIRECTION('ref_axis',(0.,1.,0.));
#37675=DIRECTION('',(0.,1.,0.));
#37676=DIRECTION('',(-1.,0.,0.));
#37677=DIRECTION('',(0.,1.,0.));
#37678=DIRECTION('center_axis',(0.,-1.,0.));
#37679=DIRECTION('ref_axis',(0.,0.,1.));
#37680=DIRECTION('',(0.,0.,1.));
#37681=DIRECTION('',(0.,0.,1.));
#37682=DIRECTION('center_axis',(-1.,0.,0.));
#37683=DIRECTION('ref_axis',(0.,0.,1.));
#37684=DIRECTION('center_axis',(0.,0.,-1.));
#37685=DIRECTION('ref_axis',(0.,-1.,0.));
#37686=DIRECTION('',(0.,-1.,0.));
#37687=DIRECTION('',(-1.,0.,0.));
#37688=DIRECTION('',(0.,-1.,0.));
#37689=DIRECTION('',(-1.,0.,0.));
#37690=DIRECTION('center_axis',(0.,1.,0.));
#37691=DIRECTION('ref_axis',(0.,0.,-1.));
#37692=DIRECTION('',(0.,0.,-1.));
#37693=DIRECTION('',(-1.,0.,0.));
#37694=DIRECTION('',(0.,0.,-1.));
#37695=DIRECTION('center_axis',(0.,0.,1.));
#37696=DIRECTION('ref_axis',(0.,1.,0.));
#37697=DIRECTION('',(0.,1.,0.));
#37698=DIRECTION('',(-1.,0.,0.));
#37699=DIRECTION('',(0.,1.,0.));
#37700=DIRECTION('center_axis',(0.,-1.,0.));
#37701=DIRECTION('ref_axis',(0.,0.,1.));
#37702=DIRECTION('',(0.,0.,1.));
#37703=DIRECTION('',(0.,0.,1.));
#37704=DIRECTION('center_axis',(-1.,0.,0.));
#37705=DIRECTION('ref_axis',(0.,0.,1.));
#37706=DIRECTION('center_axis',(0.,0.,-1.));
#37707=DIRECTION('ref_axis',(0.,-1.,0.));
#37708=DIRECTION('',(0.,-1.,0.));
#37709=DIRECTION('',(-1.,0.,0.));
#37710=DIRECTION('',(0.,-1.,0.));
#37711=DIRECTION('',(-1.,0.,0.));
#37712=DIRECTION('center_axis',(0.,1.,0.));
#37713=DIRECTION('ref_axis',(0.,0.,-1.));
#37714=DIRECTION('',(0.,0.,-1.));
#37715=DIRECTION('',(-1.,0.,0.));
#37716=DIRECTION('',(0.,0.,-1.));
#37717=DIRECTION('center_axis',(0.,0.,1.));
#37718=DIRECTION('ref_axis',(0.,1.,0.));
#37719=DIRECTION('',(0.,1.,0.));
#37720=DIRECTION('',(-1.,0.,0.));
#37721=DIRECTION('',(0.,1.,0.));
#37722=DIRECTION('center_axis',(0.,-1.,0.));
#37723=DIRECTION('ref_axis',(0.,0.,1.));
#37724=DIRECTION('',(0.,0.,1.));
#37725=DIRECTION('',(0.,0.,1.));
#37726=DIRECTION('center_axis',(-1.,0.,0.));
#37727=DIRECTION('ref_axis',(0.,0.,1.));
#37728=DIRECTION('center_axis',(0.,0.,-1.));
#37729=DIRECTION('ref_axis',(0.,-1.,0.));
#37730=DIRECTION('',(0.,-1.,0.));
#37731=DIRECTION('',(-1.,0.,0.));
#37732=DIRECTION('',(0.,-1.,0.));
#37733=DIRECTION('',(-1.,0.,0.));
#37734=DIRECTION('center_axis',(0.,1.,0.));
#37735=DIRECTION('ref_axis',(0.,0.,-1.));
#37736=DIRECTION('',(0.,0.,-1.));
#37737=DIRECTION('',(-1.,0.,0.));
#37738=DIRECTION('',(0.,0.,-1.));
#37739=DIRECTION('center_axis',(0.,0.,1.));
#37740=DIRECTION('ref_axis',(0.,1.,0.));
#37741=DIRECTION('',(0.,1.,0.));
#37742=DIRECTION('',(-1.,0.,0.));
#37743=DIRECTION('',(0.,1.,0.));
#37744=DIRECTION('center_axis',(0.,-1.,0.));
#37745=DIRECTION('ref_axis',(0.,0.,1.));
#37746=DIRECTION('',(0.,0.,1.));
#37747=DIRECTION('',(0.,0.,1.));
#37748=DIRECTION('center_axis',(-1.,0.,0.));
#37749=DIRECTION('ref_axis',(0.,0.,1.));
#37750=DIRECTION('center_axis',(0.,0.,-1.));
#37751=DIRECTION('ref_axis',(0.,-1.,0.));
#37752=DIRECTION('',(0.,-1.,0.));
#37753=DIRECTION('',(-1.,0.,0.));
#37754=DIRECTION('',(0.,-1.,0.));
#37755=DIRECTION('',(-1.,0.,0.));
#37756=DIRECTION('center_axis',(0.,1.,0.));
#37757=DIRECTION('ref_axis',(0.,0.,-1.));
#37758=DIRECTION('',(0.,0.,-1.));
#37759=DIRECTION('',(-1.,0.,0.));
#37760=DIRECTION('',(0.,0.,-1.));
#37761=DIRECTION('center_axis',(0.,0.,1.));
#37762=DIRECTION('ref_axis',(0.,1.,0.));
#37763=DIRECTION('',(0.,1.,0.));
#37764=DIRECTION('',(-1.,0.,0.));
#37765=DIRECTION('',(0.,1.,0.));
#37766=DIRECTION('center_axis',(0.,-1.,0.));
#37767=DIRECTION('ref_axis',(0.,0.,1.));
#37768=DIRECTION('',(0.,0.,1.));
#37769=DIRECTION('',(0.,0.,1.));
#37770=DIRECTION('center_axis',(-1.,0.,0.));
#37771=DIRECTION('ref_axis',(0.,0.,1.));
#37772=DIRECTION('center_axis',(0.,0.,-1.));
#37773=DIRECTION('ref_axis',(0.,-1.,0.));
#37774=DIRECTION('',(0.,-1.,0.));
#37775=DIRECTION('',(-1.,0.,0.));
#37776=DIRECTION('',(0.,-1.,0.));
#37777=DIRECTION('',(-1.,0.,0.));
#37778=DIRECTION('center_axis',(0.,1.,0.));
#37779=DIRECTION('ref_axis',(0.,0.,-1.));
#37780=DIRECTION('',(0.,0.,-1.));
#37781=DIRECTION('',(-1.,0.,0.));
#37782=DIRECTION('',(0.,0.,-1.));
#37783=DIRECTION('center_axis',(0.,0.,1.));
#37784=DIRECTION('ref_axis',(0.,1.,0.));
#37785=DIRECTION('',(0.,1.,0.));
#37786=DIRECTION('',(-1.,0.,0.));
#37787=DIRECTION('',(0.,1.,0.));
#37788=DIRECTION('center_axis',(0.,-1.,0.));
#37789=DIRECTION('ref_axis',(0.,0.,1.));
#37790=DIRECTION('',(0.,0.,1.));
#37791=DIRECTION('',(0.,0.,1.));
#37792=DIRECTION('center_axis',(-1.,0.,0.));
#37793=DIRECTION('ref_axis',(0.,0.,1.));
#37794=DIRECTION('center_axis',(0.,0.,-1.));
#37795=DIRECTION('ref_axis',(0.,-1.,0.));
#37796=DIRECTION('',(0.,-1.,0.));
#37797=DIRECTION('',(-1.,0.,0.));
#37798=DIRECTION('',(0.,-1.,0.));
#37799=DIRECTION('',(-1.,0.,0.));
#37800=DIRECTION('center_axis',(0.,1.,0.));
#37801=DIRECTION('ref_axis',(0.,0.,-1.));
#37802=DIRECTION('',(0.,0.,-1.));
#37803=DIRECTION('',(-1.,0.,0.));
#37804=DIRECTION('',(0.,0.,-1.));
#37805=DIRECTION('center_axis',(0.,0.,1.));
#37806=DIRECTION('ref_axis',(0.,1.,0.));
#37807=DIRECTION('',(0.,1.,0.));
#37808=DIRECTION('',(-1.,0.,0.));
#37809=DIRECTION('',(0.,1.,0.));
#37810=DIRECTION('center_axis',(0.,-1.,0.));
#37811=DIRECTION('ref_axis',(0.,0.,1.));
#37812=DIRECTION('',(0.,0.,1.));
#37813=DIRECTION('',(0.,0.,1.));
#37814=DIRECTION('center_axis',(-1.,0.,0.));
#37815=DIRECTION('ref_axis',(0.,0.,1.));
#37816=DIRECTION('center_axis',(0.,0.,-1.));
#37817=DIRECTION('ref_axis',(0.,-1.,0.));
#37818=DIRECTION('',(0.,-1.,0.));
#37819=DIRECTION('',(-1.,0.,0.));
#37820=DIRECTION('',(0.,-1.,0.));
#37821=DIRECTION('',(-1.,0.,0.));
#37822=DIRECTION('center_axis',(0.,1.,0.));
#37823=DIRECTION('ref_axis',(0.,0.,-1.));
#37824=DIRECTION('',(0.,0.,-1.));
#37825=DIRECTION('',(-1.,0.,0.));
#37826=DIRECTION('',(0.,0.,-1.));
#37827=DIRECTION('center_axis',(0.,0.,1.));
#37828=DIRECTION('ref_axis',(0.,1.,0.));
#37829=DIRECTION('',(0.,1.,0.));
#37830=DIRECTION('',(-1.,0.,0.));
#37831=DIRECTION('',(0.,1.,0.));
#37832=DIRECTION('center_axis',(0.,-1.,0.));
#37833=DIRECTION('ref_axis',(0.,0.,1.));
#37834=DIRECTION('',(0.,0.,1.));
#37835=DIRECTION('',(0.,0.,1.));
#37836=DIRECTION('center_axis',(-1.,0.,0.));
#37837=DIRECTION('ref_axis',(0.,0.,1.));
#37838=DIRECTION('center_axis',(0.,0.,-1.));
#37839=DIRECTION('ref_axis',(0.,-1.,0.));
#37840=DIRECTION('',(0.,-1.,0.));
#37841=DIRECTION('',(-1.,0.,0.));
#37842=DIRECTION('',(0.,-1.,0.));
#37843=DIRECTION('',(-1.,0.,0.));
#37844=DIRECTION('center_axis',(0.,1.,0.));
#37845=DIRECTION('ref_axis',(0.,0.,-1.));
#37846=DIRECTION('',(0.,0.,-1.));
#37847=DIRECTION('',(-1.,0.,0.));
#37848=DIRECTION('',(0.,0.,-1.));
#37849=DIRECTION('center_axis',(0.,0.,1.));
#37850=DIRECTION('ref_axis',(0.,1.,0.));
#37851=DIRECTION('',(0.,1.,0.));
#37852=DIRECTION('',(-1.,0.,0.));
#37853=DIRECTION('',(0.,1.,0.));
#37854=DIRECTION('center_axis',(0.,-1.,0.));
#37855=DIRECTION('ref_axis',(0.,0.,1.));
#37856=DIRECTION('',(0.,0.,1.));
#37857=DIRECTION('',(0.,0.,1.));
#37858=DIRECTION('center_axis',(-1.,0.,0.));
#37859=DIRECTION('ref_axis',(0.,0.,1.));
#37860=DIRECTION('center_axis',(0.,0.,-1.));
#37861=DIRECTION('ref_axis',(0.,-1.,0.));
#37862=DIRECTION('',(0.,-1.,0.));
#37863=DIRECTION('',(-1.,0.,0.));
#37864=DIRECTION('',(0.,-1.,0.));
#37865=DIRECTION('',(-1.,0.,0.));
#37866=DIRECTION('center_axis',(0.,1.,0.));
#37867=DIRECTION('ref_axis',(0.,0.,-1.));
#37868=DIRECTION('',(0.,0.,-1.));
#37869=DIRECTION('',(-1.,0.,0.));
#37870=DIRECTION('',(0.,0.,-1.));
#37871=DIRECTION('center_axis',(0.,0.,1.));
#37872=DIRECTION('ref_axis',(0.,1.,0.));
#37873=DIRECTION('',(0.,1.,0.));
#37874=DIRECTION('',(-1.,0.,0.));
#37875=DIRECTION('',(0.,1.,0.));
#37876=DIRECTION('center_axis',(0.,-1.,0.));
#37877=DIRECTION('ref_axis',(0.,0.,1.));
#37878=DIRECTION('',(0.,0.,1.));
#37879=DIRECTION('',(0.,0.,1.));
#37880=DIRECTION('center_axis',(-1.,0.,0.));
#37881=DIRECTION('ref_axis',(0.,0.,1.));
#37882=DIRECTION('center_axis',(0.,0.,-1.));
#37883=DIRECTION('ref_axis',(0.,-1.,0.));
#37884=DIRECTION('',(0.,-1.,0.));
#37885=DIRECTION('',(-1.,0.,0.));
#37886=DIRECTION('',(0.,-1.,0.));
#37887=DIRECTION('',(-1.,0.,0.));
#37888=DIRECTION('center_axis',(0.,1.,0.));
#37889=DIRECTION('ref_axis',(0.,0.,-1.));
#37890=DIRECTION('',(0.,0.,-1.));
#37891=DIRECTION('',(-1.,0.,0.));
#37892=DIRECTION('',(0.,0.,-1.));
#37893=DIRECTION('center_axis',(0.,0.,1.));
#37894=DIRECTION('ref_axis',(0.,1.,0.));
#37895=DIRECTION('',(0.,1.,0.));
#37896=DIRECTION('',(-1.,0.,0.));
#37897=DIRECTION('',(0.,1.,0.));
#37898=DIRECTION('center_axis',(0.,-1.,0.));
#37899=DIRECTION('ref_axis',(0.,0.,1.));
#37900=DIRECTION('',(0.,0.,1.));
#37901=DIRECTION('',(0.,0.,1.));
#37902=DIRECTION('center_axis',(-1.,0.,0.));
#37903=DIRECTION('ref_axis',(0.,0.,1.));
#37904=DIRECTION('center_axis',(0.,0.,-1.));
#37905=DIRECTION('ref_axis',(0.,-1.,0.));
#37906=DIRECTION('',(0.,-1.,0.));
#37907=DIRECTION('',(-1.,0.,0.));
#37908=DIRECTION('',(0.,-1.,0.));
#37909=DIRECTION('',(-1.,0.,0.));
#37910=DIRECTION('center_axis',(0.,1.,0.));
#37911=DIRECTION('ref_axis',(0.,0.,-1.));
#37912=DIRECTION('',(0.,0.,-1.));
#37913=DIRECTION('',(-1.,0.,0.));
#37914=DIRECTION('',(0.,0.,-1.));
#37915=DIRECTION('center_axis',(0.,0.,1.));
#37916=DIRECTION('ref_axis',(0.,1.,0.));
#37917=DIRECTION('',(0.,1.,0.));
#37918=DIRECTION('',(-1.,0.,0.));
#37919=DIRECTION('',(0.,1.,0.));
#37920=DIRECTION('center_axis',(0.,-1.,0.));
#37921=DIRECTION('ref_axis',(0.,0.,1.));
#37922=DIRECTION('',(0.,0.,1.));
#37923=DIRECTION('',(0.,0.,1.));
#37924=DIRECTION('center_axis',(-1.,0.,0.));
#37925=DIRECTION('ref_axis',(0.,0.,1.));
#37926=DIRECTION('center_axis',(0.,0.,-1.));
#37927=DIRECTION('ref_axis',(0.,-1.,0.));
#37928=DIRECTION('',(0.,-1.,0.));
#37929=DIRECTION('',(-1.,0.,0.));
#37930=DIRECTION('',(0.,-1.,0.));
#37931=DIRECTION('',(-1.,0.,0.));
#37932=DIRECTION('center_axis',(0.,1.,0.));
#37933=DIRECTION('ref_axis',(0.,0.,-1.));
#37934=DIRECTION('',(0.,0.,-1.));
#37935=DIRECTION('',(-1.,0.,0.));
#37936=DIRECTION('',(0.,0.,-1.));
#37937=DIRECTION('center_axis',(0.,0.,1.));
#37938=DIRECTION('ref_axis',(0.,1.,0.));
#37939=DIRECTION('',(0.,1.,0.));
#37940=DIRECTION('',(-1.,0.,0.));
#37941=DIRECTION('',(0.,1.,0.));
#37942=DIRECTION('center_axis',(0.,-1.,0.));
#37943=DIRECTION('ref_axis',(0.,0.,1.));
#37944=DIRECTION('',(0.,0.,1.));
#37945=DIRECTION('',(0.,0.,1.));
#37946=DIRECTION('center_axis',(-1.,0.,0.));
#37947=DIRECTION('ref_axis',(0.,0.,1.));
#37948=DIRECTION('center_axis',(0.,0.,-1.));
#37949=DIRECTION('ref_axis',(0.,-1.,0.));
#37950=DIRECTION('',(0.,-1.,0.));
#37951=DIRECTION('',(-1.,0.,0.));
#37952=DIRECTION('',(0.,-1.,0.));
#37953=DIRECTION('',(-1.,0.,0.));
#37954=DIRECTION('center_axis',(0.,1.,0.));
#37955=DIRECTION('ref_axis',(0.,0.,-1.));
#37956=DIRECTION('',(0.,0.,-1.));
#37957=DIRECTION('',(-1.,0.,0.));
#37958=DIRECTION('',(0.,0.,-1.));
#37959=DIRECTION('center_axis',(0.,0.,1.));
#37960=DIRECTION('ref_axis',(0.,1.,0.));
#37961=DIRECTION('',(0.,1.,0.));
#37962=DIRECTION('',(-1.,0.,0.));
#37963=DIRECTION('',(0.,1.,0.));
#37964=DIRECTION('center_axis',(0.,-1.,0.));
#37965=DIRECTION('ref_axis',(0.,0.,1.));
#37966=DIRECTION('',(0.,0.,1.));
#37967=DIRECTION('',(0.,0.,1.));
#37968=DIRECTION('center_axis',(-1.,0.,0.));
#37969=DIRECTION('ref_axis',(0.,0.,1.));
#37970=DIRECTION('center_axis',(0.,0.,-1.));
#37971=DIRECTION('ref_axis',(0.,-1.,0.));
#37972=DIRECTION('',(0.,-1.,0.));
#37973=DIRECTION('',(-1.,0.,0.));
#37974=DIRECTION('',(0.,-1.,0.));
#37975=DIRECTION('',(-1.,0.,0.));
#37976=DIRECTION('center_axis',(0.,1.,0.));
#37977=DIRECTION('ref_axis',(0.,0.,-1.));
#37978=DIRECTION('',(0.,0.,-1.));
#37979=DIRECTION('',(-1.,0.,0.));
#37980=DIRECTION('',(0.,0.,-1.));
#37981=DIRECTION('center_axis',(0.,0.,1.));
#37982=DIRECTION('ref_axis',(0.,1.,0.));
#37983=DIRECTION('',(0.,1.,0.));
#37984=DIRECTION('',(-1.,0.,0.));
#37985=DIRECTION('',(0.,1.,0.));
#37986=DIRECTION('center_axis',(0.,-1.,0.));
#37987=DIRECTION('ref_axis',(0.,0.,1.));
#37988=DIRECTION('',(0.,0.,1.));
#37989=DIRECTION('',(0.,0.,1.));
#37990=DIRECTION('center_axis',(-1.,0.,0.));
#37991=DIRECTION('ref_axis',(0.,0.,1.));
#37992=DIRECTION('center_axis',(0.,0.,-1.));
#37993=DIRECTION('ref_axis',(0.,-1.,0.));
#37994=DIRECTION('',(0.,-1.,0.));
#37995=DIRECTION('',(-1.,0.,0.));
#37996=DIRECTION('',(0.,-1.,0.));
#37997=DIRECTION('',(-1.,0.,0.));
#37998=DIRECTION('center_axis',(0.,1.,0.));
#37999=DIRECTION('ref_axis',(0.,0.,-1.));
#38000=DIRECTION('',(0.,0.,-1.));
#38001=DIRECTION('',(-1.,0.,0.));
#38002=DIRECTION('',(0.,0.,-1.));
#38003=DIRECTION('center_axis',(0.,0.,1.));
#38004=DIRECTION('ref_axis',(0.,1.,0.));
#38005=DIRECTION('',(0.,1.,0.));
#38006=DIRECTION('',(-1.,0.,0.));
#38007=DIRECTION('',(0.,1.,0.));
#38008=DIRECTION('center_axis',(0.,-1.,0.));
#38009=DIRECTION('ref_axis',(0.,0.,1.));
#38010=DIRECTION('',(0.,0.,1.));
#38011=DIRECTION('',(0.,0.,1.));
#38012=DIRECTION('center_axis',(-1.,0.,0.));
#38013=DIRECTION('ref_axis',(0.,0.,1.));
#38014=DIRECTION('center_axis',(0.,0.,-1.));
#38015=DIRECTION('ref_axis',(0.,-1.,0.));
#38016=DIRECTION('',(0.,-1.,0.));
#38017=DIRECTION('',(-1.,0.,0.));
#38018=DIRECTION('',(0.,-1.,0.));
#38019=DIRECTION('',(-1.,0.,0.));
#38020=DIRECTION('center_axis',(0.,1.,0.));
#38021=DIRECTION('ref_axis',(0.,0.,-1.));
#38022=DIRECTION('',(0.,0.,-1.));
#38023=DIRECTION('',(-1.,0.,0.));
#38024=DIRECTION('',(0.,0.,-1.));
#38025=DIRECTION('center_axis',(0.,0.,1.));
#38026=DIRECTION('ref_axis',(0.,1.,0.));
#38027=DIRECTION('',(0.,1.,0.));
#38028=DIRECTION('',(-1.,0.,0.));
#38029=DIRECTION('',(0.,1.,0.));
#38030=DIRECTION('center_axis',(0.,-1.,0.));
#38031=DIRECTION('ref_axis',(0.,0.,1.));
#38032=DIRECTION('',(0.,0.,1.));
#38033=DIRECTION('',(0.,0.,1.));
#38034=DIRECTION('center_axis',(-1.,0.,0.));
#38035=DIRECTION('ref_axis',(0.,0.,1.));
#38036=DIRECTION('center_axis',(0.,0.,-1.));
#38037=DIRECTION('ref_axis',(0.,-1.,0.));
#38038=DIRECTION('',(0.,-1.,0.));
#38039=DIRECTION('',(-1.,0.,0.));
#38040=DIRECTION('',(0.,-1.,0.));
#38041=DIRECTION('',(-1.,0.,0.));
#38042=DIRECTION('center_axis',(0.,1.,0.));
#38043=DIRECTION('ref_axis',(0.,0.,-1.));
#38044=DIRECTION('',(0.,0.,-1.));
#38045=DIRECTION('',(-1.,0.,0.));
#38046=DIRECTION('',(0.,0.,-1.));
#38047=DIRECTION('center_axis',(0.,0.,1.));
#38048=DIRECTION('ref_axis',(0.,1.,0.));
#38049=DIRECTION('',(0.,1.,0.));
#38050=DIRECTION('',(-1.,0.,0.));
#38051=DIRECTION('',(0.,1.,0.));
#38052=DIRECTION('center_axis',(0.,-1.,0.));
#38053=DIRECTION('ref_axis',(0.,0.,1.));
#38054=DIRECTION('',(0.,0.,1.));
#38055=DIRECTION('',(0.,0.,1.));
#38056=DIRECTION('center_axis',(-1.,0.,0.));
#38057=DIRECTION('ref_axis',(0.,0.,1.));
#38058=DIRECTION('center_axis',(0.,0.,-1.));
#38059=DIRECTION('ref_axis',(0.,-1.,0.));
#38060=DIRECTION('',(0.,-1.,0.));
#38061=DIRECTION('',(-1.,0.,0.));
#38062=DIRECTION('',(0.,-1.,0.));
#38063=DIRECTION('',(-1.,0.,0.));
#38064=DIRECTION('center_axis',(0.,1.,0.));
#38065=DIRECTION('ref_axis',(0.,0.,-1.));
#38066=DIRECTION('',(0.,0.,-1.));
#38067=DIRECTION('',(-1.,0.,0.));
#38068=DIRECTION('',(0.,0.,-1.));
#38069=DIRECTION('center_axis',(0.,0.,1.));
#38070=DIRECTION('ref_axis',(0.,1.,0.));
#38071=DIRECTION('',(0.,1.,0.));
#38072=DIRECTION('',(-1.,0.,0.));
#38073=DIRECTION('',(0.,1.,0.));
#38074=DIRECTION('center_axis',(0.,-1.,0.));
#38075=DIRECTION('ref_axis',(0.,0.,1.));
#38076=DIRECTION('',(0.,0.,1.));
#38077=DIRECTION('',(0.,0.,1.));
#38078=DIRECTION('center_axis',(-1.,0.,0.));
#38079=DIRECTION('ref_axis',(0.,0.,1.));
#38080=DIRECTION('center_axis',(0.,0.,-1.));
#38081=DIRECTION('ref_axis',(0.,-1.,0.));
#38082=DIRECTION('',(0.,-1.,0.));
#38083=DIRECTION('',(-1.,0.,0.));
#38084=DIRECTION('',(0.,-1.,0.));
#38085=DIRECTION('',(-1.,0.,0.));
#38086=DIRECTION('center_axis',(0.,1.,0.));
#38087=DIRECTION('ref_axis',(0.,0.,-1.));
#38088=DIRECTION('',(0.,0.,-1.));
#38089=DIRECTION('',(-1.,0.,0.));
#38090=DIRECTION('',(0.,0.,-1.));
#38091=DIRECTION('center_axis',(0.,0.,1.));
#38092=DIRECTION('ref_axis',(0.,1.,0.));
#38093=DIRECTION('',(0.,1.,0.));
#38094=DIRECTION('',(-1.,0.,0.));
#38095=DIRECTION('',(0.,1.,0.));
#38096=DIRECTION('center_axis',(0.,-1.,0.));
#38097=DIRECTION('ref_axis',(0.,0.,1.));
#38098=DIRECTION('',(0.,0.,1.));
#38099=DIRECTION('',(0.,0.,1.));
#38100=DIRECTION('center_axis',(-1.,0.,0.));
#38101=DIRECTION('ref_axis',(0.,0.,1.));
#38102=DIRECTION('center_axis',(0.,0.,-1.));
#38103=DIRECTION('ref_axis',(0.,-1.,0.));
#38104=DIRECTION('',(0.,-1.,0.));
#38105=DIRECTION('',(-1.,0.,0.));
#38106=DIRECTION('',(0.,-1.,0.));
#38107=DIRECTION('',(-1.,0.,0.));
#38108=DIRECTION('center_axis',(0.,1.,0.));
#38109=DIRECTION('ref_axis',(0.,0.,-1.));
#38110=DIRECTION('',(0.,0.,-1.));
#38111=DIRECTION('',(-1.,0.,0.));
#38112=DIRECTION('',(0.,0.,-1.));
#38113=DIRECTION('center_axis',(0.,0.,1.));
#38114=DIRECTION('ref_axis',(0.,1.,0.));
#38115=DIRECTION('',(0.,1.,0.));
#38116=DIRECTION('',(-1.,0.,0.));
#38117=DIRECTION('',(0.,1.,0.));
#38118=DIRECTION('center_axis',(0.,-1.,0.));
#38119=DIRECTION('ref_axis',(0.,0.,1.));
#38120=DIRECTION('',(0.,0.,1.));
#38121=DIRECTION('',(0.,0.,1.));
#38122=DIRECTION('center_axis',(-1.,0.,0.));
#38123=DIRECTION('ref_axis',(0.,0.,1.));
#38124=DIRECTION('center_axis',(0.,0.,-1.));
#38125=DIRECTION('ref_axis',(0.,-1.,0.));
#38126=DIRECTION('',(0.,-1.,0.));
#38127=DIRECTION('',(-1.,0.,0.));
#38128=DIRECTION('',(0.,-1.,0.));
#38129=DIRECTION('',(-1.,0.,0.));
#38130=DIRECTION('center_axis',(0.,1.,0.));
#38131=DIRECTION('ref_axis',(0.,0.,-1.));
#38132=DIRECTION('',(0.,0.,-1.));
#38133=DIRECTION('',(-1.,0.,0.));
#38134=DIRECTION('',(0.,0.,-1.));
#38135=DIRECTION('center_axis',(0.,0.,1.));
#38136=DIRECTION('ref_axis',(0.,1.,0.));
#38137=DIRECTION('',(0.,1.,0.));
#38138=DIRECTION('',(-1.,0.,0.));
#38139=DIRECTION('',(0.,1.,0.));
#38140=DIRECTION('center_axis',(0.,-1.,0.));
#38141=DIRECTION('ref_axis',(0.,0.,1.));
#38142=DIRECTION('',(0.,0.,1.));
#38143=DIRECTION('',(0.,0.,1.));
#38144=DIRECTION('center_axis',(-1.,0.,0.));
#38145=DIRECTION('ref_axis',(0.,0.,1.));
#38146=DIRECTION('center_axis',(0.,0.,-1.));
#38147=DIRECTION('ref_axis',(0.,-1.,0.));
#38148=DIRECTION('',(0.,-1.,0.));
#38149=DIRECTION('',(-1.,0.,0.));
#38150=DIRECTION('',(0.,-1.,0.));
#38151=DIRECTION('',(-1.,0.,0.));
#38152=DIRECTION('center_axis',(0.,1.,0.));
#38153=DIRECTION('ref_axis',(0.,0.,-1.));
#38154=DIRECTION('',(0.,0.,-1.));
#38155=DIRECTION('',(-1.,0.,0.));
#38156=DIRECTION('',(0.,0.,-1.));
#38157=DIRECTION('center_axis',(0.,0.,1.));
#38158=DIRECTION('ref_axis',(0.,1.,0.));
#38159=DIRECTION('',(0.,1.,0.));
#38160=DIRECTION('',(-1.,0.,0.));
#38161=DIRECTION('',(0.,1.,0.));
#38162=DIRECTION('center_axis',(0.,-1.,0.));
#38163=DIRECTION('ref_axis',(0.,0.,1.));
#38164=DIRECTION('',(0.,0.,1.));
#38165=DIRECTION('',(0.,0.,1.));
#38166=DIRECTION('center_axis',(-1.,0.,0.));
#38167=DIRECTION('ref_axis',(0.,0.,1.));
#38168=DIRECTION('center_axis',(0.,0.,-1.));
#38169=DIRECTION('ref_axis',(0.,-1.,0.));
#38170=DIRECTION('',(0.,-1.,0.));
#38171=DIRECTION('',(-1.,0.,0.));
#38172=DIRECTION('',(0.,-1.,0.));
#38173=DIRECTION('',(-1.,0.,0.));
#38174=DIRECTION('center_axis',(0.,1.,0.));
#38175=DIRECTION('ref_axis',(0.,0.,-1.));
#38176=DIRECTION('',(0.,0.,-1.));
#38177=DIRECTION('',(-1.,0.,0.));
#38178=DIRECTION('',(0.,0.,-1.));
#38179=DIRECTION('center_axis',(0.,0.,1.));
#38180=DIRECTION('ref_axis',(0.,1.,0.));
#38181=DIRECTION('',(0.,1.,0.));
#38182=DIRECTION('',(-1.,0.,0.));
#38183=DIRECTION('',(0.,1.,0.));
#38184=DIRECTION('center_axis',(0.,-1.,0.));
#38185=DIRECTION('ref_axis',(0.,0.,1.));
#38186=DIRECTION('',(0.,0.,1.));
#38187=DIRECTION('',(0.,0.,1.));
#38188=DIRECTION('center_axis',(-1.,0.,0.));
#38189=DIRECTION('ref_axis',(0.,0.,1.));
#38190=DIRECTION('center_axis',(0.,0.,-1.));
#38191=DIRECTION('ref_axis',(0.,-1.,0.));
#38192=DIRECTION('',(0.,-1.,0.));
#38193=DIRECTION('',(-1.,0.,0.));
#38194=DIRECTION('',(0.,-1.,0.));
#38195=DIRECTION('',(-1.,0.,0.));
#38196=DIRECTION('center_axis',(0.,1.,0.));
#38197=DIRECTION('ref_axis',(0.,0.,-1.));
#38198=DIRECTION('',(0.,0.,-1.));
#38199=DIRECTION('',(-1.,0.,0.));
#38200=DIRECTION('',(0.,0.,-1.));
#38201=DIRECTION('center_axis',(0.,0.,1.));
#38202=DIRECTION('ref_axis',(0.,1.,0.));
#38203=DIRECTION('',(0.,1.,0.));
#38204=DIRECTION('',(-1.,0.,0.));
#38205=DIRECTION('',(0.,1.,0.));
#38206=DIRECTION('center_axis',(0.,-1.,0.));
#38207=DIRECTION('ref_axis',(0.,0.,1.));
#38208=DIRECTION('',(0.,0.,1.));
#38209=DIRECTION('',(0.,0.,1.));
#38210=DIRECTION('center_axis',(-1.,0.,0.));
#38211=DIRECTION('ref_axis',(0.,0.,1.));
#38212=DIRECTION('center_axis',(0.,0.,-1.));
#38213=DIRECTION('ref_axis',(0.,-1.,0.));
#38214=DIRECTION('',(0.,-1.,0.));
#38215=DIRECTION('',(-1.,0.,0.));
#38216=DIRECTION('',(0.,-1.,0.));
#38217=DIRECTION('',(-1.,0.,0.));
#38218=DIRECTION('center_axis',(0.,1.,0.));
#38219=DIRECTION('ref_axis',(0.,0.,-1.));
#38220=DIRECTION('',(0.,0.,-1.));
#38221=DIRECTION('',(-1.,0.,0.));
#38222=DIRECTION('',(0.,0.,-1.));
#38223=DIRECTION('center_axis',(0.,0.,1.));
#38224=DIRECTION('ref_axis',(0.,1.,0.));
#38225=DIRECTION('',(0.,1.,0.));
#38226=DIRECTION('',(-1.,0.,0.));
#38227=DIRECTION('',(0.,1.,0.));
#38228=DIRECTION('center_axis',(0.,-1.,0.));
#38229=DIRECTION('ref_axis',(0.,0.,1.));
#38230=DIRECTION('',(0.,0.,1.));
#38231=DIRECTION('',(0.,0.,1.));
#38232=DIRECTION('center_axis',(-1.,0.,0.));
#38233=DIRECTION('ref_axis',(0.,0.,1.));
#38234=DIRECTION('center_axis',(0.,0.,-1.));
#38235=DIRECTION('ref_axis',(0.,-1.,0.));
#38236=DIRECTION('',(0.,-1.,0.));
#38237=DIRECTION('',(-1.,0.,0.));
#38238=DIRECTION('',(0.,-1.,0.));
#38239=DIRECTION('',(-1.,0.,0.));
#38240=DIRECTION('center_axis',(0.,1.,0.));
#38241=DIRECTION('ref_axis',(0.,0.,-1.));
#38242=DIRECTION('',(0.,0.,-1.));
#38243=DIRECTION('',(-1.,0.,0.));
#38244=DIRECTION('',(0.,0.,-1.));
#38245=DIRECTION('center_axis',(0.,0.,1.));
#38246=DIRECTION('ref_axis',(0.,1.,0.));
#38247=DIRECTION('',(0.,1.,0.));
#38248=DIRECTION('',(-1.,0.,0.));
#38249=DIRECTION('',(0.,1.,0.));
#38250=DIRECTION('center_axis',(0.,-1.,0.));
#38251=DIRECTION('ref_axis',(0.,0.,1.));
#38252=DIRECTION('',(0.,0.,1.));
#38253=DIRECTION('',(0.,0.,1.));
#38254=DIRECTION('center_axis',(-1.,0.,0.));
#38255=DIRECTION('ref_axis',(0.,0.,1.));
#38256=DIRECTION('center_axis',(1.,0.,0.));
#38257=DIRECTION('ref_axis',(0.,0.,-1.));
#38258=DIRECTION('center_axis',(1.,0.,0.));
#38259=DIRECTION('ref_axis',(0.,0.,-1.));
#38260=DIRECTION('',(1.,0.,0.));
#38261=DIRECTION('center_axis',(-1.,0.,0.));
#38262=DIRECTION('ref_axis',(0.,0.,-1.));
#38263=DIRECTION('center_axis',(1.,0.,0.));
#38264=DIRECTION('ref_axis',(0.,0.,-1.));
#38265=DIRECTION('center_axis',(1.,0.,0.));
#38266=DIRECTION('ref_axis',(0.,0.,-1.));
#38267=DIRECTION('',(1.,0.,0.));
#38268=DIRECTION('center_axis',(-1.,0.,0.));
#38269=DIRECTION('ref_axis',(0.,0.,-1.));
#38270=DIRECTION('center_axis',(0.,-1.,0.));
#38271=DIRECTION('ref_axis',(0.,0.,-1.));
#38272=DIRECTION('',(0.,0.,-1.));
#38273=DIRECTION('',(1.,0.,0.));
#38274=DIRECTION('',(0.,0.,-1.));
#38275=DIRECTION('',(1.,0.,0.));
#38276=DIRECTION('center_axis',(1.,0.,0.));
#38277=DIRECTION('ref_axis',(0.,2.7755575615629E-15,1.));
#38278=DIRECTION('center_axis',(1.,0.,0.));
#38279=DIRECTION('ref_axis',(0.,2.7755575615629E-15,1.));
#38280=DIRECTION('center_axis',(1.,0.,0.));
#38281=DIRECTION('ref_axis',(0.,2.7755575615629E-15,1.));
#38282=DIRECTION('',(1.,0.,0.));
#38283=DIRECTION('center_axis',(0.,0.,1.));
#38284=DIRECTION('ref_axis',(0.,-1.,0.));
#38285=DIRECTION('',(0.,-1.,0.));
#38286=DIRECTION('',(0.,-1.,0.));
#38287=DIRECTION('',(1.,0.,0.));
#38288=DIRECTION('center_axis',(1.,0.,0.));
#38289=DIRECTION('ref_axis',(0.,1.,3.33066907387539E-14));
#38290=DIRECTION('center_axis',(1.,0.,0.));
#38291=DIRECTION('ref_axis',(0.,1.,3.33066907387539E-14));
#38292=DIRECTION('center_axis',(1.,0.,0.));
#38293=DIRECTION('ref_axis',(0.,1.,3.33066907387539E-14));
#38294=DIRECTION('',(1.,0.,0.));
#38295=DIRECTION('center_axis',(0.,1.,0.));
#38296=DIRECTION('ref_axis',(0.,0.,1.));
#38297=DIRECTION('',(0.,0.,1.));
#38298=DIRECTION('',(0.,0.,1.));
#38299=DIRECTION('',(1.,0.,0.));
#38300=DIRECTION('center_axis',(1.,0.,0.));
#38301=DIRECTION('ref_axis',(0.,0.,-1.));
#38302=DIRECTION('center_axis',(1.,0.,0.));
#38303=DIRECTION('ref_axis',(0.,0.,-1.));
#38304=DIRECTION('center_axis',(1.,0.,0.));
#38305=DIRECTION('ref_axis',(0.,0.,-1.));
#38306=DIRECTION('',(1.,0.,0.));
#38307=DIRECTION('center_axis',(0.,0.,-1.));
#38308=DIRECTION('ref_axis',(0.,1.,0.));
#38309=DIRECTION('',(0.,1.,0.));
#38310=DIRECTION('',(0.,1.,0.));
#38311=DIRECTION('',(1.,0.,0.));
#38312=DIRECTION('center_axis',(1.,0.,0.));
#38313=DIRECTION('ref_axis',(0.,-1.,3.81639164714899E-15));
#38314=DIRECTION('center_axis',(1.,0.,0.));
#38315=DIRECTION('ref_axis',(0.,-1.,3.81639164714899E-15));
#38316=DIRECTION('center_axis',(1.,0.,0.));
#38317=DIRECTION('ref_axis',(0.,-1.,3.81639164714899E-15));
#38318=DIRECTION('center_axis',(1.,0.,0.));
#38319=DIRECTION('ref_axis',(0.,0.,-1.));
#38320=DIRECTION('center_axis',(1.,0.,0.));
#38321=DIRECTION('ref_axis',(0.,0.,-1.));
#38322=DIRECTION('axis',(0.,0.,1.));
#38323=DIRECTION('refdir',(1.,0.,0.));
#38324=DIRECTION('center_axis',(0.,0.,-1.));
#38325=DIRECTION('ref_axis',(0.,-1.,0.));
#38326=DIRECTION('',(0.,-1.,0.));
#38327=DIRECTION('',(-1.,0.,0.));
#38328=DIRECTION('',(0.,-1.,0.));
#38329=DIRECTION('',(-1.,0.,0.));
#38330=DIRECTION('center_axis',(0.,1.,0.));
#38331=DIRECTION('ref_axis',(0.,0.,-1.));
#38332=DIRECTION('',(0.,0.,-1.));
#38333=DIRECTION('',(-1.,0.,0.));
#38334=DIRECTION('',(0.,0.,-1.));
#38335=DIRECTION('center_axis',(0.,0.,1.));
#38336=DIRECTION('ref_axis',(0.,1.,0.));
#38337=DIRECTION('',(0.,1.,0.));
#38338=DIRECTION('',(-1.,0.,0.));
#38339=DIRECTION('',(0.,1.,0.));
#38340=DIRECTION('center_axis',(0.,-1.,0.));
#38341=DIRECTION('ref_axis',(0.,0.,1.));
#38342=DIRECTION('',(0.,0.,1.));
#38343=DIRECTION('',(0.,0.,1.));
#38344=DIRECTION('center_axis',(-1.,0.,0.));
#38345=DIRECTION('ref_axis',(0.,0.,1.));
#38346=DIRECTION('center_axis',(0.,0.,-1.));
#38347=DIRECTION('ref_axis',(0.,-1.,0.));
#38348=DIRECTION('',(0.,-1.,0.));
#38349=DIRECTION('',(-1.,0.,0.));
#38350=DIRECTION('',(0.,-1.,0.));
#38351=DIRECTION('',(-1.,0.,0.));
#38352=DIRECTION('center_axis',(0.,1.,0.));
#38353=DIRECTION('ref_axis',(0.,0.,-1.));
#38354=DIRECTION('',(0.,0.,-1.));
#38355=DIRECTION('',(-1.,0.,0.));
#38356=DIRECTION('',(0.,0.,-1.));
#38357=DIRECTION('center_axis',(0.,0.,1.));
#38358=DIRECTION('ref_axis',(0.,1.,0.));
#38359=DIRECTION('',(0.,1.,0.));
#38360=DIRECTION('',(-1.,0.,0.));
#38361=DIRECTION('',(0.,1.,0.));
#38362=DIRECTION('center_axis',(0.,-1.,0.));
#38363=DIRECTION('ref_axis',(0.,0.,1.));
#38364=DIRECTION('',(0.,0.,1.));
#38365=DIRECTION('',(0.,0.,1.));
#38366=DIRECTION('center_axis',(-1.,0.,0.));
#38367=DIRECTION('ref_axis',(0.,0.,1.));
#38368=DIRECTION('center_axis',(0.,0.,-1.));
#38369=DIRECTION('ref_axis',(0.,-1.,0.));
#38370=DIRECTION('',(0.,-1.,0.));
#38371=DIRECTION('',(-1.,0.,0.));
#38372=DIRECTION('',(0.,-1.,0.));
#38373=DIRECTION('',(-1.,0.,0.));
#38374=DIRECTION('center_axis',(0.,1.,0.));
#38375=DIRECTION('ref_axis',(0.,0.,-1.));
#38376=DIRECTION('',(0.,0.,-1.));
#38377=DIRECTION('',(-1.,0.,0.));
#38378=DIRECTION('',(0.,0.,-1.));
#38379=DIRECTION('center_axis',(0.,0.,1.));
#38380=DIRECTION('ref_axis',(0.,1.,0.));
#38381=DIRECTION('',(0.,1.,0.));
#38382=DIRECTION('',(-1.,0.,0.));
#38383=DIRECTION('',(0.,1.,0.));
#38384=DIRECTION('center_axis',(0.,-1.,0.));
#38385=DIRECTION('ref_axis',(0.,0.,1.));
#38386=DIRECTION('',(0.,0.,1.));
#38387=DIRECTION('',(0.,0.,1.));
#38388=DIRECTION('center_axis',(-1.,0.,0.));
#38389=DIRECTION('ref_axis',(0.,0.,1.));
#38390=DIRECTION('center_axis',(0.,0.,-1.));
#38391=DIRECTION('ref_axis',(0.,-1.,0.));
#38392=DIRECTION('',(0.,-1.,0.));
#38393=DIRECTION('',(-1.,0.,0.));
#38394=DIRECTION('',(0.,-1.,0.));
#38395=DIRECTION('',(-1.,0.,0.));
#38396=DIRECTION('center_axis',(0.,1.,0.));
#38397=DIRECTION('ref_axis',(0.,0.,-1.));
#38398=DIRECTION('',(0.,0.,-1.));
#38399=DIRECTION('',(-1.,0.,0.));
#38400=DIRECTION('',(0.,0.,-1.));
#38401=DIRECTION('center_axis',(0.,0.,1.));
#38402=DIRECTION('ref_axis',(0.,1.,0.));
#38403=DIRECTION('',(0.,1.,0.));
#38404=DIRECTION('',(-1.,0.,0.));
#38405=DIRECTION('',(0.,1.,0.));
#38406=DIRECTION('center_axis',(0.,-1.,0.));
#38407=DIRECTION('ref_axis',(0.,0.,1.));
#38408=DIRECTION('',(0.,0.,1.));
#38409=DIRECTION('',(0.,0.,1.));
#38410=DIRECTION('center_axis',(-1.,0.,0.));
#38411=DIRECTION('ref_axis',(0.,0.,1.));
#38412=DIRECTION('center_axis',(0.,0.,-1.));
#38413=DIRECTION('ref_axis',(0.,-1.,0.));
#38414=DIRECTION('',(0.,-1.,0.));
#38415=DIRECTION('',(-1.,0.,0.));
#38416=DIRECTION('',(0.,-1.,0.));
#38417=DIRECTION('',(-1.,0.,0.));
#38418=DIRECTION('center_axis',(0.,1.,0.));
#38419=DIRECTION('ref_axis',(0.,0.,-1.));
#38420=DIRECTION('',(0.,0.,-1.));
#38421=DIRECTION('',(-1.,0.,0.));
#38422=DIRECTION('',(0.,0.,-1.));
#38423=DIRECTION('center_axis',(0.,0.,1.));
#38424=DIRECTION('ref_axis',(0.,1.,0.));
#38425=DIRECTION('',(0.,1.,0.));
#38426=DIRECTION('',(-1.,0.,0.));
#38427=DIRECTION('',(0.,1.,0.));
#38428=DIRECTION('center_axis',(0.,-1.,0.));
#38429=DIRECTION('ref_axis',(0.,0.,1.));
#38430=DIRECTION('',(0.,0.,1.));
#38431=DIRECTION('',(0.,0.,1.));
#38432=DIRECTION('center_axis',(-1.,0.,0.));
#38433=DIRECTION('ref_axis',(0.,0.,1.));
#38434=DIRECTION('center_axis',(0.,0.,-1.));
#38435=DIRECTION('ref_axis',(0.,-1.,0.));
#38436=DIRECTION('',(0.,-1.,0.));
#38437=DIRECTION('',(-1.,0.,0.));
#38438=DIRECTION('',(0.,-1.,0.));
#38439=DIRECTION('',(-1.,0.,0.));
#38440=DIRECTION('center_axis',(0.,1.,0.));
#38441=DIRECTION('ref_axis',(0.,0.,-1.));
#38442=DIRECTION('',(0.,0.,-1.));
#38443=DIRECTION('',(-1.,0.,0.));
#38444=DIRECTION('',(0.,0.,-1.));
#38445=DIRECTION('center_axis',(0.,0.,1.));
#38446=DIRECTION('ref_axis',(0.,1.,0.));
#38447=DIRECTION('',(0.,1.,0.));
#38448=DIRECTION('',(-1.,0.,0.));
#38449=DIRECTION('',(0.,1.,0.));
#38450=DIRECTION('center_axis',(0.,-1.,0.));
#38451=DIRECTION('ref_axis',(0.,0.,1.));
#38452=DIRECTION('',(0.,0.,1.));
#38453=DIRECTION('',(0.,0.,1.));
#38454=DIRECTION('center_axis',(-1.,0.,0.));
#38455=DIRECTION('ref_axis',(0.,0.,1.));
#38456=DIRECTION('center_axis',(0.,0.,-1.));
#38457=DIRECTION('ref_axis',(0.,-1.,0.));
#38458=DIRECTION('',(0.,-1.,0.));
#38459=DIRECTION('',(-1.,0.,0.));
#38460=DIRECTION('',(0.,-1.,0.));
#38461=DIRECTION('',(-1.,0.,0.));
#38462=DIRECTION('center_axis',(0.,1.,0.));
#38463=DIRECTION('ref_axis',(0.,0.,-1.));
#38464=DIRECTION('',(0.,0.,-1.));
#38465=DIRECTION('',(-1.,0.,0.));
#38466=DIRECTION('',(0.,0.,-1.));
#38467=DIRECTION('center_axis',(0.,0.,1.));
#38468=DIRECTION('ref_axis',(0.,1.,0.));
#38469=DIRECTION('',(0.,1.,0.));
#38470=DIRECTION('',(-1.,0.,0.));
#38471=DIRECTION('',(0.,1.,0.));
#38472=DIRECTION('center_axis',(0.,-1.,0.));
#38473=DIRECTION('ref_axis',(0.,0.,1.));
#38474=DIRECTION('',(0.,0.,1.));
#38475=DIRECTION('',(0.,0.,1.));
#38476=DIRECTION('center_axis',(-1.,0.,0.));
#38477=DIRECTION('ref_axis',(0.,0.,1.));
#38478=DIRECTION('center_axis',(0.,0.,-1.));
#38479=DIRECTION('ref_axis',(0.,-1.,0.));
#38480=DIRECTION('',(0.,-1.,0.));
#38481=DIRECTION('',(-1.,0.,0.));
#38482=DIRECTION('',(0.,-1.,0.));
#38483=DIRECTION('',(-1.,0.,0.));
#38484=DIRECTION('center_axis',(0.,1.,0.));
#38485=DIRECTION('ref_axis',(0.,0.,-1.));
#38486=DIRECTION('',(0.,0.,-1.));
#38487=DIRECTION('',(-1.,0.,0.));
#38488=DIRECTION('',(0.,0.,-1.));
#38489=DIRECTION('center_axis',(0.,0.,1.));
#38490=DIRECTION('ref_axis',(0.,1.,0.));
#38491=DIRECTION('',(0.,1.,0.));
#38492=DIRECTION('',(-1.,0.,0.));
#38493=DIRECTION('',(0.,1.,0.));
#38494=DIRECTION('center_axis',(0.,-1.,0.));
#38495=DIRECTION('ref_axis',(0.,0.,1.));
#38496=DIRECTION('',(0.,0.,1.));
#38497=DIRECTION('',(0.,0.,1.));
#38498=DIRECTION('center_axis',(-1.,0.,0.));
#38499=DIRECTION('ref_axis',(0.,0.,1.));
#38500=DIRECTION('center_axis',(0.,0.,-1.));
#38501=DIRECTION('ref_axis',(0.,-1.,0.));
#38502=DIRECTION('',(0.,-1.,0.));
#38503=DIRECTION('',(-1.,0.,0.));
#38504=DIRECTION('',(0.,-1.,0.));
#38505=DIRECTION('',(-1.,0.,0.));
#38506=DIRECTION('center_axis',(0.,1.,0.));
#38507=DIRECTION('ref_axis',(0.,0.,-1.));
#38508=DIRECTION('',(0.,0.,-1.));
#38509=DIRECTION('',(-1.,0.,0.));
#38510=DIRECTION('',(0.,0.,-1.));
#38511=DIRECTION('center_axis',(0.,0.,1.));
#38512=DIRECTION('ref_axis',(0.,1.,0.));
#38513=DIRECTION('',(0.,1.,0.));
#38514=DIRECTION('',(-1.,0.,0.));
#38515=DIRECTION('',(0.,1.,0.));
#38516=DIRECTION('center_axis',(0.,-1.,0.));
#38517=DIRECTION('ref_axis',(0.,0.,1.));
#38518=DIRECTION('',(0.,0.,1.));
#38519=DIRECTION('',(0.,0.,1.));
#38520=DIRECTION('center_axis',(-1.,0.,0.));
#38521=DIRECTION('ref_axis',(0.,0.,1.));
#38522=DIRECTION('center_axis',(0.,0.,-1.));
#38523=DIRECTION('ref_axis',(0.,-1.,0.));
#38524=DIRECTION('',(0.,-1.,0.));
#38525=DIRECTION('',(-1.,0.,0.));
#38526=DIRECTION('',(0.,-1.,0.));
#38527=DIRECTION('',(-1.,0.,0.));
#38528=DIRECTION('center_axis',(0.,1.,0.));
#38529=DIRECTION('ref_axis',(0.,0.,-1.));
#38530=DIRECTION('',(0.,0.,-1.));
#38531=DIRECTION('',(-1.,0.,0.));
#38532=DIRECTION('',(0.,0.,-1.));
#38533=DIRECTION('center_axis',(0.,0.,1.));
#38534=DIRECTION('ref_axis',(0.,1.,0.));
#38535=DIRECTION('',(0.,1.,0.));
#38536=DIRECTION('',(-1.,0.,0.));
#38537=DIRECTION('',(0.,1.,0.));
#38538=DIRECTION('center_axis',(0.,-1.,0.));
#38539=DIRECTION('ref_axis',(0.,0.,1.));
#38540=DIRECTION('',(0.,0.,1.));
#38541=DIRECTION('',(0.,0.,1.));
#38542=DIRECTION('center_axis',(-1.,0.,0.));
#38543=DIRECTION('ref_axis',(0.,0.,1.));
#38544=DIRECTION('center_axis',(0.,0.,-1.));
#38545=DIRECTION('ref_axis',(0.,-1.,0.));
#38546=DIRECTION('',(0.,-1.,0.));
#38547=DIRECTION('',(-1.,0.,0.));
#38548=DIRECTION('',(0.,-1.,0.));
#38549=DIRECTION('',(-1.,0.,0.));
#38550=DIRECTION('center_axis',(0.,1.,0.));
#38551=DIRECTION('ref_axis',(0.,0.,-1.));
#38552=DIRECTION('',(0.,0.,-1.));
#38553=DIRECTION('',(-1.,0.,0.));
#38554=DIRECTION('',(0.,0.,-1.));
#38555=DIRECTION('center_axis',(0.,0.,1.));
#38556=DIRECTION('ref_axis',(0.,1.,0.));
#38557=DIRECTION('',(0.,1.,0.));
#38558=DIRECTION('',(-1.,0.,0.));
#38559=DIRECTION('',(0.,1.,0.));
#38560=DIRECTION('center_axis',(0.,-1.,0.));
#38561=DIRECTION('ref_axis',(0.,0.,1.));
#38562=DIRECTION('',(0.,0.,1.));
#38563=DIRECTION('',(0.,0.,1.));
#38564=DIRECTION('center_axis',(-1.,0.,0.));
#38565=DIRECTION('ref_axis',(0.,0.,1.));
#38566=DIRECTION('center_axis',(1.,0.,0.));
#38567=DIRECTION('ref_axis',(0.,0.,-1.));
#38568=DIRECTION('center_axis',(1.,0.,0.));
#38569=DIRECTION('ref_axis',(0.,0.,-1.));
#38570=DIRECTION('',(1.,0.,0.));
#38571=DIRECTION('center_axis',(-1.,0.,0.));
#38572=DIRECTION('ref_axis',(0.,0.,-1.));
#38573=DIRECTION('center_axis',(1.,0.,0.));
#38574=DIRECTION('ref_axis',(0.,0.,-1.));
#38575=DIRECTION('center_axis',(1.,0.,0.));
#38576=DIRECTION('ref_axis',(0.,0.,-1.));
#38577=DIRECTION('',(1.,0.,0.));
#38578=DIRECTION('center_axis',(-1.,0.,0.));
#38579=DIRECTION('ref_axis',(0.,0.,-1.));
#38580=DIRECTION('center_axis',(-1.,0.,0.));
#38581=DIRECTION('ref_axis',(0.,0.,1.));
#38582=DIRECTION('',(0.,0.,-1.));
#38583=DIRECTION('',(0.,1.,0.));
#38584=DIRECTION('',(0.,0.,1.));
#38585=DIRECTION('',(0.,1.,0.));
#38586=DIRECTION('center_axis',(0.,0.,-1.));
#38587=DIRECTION('ref_axis',(-1.,0.,0.));
#38588=DIRECTION('',(1.,0.,0.));
#38589=DIRECTION('',(-1.,0.,0.));
#38590=DIRECTION('',(0.,1.,0.));
#38591=DIRECTION('center_axis',(1.,0.,0.));
#38592=DIRECTION('ref_axis',(0.,0.,-1.));
#38593=DIRECTION('',(0.,0.,1.));
#38594=DIRECTION('',(0.,0.,-1.));
#38595=DIRECTION('',(0.,1.,0.));
#38596=DIRECTION('center_axis',(0.,0.,-1.));
#38597=DIRECTION('ref_axis',(-1.,0.,0.));
#38598=DIRECTION('',(1.,0.,0.));
#38599=DIRECTION('',(-1.,0.,0.));
#38600=DIRECTION('',(0.,1.,0.));
#38601=DIRECTION('center_axis',(-1.,0.,0.));
#38602=DIRECTION('ref_axis',(0.,0.,1.));
#38603=DIRECTION('',(0.,0.,-1.));
#38604=DIRECTION('',(0.,0.,1.));
#38605=DIRECTION('',(0.,1.,0.));
#38606=DIRECTION('center_axis',(0.,0.,-1.));
#38607=DIRECTION('ref_axis',(-1.,0.,0.));
#38608=DIRECTION('',(1.,0.,0.));
#38609=DIRECTION('',(-1.,0.,0.));
#38610=DIRECTION('',(0.,1.,0.));
#38611=DIRECTION('center_axis',(1.,0.,0.));
#38612=DIRECTION('ref_axis',(0.,0.,-1.));
#38613=DIRECTION('',(0.,0.,1.));
#38614=DIRECTION('',(0.,0.,-1.));
#38615=DIRECTION('',(0.,1.,0.));
#38616=DIRECTION('center_axis',(0.,0.,1.));
#38617=DIRECTION('ref_axis',(1.,0.,0.));
#38618=DIRECTION('',(-1.,0.,0.));
#38619=DIRECTION('',(1.,0.,0.));
#38620=DIRECTION('center_axis',(0.,1.,0.));
#38621=DIRECTION('ref_axis',(0.,0.,1.));
#38622=DIRECTION('center_axis',(0.,1.,0.));
#38623=DIRECTION('ref_axis',(1.,0.,0.));
#38624=DIRECTION('axis',(0.,0.,1.));
#38625=DIRECTION('refdir',(1.,0.,0.));
#38626=DIRECTION('center_axis',(0.,-1.,0.));
#38627=DIRECTION('ref_axis',(-1.83697019872103E-16,0.,-1.));
#38628=DIRECTION('center_axis',(0.,-1.,0.));
#38629=DIRECTION('ref_axis',(1.,0.,0.));
#38630=DIRECTION('center_axis',(0.,1.,0.));
#38631=DIRECTION('ref_axis',(1.,0.,0.));
#38632=DIRECTION('center_axis',(0.,1.,0.));
#38633=DIRECTION('ref_axis',(1.,0.,0.));
#38634=DIRECTION('',(-1.,0.,0.));
#38635=DIRECTION('center_axis',(0.,-1.,0.));
#38636=DIRECTION('ref_axis',(1.,0.,0.));
#38637=DIRECTION('',(-1.,0.,0.));
#38638=DIRECTION('',(0.,0.,-1.));
#38639=DIRECTION('',(1.,0.,0.));
#38640=DIRECTION('',(0.,0.,1.));
#38641=DIRECTION('',(-1.,0.,0.));
#38642=DIRECTION('',(0.,0.,-1.));
#38643=DIRECTION('center_axis',(0.,1.,0.));
#38644=DIRECTION('ref_axis',(1.,0.,-4.93432455388958E-16));
#38645=DIRECTION('',(0.,0.,1.));
#38646=DIRECTION('center_axis',(0.,1.,0.));
#38647=DIRECTION('ref_axis',(-1.,0.,4.93432455388958E-16));
#38648=DIRECTION('',(0.,0.,-1.));
#38649=DIRECTION('center_axis',(0.,1.,0.));
#38650=DIRECTION('ref_axis',(1.,0.,-4.93432455388958E-16));
#38651=DIRECTION('',(0.,0.,1.));
#38652=DIRECTION('center_axis',(0.,1.,0.));
#38653=DIRECTION('ref_axis',(-1.,0.,4.93432455388958E-16));
#38654=DIRECTION('center_axis',(0.,-1.,0.));
#38655=DIRECTION('ref_axis',(-1.83697019872103E-16,0.,-1.));
#38656=DIRECTION('center_axis',(0.,1.,0.));
#38657=DIRECTION('ref_axis',(1.,0.,0.));
#38658=DIRECTION('center_axis',(0.,0.,1.));
#38659=DIRECTION('ref_axis',(1.,0.,0.));
#38660=DIRECTION('',(0.,1.,0.));
#38661=DIRECTION('',(1.,0.,0.));
#38662=DIRECTION('',(0.,1.,0.));
#38663=DIRECTION('',(0.,1.,0.));
#38664=DIRECTION('',(1.,0.,0.));
#38665=DIRECTION('',(0.,-1.,0.));
#38666=DIRECTION('',(0.,1.,0.));
#38667=DIRECTION('',(1.,0.,0.));
#38668=DIRECTION('',(0.,-1.,0.));
#38669=DIRECTION('center_axis',(0.,1.,0.));
#38670=DIRECTION('ref_axis',(5.0532154980743E-16,0.,-1.));
#38671=DIRECTION('center_axis',(0.,1.,0.));
#38672=DIRECTION('ref_axis',(1.,0.,0.));
#38673=DIRECTION('center_axis',(0.,1.,0.));
#38674=DIRECTION('ref_axis',(1.,0.,0.));
#38675=DIRECTION('center_axis',(0.,-1.,0.));
#38676=DIRECTION('ref_axis',(1.,0.,0.));
#38677=DIRECTION('center_axis',(0.,1.,0.));
#38678=DIRECTION('ref_axis',(-1.60812264967664E-16,0.,-1.));
#38679=DIRECTION('center_axis',(0.,1.,0.));
#38680=DIRECTION('ref_axis',(1.,0.,0.));
#38681=DIRECTION('center_axis',(0.,1.,0.));
#38682=DIRECTION('ref_axis',(1.,0.,0.));
#38683=DIRECTION('center_axis',(0.,-1.,0.));
#38684=DIRECTION('ref_axis',(1.,0.,0.));
#38685=DIRECTION('center_axis',(0.,1.,0.));
#38686=DIRECTION('ref_axis',(1.,0.,0.));
#38687=DIRECTION('',(0.,1.,0.));
#38688=DIRECTION('center_axis',(0.,-1.,0.));
#38689=DIRECTION('ref_axis',(1.,0.,0.));
#38690=DIRECTION('center_axis',(0.,-0.707106781186548,-0.707106781186548));
#38691=DIRECTION('ref_axis',(0.,0.707106781186548,-0.707106781186548));
#38692=DIRECTION('center_axis',(0.,-1.,0.));
#38693=DIRECTION('ref_axis',(1.,0.,0.));
#38694=DIRECTION('center_axis',(0.,1.,0.));
#38695=DIRECTION('ref_axis',(1.,0.,0.));
#38696=DIRECTION('',(0.,1.,0.));
#38697=DIRECTION('center_axis',(0.,-1.,0.));
#38698=DIRECTION('ref_axis',(1.,0.,0.));
#38699=DIRECTION('center_axis',(0.,-0.707106781186548,-0.707106781186548));
#38700=DIRECTION('ref_axis',(0.,0.707106781186548,-0.707106781186548));
#38701=DIRECTION('center_axis',(0.,-1.,0.));
#38702=DIRECTION('ref_axis',(1.,0.,0.));
#38703=DIRECTION('center_axis',(0.,0.707106781186548,0.707106781186548));
#38704=DIRECTION('ref_axis',(1.,0.,0.));
#38705=DIRECTION('',(-1.,0.,0.));
#38706=DIRECTION('',(-0.577350269189626,-0.577350269189626,0.577350269189626));
#38707=DIRECTION('',(0.577350269189624,-0.577350269189627,0.577350269189627));
#38708=DIRECTION('',(-1.,0.,0.));
#38709=DIRECTION('',(-1.,0.,0.));
#38710=DIRECTION('center_axis',(1.,0.,0.));
#38711=DIRECTION('ref_axis',(0.,0.,1.));
#38712=DIRECTION('',(0.,0.,1.));
#38713=DIRECTION('',(0.,-1.,0.));
#38714=DIRECTION('',(0.,-1.,0.));
#38715=DIRECTION('center_axis',(0.,-1.,0.));
#38716=DIRECTION('ref_axis',(1.,0.,-4.93432455388958E-16));
#38717=DIRECTION('center_axis',(0.,-0.707106781186548,0.707106781186548));
#38718=DIRECTION('ref_axis',(3.48909435263061E-16,0.707106781186547,0.707106781186547));
#38719=DIRECTION('center_axis',(0.,-1.,0.));
#38720=DIRECTION('ref_axis',(1.,0.,-4.93432455388958E-16));
#38721=DIRECTION('',(0.,-1.,0.));
#38722=DIRECTION('center_axis',(0.,-1.,0.));
#38723=DIRECTION('ref_axis',(1.,0.,-4.93432455388958E-16));
#38724=DIRECTION('center_axis',(-1.,0.,0.));
#38725=DIRECTION('ref_axis',(0.,0.,-1.));
#38726=DIRECTION('',(0.,0.,-1.));
#38727=DIRECTION('',(0.,-1.,0.));
#38728=DIRECTION('center_axis',(0.,-1.,0.));
#38729=DIRECTION('ref_axis',(-1.,0.,4.93432455388958E-16));
#38730=DIRECTION('center_axis',(0.,-1.,0.));
#38731=DIRECTION('ref_axis',(-1.,0.,4.93432455388958E-16));
#38732=DIRECTION('center_axis',(1.,0.,0.));
#38733=DIRECTION('ref_axis',(0.,0.,1.));
#38734=DIRECTION('',(0.,0.,1.));
#38735=DIRECTION('',(0.,-1.,0.));
#38736=DIRECTION('',(0.,-1.,0.));
#38737=DIRECTION('center_axis',(0.,-1.,0.));
#38738=DIRECTION('ref_axis',(1.,0.,-4.93432455388958E-16));
#38739=DIRECTION('center_axis',(0.,-0.707106781186548,0.707106781186548));
#38740=DIRECTION('ref_axis',(3.48909435263061E-16,0.707106781186547,0.707106781186547));
#38741=DIRECTION('center_axis',(0.,-1.,0.));
#38742=DIRECTION('ref_axis',(1.,0.,-4.93432455388958E-16));
#38743=DIRECTION('',(0.,-1.,0.));
#38744=DIRECTION('center_axis',(0.,-1.,0.));
#38745=DIRECTION('ref_axis',(1.,0.,-4.93432455388958E-16));
#38746=DIRECTION('center_axis',(-1.,0.,0.));
#38747=DIRECTION('ref_axis',(0.,0.,-1.));
#38748=DIRECTION('',(0.,0.,-1.));
#38749=DIRECTION('',(0.,-1.,0.));
#38750=DIRECTION('center_axis',(0.,-1.,0.));
#38751=DIRECTION('ref_axis',(-1.,0.,4.93432455388958E-16));
#38752=DIRECTION('center_axis',(0.,-1.,0.));
#38753=DIRECTION('ref_axis',(-1.,0.,4.93432455388958E-16));
#38754=DIRECTION('center_axis',(0.,1.,0.));
#38755=DIRECTION('ref_axis',(0.,0.,1.));
#38756=DIRECTION('',(0.,0.,1.));
#38757=DIRECTION('',(1.,0.,0.));
#38758=DIRECTION('',(1.,0.,0.));
#38759=DIRECTION('',(1.,0.,0.));
#38760=DIRECTION('',(0.,0.,-1.));
#38761=DIRECTION('center_axis',(0.707106781186548,0.707106781186548,0.));
#38762=DIRECTION('ref_axis',(0.,0.,-1.));
#38763=DIRECTION('',(0.,0.,-1.));
#38764=DIRECTION('',(0.577350269189626,-0.577350269189626,-0.577350269189626));
#38765=DIRECTION('center_axis',(-0.707106781186548,0.707106781186548,0.));
#38766=DIRECTION('ref_axis',(0.,0.,1.));
#38767=DIRECTION('',(-0.577350269189623,-0.577350269189626,-0.577350269189628));
#38768=DIRECTION('',(0.,0.,1.));
#38769=DIRECTION('center_axis',(0.,0.707106781186548,-0.707106781186548));
#38770=DIRECTION('ref_axis',(-1.,0.,0.));
#38771=DIRECTION('',(-1.,0.,0.));
#38772=DIRECTION('center_axis',(0.,0.,-1.));
#38773=DIRECTION('ref_axis',(-1.,0.,0.));
#38774=DIRECTION('',(0.,1.,0.));
#38775=DIRECTION('',(0.,1.,0.));
#38776=DIRECTION('center_axis',(1.,0.,0.));
#38777=DIRECTION('ref_axis',(0.,0.,-1.));
#38778=DIRECTION('center_axis',(-1.,0.,0.));
#38779=DIRECTION('ref_axis',(0.,0.,1.));
#38780=DIRECTION('axis',(0.,0.,1.));
#38781=DIRECTION('refdir',(1.,0.,0.));
#38782=DIRECTION('center_axis',(1.,0.,0.));
#38783=DIRECTION('ref_axis',(0.,1.,0.));
#38784=DIRECTION('',(-1.,0.,0.));
#38785=DIRECTION('center_axis',(1.,0.,0.));
#38786=DIRECTION('ref_axis',(0.,1.,0.));
#38787=DIRECTION('center_axis',(1.,0.,0.));
#38788=DIRECTION('ref_axis',(0.,1.,0.));
#38789=DIRECTION('',(-1.,0.,0.));
#38790=DIRECTION('center_axis',(1.,0.,0.));
#38791=DIRECTION('ref_axis',(0.,1.,0.));
#38792=DIRECTION('',(-1.,0.,0.));
#38793=DIRECTION('center_axis',(1.,0.,0.));
#38794=DIRECTION('ref_axis',(0.,1.,0.));
#38795=DIRECTION('',(-1.,0.,0.));
#38796=DIRECTION('center_axis',(1.,0.,0.));
#38797=DIRECTION('ref_axis',(0.,1.,0.));
#38798=DIRECTION('',(-1.,0.,0.));
#38799=DIRECTION('center_axis',(1.,0.,0.));
#38800=DIRECTION('ref_axis',(0.,1.,0.));
#38801=DIRECTION('',(-1.,0.,0.));
#38802=DIRECTION('center_axis',(1.,0.,0.));
#38803=DIRECTION('ref_axis',(0.,1.,0.));
#38804=DIRECTION('',(-1.,0.,0.));
#38805=DIRECTION('center_axis',(1.,0.,0.));
#38806=DIRECTION('ref_axis',(0.,1.,0.));
#38807=DIRECTION('',(-1.,0.,0.));
#38808=DIRECTION('center_axis',(1.,0.,0.));
#38809=DIRECTION('ref_axis',(0.,1.,0.));
#38810=DIRECTION('',(-1.,0.,0.));
#38811=DIRECTION('center_axis',(1.,0.,0.));
#38812=DIRECTION('ref_axis',(0.,0.945745520993383,-0.32490830940583));
#38813=DIRECTION('',(-1.,0.,0.));
#38814=DIRECTION('center_axis',(-1.,0.,0.));
#38815=DIRECTION('ref_axis',(0.,1.,3.95919057815806E-14));
#38816=DIRECTION('center_axis',(1.,0.,0.));
#38817=DIRECTION('ref_axis',(0.,0.945745520993383,-0.32490830940583));
#38818=DIRECTION('',(-1.,0.,0.));
#38819=DIRECTION('center_axis',(1.,0.,0.));
#38820=DIRECTION('ref_axis',(0.,0.945745520993383,-0.32490830940583));
#38821=DIRECTION('',(-1.,0.,0.));
#38822=DIRECTION('center_axis',(1.,0.,0.));
#38823=DIRECTION('ref_axis',(0.,0.945745520993383,-0.32490830940583));
#38824=DIRECTION('',(-1.,0.,0.));
#38825=DIRECTION('center_axis',(1.,0.,0.));
#38826=DIRECTION('ref_axis',(0.,0.945745520993383,-0.32490830940583));
#38827=DIRECTION('',(-1.,0.,0.));
#38828=DIRECTION('center_axis',(1.,0.,0.));
#38829=DIRECTION('ref_axis',(0.,0.945745520993383,-0.32490830940583));
#38830=DIRECTION('',(-1.,0.,0.));
#38831=DIRECTION('center_axis',(1.,0.,0.));
#38832=DIRECTION('ref_axis',(0.,0.945745520993383,-0.32490830940583));
#38833=DIRECTION('',(-1.,0.,0.));
#38834=DIRECTION('center_axis',(1.,0.,0.));
#38835=DIRECTION('ref_axis',(0.,0.945745520993383,-0.32490830940583));
#38836=DIRECTION('',(-1.,0.,0.));
#38837=DIRECTION('center_axis',(1.,0.,0.));
#38838=DIRECTION('ref_axis',(0.,0.945745520993383,-0.32490830940583));
#38839=DIRECTION('center_axis',(1.,0.,0.));
#38840=DIRECTION('ref_axis',(0.,1.,3.95919057815806E-14));
#38841=DIRECTION('center_axis',(1.,0.,0.));
#38842=DIRECTION('ref_axis',(0.,-0.404759137094124,-0.914423337923317));
#38843=DIRECTION('center_axis',(-1.,0.,0.));
#38844=DIRECTION('ref_axis',(0.,1.,0.));
#38845=DIRECTION('center_axis',(1.,0.,0.));
#38846=DIRECTION('ref_axis',(0.,0.,-1.));
#38847=DIRECTION('center_axis',(-1.,0.,0.));
#38848=DIRECTION('ref_axis',(0.,1.,0.));
#38849=DIRECTION('center_axis',(-1.,0.,0.));
#38850=DIRECTION('ref_axis',(0.,1.,0.));
#38851=DIRECTION('center_axis',(1.,0.,0.));
#38852=DIRECTION('ref_axis',(0.,0.,-1.));
#38853=DIRECTION('center_axis',(1.,0.,0.));
#38854=DIRECTION('ref_axis',(0.,1.,0.));
#38855=DIRECTION('center_axis',(1.,0.,0.));
#38856=DIRECTION('ref_axis',(0.,1.,0.));
#38857=DIRECTION('center_axis',(1.,0.,0.));
#38858=DIRECTION('ref_axis',(0.,1.,0.));
#38859=DIRECTION('center_axis',(1.,0.,0.));
#38860=DIRECTION('ref_axis',(0.,0.,-1.));
#38861=DIRECTION('center_axis',(1.,0.,0.));
#38862=DIRECTION('ref_axis',(0.,0.,-1.));
#38863=DIRECTION('center_axis',(1.,0.,0.));
#38864=DIRECTION('ref_axis',(0.,0.,-1.));
#38865=DIRECTION('center_axis',(1.,0.,0.));
#38866=DIRECTION('ref_axis',(0.,0.,-1.));
#38867=DIRECTION('center_axis',(1.,0.,0.));
#38868=DIRECTION('ref_axis',(0.,0.,-1.));
#38869=DIRECTION('center_axis',(1.,0.,0.));
#38870=DIRECTION('ref_axis',(0.,0.,-1.));
#38871=DIRECTION('',(0.707106781186556,-0.707106781186539,-8.65956056235483E-17));
#38872=DIRECTION('center_axis',(-1.,0.,0.));
#38873=DIRECTION('ref_axis',(0.,1.,0.));
#38874=DIRECTION('center_axis',(1.,0.,0.));
#38875=DIRECTION('ref_axis',(0.,1.,0.));
#38876=DIRECTION('',(1.,0.,0.));
#38877=DIRECTION('',(-1.,0.,0.));
#38878=DIRECTION('center_axis',(1.,0.,0.));
#38879=DIRECTION('ref_axis',(0.,1.,0.));
#38880=DIRECTION('center_axis',(1.,0.,0.));
#38881=DIRECTION('ref_axis',(0.,1.,0.));
#38882=DIRECTION('',(-1.,0.,0.));
#38883=DIRECTION('center_axis',(1.,0.,0.));
#38884=DIRECTION('ref_axis',(0.,1.,0.));
#38885=DIRECTION('',(1.,0.,0.));
#38886=DIRECTION('center_axis',(1.,0.,0.));
#38887=DIRECTION('ref_axis',(0.,1.,0.));
#38888=DIRECTION('',(1.,0.,0.));
#38889=DIRECTION('',(-1.,0.,0.));
#38890=DIRECTION('center_axis',(1.,0.,0.));
#38891=DIRECTION('ref_axis',(0.,1.,0.));
#38892=DIRECTION('center_axis',(1.,0.,0.));
#38893=DIRECTION('ref_axis',(0.,1.,0.));
#38894=DIRECTION('',(-1.,0.,0.));
#38895=DIRECTION('center_axis',(1.,0.,0.));
#38896=DIRECTION('ref_axis',(0.,1.,0.));
#38897=DIRECTION('',(1.,0.,0.));
#38898=DIRECTION('center_axis',(1.,0.,0.));
#38899=DIRECTION('ref_axis',(0.,1.,0.));
#38900=DIRECTION('',(1.,0.,0.));
#38901=DIRECTION('',(-1.,0.,0.));
#38902=DIRECTION('center_axis',(1.,0.,0.));
#38903=DIRECTION('ref_axis',(0.,1.,0.));
#38904=DIRECTION('center_axis',(1.,0.,0.));
#38905=DIRECTION('ref_axis',(0.,1.,0.));
#38906=DIRECTION('',(-1.,0.,0.));
#38907=DIRECTION('center_axis',(1.,0.,0.));
#38908=DIRECTION('ref_axis',(0.,1.,0.));
#38909=DIRECTION('',(1.,0.,0.));
#38910=DIRECTION('center_axis',(0.,-0.866025403784431,0.500000000000014));
#38911=DIRECTION('ref_axis',(0.,0.500000000000014,0.866025403784431));
#38912=DIRECTION('',(0.,0.500000000000014,0.866025403784431));
#38913=DIRECTION('',(-1.,0.,0.));
#38914=DIRECTION('',(0.,0.500000000000014,0.866025403784431));
#38915=DIRECTION('',(-1.,0.,0.));
#38916=DIRECTION('center_axis',(0.,-0.866025403784431,-0.500000000000014));
#38917=DIRECTION('ref_axis',(0.,-0.500000000000014,0.866025403784431));
#38918=DIRECTION('',(0.,-0.500000000000014,0.866025403784431));
#38919=DIRECTION('',(-1.,0.,0.));
#38920=DIRECTION('',(0.,-0.500000000000014,0.866025403784431));
#38921=DIRECTION('center_axis',(0.,0.,-1.));
#38922=DIRECTION('ref_axis',(0.,-1.,0.));
#38923=DIRECTION('',(0.,-1.,0.));
#38924=DIRECTION('',(-1.,0.,0.));
#38925=DIRECTION('',(0.,-1.,0.));
#38926=DIRECTION('center_axis',(1.,0.,0.));
#38927=DIRECTION('ref_axis',(0.,0.,-1.));
#38928=DIRECTION('center_axis',(1.,0.,0.));
#38929=DIRECTION('ref_axis',(0.,0.,-1.));
#38930=DIRECTION('center_axis',(1.,0.,0.));
#38931=DIRECTION('ref_axis',(0.,0.,-1.));
#38932=DIRECTION('',(0.,-0.500000000000029,-0.866025403784422));
#38933=DIRECTION('center_axis',(1.,0.,0.));
#38934=DIRECTION('ref_axis',(0.,0.,-1.));
#38935=DIRECTION('center_axis',(1.,0.,0.));
#38936=DIRECTION('ref_axis',(0.,0.,-1.));
#38937=DIRECTION('',(0.,0.500000000000029,-0.866025403784422));
#38938=DIRECTION('center_axis',(1.,0.,0.));
#38939=DIRECTION('ref_axis',(0.,0.,-1.));
#38940=DIRECTION('',(0.,1.,0.));
#38941=DIRECTION('center_axis',(1.,0.,0.));
#38942=DIRECTION('ref_axis',(0.,0.,-1.));
#38943=DIRECTION('',(0.,0.500000000000029,-0.866025403784422));
#38944=DIRECTION('center_axis',(1.,0.,0.));
#38945=DIRECTION('ref_axis',(0.,0.,-1.));
#38946=DIRECTION('center_axis',(1.,0.,0.));
#38947=DIRECTION('ref_axis',(0.,0.,-1.));
#38948=DIRECTION('',(0.,-0.500000000000029,-0.866025403784422));
#38949=DIRECTION('center_axis',(1.,0.,0.));
#38950=DIRECTION('ref_axis',(0.,0.,-1.));
#38951=DIRECTION('center_axis',(1.,0.,0.));
#38952=DIRECTION('ref_axis',(0.,0.,-1.));
#38953=DIRECTION('center_axis',(1.,0.,0.));
#38954=DIRECTION('ref_axis',(0.,0.,-1.));
#38955=DIRECTION('center_axis',(1.,0.,0.));
#38956=DIRECTION('ref_axis',(0.,0.,-1.));
#38957=DIRECTION('center_axis',(1.,0.,0.));
#38958=DIRECTION('ref_axis',(0.,0.,-1.));
#38959=DIRECTION('center_axis',(1.,0.,0.));
#38960=DIRECTION('ref_axis',(0.,0.,-1.));
#38961=DIRECTION('center_axis',(1.,0.,0.));
#38962=DIRECTION('ref_axis',(0.,0.,-1.));
#38963=DIRECTION('center_axis',(1.,0.,0.));
#38964=DIRECTION('ref_axis',(0.,0.,-1.));
#38965=DIRECTION('',(0.,1.,0.));
#38966=DIRECTION('center_axis',(1.,0.,0.));
#38967=DIRECTION('ref_axis',(0.,0.,-1.));
#38968=DIRECTION('center_axis',(1.,0.,0.));
#38969=DIRECTION('ref_axis',(0.,1.,0.));
#38970=DIRECTION('',(0.515038074910049,-0.857167300702115,-1.04972719113862E-16));
#38971=DIRECTION('center_axis',(0.,0.866025403784422,0.500000000000029));
#38972=DIRECTION('ref_axis',(0.,0.500000000000029,-0.866025403784422));
#38973=DIRECTION('',(-1.,0.,0.));
#38974=DIRECTION('',(-1.,0.,0.));
#38975=DIRECTION('center_axis',(0.,0.,1.));
#38976=DIRECTION('ref_axis',(0.,1.,0.));
#38977=DIRECTION('center_axis',(0.,0.866025403784422,-0.500000000000029));
#38978=DIRECTION('ref_axis',(0.,-0.500000000000029,-0.866025403784422));
#38979=DIRECTION('center_axis',(-1.,0.,0.));
#38980=DIRECTION('ref_axis',(0.,0.,1.));
#38981=DIRECTION('center_axis',(1.,0.,0.));
#38982=DIRECTION('ref_axis',(0.,0.,-1.));
#38983=DIRECTION('center_axis',(1.,0.,0.));
#38984=DIRECTION('ref_axis',(0.,1.,0.));
#38985=DIRECTION('',(-0.707106781186542,0.707106781186553,8.659560562355E-17));
#38986=DIRECTION('center_axis',(-1.,0.,0.));
#38987=DIRECTION('ref_axis',(0.,1.,0.));
#38988=DIRECTION('',(0.707106781186533,0.707106781186562,-8.65956056235511E-17));
#38989=DIRECTION('center_axis',(1.,0.,0.));
#38990=DIRECTION('ref_axis',(0.,0.,-1.));
#38991=DIRECTION('center_axis',(1.,0.,0.));
#38992=DIRECTION('ref_axis',(0.,0.,-1.));
#38993=DIRECTION('axis',(0.,0.,1.));
#38994=DIRECTION('refdir',(1.,0.,0.));
#38995=DIRECTION('center_axis',(-1.,0.,0.));
#38996=DIRECTION('ref_axis',(0.,0.,-1.));
#38997=DIRECTION('center_axis',(1.,0.,0.));
#38998=DIRECTION('ref_axis',(0.,0.,-1.));
#38999=DIRECTION('',(-0.707106781186545,8.65956056235497E-17,0.70710678118655));
#39000=DIRECTION('center_axis',(-1.,0.,0.));
#39001=DIRECTION('ref_axis',(0.,0.,-1.));
#39002=DIRECTION('center_axis',(1.,0.,0.));
#39003=DIRECTION('ref_axis',(0.,0.,-1.));
#39004=DIRECTION('',(1.,0.,0.));
#39005=DIRECTION('center_axis',(1.,0.,0.));
#39006=DIRECTION('ref_axis',(0.,0.,-1.));
#39007=DIRECTION('center_axis',(1.,0.,0.));
#39008=DIRECTION('ref_axis',(0.,0.,-1.));
#39009=DIRECTION('center_axis',(-1.,0.,0.));
#39010=DIRECTION('ref_axis',(0.,0.,1.));
#39011=DIRECTION('',(0.,1.,0.));
#39012=DIRECTION('',(0.,0.,-1.));
#39013=DIRECTION('',(0.,-1.,0.));
#39014=DIRECTION('',(0.,0.,1.));
#39015=DIRECTION('center_axis',(-1.,0.,0.));
#39016=DIRECTION('ref_axis',(0.,1.,0.));
#39017=DIRECTION('',(-0.515038074910058,-0.85716730070211,1.04972719113862E-16));
#39018=DIRECTION('center_axis',(1.,0.,0.));
#39019=DIRECTION('ref_axis',(0.,0.,-1.));
#39020=DIRECTION('center_axis',(-1.,0.,0.));
#39021=DIRECTION('ref_axis',(0.,0.,-1.));
#39022=DIRECTION('',(0.707106781186545,-8.65956056235497E-17,0.70710678118655));
#39023=DIRECTION('center_axis',(1.,0.,0.));
#39024=DIRECTION('ref_axis',(0.,0.,-1.));
#39025=DIRECTION('center_axis',(-1.,0.,0.));
#39026=DIRECTION('ref_axis',(0.,0.,-1.));
#39027=DIRECTION('',(-1.,0.,0.));
#39028=DIRECTION('center_axis',(-1.,0.,0.));
#39029=DIRECTION('ref_axis',(0.,0.,-1.));
#39030=DIRECTION('center_axis',(-1.,0.,0.));
#39031=DIRECTION('ref_axis',(0.,0.,-1.));
#39032=DIRECTION('center_axis',(1.,0.,0.));
#39033=DIRECTION('ref_axis',(0.,0.,-1.));
#39034=DIRECTION('',(0.,1.,0.));
#39035=DIRECTION('',(0.,0.,1.));
#39036=DIRECTION('',(0.,-1.,0.));
#39037=DIRECTION('',(0.,0.,-1.));
#39038=DIRECTION('center_axis',(1.,0.,0.));
#39039=DIRECTION('ref_axis',(0.,1.,0.));
#39040=DIRECTION('',(0.515038074910058,-0.85716730070211,-1.04972719113862E-16));
#39041=DIRECTION('center_axis',(0.,-1.,0.));
#39042=DIRECTION('ref_axis',(1.,0.,0.));
#39043=DIRECTION('center_axis',(0.,1.,0.));
#39044=DIRECTION('ref_axis',(1.,0.,0.));
#39045=DIRECTION('',(-0.707106781186547,-0.707106781186548,-8.65956056235493E-17));
#39046=DIRECTION('center_axis',(0.,-1.,0.));
#39047=DIRECTION('ref_axis',(1.,0.,0.));
#39048=DIRECTION('center_axis',(0.,1.,0.));
#39049=DIRECTION('ref_axis',(1.,0.,0.));
#39050=DIRECTION('',(0.707106781186547,0.,-0.707106781186547));
#39051=DIRECTION('',(-1.,0.,0.));
#39052=DIRECTION('',(0.707106781186546,0.,0.707106781186549));
#39053=DIRECTION('',(-0.707106781186546,0.,0.707106781186549));
#39054=DIRECTION('',(1.,0.,0.));
#39055=DIRECTION('',(-0.707106781186546,0.,-0.707106781186549));
#39056=DIRECTION('center_axis',(0.,-1.,0.));
#39057=DIRECTION('ref_axis',(1.,0.,0.));
#39058=DIRECTION('center_axis',(0.,-1.,0.));
#39059=DIRECTION('ref_axis',(1.,0.,0.));
#39060=DIRECTION('center_axis',(0.,-1.,0.));
#39061=DIRECTION('ref_axis',(1.,0.,0.));
#39062=DIRECTION('center_axis',(0.,-1.,0.));
#39063=DIRECTION('ref_axis',(1.,0.,0.));
#39064=DIRECTION('center_axis',(0.,1.,0.));
#39065=DIRECTION('ref_axis',(1.,0.,0.));
#39066=DIRECTION('',(0.,1.,0.));
#39067=DIRECTION('center_axis',(0.,1.,0.));
#39068=DIRECTION('ref_axis',(1.,0.,0.));
#39069=DIRECTION('center_axis',(0.,-1.,0.));
#39070=DIRECTION('ref_axis',(1.,0.,0.));
#39071=DIRECTION('center_axis',(0.,1.,0.));
#39072=DIRECTION('ref_axis',(1.,0.,0.));
#39073=DIRECTION('',(-0.707106781186547,-0.707106781186548,-8.65956056235493E-17));
#39074=DIRECTION('center_axis',(0.,1.,0.));
#39075=DIRECTION('ref_axis',(1.,0.,0.));
#39076=DIRECTION('',(0.,1.,0.));
#39077=DIRECTION('center_axis',(0.,1.,0.));
#39078=DIRECTION('ref_axis',(1.,0.,0.));
#39079=DIRECTION('center_axis',(0.,-1.,0.));
#39080=DIRECTION('ref_axis',(1.,0.,0.));
#39081=DIRECTION('',(-0.857167300702115,-0.515038074910049,-1.04972719113862E-16));
#39082=DIRECTION('center_axis',(0.,-1.,0.));
#39083=DIRECTION('ref_axis',(1.,0.,0.));
#39084=DIRECTION('',(-0.857167300702115,-0.515038074910049,-1.04972719113862E-16));
#39085=DIRECTION('center_axis',(0.,-1.,0.));
#39086=DIRECTION('ref_axis',(1.,0.,0.));
#39087=DIRECTION('center_axis',(0.,1.,0.));
#39088=DIRECTION('ref_axis',(1.,0.,0.));
#39089=DIRECTION('',(-0.707106781186547,-0.707106781186548,-8.65956056235493E-17));
#39090=DIRECTION('center_axis',(0.,1.,0.));
#39091=DIRECTION('ref_axis',(1.,0.,0.));
#39092=DIRECTION('',(0.,1.,0.));
#39093=DIRECTION('center_axis',(0.,1.,0.));
#39094=DIRECTION('ref_axis',(1.,0.,0.));
#39095=DIRECTION('center_axis',(0.,-1.,0.));
#39096=DIRECTION('ref_axis',(1.,0.,0.));
#39097=DIRECTION('center_axis',(0.,1.,0.));
#39098=DIRECTION('ref_axis',(1.,0.,0.));
#39099=DIRECTION('',(-0.707106781186547,-0.707106781186548,-8.65956056235493E-17));
#39100=DIRECTION('center_axis',(0.,1.,0.));
#39101=DIRECTION('ref_axis',(1.,0.,0.));
#39102=DIRECTION('',(0.,1.,0.));
#39103=DIRECTION('center_axis',(0.,1.,0.));
#39104=DIRECTION('ref_axis',(1.,0.,0.));
#39105=DIRECTION('center_axis',(0.,1.,0.));
#39106=DIRECTION('ref_axis',(1.,0.,0.));
#39107=DIRECTION('center_axis',(0.,-1.,0.));
#39108=DIRECTION('ref_axis',(1.,0.,0.));
#39109=DIRECTION('center_axis',(0.,1.,0.));
#39110=DIRECTION('ref_axis',(1.,0.,0.));
#39111=DIRECTION('center_axis',(0.,-1.,0.));
#39112=DIRECTION('ref_axis',(1.,0.,0.));
#39113=DIRECTION('center_axis',(0.,1.,0.));
#39114=DIRECTION('ref_axis',(1.,0.,0.));
#39115=DIRECTION('',(0.,1.,0.));
#39116=DIRECTION('center_axis',(0.,-1.,0.));
#39117=DIRECTION('ref_axis',(1.,0.,0.));
#39118=DIRECTION('center_axis',(0.,1.,0.));
#39119=DIRECTION('ref_axis',(1.,0.,0.));
#39120=DIRECTION('',(0.,1.,0.));
#39121=DIRECTION('center_axis',(0.,-1.,0.));
#39122=DIRECTION('ref_axis',(1.,0.,0.));
#39123=DIRECTION('center_axis',(0.,1.,0.));
#39124=DIRECTION('ref_axis',(1.,0.,0.));
#39125=DIRECTION('center_axis',(0.,-1.,0.));
#39126=DIRECTION('ref_axis',(1.,0.,0.));
#39127=DIRECTION('',(-0.707106781186547,0.707106781186548,8.65956056235493E-17));
#39128=DIRECTION('center_axis',(0.,1.,0.));
#39129=DIRECTION('ref_axis',(1.,0.,0.));
#39130=DIRECTION('center_axis',(0.,1.,0.));
#39131=DIRECTION('ref_axis',(1.,0.,0.));
#39132=DIRECTION('center_axis',(0.,1.,0.));
#39133=DIRECTION('ref_axis',(1.,0.,0.));
#39134=DIRECTION('',(0.,1.,0.));
#39135=DIRECTION('center_axis',(0.,1.,0.));
#39136=DIRECTION('ref_axis',(0.,0.,1.));
#39137=DIRECTION('',(-0.707106781186547,0.,0.707106781186547));
#39138=DIRECTION('',(0.707106781186546,0.,0.707106781186549));
#39139=DIRECTION('',(-1.,0.,0.));
#39140=DIRECTION('',(0.707106781186546,0.,-0.707106781186549));
#39141=DIRECTION('',(-0.707106781186546,0.,-0.707106781186549));
#39142=DIRECTION('',(1.,0.,0.));
#39143=DIRECTION('center_axis',(0.,-1.,0.));
#39144=DIRECTION('ref_axis',(1.,0.,0.));
#39145=DIRECTION('',(-0.707106781186547,-0.707106781186548,-8.65956056235493E-17));
#39146=DIRECTION('center_axis',(0.707106781186548,0.,0.707106781186548));
#39147=DIRECTION('ref_axis',(0.707106781186548,0.,-0.707106781186548));
#39148=DIRECTION('',(0.,-1.,0.));
#39149=DIRECTION('center_axis',(0.,0.,1.));
#39150=DIRECTION('ref_axis',(1.,0.,0.));
#39151=DIRECTION('',(0.,1.,0.));
#39152=DIRECTION('center_axis',(0.707106781186549,0.,-0.707106781186546));
#39153=DIRECTION('ref_axis',(-0.707106781186546,0.,-0.707106781186549));
#39154=DIRECTION('',(0.,1.,0.));
#39155=DIRECTION('center_axis',(0.,0.,-1.));
#39156=DIRECTION('ref_axis',(-1.,0.,0.));
#39157=DIRECTION('',(0.,-1.,0.));
#39158=DIRECTION('center_axis',(-0.707106781186549,0.,-0.707106781186546));
#39159=DIRECTION('ref_axis',(-0.707106781186546,0.,0.707106781186549));
#39160=DIRECTION('center_axis',(-0.707106781186549,0.,0.707106781186546));
#39161=DIRECTION('ref_axis',(0.707106781186546,0.,0.707106781186549));
#39162=DIRECTION('axis',(0.,0.,1.));
#39163=DIRECTION('refdir',(1.,0.,0.));
#39164=DIRECTION('center_axis',(0.,1.,0.));
#39165=DIRECTION('ref_axis',(1.,0.,0.));
#39166=DIRECTION('',(0.,-1.,0.));
#39167=DIRECTION('center_axis',(0.,-1.,0.));
#39168=DIRECTION('ref_axis',(1.,0.,0.));
#39169=DIRECTION('center_axis',(0.,1.,0.));
#39170=DIRECTION('ref_axis',(1.,0.,0.));
#39171=DIRECTION('',(0.,-1.,0.));
#39172=DIRECTION('center_axis',(0.,1.,0.));
#39173=DIRECTION('ref_axis',(1.,0.,0.));
#39174=DIRECTION('',(0.,-1.,0.));
#39175=DIRECTION('center_axis',(0.,1.,0.));
#39176=DIRECTION('ref_axis',(1.,0.,0.));
#39177=DIRECTION('',(0.,-1.,0.));
#39178=DIRECTION('center_axis',(0.,1.,0.));
#39179=DIRECTION('ref_axis',(1.,0.,0.));
#39180=DIRECTION('',(0.,-1.,0.));
#39181=DIRECTION('center_axis',(0.,1.,0.));
#39182=DIRECTION('ref_axis',(1.,0.,0.));
#39183=DIRECTION('',(0.,-1.,0.));
#39184=DIRECTION('center_axis',(0.,1.,0.));
#39185=DIRECTION('ref_axis',(1.,0.,0.));
#39186=DIRECTION('',(0.,-1.,0.));
#39187=DIRECTION('center_axis',(0.,1.,0.));
#39188=DIRECTION('ref_axis',(1.,0.,0.));
#39189=DIRECTION('',(0.,-1.,0.));
#39190=DIRECTION('center_axis',(0.,1.,0.));
#39191=DIRECTION('ref_axis',(1.,0.,0.));
#39192=DIRECTION('',(0.,-1.,0.));
#39193=DIRECTION('center_axis',(0.,1.,0.));
#39194=DIRECTION('ref_axis',(1.,0.,0.));
#39195=DIRECTION('',(0.,-1.,0.));
#39196=DIRECTION('center_axis',(0.,1.,0.));
#39197=DIRECTION('ref_axis',(1.,0.,0.));
#39198=DIRECTION('',(0.,-1.,0.));
#39199=DIRECTION('center_axis',(0.,1.,0.));
#39200=DIRECTION('ref_axis',(1.,0.,0.));
#39201=DIRECTION('',(0.,-1.,0.));
#39202=DIRECTION('center_axis',(0.,1.,0.));
#39203=DIRECTION('ref_axis',(1.,0.,0.));
#39204=DIRECTION('',(0.,-1.,0.));
#39205=DIRECTION('center_axis',(0.,1.,0.));
#39206=DIRECTION('ref_axis',(1.,0.,0.));
#39207=DIRECTION('',(0.,-1.,0.));
#39208=DIRECTION('center_axis',(0.,1.,0.));
#39209=DIRECTION('ref_axis',(1.,0.,0.));
#39210=DIRECTION('',(0.,-1.,0.));
#39211=DIRECTION('center_axis',(0.,1.,0.));
#39212=DIRECTION('ref_axis',(1.,0.,0.));
#39213=DIRECTION('',(0.,-1.,0.));
#39214=DIRECTION('center_axis',(0.,1.,0.));
#39215=DIRECTION('ref_axis',(1.,0.,0.));
#39216=DIRECTION('',(0.,-1.,0.));
#39217=DIRECTION('center_axis',(0.,1.,0.));
#39218=DIRECTION('ref_axis',(1.,0.,0.));
#39219=DIRECTION('',(0.,-1.,0.));
#39220=DIRECTION('center_axis',(0.,1.,0.));
#39221=DIRECTION('ref_axis',(1.,0.,0.));
#39222=DIRECTION('',(0.,-1.,0.));
#39223=DIRECTION('center_axis',(0.,1.,0.));
#39224=DIRECTION('ref_axis',(1.,0.,0.));
#39225=DIRECTION('',(0.,-1.,0.));
#39226=DIRECTION('center_axis',(0.,1.,0.));
#39227=DIRECTION('ref_axis',(1.,0.,0.));
#39228=DIRECTION('',(0.,-1.,0.));
#39229=DIRECTION('center_axis',(0.,1.,0.));
#39230=DIRECTION('ref_axis',(1.,0.,0.));
#39231=DIRECTION('',(0.,-1.,0.));
#39232=DIRECTION('center_axis',(0.,1.,0.));
#39233=DIRECTION('ref_axis',(1.,0.,0.));
#39234=DIRECTION('',(0.,-1.,0.));
#39235=DIRECTION('center_axis',(0.,1.,0.));
#39236=DIRECTION('ref_axis',(-0.160387124847653,0.,0.987054188068266));
#39237=DIRECTION('',(0.,-1.,0.));
#39238=DIRECTION('center_axis',(0.,-1.,0.));
#39239=DIRECTION('ref_axis',(1.,0.,-2.68659360660725E-14));
#39240=DIRECTION('center_axis',(0.,1.,0.));
#39241=DIRECTION('ref_axis',(-0.160387124847653,0.,0.987054188068266));
#39242=DIRECTION('',(0.,-1.,0.));
#39243=DIRECTION('center_axis',(0.,1.,0.));
#39244=DIRECTION('ref_axis',(-0.160387124847653,0.,0.987054188068266));
#39245=DIRECTION('',(0.,-1.,0.));
#39246=DIRECTION('center_axis',(0.,1.,0.));
#39247=DIRECTION('ref_axis',(-0.160387124847653,0.,0.987054188068266));
#39248=DIRECTION('',(0.,-1.,0.));
#39249=DIRECTION('center_axis',(0.,1.,0.));
#39250=DIRECTION('ref_axis',(-0.160387124847653,0.,0.987054188068266));
#39251=DIRECTION('',(0.,-1.,0.));
#39252=DIRECTION('center_axis',(0.,1.,0.));
#39253=DIRECTION('ref_axis',(-0.160387124847653,0.,0.987054188068266));
#39254=DIRECTION('',(0.,-1.,0.));
#39255=DIRECTION('center_axis',(0.,1.,0.));
#39256=DIRECTION('ref_axis',(-0.160387124847653,0.,0.987054188068266));
#39257=DIRECTION('',(0.,-1.,0.));
#39258=DIRECTION('center_axis',(0.,1.,0.));
#39259=DIRECTION('ref_axis',(-0.160387124847653,0.,0.987054188068266));
#39260=DIRECTION('',(0.,-1.,0.));
#39261=DIRECTION('center_axis',(0.,1.,0.));
#39262=DIRECTION('ref_axis',(-0.160387124847653,0.,0.987054188068266));
#39263=DIRECTION('',(0.,-1.,0.));
#39264=DIRECTION('center_axis',(0.,1.,0.));
#39265=DIRECTION('ref_axis',(-0.160387124847653,0.,0.987054188068266));
#39266=DIRECTION('',(0.,-1.,0.));
#39267=DIRECTION('center_axis',(0.,1.,0.));
#39268=DIRECTION('ref_axis',(-0.160387124847653,0.,0.987054188068266));
#39269=DIRECTION('',(0.,-1.,0.));
#39270=DIRECTION('center_axis',(0.,1.,0.));
#39271=DIRECTION('ref_axis',(-0.160387124847653,0.,0.987054188068266));
#39272=DIRECTION('',(0.,-1.,0.));
#39273=DIRECTION('center_axis',(0.,1.,0.));
#39274=DIRECTION('ref_axis',(-0.160387124847653,0.,0.987054188068266));
#39275=DIRECTION('',(0.,-1.,0.));
#39276=DIRECTION('center_axis',(0.,1.,0.));
#39277=DIRECTION('ref_axis',(-0.160387124847653,0.,0.987054188068266));
#39278=DIRECTION('',(0.,-1.,0.));
#39279=DIRECTION('center_axis',(0.,1.,0.));
#39280=DIRECTION('ref_axis',(-0.160387124847653,0.,0.987054188068266));
#39281=DIRECTION('',(0.,-1.,0.));
#39282=DIRECTION('center_axis',(0.,1.,0.));
#39283=DIRECTION('ref_axis',(-0.160387124847653,0.,0.987054188068266));
#39284=DIRECTION('',(0.,-1.,0.));
#39285=DIRECTION('center_axis',(0.,1.,0.));
#39286=DIRECTION('ref_axis',(-0.160387124847653,0.,0.987054188068266));
#39287=DIRECTION('',(0.,-1.,0.));
#39288=DIRECTION('center_axis',(0.,1.,0.));
#39289=DIRECTION('ref_axis',(-0.160387124847653,0.,0.987054188068266));
#39290=DIRECTION('',(0.,-1.,0.));
#39291=DIRECTION('center_axis',(0.,1.,0.));
#39292=DIRECTION('ref_axis',(-0.160387124847653,0.,0.987054188068266));
#39293=DIRECTION('',(0.,-1.,0.));
#39294=DIRECTION('center_axis',(0.,1.,0.));
#39295=DIRECTION('ref_axis',(-0.160387124847653,0.,0.987054188068266));
#39296=DIRECTION('',(0.,-1.,0.));
#39297=DIRECTION('center_axis',(0.,1.,0.));
#39298=DIRECTION('ref_axis',(-0.160387124847653,0.,0.987054188068266));
#39299=DIRECTION('',(0.,-1.,0.));
#39300=DIRECTION('center_axis',(0.,1.,0.));
#39301=DIRECTION('ref_axis',(-0.160387124847653,0.,0.987054188068266));
#39302=DIRECTION('',(0.,-1.,0.));
#39303=DIRECTION('center_axis',(0.,1.,0.));
#39304=DIRECTION('ref_axis',(-0.160387124847653,0.,0.987054188068266));
#39305=DIRECTION('',(0.,-1.,0.));
#39306=DIRECTION('center_axis',(0.,1.,0.));
#39307=DIRECTION('ref_axis',(-0.160387124847653,0.,0.987054188068266));
#39308=DIRECTION('center_axis',(0.,1.,0.));
#39309=DIRECTION('ref_axis',(1.,0.,-2.68659360660725E-14));
#39310=DIRECTION('center_axis',(0.,1.,0.));
#39311=DIRECTION('ref_axis',(1.,0.,0.));
#39312=DIRECTION('center_axis',(0.,1.,0.));
#39313=DIRECTION('ref_axis',(1.,0.,0.));
#39314=DIRECTION('center_axis',(0.,1.,0.));
#39315=DIRECTION('ref_axis',(0.,0.,1.));
#39316=DIRECTION('center_axis',(0.,1.,0.));
#39317=DIRECTION('ref_axis',(1.,0.,0.));
#39318=DIRECTION('center_axis',(0.,1.,0.));
#39319=DIRECTION('ref_axis',(1.,0.,0.));
#39320=DIRECTION('center_axis',(0.,1.,0.));
#39321=DIRECTION('ref_axis',(0.,0.,1.));
#39322=DIRECTION('center_axis',(0.,-1.,0.));
#39323=DIRECTION('ref_axis',(1.,0.,0.));
#39324=DIRECTION('center_axis',(0.,-1.,0.));
#39325=DIRECTION('ref_axis',(1.,0.,0.));
#39326=DIRECTION('center_axis',(0.,-1.,0.));
#39327=DIRECTION('ref_axis',(0.,0.,-1.));
#39328=DIRECTION('center_axis',(0.,1.,0.));
#39329=DIRECTION('ref_axis',(1.,0.,0.));
#39330=DIRECTION('center_axis',(1.,0.,0.));
#39331=DIRECTION('ref_axis',(0.,0.,1.));
#39332=DIRECTION('center_axis',(0.,1.,0.));
#39333=DIRECTION('ref_axis',(1.,0.,0.));
#39334=DIRECTION('center_axis',(0.,-1.,0.));
#39335=DIRECTION('ref_axis',(1.,0.,0.));
#39336=DIRECTION('center_axis',(0.,-1.,0.));
#39337=DIRECTION('ref_axis',(1.,0.,0.));
#39338=DIRECTION('',(0.707106781186547,0.707106781186549,8.65956056235492E-17));
#39339=DIRECTION('center_axis',(0.,-1.,0.));
#39340=DIRECTION('ref_axis',(1.,0.,0.));
#39341=DIRECTION('center_axis',(0.,1.,0.));
#39342=DIRECTION('ref_axis',(1.,0.,0.));
#39343=DIRECTION('center_axis',(0.,1.,0.));
#39344=DIRECTION('ref_axis',(-0.17364817766693,0.,0.984807753012208));
#39345=DIRECTION('center_axis',(0.,1.,0.));
#39346=DIRECTION('ref_axis',(1.,0.,0.));
#39347=DIRECTION('',(0.869726513699833,0.,0.49353398197848));
#39348=DIRECTION('',(-0.986074150277955,0.,0.166306254102512));
#39349=DIRECTION('center_axis',(-0.166306254102512,0.,-0.986074150277955));
#39350=DIRECTION('ref_axis',(-0.986074150277955,0.,0.166306254102512));
#39351=DIRECTION('',(0.,-1.,0.));
#39352=DIRECTION('',(0.,1.,0.));
#39353=DIRECTION('center_axis',(-0.49353398197848,0.,0.869726513699833));
#39354=DIRECTION('ref_axis',(0.869726513699833,0.,0.49353398197848));
#39355=DIRECTION('',(0.,1.,0.));
#39356=DIRECTION('center_axis',(0.,-1.,0.));
#39357=DIRECTION('ref_axis',(1.,0.,0.));
#39358=DIRECTION('center_axis',(0.,1.,0.));
#39359=DIRECTION('ref_axis',(1.,0.,0.));
#39360=DIRECTION('',(0.,1.,0.));
#39361=DIRECTION('center_axis',(0.,1.,0.));
#39362=DIRECTION('ref_axis',(1.,0.,0.));
#39363=DIRECTION('center_axis',(0.,1.,0.));
#39364=DIRECTION('ref_axis',(1.,0.,0.));
#39365=DIRECTION('center_axis',(0.,1.,0.));
#39366=DIRECTION('ref_axis',(1.,0.,0.));
#39367=DIRECTION('',(0.,-1.,0.));
#39368=DIRECTION('center_axis',(0.,-1.,0.));
#39369=DIRECTION('ref_axis',(1.,0.,0.));
#39370=DIRECTION('',(0.,1.,0.));
#39371=DIRECTION('center_axis',(0.,1.,0.));
#39372=DIRECTION('ref_axis',(1.,0.,0.));
#39373=DIRECTION('',(0.,-1.,0.));
#39374=DIRECTION('center_axis',(0.,-1.,0.));
#39375=DIRECTION('ref_axis',(1.,0.,0.));
#39376=DIRECTION('',(0.,1.,0.));
#39377=DIRECTION('center_axis',(0.,1.,0.));
#39378=DIRECTION('ref_axis',(1.,0.,0.));
#39379=DIRECTION('',(0.,-1.,0.));
#39380=DIRECTION('center_axis',(0.,-1.,0.));
#39381=DIRECTION('ref_axis',(1.,0.,0.));
#39382=DIRECTION('',(0.,1.,0.));
#39383=DIRECTION('center_axis',(0.,1.,0.));
#39384=DIRECTION('ref_axis',(1.,0.,0.));
#39385=DIRECTION('',(0.,-1.,0.));
#39386=DIRECTION('center_axis',(0.,-1.,0.));
#39387=DIRECTION('ref_axis',(1.,0.,0.));
#39388=DIRECTION('',(0.,1.,0.));
#39389=DIRECTION('center_axis',(0.,1.,0.));
#39390=DIRECTION('ref_axis',(1.,0.,0.));
#39391=DIRECTION('',(0.,-1.,0.));
#39392=DIRECTION('center_axis',(0.,-1.,0.));
#39393=DIRECTION('ref_axis',(1.,0.,0.));
#39394=DIRECTION('',(0.,1.,0.));
#39395=DIRECTION('center_axis',(0.,1.,0.));
#39396=DIRECTION('ref_axis',(1.,0.,0.));
#39397=DIRECTION('',(0.,-1.,0.));
#39398=DIRECTION('center_axis',(0.,-1.,0.));
#39399=DIRECTION('ref_axis',(1.,0.,0.));
#39400=DIRECTION('',(0.,1.,0.));
#39401=DIRECTION('center_axis',(0.,1.,0.));
#39402=DIRECTION('ref_axis',(1.,0.,0.));
#39403=DIRECTION('',(0.,-1.,0.));
#39404=DIRECTION('center_axis',(0.,-1.,0.));
#39405=DIRECTION('ref_axis',(1.,0.,0.));
#39406=DIRECTION('',(0.,1.,0.));
#39407=DIRECTION('center_axis',(0.,1.,0.));
#39408=DIRECTION('ref_axis',(1.,0.,0.));
#39409=DIRECTION('',(0.,-1.,0.));
#39410=DIRECTION('center_axis',(0.,-1.,0.));
#39411=DIRECTION('ref_axis',(1.,0.,0.));
#39412=DIRECTION('',(0.,1.,0.));
#39413=DIRECTION('center_axis',(0.,1.,0.));
#39414=DIRECTION('ref_axis',(1.,0.,0.));
#39415=DIRECTION('',(0.,-1.,0.));
#39416=DIRECTION('center_axis',(0.,-1.,0.));
#39417=DIRECTION('ref_axis',(1.,0.,0.));
#39418=DIRECTION('',(0.,1.,0.));
#39419=DIRECTION('center_axis',(0.,1.,0.));
#39420=DIRECTION('ref_axis',(1.,0.,0.));
#39421=DIRECTION('',(0.,-1.,0.));
#39422=DIRECTION('center_axis',(0.,-1.,0.));
#39423=DIRECTION('ref_axis',(1.,0.,0.));
#39424=DIRECTION('',(0.,1.,0.));
#39425=DIRECTION('center_axis',(0.,1.,0.));
#39426=DIRECTION('ref_axis',(1.,0.,0.));
#39427=DIRECTION('',(0.,-1.,0.));
#39428=DIRECTION('center_axis',(0.,-1.,0.));
#39429=DIRECTION('ref_axis',(1.,0.,0.));
#39430=DIRECTION('',(0.,1.,0.));
#39431=DIRECTION('center_axis',(0.,1.,0.));
#39432=DIRECTION('ref_axis',(1.,0.,0.));
#39433=DIRECTION('',(0.,-1.,0.));
#39434=DIRECTION('center_axis',(0.,-1.,0.));
#39435=DIRECTION('ref_axis',(1.,0.,0.));
#39436=DIRECTION('',(0.,1.,0.));
#39437=DIRECTION('center_axis',(0.,1.,0.));
#39438=DIRECTION('ref_axis',(1.,0.,0.));
#39439=DIRECTION('',(0.,-1.,0.));
#39440=DIRECTION('center_axis',(0.,-1.,0.));
#39441=DIRECTION('ref_axis',(1.,0.,0.));
#39442=DIRECTION('',(0.,1.,0.));
#39443=DIRECTION('center_axis',(0.,1.,0.));
#39444=DIRECTION('ref_axis',(1.,0.,0.));
#39445=DIRECTION('',(0.,-1.,0.));
#39446=DIRECTION('center_axis',(0.,-1.,0.));
#39447=DIRECTION('ref_axis',(1.,0.,0.));
#39448=DIRECTION('',(0.,1.,0.));
#39449=DIRECTION('center_axis',(0.,1.,0.));
#39450=DIRECTION('ref_axis',(1.,0.,0.));
#39451=DIRECTION('',(0.,-1.,0.));
#39452=DIRECTION('center_axis',(0.,-1.,0.));
#39453=DIRECTION('ref_axis',(1.,0.,0.));
#39454=DIRECTION('',(0.,1.,0.));
#39455=DIRECTION('center_axis',(0.,1.,0.));
#39456=DIRECTION('ref_axis',(1.,0.,0.));
#39457=DIRECTION('',(0.,-1.,0.));
#39458=DIRECTION('center_axis',(0.,-1.,0.));
#39459=DIRECTION('ref_axis',(1.,0.,0.));
#39460=DIRECTION('',(0.,1.,0.));
#39461=DIRECTION('center_axis',(0.,1.,0.));
#39462=DIRECTION('ref_axis',(1.,0.,0.));
#39463=DIRECTION('',(0.,-1.,0.));
#39464=DIRECTION('center_axis',(0.,-1.,0.));
#39465=DIRECTION('ref_axis',(1.,0.,0.));
#39466=DIRECTION('center_axis',(0.,-1.,0.));
#39467=DIRECTION('ref_axis',(1.,0.,0.));
#39468=DIRECTION('',(0.,1.,0.));
#39469=DIRECTION('center_axis',(0.,1.,0.));
#39470=DIRECTION('ref_axis',(1.,0.,0.));
#39471=DIRECTION('',(0.,-1.,0.));
#39472=DIRECTION('center_axis',(0.,-1.,0.));
#39473=DIRECTION('ref_axis',(1.,0.,0.));
#39474=DIRECTION('',(0.,1.,0.));
#39475=DIRECTION('center_axis',(0.,1.,0.));
#39476=DIRECTION('ref_axis',(1.,0.,0.));
#39477=DIRECTION('',(0.,-1.,0.));
#39478=DIRECTION('center_axis',(0.,-1.,0.));
#39479=DIRECTION('ref_axis',(1.,0.,0.));
#39480=DIRECTION('',(0.,1.,0.));
#39481=DIRECTION('center_axis',(0.,1.,0.));
#39482=DIRECTION('ref_axis',(1.,0.,0.));
#39483=DIRECTION('',(0.,-1.,0.));
#39484=DIRECTION('center_axis',(0.,-1.,0.));
#39485=DIRECTION('ref_axis',(1.,0.,0.));
#39486=DIRECTION('',(0.,1.,0.));
#39487=DIRECTION('center_axis',(0.,1.,0.));
#39488=DIRECTION('ref_axis',(1.,0.,0.));
#39489=DIRECTION('',(0.,-1.,0.));
#39490=DIRECTION('center_axis',(0.,-1.,0.));
#39491=DIRECTION('ref_axis',(1.,0.,0.));
#39492=DIRECTION('',(0.,1.,0.));
#39493=DIRECTION('center_axis',(0.,1.,0.));
#39494=DIRECTION('ref_axis',(1.,0.,0.));
#39495=DIRECTION('',(0.,-1.,0.));
#39496=DIRECTION('center_axis',(0.,-1.,0.));
#39497=DIRECTION('ref_axis',(1.,0.,0.));
#39498=DIRECTION('',(0.,1.,0.));
#39499=DIRECTION('center_axis',(0.,1.,0.));
#39500=DIRECTION('ref_axis',(1.,0.,0.));
#39501=DIRECTION('',(0.,-1.,0.));
#39502=DIRECTION('center_axis',(0.,-1.,0.));
#39503=DIRECTION('ref_axis',(1.,0.,0.));
#39504=DIRECTION('',(0.,1.,0.));
#39505=DIRECTION('center_axis',(0.,1.,0.));
#39506=DIRECTION('ref_axis',(1.,0.,0.));
#39507=DIRECTION('',(0.,-1.,0.));
#39508=DIRECTION('center_axis',(0.,-1.,0.));
#39509=DIRECTION('ref_axis',(1.,0.,0.));
#39510=DIRECTION('',(0.,1.,0.));
#39511=DIRECTION('center_axis',(0.,1.,0.));
#39512=DIRECTION('ref_axis',(1.,0.,0.));
#39513=DIRECTION('',(0.,-1.,0.));
#39514=DIRECTION('center_axis',(0.,-1.,0.));
#39515=DIRECTION('ref_axis',(1.,0.,0.));
#39516=DIRECTION('',(0.,1.,0.));
#39517=DIRECTION('center_axis',(0.,1.,0.));
#39518=DIRECTION('ref_axis',(1.,0.,0.));
#39519=DIRECTION('',(0.,-1.,0.));
#39520=DIRECTION('center_axis',(0.,-1.,0.));
#39521=DIRECTION('ref_axis',(1.,0.,0.));
#39522=DIRECTION('',(0.,1.,0.));
#39523=DIRECTION('center_axis',(0.,1.,0.));
#39524=DIRECTION('ref_axis',(1.,0.,0.));
#39525=DIRECTION('',(0.,-1.,0.));
#39526=DIRECTION('center_axis',(0.,-1.,0.));
#39527=DIRECTION('ref_axis',(1.,0.,0.));
#39528=DIRECTION('',(0.,1.,0.));
#39529=DIRECTION('center_axis',(0.,1.,0.));
#39530=DIRECTION('ref_axis',(1.,0.,0.));
#39531=DIRECTION('',(0.,-1.,0.));
#39532=DIRECTION('center_axis',(0.,-1.,0.));
#39533=DIRECTION('ref_axis',(1.,0.,0.));
#39534=DIRECTION('',(0.,1.,0.));
#39535=DIRECTION('center_axis',(0.,1.,0.));
#39536=DIRECTION('ref_axis',(1.,0.,0.));
#39537=DIRECTION('',(0.,-1.,0.));
#39538=DIRECTION('center_axis',(0.,-1.,0.));
#39539=DIRECTION('ref_axis',(1.,0.,0.));
#39540=DIRECTION('',(0.,1.,0.));
#39541=DIRECTION('center_axis',(0.,1.,0.));
#39542=DIRECTION('ref_axis',(1.,0.,0.));
#39543=DIRECTION('',(0.,-1.,0.));
#39544=DIRECTION('center_axis',(0.,-1.,0.));
#39545=DIRECTION('ref_axis',(1.,0.,0.));
#39546=DIRECTION('',(0.,1.,0.));
#39547=DIRECTION('center_axis',(0.,1.,0.));
#39548=DIRECTION('ref_axis',(1.,0.,0.));
#39549=DIRECTION('',(0.,-1.,0.));
#39550=DIRECTION('center_axis',(0.,-1.,0.));
#39551=DIRECTION('ref_axis',(1.,0.,0.));
#39552=DIRECTION('',(0.,1.,0.));
#39553=DIRECTION('center_axis',(0.,1.,0.));
#39554=DIRECTION('ref_axis',(1.,0.,0.));
#39555=DIRECTION('',(0.,-1.,0.));
#39556=DIRECTION('center_axis',(0.,-1.,0.));
#39557=DIRECTION('ref_axis',(1.,0.,0.));
#39558=DIRECTION('',(0.,1.,0.));
#39559=DIRECTION('center_axis',(0.,1.,0.));
#39560=DIRECTION('ref_axis',(1.,0.,0.));
#39561=DIRECTION('',(0.,-1.,0.));
#39562=DIRECTION('center_axis',(0.,-1.,0.));
#39563=DIRECTION('ref_axis',(1.,0.,0.));
#39564=DIRECTION('',(0.,1.,0.));
#39565=DIRECTION('center_axis',(0.,1.,0.));
#39566=DIRECTION('ref_axis',(1.,0.,0.));
#39567=DIRECTION('',(0.,-1.,0.));
#39568=DIRECTION('center_axis',(0.,-1.,0.));
#39569=DIRECTION('ref_axis',(1.,0.,0.));
#39570=DIRECTION('',(0.,1.,0.));
#39571=DIRECTION('center_axis',(0.,1.,0.));
#39572=DIRECTION('ref_axis',(1.,0.,0.));
#39573=DIRECTION('',(0.,-1.,0.));
#39574=DIRECTION('center_axis',(0.,-1.,0.));
#39575=DIRECTION('ref_axis',(1.,0.,0.));
#39576=DIRECTION('',(0.,1.,0.));
#39577=DIRECTION('center_axis',(0.0074502908256619,0.,-0.99997224619817));
#39578=DIRECTION('ref_axis',(-0.99997224619817,0.,-0.0074502908256619));
#39579=DIRECTION('',(-0.99997224619817,0.,-0.0074502908256619));
#39580=DIRECTION('',(0.,1.,0.));
#39581=DIRECTION('center_axis',(-0.637062515999984,0.,0.770812137104606));
#39582=DIRECTION('ref_axis',(0.770812137104606,0.,0.637062515999984));
#39583=DIRECTION('',(0.770812137104606,0.,0.637062515999984));
#39584=DIRECTION('center_axis',(0.,1.,0.));
#39585=DIRECTION('ref_axis',(-0.342020143325669,0.,0.939692620785908));
#39586=DIRECTION('center_axis',(0.,1.,0.));
#39587=DIRECTION('ref_axis',(1.,0.,0.));
#39588=DIRECTION('',(0.707106781186547,-0.707106781186548,-8.65956056235493E-17));
#39589=DIRECTION('center_axis',(0.,1.,0.));
#39590=DIRECTION('ref_axis',(1.,0.,0.));
#39591=DIRECTION('center_axis',(0.,1.,0.));
#39592=DIRECTION('ref_axis',(-0.5,0.,0.866025403784438));
#39593=DIRECTION('',(0.648477023773219,0.,0.761234227842015));
#39594=DIRECTION('',(-0.983486691428025,0.,-0.180980462437127));
#39595=DIRECTION('center_axis',(0.180980462437127,0.,-0.983486691428025));
#39596=DIRECTION('ref_axis',(-0.983486691428025,0.,-0.180980462437127));
#39597=DIRECTION('',(0.,1.,0.));
#39598=DIRECTION('center_axis',(-0.761234227842015,0.,0.648477023773219));
#39599=DIRECTION('ref_axis',(0.648477023773219,0.,0.761234227842015));
#39600=DIRECTION('center_axis',(0.349011634277972,0.,-0.937118391207119));
#39601=DIRECTION('ref_axis',(-0.937118391207119,0.,-0.349011634277972));
#39602=DIRECTION('',(-0.937118391207119,0.,-0.349011634277972));
#39603=DIRECTION('',(0.,1.,0.));
#39604=DIRECTION('center_axis',(-0.862276222874172,0.,0.506438264219689));
#39605=DIRECTION('ref_axis',(0.506438264219689,0.,0.862276222874172));
#39606=DIRECTION('',(0.506438264219689,0.,0.862276222874172));
#39607=DIRECTION('center_axis',(0.,1.,0.));
#39608=DIRECTION('ref_axis',(-0.64278760968654,0.,0.766044443118978));
#39609=DIRECTION('center_axis',(0.,1.,0.));
#39610=DIRECTION('ref_axis',(-0.766044443118978,0.,0.642787609686539));
#39611=DIRECTION('',(0.349011634277972,0.,0.937118391207119));
#39612=DIRECTION('',(-0.862276222874171,0.,-0.50643826421969));
#39613=DIRECTION('center_axis',(0.50643826421969,0.,-0.862276222874171));
#39614=DIRECTION('ref_axis',(-0.862276222874171,0.,-0.50643826421969));
#39615=DIRECTION('',(0.,1.,0.));
#39616=DIRECTION('center_axis',(-0.937118391207119,0.,0.349011634277972));
#39617=DIRECTION('ref_axis',(0.349011634277972,0.,0.937118391207119));
#39618=DIRECTION('center_axis',(0.648477023773219,0.,-0.761234227842014));
#39619=DIRECTION('ref_axis',(-0.761234227842014,0.,-0.648477023773219));
#39620=DIRECTION('',(-0.761234227842014,0.,-0.648477023773219));
#39621=DIRECTION('',(0.,1.,0.));
#39622=DIRECTION('center_axis',(-0.983486691428025,0.,0.180980462437126));
#39623=DIRECTION('ref_axis',(0.180980462437126,0.,0.983486691428025));
#39624=DIRECTION('',(0.180980462437126,0.,0.983486691428025));
#39625=DIRECTION('center_axis',(0.,1.,0.));
#39626=DIRECTION('ref_axis',(-0.866025403784439,0.,0.5));
#39627=DIRECTION('center_axis',(0.,1.,0.));
#39628=DIRECTION('ref_axis',(-0.939692620785909,0.,0.342020143325668));
#39629=DIRECTION('',(0.00745029082566051,0.,0.99997224619817));
#39630=DIRECTION('',(-0.637062515999983,0.,-0.770812137104607));
#39631=DIRECTION('center_axis',(0.770812137104607,0.,-0.637062515999983));
#39632=DIRECTION('ref_axis',(-0.637062515999983,0.,-0.770812137104607));
#39633=DIRECTION('',(0.,1.,0.));
#39634=DIRECTION('center_axis',(-0.99997224619817,0.,0.00745029082566051));
#39635=DIRECTION('ref_axis',(0.00745029082566051,0.,0.99997224619817));
#39636=DIRECTION('center_axis',(0.869726513699833,0.,-0.49353398197848));
#39637=DIRECTION('ref_axis',(-0.49353398197848,0.,-0.869726513699833));
#39638=DIRECTION('',(-0.49353398197848,0.,-0.869726513699833));
#39639=DIRECTION('',(0.,1.,0.));
#39640=DIRECTION('center_axis',(-0.986074150277955,0.,-0.166306254102513));
#39641=DIRECTION('ref_axis',(-0.166306254102513,0.,0.986074150277955));
#39642=DIRECTION('',(-0.166306254102513,0.,0.986074150277955));
#39643=DIRECTION('center_axis',(0.,1.,0.));
#39644=DIRECTION('ref_axis',(-0.984807753012208,0.,0.17364817766693));
#39645=DIRECTION('center_axis',(0.,1.,0.));
#39646=DIRECTION('ref_axis',(-1.,0.,-1.83697019872103E-16));
#39647=DIRECTION('',(-0.335009667654806,0.,0.94221469027914));
#39648=DIRECTION('',(-0.335009667654806,0.,-0.94221469027914));
#39649=DIRECTION('center_axis',(0.94221469027914,0.,-0.335009667654806));
#39650=DIRECTION('ref_axis',(-0.335009667654806,0.,-0.94221469027914));
#39651=DIRECTION('',(0.,1.,0.));
#39652=DIRECTION('center_axis',(-0.94221469027914,0.,-0.335009667654806));
#39653=DIRECTION('ref_axis',(-0.335009667654806,0.,0.94221469027914));
#39654=DIRECTION('center_axis',(0.986074150277955,0.,-0.166306254102512));
#39655=DIRECTION('ref_axis',(-0.166306254102512,0.,-0.986074150277955));
#39656=DIRECTION('',(-0.166306254102512,0.,-0.986074150277955));
#39657=DIRECTION('',(0.,1.,0.));
#39658=DIRECTION('center_axis',(-0.869726513699833,0.,-0.49353398197848));
#39659=DIRECTION('ref_axis',(-0.49353398197848,0.,0.869726513699833));
#39660=DIRECTION('',(-0.49353398197848,0.,0.869726513699833));
#39661=DIRECTION('center_axis',(0.,1.,0.));
#39662=DIRECTION('ref_axis',(-0.984807753012208,0.,-0.17364817766693));
#39663=DIRECTION('center_axis',(0.,1.,0.));
#39664=DIRECTION('ref_axis',(-0.939692620785908,0.,-0.342020143325669));
#39665=DIRECTION('',(-0.637062515999984,0.,0.770812137104606));
#39666=DIRECTION('',(0.00745029082566179,0.,-0.99997224619817));
#39667=DIRECTION('center_axis',(0.99997224619817,0.,0.00745029082566179));
#39668=DIRECTION('ref_axis',(0.00745029082566179,0.,-0.99997224619817));
#39669=DIRECTION('',(0.,1.,0.));
#39670=DIRECTION('center_axis',(-0.770812137104606,0.,-0.637062515999984));
#39671=DIRECTION('ref_axis',(-0.637062515999984,0.,0.770812137104606));
#39672=DIRECTION('center_axis',(0.983486691428025,0.,0.180980462437127));
#39673=DIRECTION('ref_axis',(0.180980462437127,0.,-0.983486691428025));
#39674=DIRECTION('',(0.180980462437127,0.,-0.983486691428025));
#39675=DIRECTION('',(0.,1.,0.));
#39676=DIRECTION('center_axis',(-0.648477023773219,0.,-0.761234227842015));
#39677=DIRECTION('ref_axis',(-0.761234227842015,0.,0.648477023773219));
#39678=DIRECTION('',(-0.761234227842015,0.,0.648477023773219));
#39679=DIRECTION('center_axis',(0.,1.,0.));
#39680=DIRECTION('ref_axis',(-0.866025403784438,0.,-0.5));
#39681=DIRECTION('center_axis',(0.,1.,0.));
#39682=DIRECTION('ref_axis',(-0.766044443118978,0.,-0.642787609686539));
#39683=DIRECTION('',(-0.862276222874172,0.,0.506438264219689));
#39684=DIRECTION('',(0.349011634277972,0.,-0.937118391207119));
#39685=DIRECTION('center_axis',(0.937118391207119,0.,0.349011634277972));
#39686=DIRECTION('ref_axis',(0.349011634277972,0.,-0.937118391207119));
#39687=DIRECTION('',(0.,1.,0.));
#39688=DIRECTION('center_axis',(-0.506438264219689,0.,-0.862276222874172));
#39689=DIRECTION('ref_axis',(-0.862276222874172,0.,0.506438264219689));
#39690=DIRECTION('center_axis',(0.862276222874171,0.,0.50643826421969));
#39691=DIRECTION('ref_axis',(0.50643826421969,0.,-0.862276222874171));
#39692=DIRECTION('',(0.50643826421969,0.,-0.862276222874171));
#39693=DIRECTION('',(0.,1.,0.));
#39694=DIRECTION('center_axis',(-0.349011634277972,0.,-0.937118391207119));
#39695=DIRECTION('ref_axis',(-0.937118391207119,0.,0.349011634277972));
#39696=DIRECTION('',(-0.937118391207119,0.,0.349011634277972));
#39697=DIRECTION('center_axis',(0.,1.,0.));
#39698=DIRECTION('ref_axis',(-0.642787609686539,0.,-0.766044443118978));
#39699=DIRECTION('center_axis',(0.,1.,0.));
#39700=DIRECTION('ref_axis',(-0.5,0.,-0.866025403784439));
#39701=DIRECTION('',(-0.983486691428025,0.,0.180980462437126));
#39702=DIRECTION('',(0.648477023773219,0.,-0.761234227842014));
#39703=DIRECTION('center_axis',(0.761234227842014,0.,0.648477023773219));
#39704=DIRECTION('ref_axis',(0.648477023773219,0.,-0.761234227842014));
#39705=DIRECTION('',(0.,1.,0.));
#39706=DIRECTION('center_axis',(-0.180980462437126,0.,-0.983486691428025));
#39707=DIRECTION('ref_axis',(-0.983486691428025,0.,0.180980462437126));
#39708=DIRECTION('center_axis',(0.637062515999983,0.,0.770812137104607));
#39709=DIRECTION('ref_axis',(0.770812137104607,0.,-0.637062515999983));
#39710=DIRECTION('',(0.770812137104607,0.,-0.637062515999983));
#39711=DIRECTION('',(0.,1.,0.));
#39712=DIRECTION('center_axis',(-0.00745029082566107,0.,-0.99997224619817));
#39713=DIRECTION('ref_axis',(-0.99997224619817,0.,0.00745029082566107));
#39714=DIRECTION('',(-0.99997224619817,0.,0.00745029082566107));
#39715=DIRECTION('center_axis',(0.,1.,0.));
#39716=DIRECTION('ref_axis',(-0.342020143325669,0.,-0.939692620785908));
#39717=DIRECTION('center_axis',(0.,1.,0.));
#39718=DIRECTION('ref_axis',(-0.17364817766693,0.,-0.984807753012208));
#39719=DIRECTION('',(-0.986074150277955,0.,-0.166306254102513));
#39720=DIRECTION('',(0.869726513699833,0.,-0.49353398197848));
#39721=DIRECTION('center_axis',(0.49353398197848,0.,0.869726513699833));
#39722=DIRECTION('ref_axis',(0.869726513699833,0.,-0.49353398197848));
#39723=DIRECTION('',(0.,1.,0.));
#39724=DIRECTION('center_axis',(0.166306254102513,0.,-0.986074150277955));
#39725=DIRECTION('ref_axis',(-0.986074150277955,0.,-0.166306254102513));
#39726=DIRECTION('center_axis',(0.335009667654806,0.,0.94221469027914));
#39727=DIRECTION('ref_axis',(0.94221469027914,0.,-0.335009667654806));
#39728=DIRECTION('',(0.94221469027914,0.,-0.335009667654806));
#39729=DIRECTION('',(0.,1.,0.));
#39730=DIRECTION('center_axis',(0.335009667654806,0.,-0.94221469027914));
#39731=DIRECTION('ref_axis',(-0.94221469027914,0.,-0.335009667654806));
#39732=DIRECTION('',(-0.94221469027914,0.,-0.335009667654806));
#39733=DIRECTION('center_axis',(0.,1.,0.));
#39734=DIRECTION('ref_axis',(1.22464679914735E-16,0.,-1.));
#39735=DIRECTION('center_axis',(0.,1.,0.));
#39736=DIRECTION('ref_axis',(0.173648177666931,0.,-0.984807753012208));
#39737=DIRECTION('',(-0.869726513699832,0.,-0.493533981978481));
#39738=DIRECTION('',(0.986074150277955,0.,-0.166306254102512));
#39739=DIRECTION('center_axis',(0.166306254102512,0.,0.986074150277955));
#39740=DIRECTION('ref_axis',(0.986074150277955,0.,-0.166306254102512));
#39741=DIRECTION('',(0.,1.,0.));
#39742=DIRECTION('center_axis',(0.493533981978481,0.,-0.869726513699832));
#39743=DIRECTION('ref_axis',(-0.869726513699832,0.,-0.493533981978481));
#39744=DIRECTION('center_axis',(-0.00745029082566129,0.,0.99997224619817));
#39745=DIRECTION('ref_axis',(0.99997224619817,0.,0.00745029082566129));
#39746=DIRECTION('',(0.99997224619817,0.,0.00745029082566129));
#39747=DIRECTION('',(0.,1.,0.));
#39748=DIRECTION('center_axis',(0.637062515999983,0.,-0.770812137104607));
#39749=DIRECTION('ref_axis',(-0.770812137104607,0.,-0.637062515999983));
#39750=DIRECTION('',(-0.770812137104607,0.,-0.637062515999983));
#39751=DIRECTION('center_axis',(0.,1.,0.));
#39752=DIRECTION('ref_axis',(0.342020143325669,0.,-0.939692620785908));
#39753=DIRECTION('center_axis',(0.,1.,0.));
#39754=DIRECTION('ref_axis',(0.5,0.,-0.866025403784439));
#39755=DIRECTION('',(-0.648477023773219,0.,-0.761234227842014));
#39756=DIRECTION('',(0.983486691428025,0.,0.180980462437126));
#39757=DIRECTION('center_axis',(-0.180980462437126,0.,0.983486691428025));
#39758=DIRECTION('ref_axis',(0.983486691428025,0.,0.180980462437126));
#39759=DIRECTION('',(0.,1.,0.));
#39760=DIRECTION('center_axis',(0.761234227842014,0.,-0.648477023773219));
#39761=DIRECTION('ref_axis',(-0.648477023773219,0.,-0.761234227842014));
#39762=DIRECTION('center_axis',(-0.349011634277972,0.,0.937118391207119));
#39763=DIRECTION('ref_axis',(0.937118391207119,0.,0.349011634277972));
#39764=DIRECTION('',(0.937118391207119,0.,0.349011634277972));
#39765=DIRECTION('',(0.,1.,0.));
#39766=DIRECTION('center_axis',(0.862276222874172,0.,-0.506438264219689));
#39767=DIRECTION('ref_axis',(-0.506438264219689,0.,-0.862276222874172));
#39768=DIRECTION('',(-0.506438264219689,0.,-0.862276222874172));
#39769=DIRECTION('center_axis',(0.,1.,0.));
#39770=DIRECTION('ref_axis',(0.642787609686539,0.,-0.766044443118978));
#39771=DIRECTION('center_axis',(0.,1.,0.));
#39772=DIRECTION('ref_axis',(0.766044443118978,0.,-0.642787609686539));
#39773=DIRECTION('',(-0.349011634277972,0.,-0.937118391207119));
#39774=DIRECTION('',(0.862276222874172,0.,0.506438264219689));
#39775=DIRECTION('center_axis',(-0.50643826421969,0.,0.862276222874171));
#39776=DIRECTION('ref_axis',(0.862276222874171,0.,0.50643826421969));
#39777=DIRECTION('',(0.,1.,0.));
#39778=DIRECTION('center_axis',(0.937118391207119,0.,-0.349011634277972));
#39779=DIRECTION('ref_axis',(-0.349011634277972,0.,-0.937118391207119));
#39780=DIRECTION('center_axis',(-0.648477023773219,0.,0.761234227842014));
#39781=DIRECTION('ref_axis',(0.761234227842014,0.,0.648477023773219));
#39782=DIRECTION('',(0.761234227842014,0.,0.648477023773219));
#39783=DIRECTION('',(0.,1.,0.));
#39784=DIRECTION('center_axis',(0.983486691428025,0.,-0.180980462437126));
#39785=DIRECTION('ref_axis',(-0.180980462437126,0.,-0.983486691428025));
#39786=DIRECTION('',(-0.180980462437126,0.,-0.983486691428025));
#39787=DIRECTION('center_axis',(0.,1.,0.));
#39788=DIRECTION('ref_axis',(0.866025403784439,0.,-0.5));
#39789=DIRECTION('center_axis',(0.,1.,0.));
#39790=DIRECTION('ref_axis',(0.939692620785908,0.,-0.342020143325669));
#39791=DIRECTION('',(-0.00745029082566112,0.,-0.99997224619817));
#39792=DIRECTION('',(0.637062515999983,0.,0.770812137104607));
#39793=DIRECTION('center_axis',(-0.770812137104607,0.,0.637062515999983));
#39794=DIRECTION('ref_axis',(0.637062515999983,0.,0.770812137104607));
#39795=DIRECTION('',(0.,1.,0.));
#39796=DIRECTION('center_axis',(0.99997224619817,0.,-0.00745029082566112));
#39797=DIRECTION('ref_axis',(-0.00745029082566112,0.,-0.99997224619817));
#39798=DIRECTION('center_axis',(-0.869726513699833,0.,0.49353398197848));
#39799=DIRECTION('ref_axis',(0.49353398197848,0.,0.869726513699833));
#39800=DIRECTION('',(0.49353398197848,0.,0.869726513699833));
#39801=DIRECTION('',(0.,1.,0.));
#39802=DIRECTION('center_axis',(0.986074150277955,0.,0.166306254102512));
#39803=DIRECTION('ref_axis',(0.166306254102512,0.,-0.986074150277955));
#39804=DIRECTION('',(0.166306254102512,0.,-0.986074150277955));
#39805=DIRECTION('center_axis',(0.,1.,0.));
#39806=DIRECTION('ref_axis',(0.984807753012208,0.,-0.17364817766693));
#39807=DIRECTION('center_axis',(0.,1.,0.));
#39808=DIRECTION('ref_axis',(1.,0.,6.12323399573677E-17));
#39809=DIRECTION('',(0.335009667654806,0.,-0.94221469027914));
#39810=DIRECTION('',(0.335009667654806,0.,0.94221469027914));
#39811=DIRECTION('center_axis',(-0.94221469027914,0.,0.335009667654806));
#39812=DIRECTION('ref_axis',(0.335009667654806,0.,0.94221469027914));
#39813=DIRECTION('',(0.,1.,0.));
#39814=DIRECTION('center_axis',(0.94221469027914,0.,0.335009667654806));
#39815=DIRECTION('ref_axis',(0.335009667654806,0.,-0.94221469027914));
#39816=DIRECTION('center_axis',(-0.986074150277955,0.,0.166306254102512));
#39817=DIRECTION('ref_axis',(0.166306254102512,0.,0.986074150277955));
#39818=DIRECTION('',(0.166306254102512,0.,0.986074150277955));
#39819=DIRECTION('',(0.,1.,0.));
#39820=DIRECTION('center_axis',(0.869726513699833,0.,0.49353398197848));
#39821=DIRECTION('ref_axis',(0.49353398197848,0.,-0.869726513699833));
#39822=DIRECTION('',(0.49353398197848,0.,-0.869726513699833));
#39823=DIRECTION('center_axis',(0.,1.,0.));
#39824=DIRECTION('ref_axis',(0.984807753012208,0.,0.17364817766693));
#39825=DIRECTION('center_axis',(0.,1.,0.));
#39826=DIRECTION('ref_axis',(0.939692620785908,0.,0.342020143325669));
#39827=DIRECTION('',(0.637062515999983,0.,-0.770812137104607));
#39828=DIRECTION('',(-0.00745029082566129,0.,0.99997224619817));
#39829=DIRECTION('center_axis',(-0.99997224619817,0.,-0.00745029082566129));
#39830=DIRECTION('ref_axis',(-0.00745029082566129,0.,0.99997224619817));
#39831=DIRECTION('',(0.,1.,0.));
#39832=DIRECTION('center_axis',(0.770812137104607,0.,0.637062515999983));
#39833=DIRECTION('ref_axis',(0.637062515999983,0.,-0.770812137104607));
#39834=DIRECTION('center_axis',(-0.983486691428025,0.,-0.180980462437126));
#39835=DIRECTION('ref_axis',(-0.180980462437126,0.,0.983486691428025));
#39836=DIRECTION('',(-0.180980462437126,0.,0.983486691428025));
#39837=DIRECTION('',(0.,1.,0.));
#39838=DIRECTION('center_axis',(0.648477023773219,0.,0.761234227842014));
#39839=DIRECTION('ref_axis',(0.761234227842014,0.,-0.648477023773219));
#39840=DIRECTION('',(0.761234227842014,0.,-0.648477023773219));
#39841=DIRECTION('center_axis',(0.,1.,0.));
#39842=DIRECTION('ref_axis',(0.866025403784439,0.,0.5));
#39843=DIRECTION('center_axis',(0.,1.,0.));
#39844=DIRECTION('ref_axis',(0.766044443118978,0.,0.642787609686539));
#39845=DIRECTION('',(0.862276222874172,0.,-0.506438264219689));
#39846=DIRECTION('',(-0.349011634277972,0.,0.937118391207119));
#39847=DIRECTION('center_axis',(-0.937118391207119,0.,-0.349011634277972));
#39848=DIRECTION('ref_axis',(-0.349011634277972,0.,0.937118391207119));
#39849=DIRECTION('',(0.,1.,0.));
#39850=DIRECTION('center_axis',(0.50643826421969,0.,0.862276222874171));
#39851=DIRECTION('ref_axis',(0.862276222874171,0.,-0.50643826421969));
#39852=DIRECTION('center_axis',(-0.862276222874171,0.,-0.50643826421969));
#39853=DIRECTION('ref_axis',(-0.50643826421969,0.,0.862276222874171));
#39854=DIRECTION('',(-0.50643826421969,0.,0.862276222874171));
#39855=DIRECTION('',(0.,1.,0.));
#39856=DIRECTION('center_axis',(0.349011634277972,0.,0.937118391207119));
#39857=DIRECTION('ref_axis',(0.937118391207119,0.,-0.349011634277972));
#39858=DIRECTION('',(0.937118391207119,0.,-0.349011634277972));
#39859=DIRECTION('center_axis',(0.,1.,0.));
#39860=DIRECTION('ref_axis',(0.642787609686539,0.,0.766044443118978));
#39861=DIRECTION('center_axis',(0.,1.,0.));
#39862=DIRECTION('ref_axis',(0.5,0.,0.866025403784439));
#39863=DIRECTION('',(0.983486691428025,0.,-0.180980462437126));
#39864=DIRECTION('',(-0.648477023773219,0.,0.761234227842014));
#39865=DIRECTION('center_axis',(-0.761234227842014,0.,-0.648477023773219));
#39866=DIRECTION('ref_axis',(-0.648477023773219,0.,0.761234227842014));
#39867=DIRECTION('',(0.,1.,0.));
#39868=DIRECTION('center_axis',(0.180980462437126,0.,0.983486691428025));
#39869=DIRECTION('ref_axis',(0.983486691428025,0.,-0.180980462437126));
#39870=DIRECTION('center_axis',(-0.637062515999983,0.,-0.770812137104607));
#39871=DIRECTION('ref_axis',(-0.770812137104607,0.,0.637062515999983));
#39872=DIRECTION('',(-0.770812137104607,0.,0.637062515999983));
#39873=DIRECTION('',(0.,1.,0.));
#39874=DIRECTION('center_axis',(0.00745029082566112,0.,0.99997224619817));
#39875=DIRECTION('ref_axis',(0.99997224619817,0.,-0.00745029082566112));
#39876=DIRECTION('',(0.99997224619817,0.,-0.00745029082566112));
#39877=DIRECTION('center_axis',(0.,1.,0.));
#39878=DIRECTION('ref_axis',(0.342020143325669,0.,0.939692620785908));
#39879=DIRECTION('center_axis',(0.,1.,0.));
#39880=DIRECTION('ref_axis',(0.17364817766693,0.,0.984807753012208));
#39881=DIRECTION('',(0.986074150277955,0.,0.166306254102512));
#39882=DIRECTION('',(-0.869726513699833,0.,0.49353398197848));
#39883=DIRECTION('center_axis',(-0.49353398197848,0.,-0.869726513699833));
#39884=DIRECTION('ref_axis',(-0.869726513699833,0.,0.49353398197848));
#39885=DIRECTION('',(0.,1.,0.));
#39886=DIRECTION('center_axis',(-0.166306254102512,0.,0.986074150277955));
#39887=DIRECTION('ref_axis',(0.986074150277955,0.,0.166306254102512));
#39888=DIRECTION('center_axis',(-0.335009667654806,0.,-0.94221469027914));
#39889=DIRECTION('ref_axis',(-0.94221469027914,0.,0.335009667654806));
#39890=DIRECTION('',(-0.94221469027914,0.,0.335009667654806));
#39891=DIRECTION('',(0.,1.,0.));
#39892=DIRECTION('center_axis',(-0.335009667654806,0.,0.94221469027914));
#39893=DIRECTION('ref_axis',(0.94221469027914,0.,0.335009667654806));
#39894=DIRECTION('',(0.94221469027914,0.,0.335009667654806));
#39895=DIRECTION('center_axis',(0.,1.,0.));
#39896=DIRECTION('ref_axis',(0.,0.,1.));
#39897=DIRECTION('center_axis',(0.,1.,0.));
#39898=DIRECTION('ref_axis',(0.,0.,1.));
#39899=DIRECTION('center_axis',(-1.,0.,0.));
#39900=DIRECTION('ref_axis',(0.,0.,-1.));
#39901=DIRECTION('center_axis',(0.,1.,0.));
#39902=DIRECTION('ref_axis',(1.,0.,0.));
#39903=DIRECTION('center_axis',(0.,1.,0.));
#39904=DIRECTION('ref_axis',(1.,0.,0.));
#39905=DIRECTION('center_axis',(0.,-1.,0.));
#39906=DIRECTION('ref_axis',(1.,0.,0.));
#39907=DIRECTION('center_axis',(0.,-1.,0.));
#39908=DIRECTION('ref_axis',(1.,0.,0.));
#39909=DIRECTION('center_axis',(0.,-1.,0.));
#39910=DIRECTION('ref_axis',(1.,0.,0.));
#39911=DIRECTION('center_axis',(0.,-1.,0.));
#39912=DIRECTION('ref_axis',(1.,0.,0.));
#39913=DIRECTION('center_axis',(0.,-1.,0.));
#39914=DIRECTION('ref_axis',(1.,0.,0.));
#39915=DIRECTION('center_axis',(0.,-1.,0.));
#39916=DIRECTION('ref_axis',(1.,0.,0.));
#39917=DIRECTION('center_axis',(0.,-1.,0.));
#39918=DIRECTION('ref_axis',(1.,0.,0.));
#39919=DIRECTION('',(-0.707106781186552,-0.707106781186543,-8.65956056235498E-17));
#39920=DIRECTION('center_axis',(0.,-1.,0.));
#39921=DIRECTION('ref_axis',(1.,0.,0.));
#39922=DIRECTION('',(0.,-1.,0.));
#39923=DIRECTION('',(0.,1.,0.));
#39924=DIRECTION('center_axis',(0.,-1.,0.));
#39925=DIRECTION('ref_axis',(1.,0.,0.));
#39926=DIRECTION('center_axis',(0.,-1.,0.));
#39927=DIRECTION('ref_axis',(1.,0.,0.));
#39928=DIRECTION('',(0.,1.,0.));
#39929=DIRECTION('center_axis',(0.,-1.,0.));
#39930=DIRECTION('ref_axis',(1.,0.,0.));
#39931=DIRECTION('',(0.,-1.,0.));
#39932=DIRECTION('center_axis',(0.,-1.,0.));
#39933=DIRECTION('ref_axis',(1.,0.,0.));
#39934=DIRECTION('',(0.,-1.,0.));
#39935=DIRECTION('',(0.,1.,0.));
#39936=DIRECTION('center_axis',(0.,-1.,0.));
#39937=DIRECTION('ref_axis',(1.,0.,0.));
#39938=DIRECTION('center_axis',(0.,-1.,0.));
#39939=DIRECTION('ref_axis',(1.,0.,0.));
#39940=DIRECTION('',(0.,1.,0.));
#39941=DIRECTION('center_axis',(0.,-1.,0.));
#39942=DIRECTION('ref_axis',(1.,0.,0.));
#39943=DIRECTION('',(0.,-1.,0.));
#39944=DIRECTION('center_axis',(0.,-1.,0.));
#39945=DIRECTION('ref_axis',(1.,0.,0.));
#39946=DIRECTION('',(0.,-1.,0.));
#39947=DIRECTION('',(0.,1.,0.));
#39948=DIRECTION('center_axis',(0.,-1.,0.));
#39949=DIRECTION('ref_axis',(1.,0.,0.));
#39950=DIRECTION('center_axis',(0.,-1.,0.));
#39951=DIRECTION('ref_axis',(1.,0.,0.));
#39952=DIRECTION('',(0.,1.,0.));
#39953=DIRECTION('center_axis',(0.,-1.,0.));
#39954=DIRECTION('ref_axis',(1.,0.,0.));
#39955=DIRECTION('',(0.,-1.,0.));
#39956=DIRECTION('center_axis',(0.,0.,1.));
#39957=DIRECTION('ref_axis',(1.,0.,0.));
#39958=DIRECTION('',(1.,0.,0.));
#39959=DIRECTION('',(0.,1.,0.));
#39960=DIRECTION('',(1.,0.,0.));
#39961=DIRECTION('',(0.,1.,0.));
#39962=DIRECTION('center_axis',(-0.866025403784439,0.,0.499999999999999));
#39963=DIRECTION('ref_axis',(0.499999999999999,0.,0.866025403784439));
#39964=DIRECTION('',(0.499999999999999,0.,0.866025403784439));
#39965=DIRECTION('',(0.,1.,0.));
#39966=DIRECTION('',(0.499999999999999,0.,0.866025403784439));
#39967=DIRECTION('center_axis',(-0.866025403784439,0.,-0.499999999999999));
#39968=DIRECTION('ref_axis',(-0.499999999999999,0.,0.866025403784439));
#39969=DIRECTION('',(-0.499999999999999,0.,0.866025403784439));
#39970=DIRECTION('',(0.,1.,0.));
#39971=DIRECTION('',(-0.499999999999999,0.,0.866025403784439));
#39972=DIRECTION('center_axis',(0.,1.,0.));
#39973=DIRECTION('ref_axis',(1.,0.,0.));
#39974=DIRECTION('center_axis',(0.,1.,0.));
#39975=DIRECTION('ref_axis',(1.,0.,0.));
#39976=DIRECTION('center_axis',(0.,1.,0.));
#39977=DIRECTION('ref_axis',(1.,0.,0.));
#39978=DIRECTION('',(-1.,0.,0.));
#39979=DIRECTION('center_axis',(0.,1.,0.));
#39980=DIRECTION('ref_axis',(1.,0.,0.));
#39981=DIRECTION('center_axis',(0.,1.,0.));
#39982=DIRECTION('ref_axis',(1.,0.,0.));
#39983=DIRECTION('',(-0.5,0.,-0.866025403784439));
#39984=DIRECTION('center_axis',(0.,1.,0.));
#39985=DIRECTION('ref_axis',(1.,0.,0.));
#39986=DIRECTION('',(0.5,0.,-0.866025403784439));
#39987=DIRECTION('center_axis',(0.,-1.,0.));
#39988=DIRECTION('ref_axis',(0.,0.,-1.));
#39989=DIRECTION('',(-0.5,0.,-0.866025403784439));
#39990=DIRECTION('center_axis',(0.,-1.,0.));
#39991=DIRECTION('ref_axis',(1.,0.,0.));
#39992=DIRECTION('center_axis',(0.,-1.,0.));
#39993=DIRECTION('ref_axis',(0.,0.,-1.));
#39994=DIRECTION('',(-1.,0.,0.));
#39995=DIRECTION('center_axis',(0.,-1.,0.));
#39996=DIRECTION('ref_axis',(1.,0.,0.));
#39997=DIRECTION('center_axis',(0.,-1.,0.));
#39998=DIRECTION('ref_axis',(0.,0.,-1.));
#39999=DIRECTION('center_axis',(0.,-1.,0.));
#40000=DIRECTION('ref_axis',(1.,0.,0.));
#40001=DIRECTION('center_axis',(0.,-1.,0.));
#40002=DIRECTION('ref_axis',(0.,0.,-1.));
#40003=DIRECTION('center_axis',(0.,-1.,0.));
#40004=DIRECTION('ref_axis',(1.,0.,0.));
#40005=DIRECTION('center_axis',(0.,-1.,0.));
#40006=DIRECTION('ref_axis',(0.,0.,-1.));
#40007=DIRECTION('center_axis',(0.,-1.,0.));
#40008=DIRECTION('ref_axis',(1.,0.,0.));
#40009=DIRECTION('center_axis',(0.,-1.,0.));
#40010=DIRECTION('ref_axis',(0.,0.,-1.));
#40011=DIRECTION('',(0.5,0.,-0.866025403784439));
#40012=DIRECTION('center_axis',(0.,-1.,0.));
#40013=DIRECTION('ref_axis',(1.,0.,0.));
#40014=DIRECTION('center_axis',(0.,-1.,0.));
#40015=DIRECTION('ref_axis',(1.,0.,0.));
#40016=DIRECTION('',(-0.85716730070211,-0.515038074910058,-1.04972719113862E-16));
#40017=DIRECTION('center_axis',(0.866025403784439,0.,-0.5));
#40018=DIRECTION('ref_axis',(-0.5,0.,-0.866025403784439));
#40019=DIRECTION('',(0.,1.,0.));
#40020=DIRECTION('',(0.,1.,0.));
#40021=DIRECTION('center_axis',(0.866025403784439,0.,0.5));
#40022=DIRECTION('ref_axis',(0.5,0.,-0.866025403784439));
#40023=DIRECTION('center_axis',(0.,0.,-1.));
#40024=DIRECTION('ref_axis',(-1.,0.,0.));
#40025=DIRECTION('axis',(0.,0.,1.));
#40026=DIRECTION('refdir',(1.,0.,0.));
#40027=DIRECTION('center_axis',(0.,1.,0.));
#40028=DIRECTION('ref_axis',(1.,0.,0.));
#40029=DIRECTION('',(0.,-1.,0.));
#40030=DIRECTION('center_axis',(0.,-1.,0.));
#40031=DIRECTION('ref_axis',(1.,0.,0.));
#40032=DIRECTION('center_axis',(0.,1.,0.));
#40033=DIRECTION('ref_axis',(1.,0.,0.));
#40034=DIRECTION('',(0.,-1.,0.));
#40035=DIRECTION('center_axis',(0.,1.,0.));
#40036=DIRECTION('ref_axis',(1.,0.,0.));
#40037=DIRECTION('',(0.,-1.,0.));
#40038=DIRECTION('center_axis',(0.,1.,0.));
#40039=DIRECTION('ref_axis',(1.,0.,0.));
#40040=DIRECTION('',(0.,-1.,0.));
#40041=DIRECTION('center_axis',(0.,1.,0.));
#40042=DIRECTION('ref_axis',(1.,0.,0.));
#40043=DIRECTION('',(0.,-1.,0.));
#40044=DIRECTION('center_axis',(0.,1.,0.));
#40045=DIRECTION('ref_axis',(1.,0.,0.));
#40046=DIRECTION('',(0.,-1.,0.));
#40047=DIRECTION('center_axis',(0.,1.,0.));
#40048=DIRECTION('ref_axis',(1.,0.,0.));
#40049=DIRECTION('',(0.,-1.,0.));
#40050=DIRECTION('center_axis',(0.,1.,0.));
#40051=DIRECTION('ref_axis',(1.,0.,0.));
#40052=DIRECTION('',(0.,-1.,0.));
#40053=DIRECTION('center_axis',(0.,1.,0.));
#40054=DIRECTION('ref_axis',(1.,0.,0.));
#40055=DIRECTION('',(0.,-1.,0.));
#40056=DIRECTION('center_axis',(0.,1.,0.));
#40057=DIRECTION('ref_axis',(1.,0.,0.));
#40058=DIRECTION('',(0.,-1.,0.));
#40059=DIRECTION('center_axis',(0.,1.,0.));
#40060=DIRECTION('ref_axis',(1.,0.,0.));
#40061=DIRECTION('',(0.,-1.,0.));
#40062=DIRECTION('center_axis',(0.,1.,0.));
#40063=DIRECTION('ref_axis',(1.,0.,0.));
#40064=DIRECTION('',(0.,-1.,0.));
#40065=DIRECTION('center_axis',(0.,1.,0.));
#40066=DIRECTION('ref_axis',(1.,0.,0.));
#40067=DIRECTION('',(0.,-1.,0.));
#40068=DIRECTION('center_axis',(0.,1.,0.));
#40069=DIRECTION('ref_axis',(1.,0.,0.));
#40070=DIRECTION('',(0.,-1.,0.));
#40071=DIRECTION('center_axis',(0.,1.,0.));
#40072=DIRECTION('ref_axis',(1.,0.,0.));
#40073=DIRECTION('',(0.,-1.,0.));
#40074=DIRECTION('center_axis',(0.,1.,0.));
#40075=DIRECTION('ref_axis',(1.,0.,0.));
#40076=DIRECTION('',(0.,-1.,0.));
#40077=DIRECTION('center_axis',(0.,1.,0.));
#40078=DIRECTION('ref_axis',(1.,0.,0.));
#40079=DIRECTION('',(0.,-1.,0.));
#40080=DIRECTION('center_axis',(0.,1.,0.));
#40081=DIRECTION('ref_axis',(1.,0.,0.));
#40082=DIRECTION('',(0.,-1.,0.));
#40083=DIRECTION('center_axis',(0.,1.,0.));
#40084=DIRECTION('ref_axis',(1.,0.,0.));
#40085=DIRECTION('',(0.,-1.,0.));
#40086=DIRECTION('center_axis',(0.,1.,0.));
#40087=DIRECTION('ref_axis',(-0.160348714496653,0.,0.987060428625964));
#40088=DIRECTION('',(0.,-1.,0.));
#40089=DIRECTION('center_axis',(0.,-1.,0.));
#40090=DIRECTION('ref_axis',(1.,0.,-1.41399663505645E-13));
#40091=DIRECTION('center_axis',(0.,1.,0.));
#40092=DIRECTION('ref_axis',(-0.160348714496653,0.,0.987060428625964));
#40093=DIRECTION('',(0.,-1.,0.));
#40094=DIRECTION('center_axis',(0.,1.,0.));
#40095=DIRECTION('ref_axis',(-0.160348714496653,0.,0.987060428625964));
#40096=DIRECTION('',(0.,-1.,0.));
#40097=DIRECTION('center_axis',(0.,1.,0.));
#40098=DIRECTION('ref_axis',(-0.160348714496653,0.,0.987060428625964));
#40099=DIRECTION('',(0.,-1.,0.));
#40100=DIRECTION('center_axis',(0.,1.,0.));
#40101=DIRECTION('ref_axis',(-0.160348714496653,0.,0.987060428625964));
#40102=DIRECTION('',(0.,-1.,0.));
#40103=DIRECTION('center_axis',(0.,1.,0.));
#40104=DIRECTION('ref_axis',(-0.160348714496653,0.,0.987060428625964));
#40105=DIRECTION('',(0.,-1.,0.));
#40106=DIRECTION('center_axis',(0.,1.,0.));
#40107=DIRECTION('ref_axis',(-0.160348714496653,0.,0.987060428625964));
#40108=DIRECTION('',(0.,-1.,0.));
#40109=DIRECTION('center_axis',(0.,1.,0.));
#40110=DIRECTION('ref_axis',(-0.160348714496653,0.,0.987060428625964));
#40111=DIRECTION('',(0.,-1.,0.));
#40112=DIRECTION('center_axis',(0.,1.,0.));
#40113=DIRECTION('ref_axis',(-0.160348714496653,0.,0.987060428625964));
#40114=DIRECTION('',(0.,-1.,0.));
#40115=DIRECTION('center_axis',(0.,1.,0.));
#40116=DIRECTION('ref_axis',(-0.160348714496653,0.,0.987060428625964));
#40117=DIRECTION('',(0.,-1.,0.));
#40118=DIRECTION('center_axis',(0.,1.,0.));
#40119=DIRECTION('ref_axis',(-0.160348714496653,0.,0.987060428625964));
#40120=DIRECTION('',(0.,-1.,0.));
#40121=DIRECTION('center_axis',(0.,1.,0.));
#40122=DIRECTION('ref_axis',(-0.160348714496653,0.,0.987060428625964));
#40123=DIRECTION('',(0.,-1.,0.));
#40124=DIRECTION('center_axis',(0.,1.,0.));
#40125=DIRECTION('ref_axis',(-0.160348714496653,0.,0.987060428625964));
#40126=DIRECTION('',(0.,-1.,0.));
#40127=DIRECTION('center_axis',(0.,1.,0.));
#40128=DIRECTION('ref_axis',(-0.160348714496653,0.,0.987060428625964));
#40129=DIRECTION('',(0.,-1.,0.));
#40130=DIRECTION('center_axis',(0.,1.,0.));
#40131=DIRECTION('ref_axis',(-0.160348714496653,0.,0.987060428625964));
#40132=DIRECTION('',(0.,-1.,0.));
#40133=DIRECTION('center_axis',(0.,1.,0.));
#40134=DIRECTION('ref_axis',(-0.160348714496653,0.,0.987060428625964));
#40135=DIRECTION('',(0.,-1.,0.));
#40136=DIRECTION('center_axis',(0.,1.,0.));
#40137=DIRECTION('ref_axis',(-0.160348714496653,0.,0.987060428625964));
#40138=DIRECTION('',(0.,-1.,0.));
#40139=DIRECTION('center_axis',(0.,1.,0.));
#40140=DIRECTION('ref_axis',(-0.160348714496653,0.,0.987060428625964));
#40141=DIRECTION('',(0.,-1.,0.));
#40142=DIRECTION('center_axis',(0.,1.,0.));
#40143=DIRECTION('ref_axis',(-0.160348714496653,0.,0.987060428625964));
#40144=DIRECTION('',(0.,-1.,0.));
#40145=DIRECTION('center_axis',(0.,1.,0.));
#40146=DIRECTION('ref_axis',(-0.160348714496653,0.,0.987060428625964));
#40147=DIRECTION('center_axis',(0.,1.,0.));
#40148=DIRECTION('ref_axis',(1.,0.,-1.41399663505645E-13));
#40149=DIRECTION('center_axis',(0.,1.,0.));
#40150=DIRECTION('ref_axis',(1.,0.,0.));
#40151=DIRECTION('center_axis',(0.,1.,0.));
#40152=DIRECTION('ref_axis',(1.,0.,0.));
#40153=DIRECTION('center_axis',(0.,1.,0.));
#40154=DIRECTION('ref_axis',(0.,0.,1.));
#40155=DIRECTION('center_axis',(0.,1.,0.));
#40156=DIRECTION('ref_axis',(1.,0.,0.));
#40157=DIRECTION('center_axis',(0.,1.,0.));
#40158=DIRECTION('ref_axis',(1.,0.,0.));
#40159=DIRECTION('center_axis',(0.,1.,0.));
#40160=DIRECTION('ref_axis',(0.,0.,1.));
#40161=DIRECTION('center_axis',(0.,-1.,0.));
#40162=DIRECTION('ref_axis',(1.,0.,0.));
#40163=DIRECTION('center_axis',(0.,-1.,0.));
#40164=DIRECTION('ref_axis',(1.,0.,0.));
#40165=DIRECTION('center_axis',(0.,-1.,0.));
#40166=DIRECTION('ref_axis',(0.,0.,-1.));
#40167=DIRECTION('center_axis',(0.,1.,0.));
#40168=DIRECTION('ref_axis',(1.,0.,0.));
#40169=DIRECTION('center_axis',(1.,0.,0.));
#40170=DIRECTION('ref_axis',(0.,0.,1.));
#40171=DIRECTION('center_axis',(0.,1.,0.));
#40172=DIRECTION('ref_axis',(1.,0.,0.));
#40173=DIRECTION('center_axis',(0.,-1.,0.));
#40174=DIRECTION('ref_axis',(1.,0.,0.));
#40175=DIRECTION('center_axis',(0.,-1.,0.));
#40176=DIRECTION('ref_axis',(1.,0.,0.));
#40177=DIRECTION('',(0.707106781186549,0.707106781186546,8.65956056235495E-17));
#40178=DIRECTION('center_axis',(0.,-1.,0.));
#40179=DIRECTION('ref_axis',(1.,0.,0.));
#40180=DIRECTION('center_axis',(0.,1.,0.));
#40181=DIRECTION('ref_axis',(1.,0.,0.));
#40182=DIRECTION('center_axis',(0.,1.,0.));
#40183=DIRECTION('ref_axis',(-0.17364817766693,0.,0.984807753012208));
#40184=DIRECTION('center_axis',(0.,1.,0.));
#40185=DIRECTION('ref_axis',(1.,0.,0.));
#40186=DIRECTION('',(0.869726513699833,0.,0.49353398197848));
#40187=DIRECTION('',(-0.986074150277955,0.,0.166306254102512));
#40188=DIRECTION('center_axis',(-0.166306254102512,0.,-0.986074150277955));
#40189=DIRECTION('ref_axis',(-0.986074150277955,0.,0.166306254102512));
#40190=DIRECTION('',(0.,-1.,0.));
#40191=DIRECTION('',(0.,1.,0.));
#40192=DIRECTION('center_axis',(-0.49353398197848,0.,0.869726513699833));
#40193=DIRECTION('ref_axis',(0.869726513699833,0.,0.49353398197848));
#40194=DIRECTION('',(0.,1.,0.));
#40195=DIRECTION('center_axis',(0.,-1.,0.));
#40196=DIRECTION('ref_axis',(1.,0.,0.));
#40197=DIRECTION('center_axis',(0.,1.,0.));
#40198=DIRECTION('ref_axis',(1.,0.,0.));
#40199=DIRECTION('',(0.,1.,0.));
#40200=DIRECTION('center_axis',(0.,1.,0.));
#40201=DIRECTION('ref_axis',(1.,0.,0.));
#40202=DIRECTION('center_axis',(0.,1.,0.));
#40203=DIRECTION('ref_axis',(1.,0.,0.));
#40204=DIRECTION('center_axis',(0.,1.,0.));
#40205=DIRECTION('ref_axis',(1.,0.,0.));
#40206=DIRECTION('',(0.,-1.,0.));
#40207=DIRECTION('center_axis',(0.,-1.,0.));
#40208=DIRECTION('ref_axis',(1.,0.,0.));
#40209=DIRECTION('',(0.,1.,0.));
#40210=DIRECTION('center_axis',(0.,1.,0.));
#40211=DIRECTION('ref_axis',(1.,0.,0.));
#40212=DIRECTION('',(0.,-1.,0.));
#40213=DIRECTION('center_axis',(0.,-1.,0.));
#40214=DIRECTION('ref_axis',(1.,0.,0.));
#40215=DIRECTION('',(0.,1.,0.));
#40216=DIRECTION('center_axis',(0.,1.,0.));
#40217=DIRECTION('ref_axis',(1.,0.,0.));
#40218=DIRECTION('',(0.,-1.,0.));
#40219=DIRECTION('center_axis',(0.,-1.,0.));
#40220=DIRECTION('ref_axis',(1.,0.,0.));
#40221=DIRECTION('',(0.,1.,0.));
#40222=DIRECTION('center_axis',(0.,1.,0.));
#40223=DIRECTION('ref_axis',(1.,0.,0.));
#40224=DIRECTION('',(0.,-1.,0.));
#40225=DIRECTION('center_axis',(0.,-1.,0.));
#40226=DIRECTION('ref_axis',(1.,0.,0.));
#40227=DIRECTION('',(0.,1.,0.));
#40228=DIRECTION('center_axis',(0.,1.,0.));
#40229=DIRECTION('ref_axis',(1.,0.,0.));
#40230=DIRECTION('',(0.,-1.,0.));
#40231=DIRECTION('center_axis',(0.,-1.,0.));
#40232=DIRECTION('ref_axis',(1.,0.,0.));
#40233=DIRECTION('',(0.,1.,0.));
#40234=DIRECTION('center_axis',(0.,1.,0.));
#40235=DIRECTION('ref_axis',(1.,0.,0.));
#40236=DIRECTION('',(0.,-1.,0.));
#40237=DIRECTION('center_axis',(0.,-1.,0.));
#40238=DIRECTION('ref_axis',(1.,0.,0.));
#40239=DIRECTION('',(0.,1.,0.));
#40240=DIRECTION('center_axis',(0.,1.,0.));
#40241=DIRECTION('ref_axis',(1.,0.,0.));
#40242=DIRECTION('',(0.,-1.,0.));
#40243=DIRECTION('center_axis',(0.,-1.,0.));
#40244=DIRECTION('ref_axis',(1.,0.,0.));
#40245=DIRECTION('',(0.,1.,0.));
#40246=DIRECTION('center_axis',(0.,1.,0.));
#40247=DIRECTION('ref_axis',(1.,0.,0.));
#40248=DIRECTION('',(0.,-1.,0.));
#40249=DIRECTION('center_axis',(0.,-1.,0.));
#40250=DIRECTION('ref_axis',(1.,0.,0.));
#40251=DIRECTION('',(0.,1.,0.));
#40252=DIRECTION('center_axis',(0.,1.,0.));
#40253=DIRECTION('ref_axis',(1.,0.,0.));
#40254=DIRECTION('',(0.,-1.,0.));
#40255=DIRECTION('center_axis',(0.,-1.,0.));
#40256=DIRECTION('ref_axis',(1.,0.,0.));
#40257=DIRECTION('',(0.,1.,0.));
#40258=DIRECTION('center_axis',(0.,1.,0.));
#40259=DIRECTION('ref_axis',(1.,0.,0.));
#40260=DIRECTION('',(0.,-1.,0.));
#40261=DIRECTION('center_axis',(0.,-1.,0.));
#40262=DIRECTION('ref_axis',(1.,0.,0.));
#40263=DIRECTION('',(0.,1.,0.));
#40264=DIRECTION('center_axis',(0.,1.,0.));
#40265=DIRECTION('ref_axis',(1.,0.,0.));
#40266=DIRECTION('',(0.,-1.,0.));
#40267=DIRECTION('center_axis',(0.,-1.,0.));
#40268=DIRECTION('ref_axis',(1.,0.,0.));
#40269=DIRECTION('',(0.,1.,0.));
#40270=DIRECTION('center_axis',(0.,1.,0.));
#40271=DIRECTION('ref_axis',(1.,0.,0.));
#40272=DIRECTION('',(0.,-1.,0.));
#40273=DIRECTION('center_axis',(0.,-1.,0.));
#40274=DIRECTION('ref_axis',(1.,0.,0.));
#40275=DIRECTION('',(0.,1.,0.));
#40276=DIRECTION('center_axis',(0.,1.,0.));
#40277=DIRECTION('ref_axis',(1.,0.,0.));
#40278=DIRECTION('',(0.,-1.,0.));
#40279=DIRECTION('center_axis',(0.,-1.,0.));
#40280=DIRECTION('ref_axis',(1.,0.,0.));
#40281=DIRECTION('',(0.,1.,0.));
#40282=DIRECTION('center_axis',(0.,1.,0.));
#40283=DIRECTION('ref_axis',(1.,0.,0.));
#40284=DIRECTION('',(0.,-1.,0.));
#40285=DIRECTION('center_axis',(0.,-1.,0.));
#40286=DIRECTION('ref_axis',(1.,0.,0.));
#40287=DIRECTION('',(0.,1.,0.));
#40288=DIRECTION('center_axis',(0.,1.,0.));
#40289=DIRECTION('ref_axis',(1.,0.,0.));
#40290=DIRECTION('',(0.,-1.,0.));
#40291=DIRECTION('center_axis',(0.,-1.,0.));
#40292=DIRECTION('ref_axis',(1.,0.,0.));
#40293=DIRECTION('',(0.,1.,0.));
#40294=DIRECTION('center_axis',(0.,1.,0.));
#40295=DIRECTION('ref_axis',(1.,0.,0.));
#40296=DIRECTION('',(0.,-1.,0.));
#40297=DIRECTION('center_axis',(0.,-1.,0.));
#40298=DIRECTION('ref_axis',(1.,0.,0.));
#40299=DIRECTION('',(0.,1.,0.));
#40300=DIRECTION('center_axis',(0.,1.,0.));
#40301=DIRECTION('ref_axis',(1.,0.,0.));
#40302=DIRECTION('',(0.,-1.,0.));
#40303=DIRECTION('center_axis',(0.,-1.,0.));
#40304=DIRECTION('ref_axis',(1.,0.,0.));
#40305=DIRECTION('center_axis',(0.,-1.,0.));
#40306=DIRECTION('ref_axis',(1.,0.,0.));
#40307=DIRECTION('',(0.,1.,0.));
#40308=DIRECTION('center_axis',(0.,1.,0.));
#40309=DIRECTION('ref_axis',(1.,0.,0.));
#40310=DIRECTION('',(0.,-1.,0.));
#40311=DIRECTION('center_axis',(0.,-1.,0.));
#40312=DIRECTION('ref_axis',(1.,0.,0.));
#40313=DIRECTION('',(0.,1.,0.));
#40314=DIRECTION('center_axis',(0.,1.,0.));
#40315=DIRECTION('ref_axis',(1.,0.,0.));
#40316=DIRECTION('',(0.,-1.,0.));
#40317=DIRECTION('center_axis',(0.,-1.,0.));
#40318=DIRECTION('ref_axis',(1.,0.,0.));
#40319=DIRECTION('',(0.,1.,0.));
#40320=DIRECTION('center_axis',(0.,1.,0.));
#40321=DIRECTION('ref_axis',(1.,0.,0.));
#40322=DIRECTION('',(0.,-1.,0.));
#40323=DIRECTION('center_axis',(0.,-1.,0.));
#40324=DIRECTION('ref_axis',(1.,0.,0.));
#40325=DIRECTION('',(0.,1.,0.));
#40326=DIRECTION('center_axis',(0.,1.,0.));
#40327=DIRECTION('ref_axis',(1.,0.,0.));
#40328=DIRECTION('',(0.,-1.,0.));
#40329=DIRECTION('center_axis',(0.,-1.,0.));
#40330=DIRECTION('ref_axis',(1.,0.,0.));
#40331=DIRECTION('',(0.,1.,0.));
#40332=DIRECTION('center_axis',(0.,1.,0.));
#40333=DIRECTION('ref_axis',(1.,0.,0.));
#40334=DIRECTION('',(0.,-1.,0.));
#40335=DIRECTION('center_axis',(0.,-1.,0.));
#40336=DIRECTION('ref_axis',(1.,0.,0.));
#40337=DIRECTION('',(0.,1.,0.));
#40338=DIRECTION('center_axis',(0.,1.,0.));
#40339=DIRECTION('ref_axis',(1.,0.,0.));
#40340=DIRECTION('',(0.,-1.,0.));
#40341=DIRECTION('center_axis',(0.,-1.,0.));
#40342=DIRECTION('ref_axis',(1.,0.,0.));
#40343=DIRECTION('',(0.,1.,0.));
#40344=DIRECTION('center_axis',(0.,1.,0.));
#40345=DIRECTION('ref_axis',(1.,0.,0.));
#40346=DIRECTION('',(0.,-1.,0.));
#40347=DIRECTION('center_axis',(0.,-1.,0.));
#40348=DIRECTION('ref_axis',(1.,0.,0.));
#40349=DIRECTION('',(0.,1.,0.));
#40350=DIRECTION('center_axis',(0.,1.,0.));
#40351=DIRECTION('ref_axis',(1.,0.,0.));
#40352=DIRECTION('',(0.,-1.,0.));
#40353=DIRECTION('center_axis',(0.,-1.,0.));
#40354=DIRECTION('ref_axis',(1.,0.,0.));
#40355=DIRECTION('',(0.,1.,0.));
#40356=DIRECTION('center_axis',(0.,1.,0.));
#40357=DIRECTION('ref_axis',(1.,0.,0.));
#40358=DIRECTION('',(0.,-1.,0.));
#40359=DIRECTION('center_axis',(0.,-1.,0.));
#40360=DIRECTION('ref_axis',(1.,0.,0.));
#40361=DIRECTION('',(0.,1.,0.));
#40362=DIRECTION('center_axis',(0.,1.,0.));
#40363=DIRECTION('ref_axis',(1.,0.,0.));
#40364=DIRECTION('',(0.,-1.,0.));
#40365=DIRECTION('center_axis',(0.,-1.,0.));
#40366=DIRECTION('ref_axis',(1.,0.,0.));
#40367=DIRECTION('',(0.,1.,0.));
#40368=DIRECTION('center_axis',(0.,1.,0.));
#40369=DIRECTION('ref_axis',(1.,0.,0.));
#40370=DIRECTION('',(0.,-1.,0.));
#40371=DIRECTION('center_axis',(0.,-1.,0.));
#40372=DIRECTION('ref_axis',(1.,0.,0.));
#40373=DIRECTION('',(0.,1.,0.));
#40374=DIRECTION('center_axis',(0.,1.,0.));
#40375=DIRECTION('ref_axis',(1.,0.,0.));
#40376=DIRECTION('',(0.,-1.,0.));
#40377=DIRECTION('center_axis',(0.,-1.,0.));
#40378=DIRECTION('ref_axis',(1.,0.,0.));
#40379=DIRECTION('',(0.,1.,0.));
#40380=DIRECTION('center_axis',(0.,1.,0.));
#40381=DIRECTION('ref_axis',(1.,0.,0.));
#40382=DIRECTION('',(0.,-1.,0.));
#40383=DIRECTION('center_axis',(0.,-1.,0.));
#40384=DIRECTION('ref_axis',(1.,0.,0.));
#40385=DIRECTION('',(0.,1.,0.));
#40386=DIRECTION('center_axis',(0.,1.,0.));
#40387=DIRECTION('ref_axis',(1.,0.,0.));
#40388=DIRECTION('',(0.,-1.,0.));
#40389=DIRECTION('center_axis',(0.,-1.,0.));
#40390=DIRECTION('ref_axis',(1.,0.,0.));
#40391=DIRECTION('',(0.,1.,0.));
#40392=DIRECTION('center_axis',(0.,1.,0.));
#40393=DIRECTION('ref_axis',(1.,0.,0.));
#40394=DIRECTION('',(0.,-1.,0.));
#40395=DIRECTION('center_axis',(0.,-1.,0.));
#40396=DIRECTION('ref_axis',(1.,0.,0.));
#40397=DIRECTION('',(0.,1.,0.));
#40398=DIRECTION('center_axis',(0.,1.,0.));
#40399=DIRECTION('ref_axis',(1.,0.,0.));
#40400=DIRECTION('',(0.,-1.,0.));
#40401=DIRECTION('center_axis',(0.,-1.,0.));
#40402=DIRECTION('ref_axis',(1.,0.,0.));
#40403=DIRECTION('',(0.,1.,0.));
#40404=DIRECTION('center_axis',(0.,1.,0.));
#40405=DIRECTION('ref_axis',(1.,0.,0.));
#40406=DIRECTION('',(0.,-1.,0.));
#40407=DIRECTION('center_axis',(0.,-1.,0.));
#40408=DIRECTION('ref_axis',(1.,0.,0.));
#40409=DIRECTION('',(0.,1.,0.));
#40410=DIRECTION('center_axis',(0.,1.,0.));
#40411=DIRECTION('ref_axis',(1.,0.,0.));
#40412=DIRECTION('',(0.,-1.,0.));
#40413=DIRECTION('center_axis',(0.,-1.,0.));
#40414=DIRECTION('ref_axis',(1.,0.,0.));
#40415=DIRECTION('',(0.,1.,0.));
#40416=DIRECTION('center_axis',(0.0074502908256619,0.,-0.99997224619817));
#40417=DIRECTION('ref_axis',(-0.99997224619817,0.,-0.0074502908256619));
#40418=DIRECTION('',(-0.99997224619817,0.,-0.0074502908256619));
#40419=DIRECTION('',(0.,1.,0.));
#40420=DIRECTION('center_axis',(-0.637062515999984,0.,0.770812137104606));
#40421=DIRECTION('ref_axis',(0.770812137104606,0.,0.637062515999984));
#40422=DIRECTION('',(0.770812137104606,0.,0.637062515999984));
#40423=DIRECTION('center_axis',(0.,1.,0.));
#40424=DIRECTION('ref_axis',(-0.342020143325669,0.,0.939692620785908));
#40425=DIRECTION('center_axis',(0.,1.,0.));
#40426=DIRECTION('ref_axis',(1.,0.,0.));
#40427=DIRECTION('',(0.707106781186547,-0.707106781186548,-8.65956056235493E-17));
#40428=DIRECTION('center_axis',(0.,1.,0.));
#40429=DIRECTION('ref_axis',(1.,0.,0.));
#40430=DIRECTION('center_axis',(0.,1.,0.));
#40431=DIRECTION('ref_axis',(-0.5,0.,0.866025403784438));
#40432=DIRECTION('',(0.648477023773219,0.,0.761234227842015));
#40433=DIRECTION('',(-0.983486691428025,0.,-0.180980462437127));
#40434=DIRECTION('center_axis',(0.180980462437127,0.,-0.983486691428025));
#40435=DIRECTION('ref_axis',(-0.983486691428025,0.,-0.180980462437127));
#40436=DIRECTION('',(0.,1.,0.));
#40437=DIRECTION('center_axis',(-0.761234227842015,0.,0.648477023773219));
#40438=DIRECTION('ref_axis',(0.648477023773219,0.,0.761234227842015));
#40439=DIRECTION('center_axis',(0.349011634277972,0.,-0.937118391207119));
#40440=DIRECTION('ref_axis',(-0.937118391207119,0.,-0.349011634277972));
#40441=DIRECTION('',(-0.937118391207119,0.,-0.349011634277972));
#40442=DIRECTION('',(0.,1.,0.));
#40443=DIRECTION('center_axis',(-0.862276222874172,0.,0.506438264219689));
#40444=DIRECTION('ref_axis',(0.506438264219689,0.,0.862276222874172));
#40445=DIRECTION('',(0.506438264219689,0.,0.862276222874172));
#40446=DIRECTION('center_axis',(0.,1.,0.));
#40447=DIRECTION('ref_axis',(-0.64278760968654,0.,0.766044443118978));
#40448=DIRECTION('center_axis',(0.,1.,0.));
#40449=DIRECTION('ref_axis',(-0.766044443118978,0.,0.642787609686539));
#40450=DIRECTION('',(0.349011634277972,0.,0.937118391207119));
#40451=DIRECTION('',(-0.862276222874171,0.,-0.50643826421969));
#40452=DIRECTION('center_axis',(0.50643826421969,0.,-0.862276222874171));
#40453=DIRECTION('ref_axis',(-0.862276222874171,0.,-0.50643826421969));
#40454=DIRECTION('',(0.,1.,0.));
#40455=DIRECTION('center_axis',(-0.937118391207119,0.,0.349011634277972));
#40456=DIRECTION('ref_axis',(0.349011634277972,0.,0.937118391207119));
#40457=DIRECTION('center_axis',(0.648477023773219,0.,-0.761234227842014));
#40458=DIRECTION('ref_axis',(-0.761234227842014,0.,-0.648477023773219));
#40459=DIRECTION('',(-0.761234227842014,0.,-0.648477023773219));
#40460=DIRECTION('',(0.,1.,0.));
#40461=DIRECTION('center_axis',(-0.983486691428025,0.,0.180980462437126));
#40462=DIRECTION('ref_axis',(0.180980462437126,0.,0.983486691428025));
#40463=DIRECTION('',(0.180980462437126,0.,0.983486691428025));
#40464=DIRECTION('center_axis',(0.,1.,0.));
#40465=DIRECTION('ref_axis',(-0.866025403784439,0.,0.5));
#40466=DIRECTION('center_axis',(0.,1.,0.));
#40467=DIRECTION('ref_axis',(-0.939692620785909,0.,0.342020143325668));
#40468=DIRECTION('',(0.00745029082566051,0.,0.99997224619817));
#40469=DIRECTION('',(-0.637062515999983,0.,-0.770812137104607));
#40470=DIRECTION('center_axis',(0.770812137104607,0.,-0.637062515999983));
#40471=DIRECTION('ref_axis',(-0.637062515999983,0.,-0.770812137104607));
#40472=DIRECTION('',(0.,1.,0.));
#40473=DIRECTION('center_axis',(-0.99997224619817,0.,0.00745029082566051));
#40474=DIRECTION('ref_axis',(0.00745029082566051,0.,0.99997224619817));
#40475=DIRECTION('center_axis',(0.869726513699833,0.,-0.49353398197848));
#40476=DIRECTION('ref_axis',(-0.49353398197848,0.,-0.869726513699833));
#40477=DIRECTION('',(-0.49353398197848,0.,-0.869726513699833));
#40478=DIRECTION('',(0.,1.,0.));
#40479=DIRECTION('center_axis',(-0.986074150277955,0.,-0.166306254102513));
#40480=DIRECTION('ref_axis',(-0.166306254102513,0.,0.986074150277955));
#40481=DIRECTION('',(-0.166306254102513,0.,0.986074150277955));
#40482=DIRECTION('center_axis',(0.,1.,0.));
#40483=DIRECTION('ref_axis',(-0.984807753012208,0.,0.17364817766693));
#40484=DIRECTION('center_axis',(0.,1.,0.));
#40485=DIRECTION('ref_axis',(-1.,0.,-1.83697019872103E-16));
#40486=DIRECTION('',(-0.335009667654806,0.,0.94221469027914));
#40487=DIRECTION('',(-0.335009667654806,0.,-0.94221469027914));
#40488=DIRECTION('center_axis',(0.94221469027914,0.,-0.335009667654806));
#40489=DIRECTION('ref_axis',(-0.335009667654806,0.,-0.94221469027914));
#40490=DIRECTION('',(0.,1.,0.));
#40491=DIRECTION('center_axis',(-0.94221469027914,0.,-0.335009667654806));
#40492=DIRECTION('ref_axis',(-0.335009667654806,0.,0.94221469027914));
#40493=DIRECTION('center_axis',(0.986074150277955,0.,-0.166306254102512));
#40494=DIRECTION('ref_axis',(-0.166306254102512,0.,-0.986074150277955));
#40495=DIRECTION('',(-0.166306254102512,0.,-0.986074150277955));
#40496=DIRECTION('',(0.,1.,0.));
#40497=DIRECTION('center_axis',(-0.869726513699833,0.,-0.49353398197848));
#40498=DIRECTION('ref_axis',(-0.49353398197848,0.,0.869726513699833));
#40499=DIRECTION('',(-0.49353398197848,0.,0.869726513699833));
#40500=DIRECTION('center_axis',(0.,1.,0.));
#40501=DIRECTION('ref_axis',(-0.984807753012208,0.,-0.17364817766693));
#40502=DIRECTION('center_axis',(0.,1.,0.));
#40503=DIRECTION('ref_axis',(-0.939692620785908,0.,-0.342020143325669));
#40504=DIRECTION('',(-0.637062515999984,0.,0.770812137104606));
#40505=DIRECTION('',(0.00745029082566179,0.,-0.99997224619817));
#40506=DIRECTION('center_axis',(0.99997224619817,0.,0.00745029082566179));
#40507=DIRECTION('ref_axis',(0.00745029082566179,0.,-0.99997224619817));
#40508=DIRECTION('',(0.,1.,0.));
#40509=DIRECTION('center_axis',(-0.770812137104606,0.,-0.637062515999984));
#40510=DIRECTION('ref_axis',(-0.637062515999984,0.,0.770812137104606));
#40511=DIRECTION('center_axis',(0.983486691428025,0.,0.180980462437127));
#40512=DIRECTION('ref_axis',(0.180980462437127,0.,-0.983486691428025));
#40513=DIRECTION('',(0.180980462437127,0.,-0.983486691428025));
#40514=DIRECTION('',(0.,1.,0.));
#40515=DIRECTION('center_axis',(-0.648477023773219,0.,-0.761234227842015));
#40516=DIRECTION('ref_axis',(-0.761234227842015,0.,0.648477023773219));
#40517=DIRECTION('',(-0.761234227842015,0.,0.648477023773219));
#40518=DIRECTION('center_axis',(0.,1.,0.));
#40519=DIRECTION('ref_axis',(-0.866025403784438,0.,-0.5));
#40520=DIRECTION('center_axis',(0.,1.,0.));
#40521=DIRECTION('ref_axis',(-0.766044443118978,0.,-0.642787609686539));
#40522=DIRECTION('',(-0.862276222874172,0.,0.506438264219689));
#40523=DIRECTION('',(0.349011634277972,0.,-0.937118391207119));
#40524=DIRECTION('center_axis',(0.937118391207119,0.,0.349011634277972));
#40525=DIRECTION('ref_axis',(0.349011634277972,0.,-0.937118391207119));
#40526=DIRECTION('',(0.,1.,0.));
#40527=DIRECTION('center_axis',(-0.506438264219689,0.,-0.862276222874172));
#40528=DIRECTION('ref_axis',(-0.862276222874172,0.,0.506438264219689));
#40529=DIRECTION('center_axis',(0.862276222874171,0.,0.50643826421969));
#40530=DIRECTION('ref_axis',(0.50643826421969,0.,-0.862276222874171));
#40531=DIRECTION('',(0.50643826421969,0.,-0.862276222874171));
#40532=DIRECTION('',(0.,1.,0.));
#40533=DIRECTION('center_axis',(-0.349011634277972,0.,-0.937118391207119));
#40534=DIRECTION('ref_axis',(-0.937118391207119,0.,0.349011634277972));
#40535=DIRECTION('',(-0.937118391207119,0.,0.349011634277972));
#40536=DIRECTION('center_axis',(0.,1.,0.));
#40537=DIRECTION('ref_axis',(-0.642787609686539,0.,-0.766044443118978));
#40538=DIRECTION('center_axis',(0.,1.,0.));
#40539=DIRECTION('ref_axis',(-0.5,0.,-0.866025403784439));
#40540=DIRECTION('',(-0.983486691428025,0.,0.180980462437126));
#40541=DIRECTION('',(0.648477023773219,0.,-0.761234227842014));
#40542=DIRECTION('center_axis',(0.761234227842014,0.,0.648477023773219));
#40543=DIRECTION('ref_axis',(0.648477023773219,0.,-0.761234227842014));
#40544=DIRECTION('',(0.,1.,0.));
#40545=DIRECTION('center_axis',(-0.180980462437126,0.,-0.983486691428025));
#40546=DIRECTION('ref_axis',(-0.983486691428025,0.,0.180980462437126));
#40547=DIRECTION('center_axis',(0.637062515999983,0.,0.770812137104607));
#40548=DIRECTION('ref_axis',(0.770812137104607,0.,-0.637062515999983));
#40549=DIRECTION('',(0.770812137104607,0.,-0.637062515999983));
#40550=DIRECTION('',(0.,1.,0.));
#40551=DIRECTION('center_axis',(-0.00745029082566107,0.,-0.99997224619817));
#40552=DIRECTION('ref_axis',(-0.99997224619817,0.,0.00745029082566107));
#40553=DIRECTION('',(-0.99997224619817,0.,0.00745029082566107));
#40554=DIRECTION('center_axis',(0.,1.,0.));
#40555=DIRECTION('ref_axis',(-0.342020143325669,0.,-0.939692620785908));
#40556=DIRECTION('center_axis',(0.,1.,0.));
#40557=DIRECTION('ref_axis',(-0.17364817766693,0.,-0.984807753012208));
#40558=DIRECTION('',(-0.986074150277955,0.,-0.166306254102513));
#40559=DIRECTION('',(0.869726513699833,0.,-0.49353398197848));
#40560=DIRECTION('center_axis',(0.49353398197848,0.,0.869726513699833));
#40561=DIRECTION('ref_axis',(0.869726513699833,0.,-0.49353398197848));
#40562=DIRECTION('',(0.,1.,0.));
#40563=DIRECTION('center_axis',(0.166306254102513,0.,-0.986074150277955));
#40564=DIRECTION('ref_axis',(-0.986074150277955,0.,-0.166306254102513));
#40565=DIRECTION('center_axis',(0.335009667654806,0.,0.94221469027914));
#40566=DIRECTION('ref_axis',(0.94221469027914,0.,-0.335009667654806));
#40567=DIRECTION('',(0.94221469027914,0.,-0.335009667654806));
#40568=DIRECTION('',(0.,1.,0.));
#40569=DIRECTION('center_axis',(0.335009667654806,0.,-0.94221469027914));
#40570=DIRECTION('ref_axis',(-0.94221469027914,0.,-0.335009667654806));
#40571=DIRECTION('',(-0.94221469027914,0.,-0.335009667654806));
#40572=DIRECTION('center_axis',(0.,1.,0.));
#40573=DIRECTION('ref_axis',(1.22464679914735E-16,0.,-1.));
#40574=DIRECTION('center_axis',(0.,1.,0.));
#40575=DIRECTION('ref_axis',(0.173648177666931,0.,-0.984807753012208));
#40576=DIRECTION('',(-0.869726513699832,0.,-0.493533981978481));
#40577=DIRECTION('',(0.986074150277955,0.,-0.166306254102512));
#40578=DIRECTION('center_axis',(0.166306254102512,0.,0.986074150277955));
#40579=DIRECTION('ref_axis',(0.986074150277955,0.,-0.166306254102512));
#40580=DIRECTION('',(0.,1.,0.));
#40581=DIRECTION('center_axis',(0.493533981978481,0.,-0.869726513699832));
#40582=DIRECTION('ref_axis',(-0.869726513699832,0.,-0.493533981978481));
#40583=DIRECTION('center_axis',(-0.00745029082566129,0.,0.99997224619817));
#40584=DIRECTION('ref_axis',(0.99997224619817,0.,0.00745029082566129));
#40585=DIRECTION('',(0.99997224619817,0.,0.00745029082566129));
#40586=DIRECTION('',(0.,1.,0.));
#40587=DIRECTION('center_axis',(0.637062515999983,0.,-0.770812137104607));
#40588=DIRECTION('ref_axis',(-0.770812137104607,0.,-0.637062515999983));
#40589=DIRECTION('',(-0.770812137104607,0.,-0.637062515999983));
#40590=DIRECTION('center_axis',(0.,1.,0.));
#40591=DIRECTION('ref_axis',(0.342020143325669,0.,-0.939692620785908));
#40592=DIRECTION('center_axis',(0.,1.,0.));
#40593=DIRECTION('ref_axis',(0.5,0.,-0.866025403784439));
#40594=DIRECTION('',(-0.648477023773219,0.,-0.761234227842014));
#40595=DIRECTION('',(0.983486691428025,0.,0.180980462437126));
#40596=DIRECTION('center_axis',(-0.180980462437126,0.,0.983486691428025));
#40597=DIRECTION('ref_axis',(0.983486691428025,0.,0.180980462437126));
#40598=DIRECTION('',(0.,1.,0.));
#40599=DIRECTION('center_axis',(0.761234227842014,0.,-0.648477023773219));
#40600=DIRECTION('ref_axis',(-0.648477023773219,0.,-0.761234227842014));
#40601=DIRECTION('center_axis',(-0.349011634277972,0.,0.937118391207119));
#40602=DIRECTION('ref_axis',(0.937118391207119,0.,0.349011634277972));
#40603=DIRECTION('',(0.937118391207119,0.,0.349011634277972));
#40604=DIRECTION('',(0.,1.,0.));
#40605=DIRECTION('center_axis',(0.862276222874172,0.,-0.506438264219689));
#40606=DIRECTION('ref_axis',(-0.506438264219689,0.,-0.862276222874172));
#40607=DIRECTION('',(-0.506438264219689,0.,-0.862276222874172));
#40608=DIRECTION('center_axis',(0.,1.,0.));
#40609=DIRECTION('ref_axis',(0.642787609686539,0.,-0.766044443118978));
#40610=DIRECTION('center_axis',(0.,1.,0.));
#40611=DIRECTION('ref_axis',(0.766044443118978,0.,-0.642787609686539));
#40612=DIRECTION('',(-0.349011634277972,0.,-0.937118391207119));
#40613=DIRECTION('',(0.862276222874172,0.,0.506438264219689));
#40614=DIRECTION('center_axis',(-0.50643826421969,0.,0.862276222874171));
#40615=DIRECTION('ref_axis',(0.862276222874171,0.,0.50643826421969));
#40616=DIRECTION('',(0.,1.,0.));
#40617=DIRECTION('center_axis',(0.937118391207119,0.,-0.349011634277972));
#40618=DIRECTION('ref_axis',(-0.349011634277972,0.,-0.937118391207119));
#40619=DIRECTION('center_axis',(-0.648477023773219,0.,0.761234227842014));
#40620=DIRECTION('ref_axis',(0.761234227842014,0.,0.648477023773219));
#40621=DIRECTION('',(0.761234227842014,0.,0.648477023773219));
#40622=DIRECTION('',(0.,1.,0.));
#40623=DIRECTION('center_axis',(0.983486691428025,0.,-0.180980462437126));
#40624=DIRECTION('ref_axis',(-0.180980462437126,0.,-0.983486691428025));
#40625=DIRECTION('',(-0.180980462437126,0.,-0.983486691428025));
#40626=DIRECTION('center_axis',(0.,1.,0.));
#40627=DIRECTION('ref_axis',(0.866025403784439,0.,-0.5));
#40628=DIRECTION('center_axis',(0.,1.,0.));
#40629=DIRECTION('ref_axis',(0.939692620785908,0.,-0.342020143325669));
#40630=DIRECTION('',(-0.00745029082566112,0.,-0.99997224619817));
#40631=DIRECTION('',(0.637062515999983,0.,0.770812137104607));
#40632=DIRECTION('center_axis',(-0.770812137104607,0.,0.637062515999983));
#40633=DIRECTION('ref_axis',(0.637062515999983,0.,0.770812137104607));
#40634=DIRECTION('',(0.,1.,0.));
#40635=DIRECTION('center_axis',(0.99997224619817,0.,-0.00745029082566112));
#40636=DIRECTION('ref_axis',(-0.00745029082566112,0.,-0.99997224619817));
#40637=DIRECTION('center_axis',(-0.869726513699833,0.,0.49353398197848));
#40638=DIRECTION('ref_axis',(0.49353398197848,0.,0.869726513699833));
#40639=DIRECTION('',(0.49353398197848,0.,0.869726513699833));
#40640=DIRECTION('',(0.,1.,0.));
#40641=DIRECTION('center_axis',(0.986074150277955,0.,0.166306254102512));
#40642=DIRECTION('ref_axis',(0.166306254102512,0.,-0.986074150277955));
#40643=DIRECTION('',(0.166306254102512,0.,-0.986074150277955));
#40644=DIRECTION('center_axis',(0.,1.,0.));
#40645=DIRECTION('ref_axis',(0.984807753012208,0.,-0.17364817766693));
#40646=DIRECTION('center_axis',(0.,1.,0.));
#40647=DIRECTION('ref_axis',(1.,0.,6.12323399573677E-17));
#40648=DIRECTION('',(0.335009667654806,0.,-0.94221469027914));
#40649=DIRECTION('',(0.335009667654806,0.,0.94221469027914));
#40650=DIRECTION('center_axis',(-0.94221469027914,0.,0.335009667654806));
#40651=DIRECTION('ref_axis',(0.335009667654806,0.,0.94221469027914));
#40652=DIRECTION('',(0.,1.,0.));
#40653=DIRECTION('center_axis',(0.94221469027914,0.,0.335009667654806));
#40654=DIRECTION('ref_axis',(0.335009667654806,0.,-0.94221469027914));
#40655=DIRECTION('center_axis',(-0.986074150277955,0.,0.166306254102512));
#40656=DIRECTION('ref_axis',(0.166306254102512,0.,0.986074150277955));
#40657=DIRECTION('',(0.166306254102512,0.,0.986074150277955));
#40658=DIRECTION('',(0.,1.,0.));
#40659=DIRECTION('center_axis',(0.869726513699833,0.,0.49353398197848));
#40660=DIRECTION('ref_axis',(0.49353398197848,0.,-0.869726513699833));
#40661=DIRECTION('',(0.49353398197848,0.,-0.869726513699833));
#40662=DIRECTION('center_axis',(0.,1.,0.));
#40663=DIRECTION('ref_axis',(0.984807753012208,0.,0.17364817766693));
#40664=DIRECTION('center_axis',(0.,1.,0.));
#40665=DIRECTION('ref_axis',(0.939692620785908,0.,0.342020143325669));
#40666=DIRECTION('',(0.637062515999983,0.,-0.770812137104607));
#40667=DIRECTION('',(-0.00745029082566129,0.,0.99997224619817));
#40668=DIRECTION('center_axis',(-0.99997224619817,0.,-0.00745029082566129));
#40669=DIRECTION('ref_axis',(-0.00745029082566129,0.,0.99997224619817));
#40670=DIRECTION('',(0.,1.,0.));
#40671=DIRECTION('center_axis',(0.770812137104607,0.,0.637062515999983));
#40672=DIRECTION('ref_axis',(0.637062515999983,0.,-0.770812137104607));
#40673=DIRECTION('center_axis',(-0.983486691428025,0.,-0.180980462437126));
#40674=DIRECTION('ref_axis',(-0.180980462437126,0.,0.983486691428025));
#40675=DIRECTION('',(-0.180980462437126,0.,0.983486691428025));
#40676=DIRECTION('',(0.,1.,0.));
#40677=DIRECTION('center_axis',(0.648477023773219,0.,0.761234227842014));
#40678=DIRECTION('ref_axis',(0.761234227842014,0.,-0.648477023773219));
#40679=DIRECTION('',(0.761234227842014,0.,-0.648477023773219));
#40680=DIRECTION('center_axis',(0.,1.,0.));
#40681=DIRECTION('ref_axis',(0.866025403784439,0.,0.5));
#40682=DIRECTION('center_axis',(0.,1.,0.));
#40683=DIRECTION('ref_axis',(0.766044443118978,0.,0.642787609686539));
#40684=DIRECTION('',(0.862276222874172,0.,-0.506438264219689));
#40685=DIRECTION('',(-0.349011634277972,0.,0.937118391207119));
#40686=DIRECTION('center_axis',(-0.937118391207119,0.,-0.349011634277972));
#40687=DIRECTION('ref_axis',(-0.349011634277972,0.,0.937118391207119));
#40688=DIRECTION('',(0.,1.,0.));
#40689=DIRECTION('center_axis',(0.50643826421969,0.,0.862276222874171));
#40690=DIRECTION('ref_axis',(0.862276222874171,0.,-0.50643826421969));
#40691=DIRECTION('center_axis',(-0.862276222874171,0.,-0.50643826421969));
#40692=DIRECTION('ref_axis',(-0.50643826421969,0.,0.862276222874171));
#40693=DIRECTION('',(-0.50643826421969,0.,0.862276222874171));
#40694=DIRECTION('',(0.,1.,0.));
#40695=DIRECTION('center_axis',(0.349011634277972,0.,0.937118391207119));
#40696=DIRECTION('ref_axis',(0.937118391207119,0.,-0.349011634277972));
#40697=DIRECTION('',(0.937118391207119,0.,-0.349011634277972));
#40698=DIRECTION('center_axis',(0.,1.,0.));
#40699=DIRECTION('ref_axis',(0.642787609686539,0.,0.766044443118978));
#40700=DIRECTION('center_axis',(0.,1.,0.));
#40701=DIRECTION('ref_axis',(0.5,0.,0.866025403784439));
#40702=DIRECTION('',(0.983486691428025,0.,-0.180980462437126));
#40703=DIRECTION('',(-0.648477023773219,0.,0.761234227842014));
#40704=DIRECTION('center_axis',(-0.761234227842014,0.,-0.648477023773219));
#40705=DIRECTION('ref_axis',(-0.648477023773219,0.,0.761234227842014));
#40706=DIRECTION('',(0.,1.,0.));
#40707=DIRECTION('center_axis',(0.180980462437126,0.,0.983486691428025));
#40708=DIRECTION('ref_axis',(0.983486691428025,0.,-0.180980462437126));
#40709=DIRECTION('center_axis',(-0.637062515999983,0.,-0.770812137104607));
#40710=DIRECTION('ref_axis',(-0.770812137104607,0.,0.637062515999983));
#40711=DIRECTION('',(-0.770812137104607,0.,0.637062515999983));
#40712=DIRECTION('',(0.,1.,0.));
#40713=DIRECTION('center_axis',(0.00745029082566112,0.,0.99997224619817));
#40714=DIRECTION('ref_axis',(0.99997224619817,0.,-0.00745029082566112));
#40715=DIRECTION('',(0.99997224619817,0.,-0.00745029082566112));
#40716=DIRECTION('center_axis',(0.,1.,0.));
#40717=DIRECTION('ref_axis',(0.342020143325669,0.,0.939692620785908));
#40718=DIRECTION('center_axis',(0.,1.,0.));
#40719=DIRECTION('ref_axis',(0.17364817766693,0.,0.984807753012208));
#40720=DIRECTION('',(0.986074150277955,0.,0.166306254102512));
#40721=DIRECTION('',(-0.869726513699833,0.,0.49353398197848));
#40722=DIRECTION('center_axis',(-0.49353398197848,0.,-0.869726513699833));
#40723=DIRECTION('ref_axis',(-0.869726513699833,0.,0.49353398197848));
#40724=DIRECTION('',(0.,1.,0.));
#40725=DIRECTION('center_axis',(-0.166306254102512,0.,0.986074150277955));
#40726=DIRECTION('ref_axis',(0.986074150277955,0.,0.166306254102512));
#40727=DIRECTION('center_axis',(-0.335009667654806,0.,-0.94221469027914));
#40728=DIRECTION('ref_axis',(-0.94221469027914,0.,0.335009667654806));
#40729=DIRECTION('',(-0.94221469027914,0.,0.335009667654806));
#40730=DIRECTION('',(0.,1.,0.));
#40731=DIRECTION('center_axis',(-0.335009667654806,0.,0.94221469027914));
#40732=DIRECTION('ref_axis',(0.94221469027914,0.,0.335009667654806));
#40733=DIRECTION('',(0.94221469027914,0.,0.335009667654806));
#40734=DIRECTION('center_axis',(0.,1.,0.));
#40735=DIRECTION('ref_axis',(0.,0.,1.));
#40736=DIRECTION('center_axis',(0.,1.,0.));
#40737=DIRECTION('ref_axis',(0.,0.,1.));
#40738=DIRECTION('center_axis',(-1.,0.,0.));
#40739=DIRECTION('ref_axis',(0.,0.,-1.));
#40740=DIRECTION('center_axis',(0.,1.,0.));
#40741=DIRECTION('ref_axis',(1.,0.,0.));
#40742=DIRECTION('center_axis',(0.,1.,0.));
#40743=DIRECTION('ref_axis',(1.,0.,0.));
#40744=DIRECTION('center_axis',(0.,-1.,0.));
#40745=DIRECTION('ref_axis',(1.,0.,0.));
#40746=DIRECTION('center_axis',(0.,-1.,0.));
#40747=DIRECTION('ref_axis',(1.,0.,0.));
#40748=DIRECTION('center_axis',(0.,-1.,0.));
#40749=DIRECTION('ref_axis',(1.,0.,0.));
#40750=DIRECTION('center_axis',(0.,-1.,0.));
#40751=DIRECTION('ref_axis',(1.,0.,0.));
#40752=DIRECTION('center_axis',(0.,-1.,0.));
#40753=DIRECTION('ref_axis',(1.,0.,0.));
#40754=DIRECTION('center_axis',(0.,-1.,0.));
#40755=DIRECTION('ref_axis',(1.,0.,0.));
#40756=DIRECTION('center_axis',(0.,-1.,0.));
#40757=DIRECTION('ref_axis',(1.,0.,0.));
#40758=DIRECTION('',(-0.707106781186548,-0.707106781186547,-8.65956056235494E-17));
#40759=DIRECTION('center_axis',(0.,-1.,0.));
#40760=DIRECTION('ref_axis',(1.,0.,0.));
#40761=DIRECTION('',(0.,-1.,0.));
#40762=DIRECTION('',(0.,1.,0.));
#40763=DIRECTION('center_axis',(0.,-1.,0.));
#40764=DIRECTION('ref_axis',(1.,0.,0.));
#40765=DIRECTION('center_axis',(0.,-1.,0.));
#40766=DIRECTION('ref_axis',(1.,0.,0.));
#40767=DIRECTION('',(0.,1.,0.));
#40768=DIRECTION('center_axis',(0.,-1.,0.));
#40769=DIRECTION('ref_axis',(1.,0.,0.));
#40770=DIRECTION('',(0.,-1.,0.));
#40771=DIRECTION('center_axis',(0.,-1.,0.));
#40772=DIRECTION('ref_axis',(1.,0.,0.));
#40773=DIRECTION('',(0.,-1.,0.));
#40774=DIRECTION('',(0.,1.,0.));
#40775=DIRECTION('center_axis',(0.,-1.,0.));
#40776=DIRECTION('ref_axis',(1.,0.,0.));
#40777=DIRECTION('center_axis',(0.,-1.,0.));
#40778=DIRECTION('ref_axis',(1.,0.,0.));
#40779=DIRECTION('',(0.,1.,0.));
#40780=DIRECTION('center_axis',(0.,-1.,0.));
#40781=DIRECTION('ref_axis',(1.,0.,0.));
#40782=DIRECTION('',(0.,-1.,0.));
#40783=DIRECTION('center_axis',(0.,-1.,0.));
#40784=DIRECTION('ref_axis',(1.,0.,0.));
#40785=DIRECTION('',(0.,-1.,0.));
#40786=DIRECTION('',(0.,1.,0.));
#40787=DIRECTION('center_axis',(0.,-1.,0.));
#40788=DIRECTION('ref_axis',(1.,0.,0.));
#40789=DIRECTION('center_axis',(0.,-1.,0.));
#40790=DIRECTION('ref_axis',(1.,0.,0.));
#40791=DIRECTION('',(0.,1.,0.));
#40792=DIRECTION('center_axis',(0.,-1.,0.));
#40793=DIRECTION('ref_axis',(1.,0.,0.));
#40794=DIRECTION('',(0.,-1.,0.));
#40795=DIRECTION('center_axis',(0.,0.,1.));
#40796=DIRECTION('ref_axis',(1.,0.,0.));
#40797=DIRECTION('',(1.,0.,0.));
#40798=DIRECTION('',(0.,1.,0.));
#40799=DIRECTION('',(1.,0.,0.));
#40800=DIRECTION('',(0.,1.,0.));
#40801=DIRECTION('center_axis',(-0.866025403784439,0.,0.499999999999999));
#40802=DIRECTION('ref_axis',(0.499999999999999,0.,0.866025403784439));
#40803=DIRECTION('',(0.499999999999999,0.,0.866025403784439));
#40804=DIRECTION('',(0.,1.,0.));
#40805=DIRECTION('',(0.499999999999999,0.,0.866025403784439));
#40806=DIRECTION('center_axis',(-0.866025403784439,0.,-0.499999999999999));
#40807=DIRECTION('ref_axis',(-0.499999999999999,0.,0.866025403784439));
#40808=DIRECTION('',(-0.499999999999999,0.,0.866025403784439));
#40809=DIRECTION('',(0.,1.,0.));
#40810=DIRECTION('',(-0.499999999999999,0.,0.866025403784439));
#40811=DIRECTION('center_axis',(0.,1.,0.));
#40812=DIRECTION('ref_axis',(1.,0.,0.));
#40813=DIRECTION('center_axis',(0.,1.,0.));
#40814=DIRECTION('ref_axis',(1.,0.,0.));
#40815=DIRECTION('center_axis',(0.,1.,0.));
#40816=DIRECTION('ref_axis',(1.,0.,0.));
#40817=DIRECTION('',(-1.,0.,0.));
#40818=DIRECTION('center_axis',(0.,1.,0.));
#40819=DIRECTION('ref_axis',(1.,0.,0.));
#40820=DIRECTION('center_axis',(0.,1.,0.));
#40821=DIRECTION('ref_axis',(1.,0.,0.));
#40822=DIRECTION('',(-0.499999999999999,0.,-0.866025403784439));
#40823=DIRECTION('center_axis',(0.,1.,0.));
#40824=DIRECTION('ref_axis',(1.,0.,0.));
#40825=DIRECTION('',(0.5,0.,-0.866025403784439));
#40826=DIRECTION('center_axis',(0.,-1.,0.));
#40827=DIRECTION('ref_axis',(0.,0.,-1.));
#40828=DIRECTION('',(-0.499999999999999,0.,-0.866025403784439));
#40829=DIRECTION('center_axis',(0.,-1.,0.));
#40830=DIRECTION('ref_axis',(1.,0.,0.));
#40831=DIRECTION('center_axis',(0.,-1.,0.));
#40832=DIRECTION('ref_axis',(0.,0.,-1.));
#40833=DIRECTION('',(-1.,0.,0.));
#40834=DIRECTION('center_axis',(0.,-1.,0.));
#40835=DIRECTION('ref_axis',(1.,0.,0.));
#40836=DIRECTION('center_axis',(0.,-1.,0.));
#40837=DIRECTION('ref_axis',(0.,0.,-1.));
#40838=DIRECTION('center_axis',(0.,-1.,0.));
#40839=DIRECTION('ref_axis',(1.,0.,0.));
#40840=DIRECTION('center_axis',(0.,-1.,0.));
#40841=DIRECTION('ref_axis',(0.,0.,-1.));
#40842=DIRECTION('center_axis',(0.,-1.,0.));
#40843=DIRECTION('ref_axis',(1.,0.,0.));
#40844=DIRECTION('center_axis',(0.,-1.,0.));
#40845=DIRECTION('ref_axis',(0.,0.,-1.));
#40846=DIRECTION('center_axis',(0.,-1.,0.));
#40847=DIRECTION('ref_axis',(1.,0.,0.));
#40848=DIRECTION('center_axis',(0.,-1.,0.));
#40849=DIRECTION('ref_axis',(0.,0.,-1.));
#40850=DIRECTION('',(0.5,0.,-0.866025403784439));
#40851=DIRECTION('center_axis',(0.,-1.,0.));
#40852=DIRECTION('ref_axis',(1.,0.,0.));
#40853=DIRECTION('center_axis',(0.,-1.,0.));
#40854=DIRECTION('ref_axis',(1.,0.,0.));
#40855=DIRECTION('',(-0.85716730070211,-0.515038074910058,-1.04972719113862E-16));
#40856=DIRECTION('center_axis',(0.866025403784439,0.,-0.499999999999999));
#40857=DIRECTION('ref_axis',(-0.499999999999999,0.,-0.866025403784439));
#40858=DIRECTION('',(0.,1.,0.));
#40859=DIRECTION('',(0.,1.,0.));
#40860=DIRECTION('center_axis',(0.866025403784439,0.,0.5));
#40861=DIRECTION('ref_axis',(0.5,0.,-0.866025403784439));
#40862=DIRECTION('center_axis',(0.,0.,-1.));
#40863=DIRECTION('ref_axis',(-1.,0.,0.));
#40864=DIRECTION('axis',(0.,0.,1.));
#40865=DIRECTION('refdir',(1.,0.,0.));
#40866=DIRECTION('center_axis',(1.,0.,0.));
#40867=DIRECTION('ref_axis',(0.,1.,0.));
#40868=DIRECTION('',(-1.,0.,0.));
#40869=DIRECTION('center_axis',(1.,0.,0.));
#40870=DIRECTION('ref_axis',(0.,1.,0.));
#40871=DIRECTION('center_axis',(1.,0.,0.));
#40872=DIRECTION('ref_axis',(0.,1.,0.));
#40873=DIRECTION('',(-1.,0.,0.));
#40874=DIRECTION('center_axis',(1.,0.,0.));
#40875=DIRECTION('ref_axis',(0.,1.,0.));
#40876=DIRECTION('',(-1.,0.,0.));
#40877=DIRECTION('center_axis',(1.,0.,0.));
#40878=DIRECTION('ref_axis',(0.,1.,0.));
#40879=DIRECTION('',(-1.,0.,0.));
#40880=DIRECTION('center_axis',(1.,0.,0.));
#40881=DIRECTION('ref_axis',(0.,1.,0.));
#40882=DIRECTION('',(-1.,0.,0.));
#40883=DIRECTION('center_axis',(1.,0.,0.));
#40884=DIRECTION('ref_axis',(0.,1.,0.));
#40885=DIRECTION('',(-1.,0.,0.));
#40886=DIRECTION('center_axis',(1.,0.,0.));
#40887=DIRECTION('ref_axis',(0.,1.,0.));
#40888=DIRECTION('',(-1.,0.,0.));
#40889=DIRECTION('center_axis',(1.,0.,0.));
#40890=DIRECTION('ref_axis',(0.,1.,0.));
#40891=DIRECTION('',(-1.,0.,0.));
#40892=DIRECTION('center_axis',(1.,0.,0.));
#40893=DIRECTION('ref_axis',(0.,1.,0.));
#40894=DIRECTION('',(-1.,0.,0.));
#40895=DIRECTION('center_axis',(1.,0.,0.));
#40896=DIRECTION('ref_axis',(0.,1.,0.));
#40897=DIRECTION('',(-1.,0.,0.));
#40898=DIRECTION('center_axis',(1.,0.,0.));
#40899=DIRECTION('ref_axis',(0.,1.,0.));
#40900=DIRECTION('',(-1.,0.,0.));
#40901=DIRECTION('center_axis',(1.,0.,0.));
#40902=DIRECTION('ref_axis',(0.,0.941532254165013,-0.336922861152149));
#40903=DIRECTION('',(-1.,0.,0.));
#40904=DIRECTION('center_axis',(-1.,0.,0.));
#40905=DIRECTION('ref_axis',(0.,1.,6.6102588746288E-14));
#40906=DIRECTION('center_axis',(1.,0.,0.));
#40907=DIRECTION('ref_axis',(0.,0.941532254165013,-0.336922861152149));
#40908=DIRECTION('',(-1.,0.,0.));
#40909=DIRECTION('center_axis',(1.,0.,0.));
#40910=DIRECTION('ref_axis',(0.,0.941532254165013,-0.336922861152149));
#40911=DIRECTION('',(-1.,0.,0.));
#40912=DIRECTION('center_axis',(1.,0.,0.));
#40913=DIRECTION('ref_axis',(0.,0.941532254165013,-0.336922861152149));
#40914=DIRECTION('',(-1.,0.,0.));
#40915=DIRECTION('center_axis',(1.,0.,0.));
#40916=DIRECTION('ref_axis',(0.,0.941532254165013,-0.336922861152149));
#40917=DIRECTION('',(-1.,0.,0.));
#40918=DIRECTION('center_axis',(1.,0.,0.));
#40919=DIRECTION('ref_axis',(0.,0.941532254165013,-0.336922861152149));
#40920=DIRECTION('',(-1.,0.,0.));
#40921=DIRECTION('center_axis',(1.,0.,0.));
#40922=DIRECTION('ref_axis',(0.,0.941532254165013,-0.336922861152149));
#40923=DIRECTION('',(-1.,0.,0.));
#40924=DIRECTION('center_axis',(1.,0.,0.));
#40925=DIRECTION('ref_axis',(0.,0.941532254165013,-0.336922861152149));
#40926=DIRECTION('',(-1.,0.,0.));
#40927=DIRECTION('center_axis',(1.,0.,0.));
#40928=DIRECTION('ref_axis',(0.,0.941532254165013,-0.336922861152149));
#40929=DIRECTION('',(-1.,0.,0.));
#40930=DIRECTION('center_axis',(1.,0.,0.));
#40931=DIRECTION('ref_axis',(0.,0.941532254165013,-0.336922861152149));
#40932=DIRECTION('',(-1.,0.,0.));
#40933=DIRECTION('center_axis',(1.,0.,0.));
#40934=DIRECTION('ref_axis',(0.,0.941532254165013,-0.336922861152149));
#40935=DIRECTION('center_axis',(1.,0.,0.));
#40936=DIRECTION('ref_axis',(0.,1.,6.6102588746288E-14));
#40937=DIRECTION('center_axis',(1.,0.,0.));
#40938=DIRECTION('ref_axis',(0.,1.,0.));
#40939=DIRECTION('center_axis',(1.,0.,0.));
#40940=DIRECTION('ref_axis',(0.,1.,0.));
#40941=DIRECTION('center_axis',(1.,0.,0.));
#40942=DIRECTION('ref_axis',(0.,0.,-1.));
#40943=DIRECTION('center_axis',(1.,0.,0.));
#40944=DIRECTION('ref_axis',(0.,1.,0.));
#40945=DIRECTION('center_axis',(1.,0.,0.));
#40946=DIRECTION('ref_axis',(0.,1.,0.));
#40947=DIRECTION('center_axis',(1.,0.,0.));
#40948=DIRECTION('ref_axis',(0.,0.,-1.));
#40949=DIRECTION('center_axis',(-1.,0.,0.));
#40950=DIRECTION('ref_axis',(0.,1.,0.));
#40951=DIRECTION('center_axis',(0.,1.,0.));
#40952=DIRECTION('ref_axis',(0.,0.,1.));
#40953=DIRECTION('center_axis',(-1.,0.,0.));
#40954=DIRECTION('ref_axis',(0.,0.,1.));
#40955=DIRECTION('center_axis',(1.,0.,0.));
#40956=DIRECTION('ref_axis',(0.,0.,-1.));
#40957=DIRECTION('center_axis',(-1.,0.,0.));
#40958=DIRECTION('ref_axis',(0.,0.,1.));
#40959=DIRECTION('center_axis',(-1.,0.,0.));
#40960=DIRECTION('ref_axis',(0.,1.,0.));
#40961=DIRECTION('',(0.,-1.,0.));
#40962=DIRECTION('center_axis',(-1.,0.,0.));
#40963=DIRECTION('ref_axis',(0.,1.,0.));
#40964=DIRECTION('',(0.,1.,0.));
#40965=DIRECTION('center_axis',(-1.,0.,0.));
#40966=DIRECTION('ref_axis',(0.,1.,0.));
#40967=DIRECTION('center_axis',(0.,0.,1.));
#40968=DIRECTION('ref_axis',(0.,1.,0.));
#40969=DIRECTION('',(1.,0.,0.));
#40970=DIRECTION('',(-1.,0.,0.));
#40971=DIRECTION('',(0.,1.,0.));
#40972=DIRECTION('center_axis',(0.,0.,-1.));
#40973=DIRECTION('ref_axis',(0.,-1.,0.));
#40974=DIRECTION('',(-1.,0.,0.));
#40975=DIRECTION('',(0.,-1.,0.));
#40976=DIRECTION('',(1.,0.,0.));
#40977=DIRECTION('center_axis',(1.,0.,0.));
#40978=DIRECTION('ref_axis',(0.,1.,0.));
#40979=DIRECTION('',(-1.,0.,0.));
#40980=DIRECTION('center_axis',(1.,0.,0.));
#40981=DIRECTION('ref_axis',(0.,0.,-1.));
#40982=DIRECTION('center_axis',(1.,0.,0.));
#40983=DIRECTION('ref_axis',(0.,0.,-1.));
#40984=DIRECTION('center_axis',(1.,0.,0.));
#40985=DIRECTION('ref_axis',(0.,0.,-1.));
#40986=DIRECTION('center_axis',(1.,0.,0.));
#40987=DIRECTION('ref_axis',(0.,0.,-1.));
#40988=DIRECTION('center_axis',(1.,0.,0.));
#40989=DIRECTION('ref_axis',(0.,0.,-1.));
#40990=DIRECTION('center_axis',(1.,0.,0.));
#40991=DIRECTION('ref_axis',(0.,0.,-1.));
#40992=DIRECTION('center_axis',(-1.,0.,0.));
#40993=DIRECTION('ref_axis',(0.,1.,0.));
#40994=DIRECTION('center_axis',(-1.,0.,0.));
#40995=DIRECTION('ref_axis',(0.,0.,1.));
#40996=DIRECTION('center_axis',(1.,0.,0.));
#40997=DIRECTION('ref_axis',(0.,0.,-1.));
#40998=DIRECTION('center_axis',(-1.,0.,0.));
#40999=DIRECTION('ref_axis',(0.,1.,0.));
#41000=DIRECTION('',(-0.707106781186548,-0.707106781186547,8.65956056235493E-17));
#41001=DIRECTION('center_axis',(-1.,0.,0.));
#41002=DIRECTION('ref_axis',(0.,1.,0.));
#41003=DIRECTION('',(0.,0.,1.));
#41004=DIRECTION('',(1.,0.,0.));
#41005=DIRECTION('',(0.,0.,1.));
#41006=DIRECTION('',(1.,0.,0.));
#41007=DIRECTION('',(0.,0.,1.));
#41008=DIRECTION('',(1.,0.,0.));
#41009=DIRECTION('',(0.,0.,1.));
#41010=DIRECTION('',(1.,0.,0.));
#41011=DIRECTION('',(0.,0.,1.));
#41012=DIRECTION('',(1.,0.,0.));
#41013=DIRECTION('',(0.,0.,1.));
#41014=DIRECTION('',(1.,0.,0.));
#41015=DIRECTION('',(0.,0.,1.));
#41016=DIRECTION('',(1.,0.,0.));
#41017=DIRECTION('',(0.,0.,1.));
#41018=DIRECTION('',(1.,0.,0.));
#41019=DIRECTION('',(0.,0.,1.));
#41020=DIRECTION('',(1.,0.,0.));
#41021=DIRECTION('',(0.,0.,1.));
#41022=DIRECTION('',(1.,0.,0.));
#41023=DIRECTION('',(0.,0.,1.));
#41024=DIRECTION('',(1.,0.,0.));
#41025=DIRECTION('',(0.,0.,1.));
#41026=DIRECTION('',(1.,0.,0.));
#41027=DIRECTION('',(0.,0.,1.));
#41028=DIRECTION('',(1.,0.,0.));
#41029=DIRECTION('',(0.,0.,1.));
#41030=DIRECTION('',(-1.,1.22464679914735E-16,0.));
#41031=DIRECTION('',(0.,0.,1.));
#41032=DIRECTION('',(1.,0.,0.));
#41033=DIRECTION('',(0.,0.,1.));
#41034=DIRECTION('',(-1.,1.22464679914735E-16,0.));
#41035=DIRECTION('',(0.,0.,1.));
#41036=DIRECTION('',(-1.,1.22464679914735E-16,0.));
#41037=DIRECTION('',(0.,0.,1.));
#41038=DIRECTION('',(1.,0.,0.));
#41039=DIRECTION('',(0.,0.,1.));
#41040=DIRECTION('',(1.,0.,0.));
#41041=DIRECTION('',(0.,0.,1.));
#41042=DIRECTION('',(1.,0.,0.));
#41043=DIRECTION('',(0.,0.,1.));
#41044=DIRECTION('',(1.,0.,0.));
#41045=CARTESIAN_POINT('',(0.,0.,0.));
#41046=CARTESIAN_POINT('',(0.,0.,0.));
#41047=CARTESIAN_POINT('Origin',(10.,119.9,3.5));
#41048=CARTESIAN_POINT('',(8.45,119.8,3.5));
#41049=CARTESIAN_POINT('Origin',(10.,119.8,3.5));
#41050=CARTESIAN_POINT('',(8.25,120.,3.5));
#41051=CARTESIAN_POINT('',(8.35,119.9,3.5));
#41052=CARTESIAN_POINT('Origin',(10.,120.,3.5));
#41053=CARTESIAN_POINT('Origin',(0.,120.,8.));
#41054=CARTESIAN_POINT('',(-7.6,120.,15.8267949192431));
#41055=CARTESIAN_POINT('',(-7.7,120.,16.));
#41056=CARTESIAN_POINT('',(-4.98044919243113,120.,11.2895998275257));
#41057=CARTESIAN_POINT('',(-10.3867513459481,120.,11.));
#41058=CARTESIAN_POINT('',(-10.3867513459481,120.,11.));
#41059=CARTESIAN_POINT('',(-10.3867513459481,120.,7.));
#41060=CARTESIAN_POINT('',(-10.3867513459481,120.,7.));
#41061=CARTESIAN_POINT('',(10.3867513459481,120.,7.));
#41062=CARTESIAN_POINT('',(10.3867513459481,120.,7.));
#41063=CARTESIAN_POINT('',(10.3867513459481,120.,11.));
#41064=CARTESIAN_POINT('',(10.3867513459481,120.,11.));
#41065=CARTESIAN_POINT('',(7.6,120.,15.8267949192431));
#41066=CARTESIAN_POINT('',(7.5,120.,16.));
#41067=CARTESIAN_POINT('',(7.7,120.,16.));
#41068=CARTESIAN_POINT('',(4.98044919243111,120.,11.2895998275257));
#41069=CARTESIAN_POINT('',(12.1,120.,16.));
#41070=CARTESIAN_POINT('',(12.5,120.,16.));
#41071=CARTESIAN_POINT('',(12.5,120.,15.6));
#41072=CARTESIAN_POINT('',(11.175,120.,16.925));
#41073=CARTESIAN_POINT('',(12.5,120.,0.4));
#41074=CARTESIAN_POINT('',(12.5,120.,0.));
#41075=CARTESIAN_POINT('',(12.1,120.,0.));
#41076=CARTESIAN_POINT('',(11.175,120.,-0.925));
#41077=CARTESIAN_POINT('',(-12.1,120.,0.));
#41078=CARTESIAN_POINT('',(-12.5,120.,0.));
#41079=CARTESIAN_POINT('',(-12.5,120.,0.4));
#41080=CARTESIAN_POINT('',(-11.175,120.,-0.925000000000002));
#41081=CARTESIAN_POINT('',(-12.5,120.,15.6));
#41082=CARTESIAN_POINT('',(-12.5,120.,16.));
#41083=CARTESIAN_POINT('',(-12.1,120.,16.));
#41084=CARTESIAN_POINT('',(-11.175,120.,16.925));
#41085=CARTESIAN_POINT('',(-7.5,120.,16.));
#41086=CARTESIAN_POINT('',(-11.75,120.,3.5));
#41087=CARTESIAN_POINT('Origin',(-10.,120.,3.5));
#41088=CARTESIAN_POINT('Origin',(10.,120.,3.5));
#41089=CARTESIAN_POINT('',(8.45,112.,3.5));
#41090=CARTESIAN_POINT('',(8.45,120.,3.5));
#41091=CARTESIAN_POINT('Origin',(10.,112.,3.5));
#41092=CARTESIAN_POINT('Origin',(-10.,119.9,3.5));
#41093=CARTESIAN_POINT('',(-11.55,119.8,3.5));
#41094=CARTESIAN_POINT('Origin',(-10.,119.8,3.5));
#41095=CARTESIAN_POINT('',(-11.65,119.9,3.5));
#41096=CARTESIAN_POINT('Origin',(-10.,120.,3.5));
#41097=CARTESIAN_POINT('',(-11.55,112.,3.5));
#41098=CARTESIAN_POINT('',(-11.55,120.,3.5));
#41099=CARTESIAN_POINT('Origin',(-10.,112.,3.5));
#41100=CARTESIAN_POINT('Origin',(10.,112.,3.5));
#41101=CARTESIAN_POINT('',(10.,111.068666040507,3.5));
#41102=CARTESIAN_POINT('',(8.45,112.,3.5));
#41103=CARTESIAN_POINT('Origin',(-10.,112.,3.5));
#41104=CARTESIAN_POINT('',(-10.,111.068666040507,3.5));
#41105=CARTESIAN_POINT('',(-11.55,112.,3.5));
#41106=CARTESIAN_POINT('Origin',(10.,20.1,3.5));
#41107=CARTESIAN_POINT('',(8.45,20.2,3.5));
#41108=CARTESIAN_POINT('Origin',(10.,20.2,3.5));
#41109=CARTESIAN_POINT('',(8.25,20.,3.5));
#41110=CARTESIAN_POINT('',(8.35,20.1,3.5));
#41111=CARTESIAN_POINT('Origin',(10.,20.,3.5));
#41112=CARTESIAN_POINT('Origin',(0.,20.,8.));
#41113=CARTESIAN_POINT('',(-7.7,20.,16.));
#41114=CARTESIAN_POINT('',(-7.6,20.,15.8267949192431));
#41115=CARTESIAN_POINT('',(-4.98044919243113,20.,11.2895998275257));
#41116=CARTESIAN_POINT('',(-12.1,20.,16.));
#41117=CARTESIAN_POINT('',(-7.5,20.,16.));
#41118=CARTESIAN_POINT('',(-12.5,20.,15.6));
#41119=CARTESIAN_POINT('',(-11.175,20.,16.925));
#41120=CARTESIAN_POINT('',(-12.5,20.,0.4));
#41121=CARTESIAN_POINT('',(-12.5,20.,16.));
#41122=CARTESIAN_POINT('',(-12.1,20.,0.));
#41123=CARTESIAN_POINT('',(-11.175,20.,-0.925000000000002));
#41124=CARTESIAN_POINT('',(12.1,20.,0.));
#41125=CARTESIAN_POINT('',(-12.5,20.,0.));
#41126=CARTESIAN_POINT('',(12.5,20.,0.4));
#41127=CARTESIAN_POINT('',(11.175,20.,-0.925));
#41128=CARTESIAN_POINT('',(12.5,20.,15.6));
#41129=CARTESIAN_POINT('',(12.5,20.,0.));
#41130=CARTESIAN_POINT('',(12.1,20.,16.));
#41131=CARTESIAN_POINT('',(11.175,20.,16.925));
#41132=CARTESIAN_POINT('',(7.7,20.,16.));
#41133=CARTESIAN_POINT('',(12.5,20.,16.));
#41134=CARTESIAN_POINT('',(7.6,20.,15.8267949192431));
#41135=CARTESIAN_POINT('',(4.98044919243111,20.,11.2895998275257));
#41136=CARTESIAN_POINT('',(10.3867513459481,20.,11.));
#41137=CARTESIAN_POINT('',(7.5,20.,16.));
#41138=CARTESIAN_POINT('',(10.3867513459481,20.,7.));
#41139=CARTESIAN_POINT('',(10.3867513459481,20.,11.));
#41140=CARTESIAN_POINT('',(-10.3867513459481,20.,7.));
#41141=CARTESIAN_POINT('',(10.3867513459481,20.,7.));
#41142=CARTESIAN_POINT('',(-10.3867513459481,20.,11.));
#41143=CARTESIAN_POINT('',(-10.3867513459481,20.,7.));
#41144=CARTESIAN_POINT('',(-10.3867513459481,20.,11.));
#41145=CARTESIAN_POINT('',(-11.75,20.,3.5));
#41146=CARTESIAN_POINT('Origin',(-10.,20.,3.5));
#41147=CARTESIAN_POINT('Origin',(10.,20.,3.5));
#41148=CARTESIAN_POINT('',(8.45,28.,3.5));
#41149=CARTESIAN_POINT('',(8.45,20.,3.5));
#41150=CARTESIAN_POINT('Origin',(10.,28.,3.5));
#41151=CARTESIAN_POINT('Origin',(-10.,20.1,3.5));
#41152=CARTESIAN_POINT('',(-11.55,20.2,3.5));
#41153=CARTESIAN_POINT('Origin',(-10.,20.2,3.5));
#41154=CARTESIAN_POINT('',(-11.65,20.1,3.5));
#41155=CARTESIAN_POINT('Origin',(-10.,20.,3.5));
#41156=CARTESIAN_POINT('',(-11.55,28.,3.5));
#41157=CARTESIAN_POINT('',(-11.55,20.,3.5));
#41158=CARTESIAN_POINT('Origin',(-10.,28.,3.5));
#41159=CARTESIAN_POINT('Origin',(10.,28.4656669797464,3.5));
#41160=CARTESIAN_POINT('',(10.,28.9313339594927,3.5));
#41161=CARTESIAN_POINT('',(9.225,28.4656669797464,3.5));
#41162=CARTESIAN_POINT('Origin',(-10.,28.4656669797464,3.5));
#41163=CARTESIAN_POINT('',(-10.,28.9313339594927,3.5));
#41164=CARTESIAN_POINT('',(-10.775,28.4656669797464,3.5));
#41165=CARTESIAN_POINT('Origin',(-7.65,20.,15.9133974596216));
#41166=CARTESIAN_POINT('',(-7.7,20.,16.));
#41167=CARTESIAN_POINT('',(-7.6,20.,15.8267949192431));
#41168=CARTESIAN_POINT('Origin',(-12.5,20.,16.));
#41169=CARTESIAN_POINT('',(-12.1,20.,16.));
#41170=CARTESIAN_POINT('Origin',(7.65,20.,15.9133974596216));
#41171=CARTESIAN_POINT('',(7.6,20.,15.8267949192431));
#41172=CARTESIAN_POINT('',(7.7,20.,16.));
#41173=CARTESIAN_POINT('Origin',(7.5,20.,16.));
#41174=CARTESIAN_POINT('',(12.1,20.,16.));
#41175=CARTESIAN_POINT('Origin',(12.3,20.,15.8));
#41176=CARTESIAN_POINT('',(12.5,20.,15.6));
#41177=CARTESIAN_POINT('Origin',(12.3,20.,0.2));
#41178=CARTESIAN_POINT('',(12.5,20.,0.4));
#41179=CARTESIAN_POINT('',(12.1,20.,0.));
#41180=CARTESIAN_POINT('Origin',(12.5,20.,0.));
#41181=CARTESIAN_POINT('',(-12.1,20.,0.));
#41182=CARTESIAN_POINT('Origin',(-12.3,20.,0.2));
#41183=CARTESIAN_POINT('',(-12.5,20.,0.4));
#41184=CARTESIAN_POINT('Origin',(-12.3,20.,15.8));
#41185=CARTESIAN_POINT('',(-12.5,20.,15.6));
#41186=CARTESIAN_POINT('Origin',(-12.5,20.,0.));
#41187=CARTESIAN_POINT('Origin',(12.5,20.,16.));
#41188=CARTESIAN_POINT('Origin',(10.3867513459481,20.,11.));
#41189=CARTESIAN_POINT('',(10.3867513459481,20.,11.));
#41190=CARTESIAN_POINT('Origin',(10.3867513459481,20.,7.));
#41191=CARTESIAN_POINT('',(10.3867513459481,20.,7.));
#41192=CARTESIAN_POINT('Origin',(-10.3867513459481,20.,7.));
#41193=CARTESIAN_POINT('',(-10.3867513459481,20.,7.));
#41194=CARTESIAN_POINT('Origin',(-10.3867513459481,20.,11.));
#41195=CARTESIAN_POINT('',(-10.3867513459481,20.,11.));
#41196=CARTESIAN_POINT('Origin',(-7.5,20.,16.));
#41197=CARTESIAN_POINT('',(0.,0.,0.));
#41198=CARTESIAN_POINT('Origin',(12.425,73.,21.5));
#41199=CARTESIAN_POINT('',(12.35,73.,22.55));
#41200=CARTESIAN_POINT('Origin',(12.35,73.,21.5));
#41201=CARTESIAN_POINT('',(12.5,73.,22.7));
#41202=CARTESIAN_POINT('',(12.425,73.,22.625));
#41203=CARTESIAN_POINT('Origin',(12.5,73.,21.5));
#41204=CARTESIAN_POINT('Origin',(12.5,50.,26.3));
#41205=CARTESIAN_POINT('',(12.5,50.,25.8));
#41206=CARTESIAN_POINT('',(12.5,90.,25.8));
#41207=CARTESIAN_POINT('',(12.5,50.,25.8));
#41208=CARTESIAN_POINT('',(12.5,50.,16.15));
#41209=CARTESIAN_POINT('',(12.5,50.,16.15));
#41210=CARTESIAN_POINT('',(12.5,90.,16.15));
#41211=CARTESIAN_POINT('',(12.5,50.,16.15));
#41212=CARTESIAN_POINT('',(12.5,90.,16.15));
#41213=CARTESIAN_POINT('',(12.5,67.,22.7));
#41214=CARTESIAN_POINT('Origin',(12.5,67.,21.5));
#41215=CARTESIAN_POINT('Origin',(12.5,73.,21.5));
#41216=CARTESIAN_POINT('',(7.5,73.,22.55));
#41217=CARTESIAN_POINT('',(12.5,73.,22.55));
#41218=CARTESIAN_POINT('',(7.5,71.95,21.5));
#41219=CARTESIAN_POINT('Origin',(7.5,73.,21.5));
#41220=CARTESIAN_POINT('Origin',(7.5,73.,21.5));
#41221=CARTESIAN_POINT('Origin',(12.425,67.,21.5));
#41222=CARTESIAN_POINT('',(12.35,67.,22.55));
#41223=CARTESIAN_POINT('Origin',(12.35,67.,21.5));
#41224=CARTESIAN_POINT('',(12.425,67.,22.625));
#41225=CARTESIAN_POINT('Origin',(12.5,67.,21.5));
#41226=CARTESIAN_POINT('',(7.5,67.,22.55));
#41227=CARTESIAN_POINT('',(12.5,67.,22.55));
#41228=CARTESIAN_POINT('',(7.5,65.95,21.5));
#41229=CARTESIAN_POINT('Origin',(7.5,67.,21.5));
#41230=CARTESIAN_POINT('Origin',(7.5,67.,21.5));
#41231=CARTESIAN_POINT('Origin',(7.18454817501053,73.,21.5));
#41232=CARTESIAN_POINT('',(6.86909635002106,73.,21.5));
#41233=CARTESIAN_POINT('',(7.18454817501053,72.475,21.5));
#41234=CARTESIAN_POINT('Origin',(7.18454817501053,67.,21.5));
#41235=CARTESIAN_POINT('',(6.86909635002106,67.,21.5));
#41236=CARTESIAN_POINT('',(7.18454817501053,66.475,21.5));
#41237=CARTESIAN_POINT('Origin',(7.5,77.5,26.225));
#41238=CARTESIAN_POINT('',(6.45,77.5,26.15));
#41239=CARTESIAN_POINT('Origin',(7.5,77.5,26.15));
#41240=CARTESIAN_POINT('',(6.3,77.5,26.3));
#41241=CARTESIAN_POINT('',(6.375,77.5,26.225));
#41242=CARTESIAN_POINT('Origin',(7.5,77.5,26.3));
#41243=CARTESIAN_POINT('Origin',(-12.5,50.,26.3));
#41244=CARTESIAN_POINT('',(12.,50.5,26.3));
#41245=CARTESIAN_POINT('',(-12.,50.5,26.3));
#41246=CARTESIAN_POINT('',(-6.25,50.5,26.3));
#41247=CARTESIAN_POINT('',(12.,89.5,26.3));
#41248=CARTESIAN_POINT('',(12.,50.,26.3));
#41249=CARTESIAN_POINT('',(-12.,89.5,26.3));
#41250=CARTESIAN_POINT('',(-6.25,89.5,26.3));
#41251=CARTESIAN_POINT('',(-12.,50.,26.3));
#41252=CARTESIAN_POINT('',(-8.7,62.5,26.3));
#41253=CARTESIAN_POINT('Origin',(-7.5,62.5,26.3));
#41254=CARTESIAN_POINT('',(6.3,62.5,26.3));
#41255=CARTESIAN_POINT('Origin',(7.5,62.5,26.3));
#41256=CARTESIAN_POINT('',(-2.35,85.,26.3));
#41257=CARTESIAN_POINT('Origin',(0.,85.,26.3));
#41258=CARTESIAN_POINT('',(5.15,57.5,26.3));
#41259=CARTESIAN_POINT('Origin',(7.5,57.5,26.3));
#41260=CARTESIAN_POINT('',(-9.85,57.5,26.3));
#41261=CARTESIAN_POINT('Origin',(-7.5,57.5,26.3));
#41262=CARTESIAN_POINT('',(-2.35,55.,26.3));
#41263=CARTESIAN_POINT('Origin',(0.,55.,26.3));
#41264=CARTESIAN_POINT('',(-9.85,82.5,26.3));
#41265=CARTESIAN_POINT('Origin',(-7.5,82.5,26.3));
#41266=CARTESIAN_POINT('',(5.15,82.5,26.3));
#41267=CARTESIAN_POINT('Origin',(7.5,82.5,26.3));
#41268=CARTESIAN_POINT('',(-8.7,77.5,26.3));
#41269=CARTESIAN_POINT('Origin',(-7.5,77.5,26.3));
#41270=CARTESIAN_POINT('Origin',(7.5,77.5,26.3));
#41271=CARTESIAN_POINT('',(6.45,77.5,21.3));
#41272=CARTESIAN_POINT('',(6.45,77.5,26.3));
#41273=CARTESIAN_POINT('Origin',(7.5,77.5,21.3));
#41274=CARTESIAN_POINT('Origin',(-7.5,62.5,26.225));
#41275=CARTESIAN_POINT('',(-8.55,62.5,26.15));
#41276=CARTESIAN_POINT('Origin',(-7.5,62.5,26.15));
#41277=CARTESIAN_POINT('',(-8.625,62.5,26.225));
#41278=CARTESIAN_POINT('Origin',(-7.5,62.5,26.3));
#41279=CARTESIAN_POINT('',(-8.55,62.5,21.3));
#41280=CARTESIAN_POINT('',(-8.55,62.5,26.3));
#41281=CARTESIAN_POINT('Origin',(-7.5,62.5,21.3));
#41282=CARTESIAN_POINT('Origin',(-7.5,77.5,26.225));
#41283=CARTESIAN_POINT('',(-8.55,77.5,26.15));
#41284=CARTESIAN_POINT('Origin',(-7.5,77.5,26.15));
#41285=CARTESIAN_POINT('',(-8.625,77.5,26.225));
#41286=CARTESIAN_POINT('Origin',(-7.5,77.5,26.3));
#41287=CARTESIAN_POINT('',(-8.55,77.5,21.3));
#41288=CARTESIAN_POINT('',(-8.55,77.5,26.3));
#41289=CARTESIAN_POINT('Origin',(-7.5,77.5,21.3));
#41290=CARTESIAN_POINT('Origin',(7.5,62.5,26.225));
#41291=CARTESIAN_POINT('',(6.45,62.5,26.15));
#41292=CARTESIAN_POINT('Origin',(7.5,62.5,26.15));
#41293=CARTESIAN_POINT('',(6.375,62.5,26.225));
#41294=CARTESIAN_POINT('Origin',(7.5,62.5,26.3));
#41295=CARTESIAN_POINT('',(6.45,62.5,21.3));
#41296=CARTESIAN_POINT('',(6.45,62.5,26.3));
#41297=CARTESIAN_POINT('Origin',(7.5,62.5,21.3));
#41298=CARTESIAN_POINT('Origin',(7.5,77.5,20.9845481750105));
#41299=CARTESIAN_POINT('',(7.5,77.5,20.6690963500211));
#41300=CARTESIAN_POINT('',(6.975,77.5,20.9845481750105));
#41301=CARTESIAN_POINT('Origin',(7.5,62.5,20.9845481750105));
#41302=CARTESIAN_POINT('',(7.5,62.5,20.6690963500211));
#41303=CARTESIAN_POINT('',(6.975,62.5,20.9845481750105));
#41304=CARTESIAN_POINT('Origin',(-7.5,77.5,20.9845481750105));
#41305=CARTESIAN_POINT('',(-7.5,77.5,20.6690963500211));
#41306=CARTESIAN_POINT('',(-8.025,77.5,20.9845481750105));
#41307=CARTESIAN_POINT('Origin',(-7.5,62.5,20.9845481750105));
#41308=CARTESIAN_POINT('',(-7.5,62.5,20.6690963500211));
#41309=CARTESIAN_POINT('',(-8.025,62.5,20.9845481750105));
#41310=CARTESIAN_POINT('Origin',(0.,85.,26.15));
#41311=CARTESIAN_POINT('',(-2.05,85.,26.));
#41312=CARTESIAN_POINT('Origin',(0.,85.,26.));
#41313=CARTESIAN_POINT('',(-2.2,85.,26.15));
#41314=CARTESIAN_POINT('Origin',(0.,85.,26.3));
#41315=CARTESIAN_POINT('',(-2.05,85.,21.3));
#41316=CARTESIAN_POINT('',(-2.05,85.,26.3));
#41317=CARTESIAN_POINT('Origin',(0.,85.,21.3));
#41318=CARTESIAN_POINT('Origin',(7.5,82.5,26.15));
#41319=CARTESIAN_POINT('',(5.45,82.5,26.));
#41320=CARTESIAN_POINT('Origin',(7.5,82.5,26.));
#41321=CARTESIAN_POINT('',(5.3,82.5,26.15));
#41322=CARTESIAN_POINT('Origin',(7.5,82.5,26.3));
#41323=CARTESIAN_POINT('',(5.45,82.5,21.3));
#41324=CARTESIAN_POINT('',(5.45,82.5,26.3));
#41325=CARTESIAN_POINT('Origin',(7.5,82.5,21.3));
#41326=CARTESIAN_POINT('Origin',(7.5,57.5,26.15));
#41327=CARTESIAN_POINT('',(5.45,57.5,26.));
#41328=CARTESIAN_POINT('Origin',(7.5,57.5,26.));
#41329=CARTESIAN_POINT('',(5.3,57.5,26.15));
#41330=CARTESIAN_POINT('Origin',(7.5,57.5,26.3));
#41331=CARTESIAN_POINT('',(5.45,57.5,21.3));
#41332=CARTESIAN_POINT('',(5.45,57.5,26.3));
#41333=CARTESIAN_POINT('Origin',(7.5,57.5,21.3));
#41334=CARTESIAN_POINT('Origin',(-7.5,82.5,26.15));
#41335=CARTESIAN_POINT('',(-9.55,82.5,26.));
#41336=CARTESIAN_POINT('Origin',(-7.5,82.5,26.));
#41337=CARTESIAN_POINT('',(-9.7,82.5,26.15));
#41338=CARTESIAN_POINT('Origin',(-7.5,82.5,26.3));
#41339=CARTESIAN_POINT('',(-9.55,82.5,21.3));
#41340=CARTESIAN_POINT('',(-9.55,82.5,26.3));
#41341=CARTESIAN_POINT('Origin',(-7.5,82.5,21.3));
#41342=CARTESIAN_POINT('Origin',(-7.5,57.5,26.15));
#41343=CARTESIAN_POINT('',(-9.55,57.5,26.));
#41344=CARTESIAN_POINT('Origin',(-7.5,57.5,26.));
#41345=CARTESIAN_POINT('',(-9.7,57.5,26.15));
#41346=CARTESIAN_POINT('Origin',(-7.5,57.5,26.3));
#41347=CARTESIAN_POINT('',(-9.55,57.5,21.3));
#41348=CARTESIAN_POINT('',(-9.55,57.5,26.3));
#41349=CARTESIAN_POINT('Origin',(-7.5,57.5,21.3));
#41350=CARTESIAN_POINT('Origin',(0.,55.,26.15));
#41351=CARTESIAN_POINT('',(-2.05,55.,26.));
#41352=CARTESIAN_POINT('Origin',(0.,55.,26.));
#41353=CARTESIAN_POINT('',(-2.2,55.,26.15));
#41354=CARTESIAN_POINT('Origin',(0.,55.,26.3));
#41355=CARTESIAN_POINT('',(-2.05,55.,21.3));
#41356=CARTESIAN_POINT('',(-2.05,55.,26.3));
#41357=CARTESIAN_POINT('Origin',(0.,55.,21.3));
#41358=CARTESIAN_POINT('Origin',(0.,85.,20.6841178654968));
#41359=CARTESIAN_POINT('',(0.,85.,20.0682357309935));
#41360=CARTESIAN_POINT('',(-1.025,85.,20.6841178654968));
#41361=CARTESIAN_POINT('Origin',(0.,55.,20.6841178654968));
#41362=CARTESIAN_POINT('',(0.,55.,20.0682357309935));
#41363=CARTESIAN_POINT('',(-1.025,55.,20.6841178654968));
#41364=CARTESIAN_POINT('Origin',(7.5,82.5,20.6841178654968));
#41365=CARTESIAN_POINT('',(7.5,82.5,20.0682357309935));
#41366=CARTESIAN_POINT('',(6.475,82.5,20.6841178654968));
#41367=CARTESIAN_POINT('Origin',(7.5,57.5,20.6841178654968));
#41368=CARTESIAN_POINT('',(7.5,57.5,20.0682357309935));
#41369=CARTESIAN_POINT('',(6.475,57.5,20.6841178654968));
#41370=CARTESIAN_POINT('Origin',(-7.5,82.5,20.6841178654968));
#41371=CARTESIAN_POINT('',(-7.5,82.5,20.0682357309935));
#41372=CARTESIAN_POINT('',(-8.525,82.5,20.6841178654968));
#41373=CARTESIAN_POINT('Origin',(-7.5,57.5,20.6841178654968));
#41374=CARTESIAN_POINT('',(-7.5,57.5,20.0682357309935));
#41375=CARTESIAN_POINT('',(-8.525,57.5,20.6841178654968));
#41376=CARTESIAN_POINT('Origin',(0.,90.,13.3));
#41377=CARTESIAN_POINT('',(0.936749699759769,77.5,16.15));
#41378=CARTESIAN_POINT('',(0.936749699759769,90.,16.15));
#41379=CARTESIAN_POINT('',(0.936749699759769,90.,16.15));
#41380=CARTESIAN_POINT('',(-0.936749699759769,77.5,16.15));
#41381=CARTESIAN_POINT('Origin',(0.,77.5,13.3));
#41382=CARTESIAN_POINT('',(-0.936749699759769,90.,16.15));
#41383=CARTESIAN_POINT('',(-0.936749699759769,90.,16.15));
#41384=CARTESIAN_POINT('Origin',(0.,90.,13.3));
#41385=CARTESIAN_POINT('Origin',(0.,90.,21.225));
#41386=CARTESIAN_POINT('',(-12.5,90.,16.15));
#41387=CARTESIAN_POINT('',(-12.5,90.,16.15));
#41388=CARTESIAN_POINT('',(-12.5,90.,25.8));
#41389=CARTESIAN_POINT('',(-12.5,90.,26.3));
#41390=CARTESIAN_POINT('',(-6.25,90.,25.8));
#41391=CARTESIAN_POINT('',(-12.5,90.,16.15));
#41392=CARTESIAN_POINT('Origin',(12.5,50.,16.15));
#41393=CARTESIAN_POINT('',(-3.48245602987317,77.5,16.15));
#41394=CARTESIAN_POINT('',(6.25,77.5,16.15));
#41395=CARTESIAN_POINT('',(-7.35566243270259,77.5,16.15));
#41396=CARTESIAN_POINT('',(6.25,77.5,16.15));
#41397=CARTESIAN_POINT('',(-7.35566243270259,62.5,16.15));
#41398=CARTESIAN_POINT('',(-7.35566243270259,56.25,16.15));
#41399=CARTESIAN_POINT('',(-3.48245602987317,62.5,16.15));
#41400=CARTESIAN_POINT('',(6.25,62.5,16.15));
#41401=CARTESIAN_POINT('',(-0.936749699759769,62.5,16.15));
#41402=CARTESIAN_POINT('',(6.25,62.5,16.15));
#41403=CARTESIAN_POINT('',(-0.936749699759769,50.,16.15));
#41404=CARTESIAN_POINT('',(-0.936749699759769,50.,16.15));
#41405=CARTESIAN_POINT('',(-12.5,50.,16.15));
#41406=CARTESIAN_POINT('',(-12.5,50.,16.15));
#41407=CARTESIAN_POINT('',(-12.5,50.,16.15));
#41408=CARTESIAN_POINT('Origin',(0.,50.,13.3));
#41409=CARTESIAN_POINT('',(0.936749699759769,50.,16.15));
#41410=CARTESIAN_POINT('',(0.936749699759769,62.5,16.15));
#41411=CARTESIAN_POINT('',(0.936749699759769,50.,16.15));
#41412=CARTESIAN_POINT('Origin',(0.,50.,13.3));
#41413=CARTESIAN_POINT('Origin',(0.,62.5,13.3));
#41414=CARTESIAN_POINT('Origin',(0.,62.5,13.3));
#41415=CARTESIAN_POINT('',(3.48245602987317,62.5,16.15));
#41416=CARTESIAN_POINT('Origin',(0.,62.5,13.3));
#41417=CARTESIAN_POINT('',(6.25,62.5,16.15));
#41418=CARTESIAN_POINT('Origin',(0.,77.5,13.3));
#41419=CARTESIAN_POINT('',(3.48245602987317,77.5,16.15));
#41420=CARTESIAN_POINT('',(6.25,77.5,16.15));
#41421=CARTESIAN_POINT('Origin',(0.,77.5,13.3));
#41422=CARTESIAN_POINT('Origin',(0.,62.5,13.3));
#41423=CARTESIAN_POINT('',(-4.5,62.5,13.3));
#41424=CARTESIAN_POINT('Origin',(0.,62.5,13.3));
#41425=CARTESIAN_POINT('Origin',(0.,62.5,13.3));
#41426=CARTESIAN_POINT('',(-4.5,77.5,13.3));
#41427=CARTESIAN_POINT('',(-4.5,62.5,13.3));
#41428=CARTESIAN_POINT('Origin',(0.,77.5,13.3));
#41429=CARTESIAN_POINT('Origin',(0.,77.5,13.3));
#41430=CARTESIAN_POINT('Origin',(-6.25,50.25,26.05));
#41431=CARTESIAN_POINT('',(-12.5,50.,25.8));
#41432=CARTESIAN_POINT('',(-12.,50.5,26.3));
#41433=CARTESIAN_POINT('',(-6.25,50.,25.8));
#41434=CARTESIAN_POINT('',(12.5,50.,25.8));
#41435=CARTESIAN_POINT('Origin',(-12.25,50.,26.05));
#41436=CARTESIAN_POINT('',(-12.5,50.,25.8));
#41437=CARTESIAN_POINT('',(-12.,89.5,26.3));
#41438=CARTESIAN_POINT('Origin',(-6.25,89.75,26.05));
#41439=CARTESIAN_POINT('',(12.5,90.,25.8));
#41440=CARTESIAN_POINT('Origin',(12.25,50.,26.05));
#41441=CARTESIAN_POINT('Origin',(0.,50.,21.225));
#41442=CARTESIAN_POINT('',(-12.5,50.,16.15));
#41443=CARTESIAN_POINT('',(-12.5,50.,26.3));
#41444=CARTESIAN_POINT('Origin',(0.,77.5,12.125));
#41445=CARTESIAN_POINT('',(7.35566243270259,77.5,16.15));
#41446=CARTESIAN_POINT('',(6.25,77.5,16.15));
#41447=CARTESIAN_POINT('',(10.2135462651912,77.5,11.2));
#41448=CARTESIAN_POINT('',(10.2135462651912,77.5,11.2));
#41449=CARTESIAN_POINT('',(10.2135462651912,77.5,7.6));
#41450=CARTESIAN_POINT('',(10.2135462651912,77.5,7.6));
#41451=CARTESIAN_POINT('',(-10.2135462651912,77.5,7.6));
#41452=CARTESIAN_POINT('',(-10.2135462651912,77.5,7.6));
#41453=CARTESIAN_POINT('',(-10.2135462651912,77.5,11.2));
#41454=CARTESIAN_POINT('',(-10.2135462651912,77.5,11.2));
#41455=CARTESIAN_POINT('',(-7.35566243270259,77.5,16.15));
#41456=CARTESIAN_POINT('Origin',(-10.2135462651912,62.5,11.2));
#41457=CARTESIAN_POINT('',(-10.2135462651912,62.5,11.2));
#41458=CARTESIAN_POINT('',(-7.35566243270259,62.5,16.15));
#41459=CARTESIAN_POINT('',(-10.2135462651912,62.5,11.2));
#41460=CARTESIAN_POINT('Origin',(-10.2135462651912,62.5,7.6));
#41461=CARTESIAN_POINT('',(-10.2135462651912,62.5,7.6));
#41462=CARTESIAN_POINT('',(-10.2135462651912,62.5,11.2));
#41463=CARTESIAN_POINT('',(-10.2135462651912,62.5,7.6));
#41464=CARTESIAN_POINT('Origin',(10.2135462651912,62.5,7.6));
#41465=CARTESIAN_POINT('',(10.2135462651912,62.5,7.6));
#41466=CARTESIAN_POINT('',(-10.2135462651912,62.5,7.6));
#41467=CARTESIAN_POINT('',(10.2135462651912,62.5,7.6));
#41468=CARTESIAN_POINT('Origin',(10.2135462651912,62.5,11.2));
#41469=CARTESIAN_POINT('',(10.2135462651912,62.5,11.2));
#41470=CARTESIAN_POINT('',(10.2135462651912,62.5,7.6));
#41471=CARTESIAN_POINT('',(10.2135462651912,62.5,11.2));
#41472=CARTESIAN_POINT('Origin',(7.35566243270259,62.5,16.15));
#41473=CARTESIAN_POINT('',(7.35566243270259,62.5,16.15));
#41474=CARTESIAN_POINT('',(10.2135462651912,62.5,11.2));
#41475=CARTESIAN_POINT('',(7.35566243270259,56.25,16.15));
#41476=CARTESIAN_POINT('Origin',(0.,62.5,12.125));
#41477=CARTESIAN_POINT('',(6.25,62.5,16.15));
#41478=CARTESIAN_POINT('Origin',(-12.5,50.,16.15));
#41479=CARTESIAN_POINT('Origin',(12.5,50.,16.15));
#41480=CARTESIAN_POINT('',(0.,0.,0.));
#41481=CARTESIAN_POINT('Origin',(0.,77.35,13.3));
#41482=CARTESIAN_POINT('',(-2.525,77.2,13.3));
#41483=CARTESIAN_POINT('',(2.52500000000001,77.2,13.3));
#41484=CARTESIAN_POINT('Origin',(0.,77.2,13.3));
#41485=CARTESIAN_POINT('',(2.825,77.5,13.3));
#41486=CARTESIAN_POINT('',(2.675,77.35,13.3));
#41487=CARTESIAN_POINT('Origin',(0.,77.5,13.3));
#41488=CARTESIAN_POINT('Origin',(0.,77.2,13.3));
#41489=CARTESIAN_POINT('Origin',(0.,70.,13.3));
#41490=CARTESIAN_POINT('',(-2.525,62.8,13.3));
#41491=CARTESIAN_POINT('',(-2.525,70.,13.3));
#41492=CARTESIAN_POINT('',(2.525,62.8,13.3));
#41493=CARTESIAN_POINT('Origin',(0.,62.8,13.3));
#41494=CARTESIAN_POINT('Origin',(0.,62.8,13.3));
#41495=CARTESIAN_POINT('Origin',(4.2,77.5,13.3));
#41496=CARTESIAN_POINT('',(-4.2,77.5,13.3));
#41497=CARTESIAN_POINT('Origin',(0.,77.5,13.3));
#41498=CARTESIAN_POINT('Origin',(0.,62.65,13.3));
#41499=CARTESIAN_POINT('',(2.825,62.5,13.3));
#41500=CARTESIAN_POINT('',(2.675,62.65,13.3));
#41501=CARTESIAN_POINT('Origin',(0.,62.5,13.3));
#41502=CARTESIAN_POINT('Origin',(2.525,62.5,13.3));
#41503=CARTESIAN_POINT('',(-4.2,62.5,13.3));
#41504=CARTESIAN_POINT('Origin',(0.,62.5,13.3));
#41505=CARTESIAN_POINT('Origin',(0.,77.35,13.3));
#41506=CARTESIAN_POINT('',(-4.5,77.2,13.3));
#41507=CARTESIAN_POINT('Origin',(0.,77.2,13.3));
#41508=CARTESIAN_POINT('',(-4.35,77.35,13.3));
#41509=CARTESIAN_POINT('Origin',(0.,70.,13.3));
#41510=CARTESIAN_POINT('',(-4.5,62.8,13.3));
#41511=CARTESIAN_POINT('Origin',(0.,62.8,13.3));
#41512=CARTESIAN_POINT('',(-4.5,70.,13.3));
#41513=CARTESIAN_POINT('Origin',(0.,62.65,13.3));
#41514=CARTESIAN_POINT('',(-4.35,62.65,13.3));
#41515=CARTESIAN_POINT('',(0.,0.,0.));
#41516=CARTESIAN_POINT('Origin',(0.,70.2,13.3));
#41517=CARTESIAN_POINT('',(-2.49999999985264,117.652418880134,13.2999728563934));
#41518=CARTESIAN_POINT('',(-2.5,120.,13.3));
#41519=CARTESIAN_POINT('',(-2.5,70.2,13.3));
#41520=CARTESIAN_POINT('Origin',(0.,120.,13.3));
#41521=CARTESIAN_POINT('',(2.31548671935009,116.940942573699,14.2367878010894));
#41522=CARTESIAN_POINT('Ctrl Pts',(-2.5,117.652415863143,13.2999999999964));
#41523=CARTESIAN_POINT('Ctrl Pts',(-2.50000000000024,117.633767919634,13.4677740226832));
#41524=CARTESIAN_POINT('Ctrl Pts',(-2.48311159749416,117.615475457,13.6351341300433));
#41525=CARTESIAN_POINT('Ctrl Pts',(-2.41467031439132,117.578040264004,13.970738634694));
#41526=CARTESIAN_POINT('Ctrl Pts',(-2.36192374370731,117.558925190662,14.1377499846458));
#41527=CARTESIAN_POINT('Ctrl Pts',(-2.15914690247099,117.50166870114,14.6035341083317));
#41528=CARTESIAN_POINT('Ctrl Pts',(-1.96622718300721,117.463802365995,14.8796290223583));
#41529=CARTESIAN_POINT('Ctrl Pts',(-1.49981270374707,117.394137936618,15.3241315427021));
#41530=CARTESIAN_POINT('Ctrl Pts',(-1.23689840087897,117.362604344116,15.4946851089548));
#41531=CARTESIAN_POINT('Ctrl Pts',(-0.797897943810747,117.311924098983,
15.6749091698224));
#41532=CARTESIAN_POINT('Ctrl Pts',(-0.640607813401521,117.294176141788,
15.7220777314919));
#41533=CARTESIAN_POINT('Ctrl Pts',(-0.192100260886219,117.245478021646,
15.8097910077299));
#41534=CARTESIAN_POINT('Ctrl Pts',(0.103385439683299,117.215867900195,15.8150373826655));
#41535=CARTESIAN_POINT('Ctrl Pts',(0.547510877878541,117.172003103533,15.7443114965582));
#41536=CARTESIAN_POINT('Ctrl Pts',(0.699199333265182,117.157044512303,15.7053151288251));
#41537=CARTESIAN_POINT('Ctrl Pts',(1.1602968287484,117.108884869839,15.5394426026382));
#41538=CARTESIAN_POINT('Ctrl Pts',(1.44852396879158,117.073855997147,15.3647510728443));
#41539=CARTESIAN_POINT('Ctrl Pts',(1.83412146311951,117.023015998026,15.0094727975578));
#41540=CARTESIAN_POINT('Ctrl Pts',(1.95905169782132,117.005486607079,14.8647559879435));
#41541=CARTESIAN_POINT('Ctrl Pts',(2.16656823945866,116.972514041558,14.5600305887085));
#41542=CARTESIAN_POINT('Ctrl Pts',(2.2507575437618,116.957083588901,14.4026200111203));
#41543=CARTESIAN_POINT('Ctrl Pts',(2.31751248124682,116.940955446993,14.2376224716085));
#41544=CARTESIAN_POINT('',(-2.50000780325734,115.753171725698,13.2992871105637));
#41545=CARTESIAN_POINT('Ctrl Pts',(2.31558471872693,116.940912503669,14.2365676273829));
#41546=CARTESIAN_POINT('Ctrl Pts',(2.31659029782528,116.940603919617,14.2343081169145));
#41547=CARTESIAN_POINT('Ctrl Pts',(2.31755492533272,116.940306937475,14.2321321519896));
#41548=CARTESIAN_POINT('Ctrl Pts',(2.31856222833977,116.939995783467,14.2298508630467));
#41549=CARTESIAN_POINT('Ctrl Pts',(2.32625422732343,116.937619739418,14.2124304124893));
#41550=CARTESIAN_POINT('Ctrl Pts',(2.33371980469038,116.935252897235,14.1949902343915));
#41551=CARTESIAN_POINT('Ctrl Pts',(2.34047657787375,116.932574974244,14.1772308598749));
#41552=CARTESIAN_POINT('Ctrl Pts',(2.3410009256349,116.932367158637,14.175852674162));
#41553=CARTESIAN_POINT('Ctrl Pts',(2.34152098933304,116.932157472739,14.1744725868393));
#41554=CARTESIAN_POINT('Ctrl Pts',(2.34203653579483,116.931945768446,14.1730904684601));
#41555=CARTESIAN_POINT('Ctrl Pts',(2.35633192712406,116.926075500808,14.1347662347449));
#41556=CARTESIAN_POINT('Ctrl Pts',(2.36967758476892,116.920203373036,14.096091830941));
#41557=CARTESIAN_POINT('Ctrl Pts',(2.38206951868707,116.914333784119,14.0571084522397));
#41558=CARTESIAN_POINT('Ctrl Pts',(2.40895222770159,116.901600464852,13.9725390191753));
#41559=CARTESIAN_POINT('Ctrl Pts',(2.43130345019459,116.888898275388,13.8866537464038));
#41560=CARTESIAN_POINT('Ctrl Pts',(2.44903453897375,116.876229637983,13.7998201531797));
#41561=CARTESIAN_POINT('Ctrl Pts',(2.45662057711109,116.870809510223,13.7626694199108));
#41562=CARTESIAN_POINT('Ctrl Pts',(2.46336092360456,116.8653957767,13.7253447121415));
#41563=CARTESIAN_POINT('Ctrl Pts',(2.46924841009455,116.859989647685,13.6878728787018));
#41564=CARTESIAN_POINT('Ctrl Pts',(2.46926386831748,116.859975453317,13.6877744924115));
#41565=CARTESIAN_POINT('Ctrl Pts',(2.46927932066003,116.859961259002,13.6876761051061));
#41566=CARTESIAN_POINT('Ctrl Pts',(2.46929476712233,116.859947064739,13.6875777167863));
#41567=CARTESIAN_POINT('Ctrl Pts',(2.47479064415234,116.854896722356,13.6525709886025));
#41568=CARTESIAN_POINT('Ctrl Pts',(2.47954223469556,116.849852988345,13.6174357226674));
#41569=CARTESIAN_POINT('Ctrl Pts',(2.48354560772627,116.844812250552,13.5821956513399));
#41570=CARTESIAN_POINT('Ctrl Pts',(2.49342863155305,116.83236831107,13.4951993954539));
#41571=CARTESIAN_POINT('Ctrl Pts',(2.49871470380525,116.819988043894,13.4078942964491));
#41572=CARTESIAN_POINT('Ctrl Pts',(2.49944034464196,116.807632739007,13.3206537489573));
#41573=CARTESIAN_POINT('Ctrl Pts',(2.50017539447477,116.795117229498,13.2322820000103));
#41574=CARTESIAN_POINT('Ctrl Pts',(2.49623080101212,116.782627493706,13.1439770724103));
#41575=CARTESIAN_POINT('Ctrl Pts',(2.48763810528317,116.770145896355,13.0561199186723));
#41576=CARTESIAN_POINT('Ctrl Pts',(2.47905530371016,116.75767867108,12.9683639290402));
#41577=CARTESIAN_POINT('Ctrl Pts',(2.46583555096674,116.745219851162,12.881055195064));
#41578=CARTESIAN_POINT('Ctrl Pts',(2.44800189138904,116.732770812033,12.7945577675241));
#41579=CARTESIAN_POINT('Ctrl Pts',(2.43642053850014,116.724686284309,12.738385492397));
#41580=CARTESIAN_POINT('Ctrl Pts',(2.42289321852048,116.7166062611,12.6825550060511));
#41581=CARTESIAN_POINT('Ctrl Pts',(2.40742217001043,116.708534470064,12.6271612767138));
#41582=CARTESIAN_POINT('Ctrl Pts',(2.40317285018602,116.706317450212,12.6119466859207));
#41583=CARTESIAN_POINT('Ctrl Pts',(2.39878073164306,116.704103078828,12.5967788316271));
#41584=CARTESIAN_POINT('Ctrl Pts',(2.39424657911186,116.701891450801,12.5816593997127));
#41585=CARTESIAN_POINT('Ctrl Pts',(2.39422205165848,116.701879487021,12.5815776112949));
#41586=CARTESIAN_POINT('Ctrl Pts',(2.39419752004866,116.701867523321,12.581495824294));
#41587=CARTESIAN_POINT('Ctrl Pts',(2.3941729842827,116.701855559702,12.5814140387102));
#41588=CARTESIAN_POINT('Ctrl Pts',(2.36913525351378,116.689647182624,12.4979552450586));
#41589=CARTESIAN_POINT('Ctrl Pts',(2.33976991854307,116.677520410264,12.4159705665369));
#41590=CARTESIAN_POINT('Ctrl Pts',(2.30624651142751,116.66542454348,12.3357854461982));
#41591=CARTESIAN_POINT('Ctrl Pts',(2.27221433430887,116.653145103045,12.2543833915609));
#41592=CARTESIAN_POINT('Ctrl Pts',(2.23389660514796,116.640897607304,12.1748367615522));
#41593=CARTESIAN_POINT('Ctrl Pts',(2.19146914410303,116.628652174829,12.0974947553472));
#41594=CARTESIAN_POINT('Ctrl Pts',(2.14893240047266,116.616375201165,12.0199535353737));
#41595=CARTESIAN_POINT('Ctrl Pts',(2.10226509706415,116.60410053041,11.9446289849932));
#41596=CARTESIAN_POINT('Ctrl Pts',(2.0516424135292,116.591818631987,11.8718700282806));
#41597=CARTESIAN_POINT('Ctrl Pts',(2.02733790787834,116.585921957832,11.836937655062));
#41598=CARTESIAN_POINT('Ctrl Pts',(2.00212159864347,116.580023900124,11.8025965566306));
#41599=CARTESIAN_POINT('Ctrl Pts',(1.97601207576289,116.574124817132,11.7688845677729));
#41600=CARTESIAN_POINT('Ctrl Pts',(1.93528800816622,116.564923781341,11.7163026297826));
#41601=CARTESIAN_POINT('Ctrl Pts',(1.89254740546535,116.555755273503,11.6654526254126));
#41602=CARTESIAN_POINT('Ctrl Pts',(1.84790062309802,116.546623642951,11.6164344471128));
#41603=CARTESIAN_POINT('Ctrl Pts',(1.84785790318654,116.546614905425,11.6163875444666));
#41604=CARTESIAN_POINT('Ctrl Pts',(1.84781518152816,116.546606167932,11.6163406434974));
#41605=CARTESIAN_POINT('Ctrl Pts',(1.84777245812297,116.546597430472,11.6162937442053));
#41606=CARTESIAN_POINT('Ctrl Pts',(1.78880671836136,116.534538214999,11.5515645531837));
#41607=CARTESIAN_POINT('Ctrl Pts',(1.72651412330931,116.522542000416,11.4900271582674));
#41608=CARTESIAN_POINT('Ctrl Pts',(1.66117508174235,116.510564512528,11.4319174966237));
#41609=CARTESIAN_POINT('Ctrl Pts',(1.59497422136402,116.498429042151,11.3730413713416));
#41610=CARTESIAN_POINT('Ctrl Pts',(1.52564613907004,116.48631290844,11.3176849042504));
#41611=CARTESIAN_POINT('Ctrl Pts',(1.45348844373583,116.474190351703,11.2661036490813));
#41612=CARTESIAN_POINT('Ctrl Pts',(1.38834739291626,116.463246597461,11.2195381767676));
#41613=CARTESIAN_POINT('Ctrl Pts',(1.3209007494497,116.452297992488,11.1760497257851));
#41614=CARTESIAN_POINT('Ctrl Pts',(1.2513674883898,116.441337882707,11.1358262063494));
#41615=CARTESIAN_POINT('Ctrl Pts',(1.17929482046512,116.429977501493,11.0941336938041));
#41616=CARTESIAN_POINT('Ctrl Pts',(1.10532794360825,116.418659279662,11.0561498523986));
#41617=CARTESIAN_POINT('Ctrl Pts',(1.02975113129391,116.407385635209,11.0219720448883));
#41618=CARTESIAN_POINT('Ctrl Pts',(1.02486966711646,116.406657476798,11.0197645193534));
#41619=CARTESIAN_POINT('Ctrl Pts',(1.01998147000137,116.405929503522,11.0175728786915));
#41620=CARTESIAN_POINT('Ctrl Pts',(1.01508660977429,116.405201715687,11.0153971521677));
#41621=CARTESIAN_POINT('Ctrl Pts',(0.989532427173145,116.401402215322,11.0040385208075));
#41622=CARTESIAN_POINT('Ctrl Pts',(0.963796808589488,116.39760786875,10.9931133169629));
#41623=CARTESIAN_POINT('Ctrl Pts',(0.937889563447039,116.393818941974,10.9826251250953));
#41624=CARTESIAN_POINT('Ctrl Pts',(0.937876528580895,116.393817035628,10.982619848109));
#41625=CARTESIAN_POINT('Ctrl Pts',(0.937863493671292,116.393815129285,10.9826145712334));
#41626=CARTESIAN_POINT('Ctrl Pts',(0.937850458718229,116.393813222942,10.9826092944684));
#41627=CARTESIAN_POINT('Ctrl Pts',(0.856558251270879,116.38192435854,10.9497008617622));
#41628=CARTESIAN_POINT('Ctrl Pts',(0.773574022102526,116.370087314127,10.9210938611651));
#41629=CARTESIAN_POINT('Ctrl Pts',(0.689246936165983,116.358259657402,10.8969044369372));
#41630=CARTESIAN_POINT('Ctrl Pts',(0.604144768993149,116.346323288338,10.8724926788217));
#41631=CARTESIAN_POINT('Ctrl Pts',(0.517675482596711,116.334396606344,10.8525809850961));
#41632=CARTESIAN_POINT('Ctrl Pts',(0.430216206818991,116.322454369358,10.8372950323008));
#41633=CARTESIAN_POINT('Ctrl Pts',(0.400085229039446,116.31834009704,10.8320288018191));
#41634=CARTESIAN_POINT('Ctrl Pts',(0.369836865368955,116.314224127933,10.827311598678));
#41635=CARTESIAN_POINT('Ctrl Pts',(0.339486805344473,116.310105876929,10.8231485103331));
#41636=CARTESIAN_POINT('Ctrl Pts',(0.251592673824735,116.298179373486,10.8110921574225));
#41637=CARTESIAN_POINT('Ctrl Pts',(0.163299503256435,116.286294065945,10.8037453205576));
#41638=CARTESIAN_POINT('Ctrl Pts',(0.0749915624963321,116.274444109565,
10.801084345815));
#41639=CARTESIAN_POINT('Ctrl Pts',(-0.00218809746395864,116.264087446324,
10.7987586984946));
#41640=CARTESIAN_POINT('Ctrl Pts',(-0.0793792441935915,116.253758137179,
10.8000117096716));
#41641=CARTESIAN_POINT('Ctrl Pts',(-0.156350655397556,116.243457913992,
10.8048298747349));
#41642=CARTESIAN_POINT('Ctrl Pts',(-0.156400196120542,116.243451284512,
10.8048329758262));
#41643=CARTESIAN_POINT('Ctrl Pts',(-0.156449736753255,116.243444655042,
10.804836078396));
#41644=CARTESIAN_POINT('Ctrl Pts',(-0.156499277295674,116.243438025585,
10.8048391824442));
#41645=CARTESIAN_POINT('Ctrl Pts',(-0.24456415739787,116.231653286752,10.8103570394452));
#41646=CARTESIAN_POINT('Ctrl Pts',(-0.332346265444591,116.219905715678,
10.820542262043));
#41647=CARTESIAN_POINT('Ctrl Pts',(-0.419477796327602,116.20816041902,10.8353707649117));
#41648=CARTESIAN_POINT('Ctrl Pts',(-0.488449146412123,116.198863107709,
10.847108672558));
#41649=CARTESIAN_POINT('Ctrl Pts',(-0.557012073175496,116.189567578866,
10.8617562465931));
#41650=CARTESIAN_POINT('Ctrl Pts',(-0.624975132408264,116.180262954861,
10.8793013943141));
#41651=CARTESIAN_POINT('Ctrl Pts',(-0.65193249278898,116.176572301359,10.8862606288657));
#41652=CARTESIAN_POINT('Ctrl Pts',(-0.678751888420746,116.172886231536,
10.8936644806514));
#41653=CARTESIAN_POINT('Ctrl Pts',(-0.705422444723274,116.169204265486,
10.9015078227887));
#41654=CARTESIAN_POINT('Ctrl Pts',(-0.705495663032793,116.169194157435,
10.9015293550075));
#41655=CARTESIAN_POINT('Ctrl Pts',(-0.705568880219835,116.169184049415,
10.9015508905417));
#41656=CARTESIAN_POINT('Ctrl Pts',(-0.705642096283931,116.169173941425,
10.9015724293912));
#41657=CARTESIAN_POINT('Ctrl Pts',(-0.790078629159663,116.157516887221,
10.926412139052));
#41658=CARTESIAN_POINT('Ctrl Pts',(-0.873021144427934,116.145900151257,
10.9556566826382));
#41659=CARTESIAN_POINT('Ctrl Pts',(-0.954125624468592,116.134312207952,
10.989140873903));
#41660=CARTESIAN_POINT('Ctrl Pts',(-1.03160398465552,116.123242352812,11.0211280123456));
#41661=CARTESIAN_POINT('Ctrl Pts',(-1.10740468305274,116.112199021028,11.0569836383265));
#41662=CARTESIAN_POINT('Ctrl Pts',(-1.18125236023816,116.101179283222,11.0965733416553));
#41663=CARTESIAN_POINT('Ctrl Pts',(-1.1854452336852,116.100553612005,11.0988211390429));
#41664=CARTESIAN_POINT('Ctrl Pts',(-1.18963181315389,116.099928016101,11.1010809876576));
#41665=CARTESIAN_POINT('Ctrl Pts',(-1.19381204878256,116.099302494702,11.1033528679144));
#41666=CARTESIAN_POINT('Ctrl Pts',(-1.20234052067155,116.098026312654,11.1079879336443));
#41667=CARTESIAN_POINT('Ctrl Pts',(-1.21084260999004,116.096750449632,11.1126730392948));
#41668=CARTESIAN_POINT('Ctrl Pts',(-1.21931791193801,116.095474904488,11.1174079983053));
#41669=CARTESIAN_POINT('Ctrl Pts',(-1.21941892058687,116.095459702541,11.1174644295469));
#41670=CARTESIAN_POINT('Ctrl Pts',(-1.21951992542756,116.095444500638,11.1175208678753));
#41671=CARTESIAN_POINT('Ctrl Pts',(-1.21962092645903,116.095429298779,11.1175773132903));
#41672=CARTESIAN_POINT('Ctrl Pts',(-1.29230581112784,116.084489357145,11.1581979725452));
#41673=CARTESIAN_POINT('Ctrl Pts',(-1.36302191930873,116.073571818357,11.2024869421495));
#41674=CARTESIAN_POINT('Ctrl Pts',(-1.43148894550428,116.062648657739,11.2503077186718));
#41675=CARTESIAN_POINT('Ctrl Pts',(-1.43561009700005,116.061991173367,11.2531861358552));
#41676=CARTESIAN_POINT('Ctrl Pts',(-1.43972308545627,116.061333669725,11.2560773547882));
#41677=CARTESIAN_POINT('Ctrl Pts',(-1.44382784410453,116.060676141123,11.2589813477688));
#41678=CARTESIAN_POINT('Ctrl Pts',(-1.46186642054003,116.057786597312,11.2717430967139));
#41679=CARTESIAN_POINT('Ctrl Pts',(-1.4797462227181,116.054896613924,11.2847513374824));
#41680=CARTESIAN_POINT('Ctrl Pts',(-1.49746176129706,116.052005801828,11.2980033881251));
#41681=CARTESIAN_POINT('Ctrl Pts',(-1.56781347313938,116.040525847175,11.3506297558742));
#41682=CARTESIAN_POINT('Ctrl Pts',(-1.63521555084676,116.029090470488,11.4068327759038));
#41683=CARTESIAN_POINT('Ctrl Pts',(-1.69941062671312,116.017681713284,11.4663298991271));
#41684=CARTESIAN_POINT('Ctrl Pts',(-1.76448188855156,116.006117240194,11.5266390868903));
#41685=CARTESIAN_POINT('Ctrl Pts',(-1.82625756826401,115.994580378614,11.5903320231517));
#41686=CARTESIAN_POINT('Ctrl Pts',(-1.88448516423124,115.983060855372,11.6571244196917));
#41687=CARTESIAN_POINT('Ctrl Pts',(-1.94054639750562,115.971969916979,11.7214317994002));
#41688=CARTESIAN_POINT('Ctrl Pts',(-1.99331901776561,115.960895321955,11.7886113724769));
#41689=CARTESIAN_POINT('Ctrl Pts',(-2.04259213004864,115.949831653556,11.858432055086));
#41690=CARTESIAN_POINT('Ctrl Pts',(-2.04268247864119,115.949811366897,11.8585600802931));
#41691=CARTESIAN_POINT('Ctrl Pts',(-2.04277281546547,115.949791080273,11.8586881143922));
#41692=CARTESIAN_POINT('Ctrl Pts',(-2.04286314051931,115.949770793686,11.8588161573824));
#41693=CARTESIAN_POINT('Ctrl Pts',(-2.07925508584214,115.941597331938,11.9104046513913));
#41694=CARTESIAN_POINT('Ctrl Pts',(-2.11373782549542,115.933429652993,11.9634365047525));
#41695=CARTESIAN_POINT('Ctrl Pts',(-2.14621742886547,115.92525735781,12.017807968242));
#41696=CARTESIAN_POINT('Ctrl Pts',(-2.19103295219095,115.913981183,12.0928299924489));
#41697=CARTESIAN_POINT('Ctrl Pts',(-2.23180572449633,115.902753224868,12.1700199717333));
#41698=CARTESIAN_POINT('Ctrl Pts',(-2.26840497157125,115.891554051651,12.2490219104932));
#41699=CARTESIAN_POINT('Ctrl Pts',(-2.28335615916443,115.886979068474,12.2812950554627));
#41700=CARTESIAN_POINT('Ctrl Pts',(-2.29761095150448,115.882408989736,12.3138705897435));
#41701=CARTESIAN_POINT('Ctrl Pts',(-2.3111608945923,115.877842846099,12.3467244888677));
#41702=CARTESIAN_POINT('Ctrl Pts',(-2.31122345482284,115.877821764166,12.3468761756674));
#41703=CARTESIAN_POINT('Ctrl Pts',(-2.31128600001604,115.877800682315,12.3470278684067));
#41704=CARTESIAN_POINT('Ctrl Pts',(-2.31134853017173,115.877779600547,12.3471795670829));
#41705=CARTESIAN_POINT('Ctrl Pts',(-2.34169064308544,115.86754989006,12.4207897846128));
#41706=CARTESIAN_POINT('Ctrl Pts',(-2.36849361581318,115.857339984831,12.4957938787982));
#41707=CARTESIAN_POINT('Ctrl Pts',(-2.39167540751614,115.847146677697,12.5719549633683));
#41708=CARTESIAN_POINT('Ctrl Pts',(-2.39554800156618,115.845443852434,12.5846779214006));
#41709=CARTESIAN_POINT('Ctrl Pts',(-2.39931949254203,115.843741481025,12.5974332747695));
#41710=CARTESIAN_POINT('Ctrl Pts',(-2.40298943501363,115.842039537261,12.6102200465974));
#41711=CARTESIAN_POINT('Ctrl Pts',(-2.40303577089737,115.842018048894,12.6103814895566));
#41712=CARTESIAN_POINT('Ctrl Pts',(-2.40308209060529,115.841996560598,12.6105429375206));
#41713=CARTESIAN_POINT('Ctrl Pts',(-2.40312839413032,115.841975072369,12.610704390489));
#41714=CARTESIAN_POINT('Ctrl Pts',(-2.41590288462029,115.836046772837,12.6552469908212));
#41715=CARTESIAN_POINT('Ctrl Pts',(-2.42744647790313,115.830123446056,12.7001724516602));
#41716=CARTESIAN_POINT('Ctrl Pts',(-2.43773795250823,115.824192790862,12.7454148170031));
#41717=CARTESIAN_POINT('Ctrl Pts',(-2.43777476533889,115.824171576778,12.7455766499374));
#41718=CARTESIAN_POINT('Ctrl Pts',(-2.43781156212925,115.824150362603,12.7457384869042));
#41719=CARTESIAN_POINT('Ctrl Pts',(-2.43784834289122,115.824129148337,12.7459003278972));
#41720=CARTESIAN_POINT('Ctrl Pts',(-2.44811410441784,115.818208102025,12.7910712528639));
#41721=CARTESIAN_POINT('Ctrl Pts',(-2.45713095097772,115.8122803864,12.8365526619577));
#41722=CARTESIAN_POINT('Ctrl Pts',(-2.46488253727775,115.806358415083,12.8823025199197));
#41723=CARTESIAN_POINT('Ctrl Pts',(-2.46491177598373,115.80633607762,12.8824750867459));
#41724=CARTESIAN_POINT('Ctrl Pts',(-2.46494099670432,115.806313740233,12.8826476574335));
#41725=CARTESIAN_POINT('Ctrl Pts',(-2.46497019942748,115.806291402924,12.8828202319817));
#41726=CARTESIAN_POINT('Ctrl Pts',(-2.46774729796264,115.804167186348,12.8992315961665));
#41727=CARTESIAN_POINT('Ctrl Pts',(-2.47036163655441,115.802043666934,12.9156778827472));
#41728=CARTESIAN_POINT('Ctrl Pts',(-2.47281230648096,115.799920717301,12.9321560233193));
#41729=CARTESIAN_POINT('Ctrl Pts',(-2.48403796215045,115.790196232858,13.0076365807501));
#41730=CARTESIAN_POINT('Ctrl Pts',(-2.49178559071337,115.780521771062,13.0834875586044));
#41731=CARTESIAN_POINT('Ctrl Pts',(-2.49606163842758,115.770873778594,13.1594975034073));
#41732=CARTESIAN_POINT('Ctrl Pts',(-2.49665765041311,115.769529004276,13.170092062016));
#41733=CARTESIAN_POINT('Ctrl Pts',(-2.49718615364143,115.768184753474,13.180689656827));
#41734=CARTESIAN_POINT('Ctrl Pts',(-2.49764710684871,115.76684097141,13.1912896626918));
#41735=CARTESIAN_POINT('Ctrl Pts',(-2.49921172934089,115.762279745649,13.2272694700374));
#41736=CARTESIAN_POINT('Ctrl Pts',(-2.49999871575296,115.757723936595,13.2632771489192));
#41737=CARTESIAN_POINT('Ctrl Pts',(-2.50000780325734,115.753171725698,13.2992871105637));
#41738=CARTESIAN_POINT('',(-2.5,116.590949403176,13.3));
#41739=CARTESIAN_POINT('',(-2.5,70.2,13.3));
#41740=CARTESIAN_POINT('',(-0.113189986264273,116.915604014531,10.8025547582574));
#41741=CARTESIAN_POINT('Ctrl Pts',(-2.5,116.590949403176,13.3));
#41742=CARTESIAN_POINT('Ctrl Pts',(-2.5,116.620953768662,12.9872092797494));
#41743=CARTESIAN_POINT('Ctrl Pts',(-2.44132738978406,116.653364211068,12.6770829675089));
#41744=CARTESIAN_POINT('Ctrl Pts',(-2.22541193652053,116.708445952147,12.1276873243219));
#41745=CARTESIAN_POINT('Ctrl Pts',(-2.08195957546983,116.731312087827,11.8885330538203));
#41746=CARTESIAN_POINT('Ctrl Pts',(-1.68507892689696,116.782726034039,11.4231982379589));
#41747=CARTESIAN_POINT('Ctrl Pts',(-1.41928106560156,116.814133195958,11.2149293621363));
#41748=CARTESIAN_POINT('Ctrl Pts',(-0.953296569348058,116.856517921123,
10.981356754033));
#41749=CARTESIAN_POINT('Ctrl Pts',(-0.77746724983857,116.870233032691,10.9166232730901));
#41750=CARTESIAN_POINT('Ctrl Pts',(-0.43764187396164,116.89413879085,10.8332135767708));
#41751=CARTESIAN_POINT('Ctrl Pts',(-0.275985400295147,116.9045269682,10.8099444629497));
#41752=CARTESIAN_POINT('Ctrl Pts',(-0.113227701620156,116.915647816343,
10.8025654187575));
#41753=CARTESIAN_POINT('',(2.37817680705653,117.418248384963,12.5291084093352));
#41754=CARTESIAN_POINT('Ctrl Pts',(-0.11318991391854,116.91570063764,10.8025637058401));
#41755=CARTESIAN_POINT('Ctrl Pts',(-0.0267483415987858,116.929017161337,
10.7986459626117));
#41756=CARTESIAN_POINT('Ctrl Pts',(0.0596926633871199,116.942504266172,
10.7992268895155));
#41757=CARTESIAN_POINT('Ctrl Pts',(0.145739837161053,116.956081811018,10.8042516353077));
#41758=CARTESIAN_POINT('Ctrl Pts',(0.231953820853551,116.969685677113,10.809286122006));
#41759=CARTESIAN_POINT('Ctrl Pts',(0.317771656242895,116.983380328598,10.8187801658181));
#41760=CARTESIAN_POINT('Ctrl Pts',(0.402846612778607,116.997089241994,10.8326705516748));
#41761=CARTESIAN_POINT('Ctrl Pts',(0.486360317026859,117.010546576391,10.8463060282423));
#41762=CARTESIAN_POINT('Ctrl Pts',(0.569158212026128,117.024017660618,10.8641761280544));
#41763=CARTESIAN_POINT('Ctrl Pts',(0.650964467559707,117.037434010971,10.8862383585004));
#41764=CARTESIAN_POINT('Ctrl Pts',(0.721054977793133,117.048928961273,10.9051409837185));
#41765=CARTESIAN_POINT('Ctrl Pts',(0.790418663365023,117.06038379259,10.9271204666373));
#41766=CARTESIAN_POINT('Ctrl Pts',(0.858910376226253,117.071757742589,10.9521769731066));
#41767=CARTESIAN_POINT('Ctrl Pts',(0.861120381724083,117.072124743077,10.9529854653276));
#41768=CARTESIAN_POINT('Ctrl Pts',(0.863329073610727,117.072491648114,10.9537970150146));
#41769=CARTESIAN_POINT('Ctrl Pts',(0.86553645088459,117.072858459449,10.954611620181));
#41770=CARTESIAN_POINT('Ctrl Pts',(0.935076433748151,117.084414279223,10.9802744871416));
#41771=CARTESIAN_POINT('Ctrl Pts',(1.00331537275581,117.095877243229,11.0089698285396));
#41772=CARTESIAN_POINT('Ctrl Pts',(1.07010181240248,117.10730088397,11.0406013828691));
#41773=CARTESIAN_POINT('Ctrl Pts',(1.13672507294348,117.118696613364,11.0721556519178));
#41774=CARTESIAN_POINT('Ctrl Pts',(1.20190196549986,117.130053212562,11.1066325777123));
#41775=CARTESIAN_POINT('Ctrl Pts',(1.26544711283963,117.141422144751,11.1439286643049));
#41776=CARTESIAN_POINT('Ctrl Pts',(1.32922572009029,117.152832845509,11.1813617738084));
#41777=CARTESIAN_POINT('Ctrl Pts',(1.39135968082058,117.16425597846,11.221635184068));
#41778=CARTESIAN_POINT('Ctrl Pts',(1.45164008493825,117.175741809776,11.2646275368374));
#41779=CARTESIAN_POINT('Ctrl Pts',(1.51192048905591,117.187227641092,11.3076198896069));
#41780=CARTESIAN_POINT('Ctrl Pts',(1.57034651217938,117.198776184031,11.3533311812538));
#41781=CARTESIAN_POINT('Ctrl Pts',(1.62670074151225,117.210435781116,11.401620507495));
#41782=CARTESIAN_POINT('Ctrl Pts',(1.67550891578635,117.220534111858,11.4434437012226));
#41783=CARTESIAN_POINT('Ctrl Pts',(1.72274007319172,117.230657724238,11.4871857180797));
#41784=CARTESIAN_POINT('Ctrl Pts',(1.76816646432715,117.240762291144,11.5326326487035));
#41785=CARTESIAN_POINT('Ctrl Pts',(1.78004664653425,117.243404898073,11.5445182025207));
#41786=CARTESIAN_POINT('Ctrl Pts',(1.79180358181125,117.24604620237,11.5565201652442));
#41787=CARTESIAN_POINT('Ctrl Pts',(1.8034336175365,117.248685411144,11.5686342999992));
#41788=CARTESIAN_POINT('Ctrl Pts',(1.8581769435127,117.261108336546,11.6256563112365));
#41789=CARTESIAN_POINT('Ctrl Pts',(1.9101109785362,117.273484663151,11.6851578292605));
#41790=CARTESIAN_POINT('Ctrl Pts',(1.95917679036972,117.285737949046,11.747058821437));
#41791=CARTESIAN_POINT('Ctrl Pts',(1.98646034826758,117.292551516837,11.7814795156205));
#41792=CARTESIAN_POINT('Ctrl Pts',(2.01285694050732,117.299327138072,11.8166436662805));
#41793=CARTESIAN_POINT('Ctrl Pts',(2.03835233884761,117.306052387535,11.8525471535437));
#41794=CARTESIAN_POINT('Ctrl Pts',(2.07762546147216,117.316411964715,11.9078529008443));
#41795=CARTESIAN_POINT('Ctrl Pts',(2.11456156585197,117.326577774003,11.9646335879006));
#41796=CARTESIAN_POINT('Ctrl Pts',(2.14911406704124,117.336628105394,12.0227730323684));
#41797=CARTESIAN_POINT('Ctrl Pts',(2.18321742229141,117.346547793116,12.0801567256029));
#41798=CARTESIAN_POINT('Ctrl Pts',(2.21499884773677,117.356354970737,12.1388654478325));
#41799=CARTESIAN_POINT('Ctrl Pts',(2.24439421061938,117.366121279219,12.1987758505471));
#41800=CARTESIAN_POINT('Ctrl Pts',(2.27355623419998,117.375810063106,12.2582106867036));
#41801=CARTESIAN_POINT('Ctrl Pts',(2.30036947417557,117.385458589752,12.3188293335521));
#41802=CARTESIAN_POINT('Ctrl Pts',(2.32475484863219,117.395133573531,12.3804811618237));
#41803=CARTESIAN_POINT('Ctrl Pts',(2.34410593556398,117.402811185885,12.4294051547896));
#41804=CARTESIAN_POINT('Ctrl Pts',(2.36192759828503,117.41050538556,12.4789793027436));
#41805=CARTESIAN_POINT('Ctrl Pts',(2.37817704323118,117.418248311024,12.5291083402655));
#41806=CARTESIAN_POINT('',(2.37639371954888,118.486854168824,12.5236287354052));
#41807=CARTESIAN_POINT('',(2.37732998843941,117.925623783712,12.5265067145218));
#41808=CARTESIAN_POINT('Ctrl Pts',(2.37639382411024,118.486854164655,12.5236287017601));
#41809=CARTESIAN_POINT('Ctrl Pts',(2.29237449868435,118.455071882635,12.2664540657314));
#41810=CARTESIAN_POINT('Ctrl Pts',(2.16719785357465,118.422212612927,12.0247183887063));
#41811=CARTESIAN_POINT('Ctrl Pts',(1.84820554614646,118.35618592643,11.5959234906477));
#41812=CARTESIAN_POINT('Ctrl Pts',(1.65797254561086,118.323870392737,11.4103165284456));
#41813=CARTESIAN_POINT('Ctrl Pts',(1.17168681790221,118.251443979973,11.0668784972995));
#41814=CARTESIAN_POINT('Ctrl Pts',(0.865841333419305,118.211595169798,10.9314448594032));
#41815=CARTESIAN_POINT('Ctrl Pts',(0.388388355687752,118.153118629885,10.8253143118232));
#41816=CARTESIAN_POINT('Ctrl Pts',(0.231386992078417,118.134476740984,10.8057288724813));
#41817=CARTESIAN_POINT('Ctrl Pts',(-0.0819192501568569,118.09774354819,
10.7965051430853));
#41818=CARTESIAN_POINT('Ctrl Pts',(-0.23750455082634,118.079729277626,10.8064492283048));
#41819=CARTESIAN_POINT('Ctrl Pts',(-0.540961868585215,118.044110016183,
10.8545219930496));
#41820=CARTESIAN_POINT('Ctrl Pts',(-0.688276731890548,118.026578242465,
10.8918327871561));
#41821=CARTESIAN_POINT('Ctrl Pts',(-1.06771232274408,117.979320612286,11.0256130190422));
#41822=CARTESIAN_POINT('Ctrl Pts',(-1.29025443117006,117.949427715848,11.1440578220645));
#41823=CARTESIAN_POINT('Ctrl Pts',(-1.73483039841509,117.884058903072,11.4745320778206));
#41824=CARTESIAN_POINT('Ctrl Pts',(-1.94332056132931,117.849380326021,11.6982671554484));
#41825=CARTESIAN_POINT('Ctrl Pts',(-2.16869487811854,117.801600611764,12.0509879017169));
#41826=CARTESIAN_POINT('Ctrl Pts',(-2.22393087527522,117.788485405148,12.1522204186784));
#41827=CARTESIAN_POINT('Ctrl Pts',(-2.34892858865178,117.754045018187,12.4244783697562));
#41828=CARTESIAN_POINT('Ctrl Pts',(-2.40709440953146,117.732674965509,12.6000681821379));
#41829=CARTESIAN_POINT('Ctrl Pts',(-2.48169828832362,117.691521844839,12.951217002664));
#41830=CARTESIAN_POINT('Ctrl Pts',(-2.49999810368946,117.671830201486,13.1253310693141));
#41831=CARTESIAN_POINT('Ctrl Pts',(-2.49999999985264,117.652418880134,13.2999728563934));
#41832=CARTESIAN_POINT('Origin',(0.,70.2,13.3));
#41833=CARTESIAN_POINT('',(-2.50002326288683,113.63543715375,13.3006174987927));
#41834=CARTESIAN_POINT('',(-2.5,114.793997579998,13.3000000010378));
#41835=CARTESIAN_POINT('',(-2.5,70.2,13.3));
#41836=CARTESIAN_POINT('Ctrl Pts',(-2.5,114.793997579998,13.3000000020756));
#41837=CARTESIAN_POINT('Ctrl Pts',(-2.50000000002252,114.797385889231,13.2728777046832));
#41838=CARTESIAN_POINT('Ctrl Pts',(-2.49955862869347,114.800774717604,13.2457529010415));
#41839=CARTESIAN_POINT('Ctrl Pts',(-2.49190150031146,114.830166814656,13.0106026288428));
#41840=CARTESIAN_POINT('Ctrl Pts',(-2.45917284392043,114.856049634189,12.8042153754441));
#41841=CARTESIAN_POINT('Ctrl Pts',(-2.35146918787085,114.904049605931,12.4324861684175));
#41842=CARTESIAN_POINT('Ctrl Pts',(-2.28340152883787,114.926045267411,12.2665224602698));
#41843=CARTESIAN_POINT('Ctrl Pts',(-2.05669318098404,114.984410429985,11.8480094363152));
#41844=CARTESIAN_POINT('Ctrl Pts',(-1.86974559343431,115.02018752997,11.6140809587873));
#41845=CARTESIAN_POINT('Ctrl Pts',(-1.39300455220041,115.097611737711,11.1969877167693));
#41846=CARTESIAN_POINT('Ctrl Pts',(-1.0977401884382,115.138312755489,11.0288491360474));
#41847=CARTESIAN_POINT('Ctrl Pts',(-0.479917790473351,115.216913456915,
10.8265213203945));
#41848=CARTESIAN_POINT('Ctrl Pts',(-0.166029962590372,115.254399332085,
10.7858645153009));
#41849=CARTESIAN_POINT('Ctrl Pts',(0.298014978088405,115.310102267509,10.8132316813518));
#41850=CARTESIAN_POINT('Ctrl Pts',(0.447726592942345,115.328138530198,10.8357825773864));
#41851=CARTESIAN_POINT('Ctrl Pts',(0.887437456843971,115.382620288385,10.9434296106405));
#41852=CARTESIAN_POINT('Ctrl Pts',(1.16505368337756,115.419006550745,11.0675878969932));
#41853=CARTESIAN_POINT('Ctrl Pts',(1.64964681615153,115.488688629676,11.3998934724379));
#41854=CARTESIAN_POINT('Ctrl Pts',(1.85596666936301,115.521525836049,11.6008398262939));
#41855=CARTESIAN_POINT('Ctrl Pts',(2.21975084583485,115.594032687924,12.1024705868506));
#41856=CARTESIAN_POINT('Ctrl Pts',(2.35959987421961,115.633928398604,12.4091249040404));
#41857=CARTESIAN_POINT('Ctrl Pts',(2.49930674860258,115.70608305261,13.0103911353894));
#41858=CARTESIAN_POINT('Ctrl Pts',(2.51603037566584,115.738004574514,13.2955135399316));
#41859=CARTESIAN_POINT('Ctrl Pts',(2.44754858026923,115.808810143904,13.9089612556534));
#41860=CARTESIAN_POINT('Ctrl Pts',(2.34452701964057,115.848357358424,14.2297832668353));
#41861=CARTESIAN_POINT('Ctrl Pts',(2.11048949387997,115.9035194425,14.6479741892287));
#41862=CARTESIAN_POINT('Ctrl Pts',(2.02840636605182,115.919980245341,14.768599183933));
#41863=CARTESIAN_POINT('Ctrl Pts',(1.83699748384671,115.95379355059,15.0029588351278));
#41864=CARTESIAN_POINT('Ctrl Pts',(1.72650133924465,115.971036476695,15.1148894878823));
#41865=CARTESIAN_POINT('Ctrl Pts',(1.34988225547283,116.02560205963,15.4306657198259));
#41866=CARTESIAN_POINT('Ctrl Pts',(1.05299152127506,116.063637079497,15.5919691090266));
#41867=CARTESIAN_POINT('Ctrl Pts',(0.439708259853296,116.134956646751,15.7800962773638));
#41868=CARTESIAN_POINT('Ctrl Pts',(0.132191672253177,116.167781256259,15.8153000771159));
#41869=CARTESIAN_POINT('Ctrl Pts',(-0.507456022132339,116.238328474224,
15.7706726198806));
#41870=CARTESIAN_POINT('Ctrl Pts',(-0.832956242345116,116.276364335092,
15.6807642589591));
#41871=CARTESIAN_POINT('Ctrl Pts',(-1.38386970925306,116.342148183849,15.4012326146894));
#41872=CARTESIAN_POINT('Ctrl Pts',(-1.61286175207875,116.370129562098,15.2310486178901));
#41873=CARTESIAN_POINT('Ctrl Pts',(-2.03856336916099,116.433471672011,14.7850290700612));
#41874=CARTESIAN_POINT('Ctrl Pts',(-2.21813157489942,116.469971070782,14.5004154086595));
#41875=CARTESIAN_POINT('Ctrl Pts',(-2.4365058001107,116.531934314149,13.9263584664292));
#41876=CARTESIAN_POINT('Ctrl Pts',(-2.49140634538486,116.557734397389,13.648972460494));
#41877=CARTESIAN_POINT('Ctrl Pts',(-2.49969015735141,116.586599767941,13.3454626860678));
#41878=CARTESIAN_POINT('Ctrl Pts',(-2.5,116.588769567576,13.3227244381384));
#41879=CARTESIAN_POINT('Ctrl Pts',(-2.5,116.590949403176,13.3));
#41880=CARTESIAN_POINT('',(2.40669191446942,114.731988374668,12.6249749337064));
#41881=CARTESIAN_POINT('Ctrl Pts',(-2.49999989834126,115.75317125154,13.2992870528137));
#41882=CARTESIAN_POINT('Ctrl Pts',(-2.50008184411521,115.716846549025,13.5866357239191));
#41883=CARTESIAN_POINT('Ctrl Pts',(-2.4506214260268,115.68099481083,13.8718771511382));
#41884=CARTESIAN_POINT('Ctrl Pts',(-2.27148199259844,115.614307807583,14.3723863367816));
#41885=CARTESIAN_POINT('Ctrl Pts',(-2.15593128189566,115.583903092524,14.5890356131345));
#41886=CARTESIAN_POINT('Ctrl Pts',(-1.83762731193967,115.517060933905,15.0199042209758));
#41887=CARTESIAN_POINT('Ctrl Pts',(-1.62476569711639,115.481067765976,15.222266975671));
#41888=CARTESIAN_POINT('Ctrl Pts',(-1.11286078002683,115.405310811968,15.5617954833605));
#41889=CARTESIAN_POINT('Ctrl Pts',(-0.811821305593659,115.366328837562,
15.6864587765518));
#41890=CARTESIAN_POINT('Ctrl Pts',(-0.220822194139709,115.293507807071,
15.8059308778056));
#41891=CARTESIAN_POINT('Ctrl Pts',(0.0611000182903552,115.260078353759,
15.814898816406));
#41892=CARTESIAN_POINT('Ctrl Pts',(0.646198561619679,115.188655291391,15.73491437931));
#41893=CARTESIAN_POINT('Ctrl Pts',(0.943342589834492,115.151546914754,15.6359278686744));
#41894=CARTESIAN_POINT('Ctrl Pts',(1.47010395231188,115.080581081869,15.3430692761423));
#41895=CARTESIAN_POINT('Ctrl Pts',(1.69861033226413,115.047205451045,15.15744647314));
#41896=CARTESIAN_POINT('Ctrl Pts',(2.10719160069082,114.975377847186,14.6856154627772));
#41897=CARTESIAN_POINT('Ctrl Pts',(2.27235073686159,114.937009102848,14.3938971371417));
#41898=CARTESIAN_POINT('Ctrl Pts',(2.4547506584159,114.869659507586,13.8372419312285));
#41899=CARTESIAN_POINT('Ctrl Pts',(2.49660250556101,114.840873704305,13.5853658481135));
#41900=CARTESIAN_POINT('Ctrl Pts',(2.50281009642801,114.785206180601,13.0927502466165));
#41901=CARTESIAN_POINT('Ctrl Pts',(2.4716000689058,114.758700075465,12.8547783578521));
#41902=CARTESIAN_POINT('Ctrl Pts',(2.40710702503148,114.732100473491,12.624843892093));
#41903=CARTESIAN_POINT('Ctrl Pts',(2.40671107393509,114.732017803112,12.6249492691423));
#41904=CARTESIAN_POINT('Ctrl Pts',(2.38603655571224,114.719000108274,12.550738421636));
#41905=CARTESIAN_POINT('Ctrl Pts',(2.36192028942924,114.705932228044,12.4776884630487));
#41906=CARTESIAN_POINT('Ctrl Pts',(2.33452665970069,114.692929106293,12.4060060713853));
#41907=CARTESIAN_POINT('Ctrl Pts',(2.33039701405768,114.690968859126,12.3951998044048));
#41908=CARTESIAN_POINT('Ctrl Pts',(2.32619281813754,114.689010075427,12.3844245493953));
#41909=CARTESIAN_POINT('Ctrl Pts',(2.32191456017635,114.68705314018,12.373680944972));
#41910=CARTESIAN_POINT('Ctrl Pts',(2.28917399573477,114.672077146412,12.2914625102381));
#41911=CARTESIAN_POINT('Ctrl Pts',(2.2521012679024,114.657209864433,12.2110977667261));
#41912=CARTESIAN_POINT('Ctrl Pts',(2.21077820277219,114.6424849766,12.1329078564742));
#41913=CARTESIAN_POINT('Ctrl Pts',(2.21077697653088,114.642484539647,12.1329055362277));
#41914=CARTESIAN_POINT('Ctrl Pts',(2.2107757502859,114.642484102693,12.1329032159833));
#41915=CARTESIAN_POINT('Ctrl Pts',(2.2107745240371,114.64248366574,12.1329008957406));
#41916=CARTESIAN_POINT('Ctrl Pts',(2.1698507369237,114.627901152448,12.0554670850472));
#41917=CARTESIAN_POINT('Ctrl Pts',(2.12475641430129,114.613457757854,11.9801627370877));
#41918=CARTESIAN_POINT('Ctrl Pts',(2.07571785117442,114.599065288004,11.9072896599852));
#41919=CARTESIAN_POINT('Ctrl Pts',(2.03735758410725,114.587806822177,11.8502849167503));
#41920=CARTESIAN_POINT('Ctrl Pts',(1.99658309629734,114.576579921931,11.7947685263937));
#41921=CARTESIAN_POINT('Ctrl Pts',(1.95349531511491,114.565353621623,11.7408980764147));
#41922=CARTESIAN_POINT('Ctrl Pts',(1.8986874944664,114.551073725166,11.6723746602703));
#41923=CARTESIAN_POINT('Ctrl Pts',(1.84042639462137,114.536869361689,11.606874339813));
#41924=CARTESIAN_POINT('Ctrl Pts',(1.7790153456993,114.522703384979,11.5446440296108));
#41925=CARTESIAN_POINT('Ctrl Pts',(1.71698406067292,114.508394335478,11.4817852089721));
#41926=CARTESIAN_POINT('Ctrl Pts',(1.6517389305043,114.494124544484,11.4222627597994));
#41927=CARTESIAN_POINT('Ctrl Pts',(1.58356346547917,114.479885790931,11.3663342036022));
#41928=CARTESIAN_POINT('Ctrl Pts',(1.51591781669985,114.465757691892,11.3108402884841));
#41929=CARTESIAN_POINT('Ctrl Pts',(1.44538739137413,114.451660416136,11.2588842683477));
#41930=CARTESIAN_POINT('Ctrl Pts',(1.37221876351566,114.437612544851,11.2107234020551));
#41931=CARTESIAN_POINT('Ctrl Pts',(1.31353379465473,114.426345436076,11.1720959325861));
#41932=CARTESIAN_POINT('Ctrl Pts',(1.2531511881548,114.415110690171,11.1359097259345));
#41933=CARTESIAN_POINT('Ctrl Pts',(1.19118238541695,114.403928443348,11.1023038300403));
#41934=CARTESIAN_POINT('Ctrl Pts',(1.18018643235601,114.401944227811,11.0963406866924));
#41935=CARTESIAN_POINT('Ctrl Pts',(1.16914870734806,114.39996316254,11.0904632670091));
#41936=CARTESIAN_POINT('Ctrl Pts',(1.15806998550336,114.397985378393,11.0846719975152));
#41937=CARTESIAN_POINT('Ctrl Pts',(1.15806078809735,114.397983736463,11.084667189681));
#41938=CARTESIAN_POINT('Ctrl Pts',(1.15805159066309,114.397982094536,11.0846623819063));
#41939=CARTESIAN_POINT('Ctrl Pts',(1.15804239320057,114.39798045261,11.0846575741909));
#41940=CARTESIAN_POINT('Ctrl Pts',(1.08167856283755,114.384348029017,11.0447405253777));
#41941=CARTESIAN_POINT('Ctrl Pts',(1.00336763378465,114.370869434528,11.0089137747217));
#41942=CARTESIAN_POINT('Ctrl Pts',(0.923470403547197,114.357462176603,10.9772313192681));
#41943=CARTESIAN_POINT('Ctrl Pts',(0.842120924938991,114.343811222264,10.9449729891043));
#41944=CARTESIAN_POINT('Ctrl Pts',(0.759126514312415,114.330233992969,10.9170115020167));
#41945=CARTESIAN_POINT('Ctrl Pts',(0.674860844878216,114.316671171922,10.8934318208214));
#41946=CARTESIAN_POINT('Ctrl Pts',(0.589942358421628,114.303003277949,10.8696694647909));
#41947=CARTESIAN_POINT('Ctrl Pts',(0.503732788690918,114.289349949821,10.8503574469222));
#41948=CARTESIAN_POINT('Ctrl Pts',(0.416611040688116,114.275680587882,10.8356037522074));
#41949=CARTESIAN_POINT('Ctrl Pts',(0.358168881629512,114.266511040175,10.8257068229907));
#41950=CARTESIAN_POINT('Ctrl Pts',(0.299316209581032,114.257334914046,10.8178614586516));
#41951=CARTESIAN_POINT('Ctrl Pts',(0.240166277877519,114.248150523747,10.8121047457223));
#41952=CARTESIAN_POINT('Ctrl Pts',(0.155211410934926,114.23495932245,10.8038365911049));
#41953=CARTESIAN_POINT('Ctrl Pts',(0.0700788031493985,114.221816744476,
10.799919257017));
#41954=CARTESIAN_POINT('Ctrl Pts',(-0.0149028882690931,114.208738362147,
10.8003417600113));
#41955=CARTESIAN_POINT('Ctrl Pts',(-0.0208006222667158,114.207830721704,
10.800371081742));
#41956=CARTESIAN_POINT('Ctrl Pts',(-0.0266976415687111,114.206923389794,
10.8004213225244));
#41957=CARTESIAN_POINT('Ctrl Pts',(-0.0325938415091329,114.206016371328,
10.8004924863282));
#41958=CARTESIAN_POINT('Ctrl Pts',(-0.115617731118418,114.193244721498,
10.8014945377932));
#41959=CARTESIAN_POINT('Ctrl Pts',(-0.198477037236091,114.18053572853,10.8066410517021));
#41960=CARTESIAN_POINT('Ctrl Pts',(-0.280897820046986,114.167922066076,
10.8159439136147));
#41961=CARTESIAN_POINT('Ctrl Pts',(-0.288667161823087,114.166733047344,
10.8168208418751));
#41962=CARTESIAN_POINT('Ctrl Pts',(-0.296432625531919,114.165544873754,
10.8177347359478));
#41963=CARTESIAN_POINT('Ctrl Pts',(-0.304193992661227,114.164357571456,
10.8186856271663));
#41964=CARTESIAN_POINT('Ctrl Pts',(-0.304199649362122,114.164356706117,
10.8186863202023));
#41965=CARTESIAN_POINT('Ctrl Pts',(-0.304205306060841,114.164355840778,
10.818687013258));
#41966=CARTESIAN_POINT('Ctrl Pts',(-0.304210962757384,114.16435497544,10.8186877063334));
#41967=CARTESIAN_POINT('Ctrl Pts',(-0.391348216434744,114.151025077656,
10.8293640228845));
#41968=CARTESIAN_POINT('Ctrl Pts',(-0.477972035296507,114.13780468443,10.8446995212591));
#41969=CARTESIAN_POINT('Ctrl Pts',(-0.563722922960105,114.124609062505,
10.8646086883252));
#41970=CARTESIAN_POINT('Ctrl Pts',(-0.62561406599761,114.115085054693,10.8789782317809));
#41971=CARTESIAN_POINT('Ctrl Pts',(-0.687049844929214,114.105574437132,
10.8957310521915));
#41972=CARTESIAN_POINT('Ctrl Pts',(-0.747885721084445,114.096054101726,
10.9148412182077));
#41973=CARTESIAN_POINT('Ctrl Pts',(-0.831713446375473,114.082935723041,
10.9411737352735));
#41974=CARTESIAN_POINT('Ctrl Pts',(-0.913961186335416,114.069866479222,
10.9718430192832));
#41975=CARTESIAN_POINT('Ctrl Pts',(-0.994286798253288,114.056811004444,
11.0066559216147));
#41976=CARTESIAN_POINT('Ctrl Pts',(-1.07540901325354,114.043626056248,11.0418140695614));
#41977=CARTESIAN_POINT('Ctrl Pts',(-1.15457050931461,114.030455293469,11.0811982831899));
#41978=CARTESIAN_POINT('Ctrl Pts',(-1.23142813047825,114.017291787493,11.1246288716901));
#41979=CARTESIAN_POINT('Ctrl Pts',(-1.30769828236307,114.004228898154,11.1677274939373));
#41980=CARTESIAN_POINT('Ctrl Pts',(-1.3816996941409,113.991173464214,11.2148103537045));
#41981=CARTESIAN_POINT('Ctrl Pts',(-1.45310796354058,113.978144094454,11.2657257295881));
#41982=CARTESIAN_POINT('Ctrl Pts',(-1.50981508815594,113.967797140231,11.306158925762));
#41983=CARTESIAN_POINT('Ctrl Pts',(-1.56488724741967,113.957467187443,11.349009316401));
#41984=CARTESIAN_POINT('Ctrl Pts',(-1.61816535072865,113.947172949771,11.3942159583652));
#41985=CARTESIAN_POINT('Ctrl Pts',(-1.63206269290655,113.944487746385,11.4060078978877));
#41986=CARTESIAN_POINT('Ctrl Pts',(-1.6458229034023,113.941807941329,11.4179474284215));
#41987=CARTESIAN_POINT('Ctrl Pts',(-1.65944402960632,113.939133916623,11.4300326652617));
#41988=CARTESIAN_POINT('Ctrl Pts',(-1.65944918529116,113.939132904487,11.4300372396024));
#41989=CARTESIAN_POINT('Ctrl Pts',(-1.65945434095606,113.939131892352,11.430041813964));
#41990=CARTESIAN_POINT('Ctrl Pts',(-1.65945949660102,113.939130880218,11.4300463883465));
#41991=CARTESIAN_POINT('Ctrl Pts',(-1.72416273610041,113.926428617768,11.487454795743));
#41992=CARTESIAN_POINT('Ctrl Pts',(-1.78572985027925,113.913854680771,11.5481503010416));
#41993=CARTESIAN_POINT('Ctrl Pts',(-1.84396740565358,113.901329775944,11.6118290328535));
#41994=CARTESIAN_POINT('Ctrl Pts',(-1.90321619869904,113.888587388506,11.6766134829952));
#41995=CARTESIAN_POINT('Ctrl Pts',(-1.9590181108991,113.875895587199,11.7444861696485));
#41996=CARTESIAN_POINT('Ctrl Pts',(-2.01114658435125,113.863199429364,11.8151322313827));
#41997=CARTESIAN_POINT('Ctrl Pts',(-2.06359350863811,113.850425711191,11.8862098671846));
#41998=CARTESIAN_POINT('Ctrl Pts',(-2.11232137609723,113.837647590056,11.960094833088));
#41999=CARTESIAN_POINT('Ctrl Pts',(-2.15708658914897,113.824838879979,12.0364679833058));
#42000=CARTESIAN_POINT('Ctrl Pts',(-2.18365740274702,113.817236149539,12.0817999855458));
#42001=CARTESIAN_POINT('Ctrl Pts',(-2.20883194412841,113.809623213022,12.128008616839));
#42002=CARTESIAN_POINT('Ctrl Pts',(-2.23255814550346,113.801999384522,12.1750278963945));
#42003=CARTESIAN_POINT('Ctrl Pts',(-2.272374403431,113.789205413959,12.2539335641311));
#42004=CARTESIAN_POINT('Ctrl Pts',(-2.30790217841304,113.776446866853,12.3347046854354));
#42005=CARTESIAN_POINT('Ctrl Pts',(-2.33902960370211,113.763740361142,12.4169872092265));
#42006=CARTESIAN_POINT('Ctrl Pts',(-2.36798167871121,113.751921853732,12.4935193919757));
#42007=CARTESIAN_POINT('Ctrl Pts',(-2.39312741066382,113.74014868853,12.5713592310076));
#42008=CARTESIAN_POINT('Ctrl Pts',(-2.41437667314438,113.728449496644,12.6502582010047));
#42009=CARTESIAN_POINT('Ctrl Pts',(-2.41607055463293,113.727516897473,12.6565476195136));
#42010=CARTESIAN_POINT('Ctrl Pts',(-2.41773966055965,113.7265847667,12.662843790757));
#42011=CARTESIAN_POINT('Ctrl Pts',(-2.41938393675111,113.725653117961,12.6691466003444));
#42012=CARTESIAN_POINT('Ctrl Pts',(-2.42234077420046,113.723977770536,12.6804806958697));
#42013=CARTESIAN_POINT('Ctrl Pts',(-2.42521736162318,113.722304009972,12.6918362489259));
#42014=CARTESIAN_POINT('Ctrl Pts',(-2.42801341001787,113.720631938887,12.7032126026095));
#42015=CARTESIAN_POINT('Ctrl Pts',(-2.42801894130329,113.72062863111,12.7032351078921));
#42016=CARTESIAN_POINT('Ctrl Pts',(-2.42802447227337,113.720625323341,12.7032576132562));
#42017=CARTESIAN_POINT('Ctrl Pts',(-2.42803000292807,113.720622015577,12.7032801187016));
#42018=CARTESIAN_POINT('Ctrl Pts',(-2.44761689028156,113.708907528007,12.7829834538748));
#42019=CARTESIAN_POINT('Ctrl Pts',(-2.46325232600675,113.697274312845,12.863709368401));
#42020=CARTESIAN_POINT('Ctrl Pts',(-2.47488540907793,113.685656562519,12.9451701077313));
#42021=CARTESIAN_POINT('Ctrl Pts',(-2.47571690509852,113.684826162434,12.950992663985));
#42022=CARTESIAN_POINT('Ctrl Pts',(-2.47652793341817,113.68399584297,12.9568189651233));
#42023=CARTESIAN_POINT('Ctrl Pts',(-2.47731846642314,113.683165580842,12.9626489014737));
#42024=CARTESIAN_POINT('Ctrl Pts',(-2.48494713330537,113.67515352674,13.0189079597056));
#42025=CARTESIAN_POINT('Ctrl Pts',(-2.49066846227995,113.667147117449,13.0755059584162));
#42026=CARTESIAN_POINT('Ctrl Pts',(-2.49445986057212,113.659131020065,13.1323371808067));
#42027=CARTESIAN_POINT('Ctrl Pts',(-2.4982010969503,113.651220979274,13.1884165004242));
#42028=CARTESIAN_POINT('Ctrl Pts',(-2.50005122341816,113.643325754841,13.2445504344204));
#42029=CARTESIAN_POINT('Ctrl Pts',(-2.50002326288683,113.63543715375,13.3006174987927));
#42030=CARTESIAN_POINT('Origin',(0.,70.2,13.3));
#42031=CARTESIAN_POINT('',(-2.5,111.608333038426,13.3));
#42032=CARTESIAN_POINT('',(-2.5,112.746400080882,13.3));
#42033=CARTESIAN_POINT('',(-2.5,70.2,13.3));
#42034=CARTESIAN_POINT('Ctrl Pts',(-2.5,112.746400080882,13.2999999999999));
#42035=CARTESIAN_POINT('Ctrl Pts',(-2.5,112.753815786924,13.2504512721242));
#42036=CARTESIAN_POINT('Ctrl Pts',(-2.49852698225489,112.761198580106,13.2008614963978));
#42037=CARTESIAN_POINT('Ctrl Pts',(-2.48028274540318,112.806419689986,12.8946851924858));
#42038=CARTESIAN_POINT('Ctrl Pts',(-2.42555695618829,112.84118494686,12.6420817968267));
#42039=CARTESIAN_POINT('Ctrl Pts',(-2.21899081222048,112.919059926422,12.1053950897869));
#42040=CARTESIAN_POINT('Ctrl Pts',(-2.04929591841819,112.962172914944,11.8332456817295));
#42041=CARTESIAN_POINT('Ctrl Pts',(-1.60442086699413,113.050703854793,11.3534413243468));
#42042=CARTESIAN_POINT('Ctrl Pts',(-1.32811556445397,113.094201856163,11.1553801417068));
#42043=CARTESIAN_POINT('Ctrl Pts',(-0.879925922177475,113.160160743817,
10.9548829918448));
#42044=CARTESIAN_POINT('Ctrl Pts',(-0.733439588801397,113.181027151995,
10.9050249548889));
#42045=CARTESIAN_POINT('Ctrl Pts',(-0.284824237775757,113.24324131313,10.797382739653));
#42046=CARTESIAN_POINT('Ctrl Pts',(0.024324916665919,113.282911646403,10.78133244488));
#42047=CARTESIAN_POINT('Ctrl Pts',(0.652270566389332,113.366151142462,10.8646194126178));
#42048=CARTESIAN_POINT('Ctrl Pts',(0.964289224234859,113.409690487182,10.9704902790412));
#42049=CARTESIAN_POINT('Ctrl Pts',(1.38203089680102,113.473742733204,11.2109255478757));
#42050=CARTESIAN_POINT('Ctrl Pts',(1.50943061924174,113.494103088808,11.3010326495817));
#42051=CARTESIAN_POINT('Ctrl Pts',(1.86959923854331,113.556243189497,11.6099642513656));
#42052=CARTESIAN_POINT('Ctrl Pts',(2.06966085364777,113.597807703668,11.8618964340852));
#42053=CARTESIAN_POINT('Ctrl Pts',(2.29488090205699,113.661365951993,12.2940574152866));
#42054=CARTESIAN_POINT('Ctrl Pts',(2.35745257094803,113.683239454434,12.4509914927382));
#42055=CARTESIAN_POINT('Ctrl Pts',(2.48859592421676,113.745564407196,12.9098662641539));
#42056=CARTESIAN_POINT('Ctrl Pts',(2.51772212539333,113.785664064245,13.2198960333267));
#42057=CARTESIAN_POINT('Ctrl Pts',(2.46033119197494,113.867377867542,13.8482550563151));
#42058=CARTESIAN_POINT('Ctrl Pts',(2.36926741833782,113.908887818044,14.1604597562973));
#42059=CARTESIAN_POINT('Ctrl Pts',(2.14519752951451,113.971987167063,14.5945166550251));
#42060=CARTESIAN_POINT('Ctrl Pts',(2.05437536733974,113.993303992244,14.7342912266888));
#42061=CARTESIAN_POINT('Ctrl Pts',(1.84927709341868,114.035494934116,14.9900518678522));
#42062=CARTESIAN_POINT('Ctrl Pts',(1.73622571015375,114.056263044081,15.1059958276731));
#42063=CARTESIAN_POINT('Ctrl Pts',(1.35751648450548,114.120075409954,15.4257370132797));
#42064=CARTESIAN_POINT('Ctrl Pts',(1.06160829432475,114.162309883462,15.587929557014));
#42065=CARTESIAN_POINT('Ctrl Pts',(0.590639130471669,114.225336214171,15.7344326429001));
#42066=CARTESIAN_POINT('Ctrl Pts',(0.434537905454778,114.245626749545,15.7670825428223));
#42067=CARTESIAN_POINT('Ctrl Pts',(0.112837426690217,114.286850657165,15.8028681481862));
#42068=CARTESIAN_POINT('Ctrl Pts',(-0.0521207760547313,114.307672043328,
15.8048689549461));
#42069=CARTESIAN_POINT('Ctrl Pts',(-0.520815329524812,114.367317752154,
15.7642065263245));
#42070=CARTESIAN_POINT('Ctrl Pts',(-0.818140092689986,114.405780165051,
15.682063214996));
#42071=CARTESIAN_POINT('Ctrl Pts',(-1.24044431316074,114.464991016743,15.4767150278274));
#42072=CARTESIAN_POINT('Ctrl Pts',(-1.3802617770565,114.485534910198,15.390854010734));
#42073=CARTESIAN_POINT('Ctrl Pts',(-1.76464981009766,114.546171400412,15.0993354063904));
#42074=CARTESIAN_POINT('Ctrl Pts',(-1.97946570119846,114.585773662872,14.8599139110405));
#42075=CARTESIAN_POINT('Ctrl Pts',(-2.22891130005095,114.646316726717,14.444328010222));
#42076=CARTESIAN_POINT('Ctrl Pts',(-2.29993057925986,114.666982413506,14.2939082640419));
#42077=CARTESIAN_POINT('Ctrl Pts',(-2.39934061676893,114.703943623379,14.0143321805558));
#42078=CARTESIAN_POINT('Ctrl Pts',(-2.4334205579743,114.720134853252,13.8878527112955));
#42079=CARTESIAN_POINT('Ctrl Pts',(-2.47361631768746,114.747333541985,13.6727824881431));
#42080=CARTESIAN_POINT('Ctrl Pts',(-2.48520435230191,114.75829395106,13.5854870139385));
#42081=CARTESIAN_POINT('Ctrl Pts',(-2.49738731604369,114.777513152509,13.4319620063582));
#42082=CARTESIAN_POINT('Ctrl Pts',(-2.49999999994521,114.78575383967,13.3659884232862));
#42083=CARTESIAN_POINT('Ctrl Pts',(-2.5,114.793997579998,13.3000000020756));
#42084=CARTESIAN_POINT('Ctrl Pts',(-2.49999992423213,113.635422974112,13.300615499269));
#42085=CARTESIAN_POINT('Ctrl Pts',(-2.49993703972846,113.599525349135,13.5560361997111));
#42086=CARTESIAN_POINT('Ctrl Pts',(-2.46072864461712,113.563484692851,13.8099450047488));
#42087=CARTESIAN_POINT('Ctrl Pts',(-2.30125078341498,113.489021137123,14.3144855223787));
#42088=CARTESIAN_POINT('Ctrl Pts',(-2.17642926892917,113.451620898376,14.5602141872255));
#42089=CARTESIAN_POINT('Ctrl Pts',(-1.91840788023706,113.391588607151,14.9111734902358));
#42090=CARTESIAN_POINT('Ctrl Pts',(-1.81015694310975,113.369367075414,15.0319084127732));
#42091=CARTESIAN_POINT('Ctrl Pts',(-1.45341965586932,113.303011864418,15.3595181248978));
#42092=CARTESIAN_POINT('Ctrl Pts',(-1.1758217445381,113.25950062641,15.5296935957019));
#42093=CARTESIAN_POINT('Ctrl Pts',(-0.575113398708736,113.172776977878,
15.753707228805));
#42094=CARTESIAN_POINT('Ctrl Pts',(-0.258131681584966,113.130256384498,
15.8069594504734));
#42095=CARTESIAN_POINT('Ctrl Pts',(0.225640896538735,113.065624474727,15.7952814337151));
#42096=CARTESIAN_POINT('Ctrl Pts',(0.390155687127908,113.043696451551,15.7748992481072));
#42097=CARTESIAN_POINT('Ctrl Pts',(0.709368130684422,113.000177211355,15.7027087118395));
#42098=CARTESIAN_POINT('Ctrl Pts',(0.863446950582938,112.978695790749,15.6517389144345));
#42099=CARTESIAN_POINT('Ctrl Pts',(1.16118397455973,112.935601926959,15.5200083080719));
#42100=CARTESIAN_POINT('Ctrl Pts',(1.30399495537044,112.914070477901,15.4392491879532));
#42101=CARTESIAN_POINT('Ctrl Pts',(1.70549608395798,112.849440648973,15.1569591150295));
#42102=CARTESIAN_POINT('Ctrl Pts',(1.93360969618146,112.80698865331,14.9180853483908));
#42103=CARTESIAN_POINT('Ctrl Pts',(2.25740820833291,112.728316740063,14.4091821727227));
#42104=CARTESIAN_POINT('Ctrl Pts',(2.36601508132898,112.692603330238,14.1533448227506));
#42105=CARTESIAN_POINT('Ctrl Pts',(2.50850694176593,112.614544139567,13.5612253178054));
#42106=CARTESIAN_POINT('Ctrl Pts',(2.52096213046626,112.572601534465,13.2252118158867));
#42107=CARTESIAN_POINT('Ctrl Pts',(2.41709491232301,112.489920817314,12.5898799708317));
#42108=CARTESIAN_POINT('Ctrl Pts',(2.31016801046288,112.450069933046,12.2951335602315));
#42109=CARTESIAN_POINT('Ctrl Pts',(2.07260478440973,112.390452895359,11.8933692380529));
#42110=CARTESIAN_POINT('Ctrl Pts',(1.98087889419261,112.370731470586,11.766889657077));
#42111=CARTESIAN_POINT('Ctrl Pts',(1.65779674484082,112.30887275318,11.3992217548214));
#42112=CARTESIAN_POINT('Ctrl Pts',(1.38968520537882,112.267366551738,11.1952314586677));
#42113=CARTESIAN_POINT('Ctrl Pts',(0.81345988725467,112.187108651779,10.9162411771611));
#42114=CARTESIAN_POINT('Ctrl Pts',(0.515214082937537,112.14909830415,10.8345182190889));
#42115=CARTESIAN_POINT('Ctrl Pts',(0.0426735369502148,112.090135804759,
10.7947556834444));
#42116=CARTESIAN_POINT('Ctrl Pts',(-0.125275961184913,112.069417461386,
10.7975249440082));
#42117=CARTESIAN_POINT('Ctrl Pts',(-0.450578970442157,112.028950133878,
10.8357408701125));
#42118=CARTESIAN_POINT('Ctrl Pts',(-0.607317692404308,112.009294118061,
10.8696164886111));
#42119=CARTESIAN_POINT('Ctrl Pts',(-0.910150655858293,111.97024560837,10.9662157634045));
#42120=CARTESIAN_POINT('Ctrl Pts',(-1.05567456213932,111.950940981782,11.0283319576753));
#42121=CARTESIAN_POINT('Ctrl Pts',(-1.48650189218199,111.890811950433,11.2626256411866));
#42122=CARTESIAN_POINT('Ctrl Pts',(-1.74405103235562,111.850495529867,11.4782126146685));
#42123=CARTESIAN_POINT('Ctrl Pts',(-2.0521156317544,111.790817004304,11.8631430548332));
#42124=CARTESIAN_POINT('Ctrl Pts',(-2.14007229732545,111.771531826763,11.9977590917231));
#42125=CARTESIAN_POINT('Ctrl Pts',(-2.29138224948472,111.732301509873,12.2865903534652));
#42126=CARTESIAN_POINT('Ctrl Pts',(-2.3534748359072,111.712448014133,12.4405854442097));
#42127=CARTESIAN_POINT('Ctrl Pts',(-2.46639860400545,111.664286612685,12.8275089131858));
#42128=CARTESIAN_POINT('Ctrl Pts',(-2.5,111.636366988851,13.0633546777397));
#42129=CARTESIAN_POINT('Ctrl Pts',(-2.5,111.608333038426,13.3000000000001));
#42130=CARTESIAN_POINT('Origin',(0.,70.2,13.3));
#42131=CARTESIAN_POINT('',(-2.50004052090194,109.508185544341,13.2983771895099));
#42132=CARTESIAN_POINT('',(-2.5,110.560415842511,13.3));
#42133=CARTESIAN_POINT('',(-2.5,70.2,13.3));
#42134=CARTESIAN_POINT('',(2.08929110769117,111.244289249369,11.9274842264238));
#42135=CARTESIAN_POINT('Ctrl Pts',(-2.5,110.560415842511,13.3));
#42136=CARTESIAN_POINT('Ctrl Pts',(-2.5,110.584370683036,13.0920730468922));
#42137=CARTESIAN_POINT('Ctrl Pts',(-2.47405787245171,110.608200817813,12.8844414018608));
#42138=CARTESIAN_POINT('Ctrl Pts',(-2.34533043690075,110.666949896553,12.3798636818324));
#42139=CARTESIAN_POINT('Ctrl Pts',(-2.21240249612852,110.700901144954,12.0947971695117));
#42140=CARTESIAN_POINT('Ctrl Pts',(-1.93504890783741,110.754245183841,11.7086651471274));
#42141=CARTESIAN_POINT('Ctrl Pts',(-1.82679420764696,110.77260141554,11.5854759040186));
#42142=CARTESIAN_POINT('Ctrl Pts',(-1.49275364881193,110.82329675654,11.2731990013751));
#42143=CARTESIAN_POINT('Ctrl Pts',(-1.24455563837577,110.854538016865,11.1119955566233));
#42144=CARTESIAN_POINT('Ctrl Pts',(-0.666284738689302,110.921965062839,
10.8673635729908));
#42145=CARTESIAN_POINT('Ctrl Pts',(-0.335518588013175,110.958559556211,
10.8001728934193));
#42146=CARTESIAN_POINT('Ctrl Pts',(0.304137976284174,111.025977192425,10.7998426418367));
#42147=CARTESIAN_POINT('Ctrl Pts',(0.607020187212292,111.056459374609,10.85565220922));
#42148=CARTESIAN_POINT('Ctrl Pts',(1.15445527186085,111.117362606322,11.0648367239618));
#42149=CARTESIAN_POINT('Ctrl Pts',(1.39792202246711,111.146470397471,11.2084369697607));
#42150=CARTESIAN_POINT('Ctrl Pts',(1.79660522546318,111.198230322861,11.5449307811442));
#42151=CARTESIAN_POINT('Ctrl Pts',(1.95729847396441,111.2210116332,11.7261365923488));
#42152=CARTESIAN_POINT('Ctrl Pts',(2.08958333087649,111.244414321256,11.9275418027047));
#42153=CARTESIAN_POINT('Ctrl Pts',(2.09091184280958,111.244255274751,11.9295666139507));
#42154=CARTESIAN_POINT('Ctrl Pts',(2.21253054010004,111.284970005518,12.1151239544681));
#42155=CARTESIAN_POINT('Ctrl Pts',(2.30900676795492,111.322684435055,12.3161256252589));
#42156=CARTESIAN_POINT('Ctrl Pts',(2.4335077814834,111.396411513387,12.699475347969));
#42157=CARTESIAN_POINT('Ctrl Pts',(2.47041201735562,111.430872891983,12.8763747611042));
#42158=CARTESIAN_POINT('Ctrl Pts',(2.51455206744934,111.52046245954,13.3255314183865));
#42159=CARTESIAN_POINT('Ctrl Pts',(2.49698051169547,111.576796334274,13.5981174230396));
#42160=CARTESIAN_POINT('Ctrl Pts',(2.37858078191885,111.673883613869,14.1105762969879));
#42161=CARTESIAN_POINT('Ctrl Pts',(2.28459425240552,111.711900278876,14.3464732099622));
#42162=CARTESIAN_POINT('Ctrl Pts',(1.99690981083706,111.799221855829,14.8366222558941));
#42163=CARTESIAN_POINT('Ctrl Pts',(1.78845502181753,111.84947094421,15.0747534766737));
#42164=CARTESIAN_POINT('Ctrl Pts',(1.30072923679471,111.95792292333,15.4567854333267));
#42165=CARTESIAN_POINT('Ctrl Pts',(1.02715427425439,112.014195572234,15.5997573803887));
#42166=CARTESIAN_POINT('Ctrl Pts',(0.460068335352404,112.107566443777,15.7739788484136));
#42167=CARTESIAN_POINT('Ctrl Pts',(0.173105402682947,112.145123549888,15.8105554982885));
#42168=CARTESIAN_POINT('Ctrl Pts',(-0.400038856030687,112.226856181371,
15.7842923455795));
#42169=CARTESIAN_POINT('Ctrl Pts',(-0.680788012692494,112.270155761364,
15.7223579870173));
#42170=CARTESIAN_POINT('Ctrl Pts',(-1.17642460918943,112.355810486072,15.5200529135176));
#42171=CARTESIAN_POINT('Ctrl Pts',(-1.39271240502498,112.396836001962,15.3912018963467));
#42172=CARTESIAN_POINT('Ctrl Pts',(-1.78057712168394,112.471085378176,15.0727642185427));
#42173=CARTESIAN_POINT('Ctrl Pts',(-1.94979358068073,112.503478099725,14.8848190501461));
#42174=CARTESIAN_POINT('Ctrl Pts',(-2.2108818967367,112.56679614799,14.4881925581217));
#42175=CARTESIAN_POINT('Ctrl Pts',(-2.3079716862597,112.597127401879,14.2863784741139));
#42176=CARTESIAN_POINT('Ctrl Pts',(-2.45861922979916,112.667161857475,13.8240036655302));
#42177=CARTESIAN_POINT('Ctrl Pts',(-2.50000000000002,112.707104458557,13.5625573460289));
#42178=CARTESIAN_POINT('Ctrl Pts',(-2.5,112.746400080882,13.2999999999999));
#42179=CARTESIAN_POINT('',(2.02616441126019,110.570072536149,11.8332575276011));
#42180=CARTESIAN_POINT('Ctrl Pts',(-2.5,111.608333038426,13.3000000000001));
#42181=CARTESIAN_POINT('Ctrl Pts',(-2.5,111.599099972718,13.3779398471102));
#42182=CARTESIAN_POINT('Ctrl Pts',(-2.49635527151303,111.589849429157,13.4559658240946));
#42183=CARTESIAN_POINT('Ctrl Pts',(-2.45782573638485,111.540839411838,13.8661148409415));
#42184=CARTESIAN_POINT('Ctrl Pts',(-2.36038044542047,111.500725318644,14.188839459168));
#42185=CARTESIAN_POINT('Ctrl Pts',(-2.07403389666084,111.429575424823,14.7219765098093));
#42186=CARTESIAN_POINT('Ctrl Pts',(-1.90754689405118,111.398723164012,14.938585373499));
#42187=CARTESIAN_POINT('Ctrl Pts',(-1.60894576554472,111.352314194306,15.2184023803056));
#42188=CARTESIAN_POINT('Ctrl Pts',(-1.50082700824554,111.336760607205,15.3041176577776));
#42189=CARTESIAN_POINT('Ctrl Pts',(-1.10869991052263,111.282813234414,15.5653884913637));
#42190=CARTESIAN_POINT('Ctrl Pts',(-0.797013834972896,111.243261016893,
15.6928940675935));
#42191=CARTESIAN_POINT('Ctrl Pts',(-0.20644117228775,111.174112361976,15.8058178927713));
#42192=CARTESIAN_POINT('Ctrl Pts',(0.0630844876198906,111.144594308231,
15.8135337508679));
#42193=CARTESIAN_POINT('Ctrl Pts',(0.468275405891716,111.100142798027,15.7597809139009));
#42194=CARTESIAN_POINT('Ctrl Pts',(0.605959960202172,111.084978704884,15.7295292123011));
#42195=CARTESIAN_POINT('Ctrl Pts',(1.05860852404524,111.033049732935,15.5891847846559));
#42196=CARTESIAN_POINT('Ctrl Pts',(1.35384735043083,110.994368749858,15.4279096556827));
#42197=CARTESIAN_POINT('Ctrl Pts',(1.81164290653522,110.927253643264,15.0430450286317));
#42198=CARTESIAN_POINT('Ctrl Pts',(1.98618968804743,110.898960372943,14.841242264169));
#42199=CARTESIAN_POINT('Ctrl Pts',(2.2986154924933,110.837435784167,14.3364359854441));
#42200=CARTESIAN_POINT('Ctrl Pts',(2.41469370167995,110.804257223341,14.0259655219129));
#42201=CARTESIAN_POINT('Ctrl Pts',(2.51465739242552,110.736456998861,13.4123130466841));
#42202=CARTESIAN_POINT('Ctrl Pts',(2.51050112902319,110.704723726827,13.1164427349614));
#42203=CARTESIAN_POINT('Ctrl Pts',(2.41984859048833,110.656429980299,12.6449855490945));
#42204=CARTESIAN_POINT('Ctrl Pts',(2.36432368622815,110.638620572774,12.4664997137897));
#42205=CARTESIAN_POINT('Ctrl Pts',(2.21797786032354,110.604334355112,12.1328542246681));
#42206=CARTESIAN_POINT('Ctrl Pts',(2.12933557305595,110.587912623738,11.9780460502149));
#42207=CARTESIAN_POINT('Ctrl Pts',(2.02504033628985,110.570623332967,11.8339810245433));
#42208=CARTESIAN_POINT('Ctrl Pts',(2.0259834028522,110.570059235584,11.8329696480696));
#42209=CARTESIAN_POINT('Ctrl Pts',(1.97582883419295,110.552650219366,11.7640425834076));
#42210=CARTESIAN_POINT('Ctrl Pts',(1.92223002912362,110.535504701489,11.6978035383405));
#42211=CARTESIAN_POINT('Ctrl Pts',(1.86548929155874,110.518551901166,11.6344613355438));
#42212=CARTESIAN_POINT('Ctrl Pts',(1.80790616229344,110.501347413978,11.570178733517));
#42213=CARTESIAN_POINT('Ctrl Pts',(1.74708657362578,110.484341204005,11.508879272392));
#42214=CARTESIAN_POINT('Ctrl Pts',(1.68330635111696,110.467480210923,11.4508013479066));
#42215=CARTESIAN_POINT('Ctrl Pts',(1.61950186928453,110.450612804625,11.3927013330129));
#42216=CARTESIAN_POINT('Ctrl Pts',(1.55273409637837,110.43389064751,11.3378249928812));
#42217=CARTESIAN_POINT('Ctrl Pts',(1.48324649033605,110.417283438422,11.2864357495786));
#42218=CARTESIAN_POINT('Ctrl Pts',(1.42375348366725,110.403064891299,11.2424379668282));
#42219=CARTESIAN_POINT('Ctrl Pts',(1.36226614263345,110.388930975654,11.2009965189817));
#42220=CARTESIAN_POINT('Ctrl Pts',(1.29892115578174,110.374876370531,11.1622943661129));
#42221=CARTESIAN_POINT('Ctrl Pts',(1.22445648225379,110.358354596133,11.1167983715373));
#42222=CARTESIAN_POINT('Ctrl Pts',(1.14782225782505,110.342029277239,11.0753299337114));
#42223=CARTESIAN_POINT('Ctrl Pts',(1.06928416796316,110.325917111898,11.0380836744721));
#42224=CARTESIAN_POINT('Ctrl Pts',(1.02577658878568,110.316991489814,11.0174504431856));
#42225=CARTESIAN_POINT('Ctrl Pts',(0.981683939057707,110.308131636343,10.9981133110716));
#42226=CARTESIAN_POINT('Ctrl Pts',(0.937046037671465,110.299342770227,10.9801092332557));
#42227=CARTESIAN_POINT('Ctrl Pts',(0.858005356480925,110.28378025624,10.9482292718198));
#42228=CARTESIAN_POINT('Ctrl Pts',(0.777257832873348,110.268440135178,10.9205269907542));
#42229=CARTESIAN_POINT('Ctrl Pts',(0.695160321559169,110.253234098766,10.897021913865));
#42230=CARTESIAN_POINT('Ctrl Pts',(0.611789196225796,110.237792164568,10.8731521926038));
#42231=CARTESIAN_POINT('Ctrl Pts',(0.527024854495964,110.222488069096,10.8536110550817));
#42232=CARTESIAN_POINT('Ctrl Pts',(0.441234528753111,110.20724710615,10.8384635423577));
#42233=CARTESIAN_POINT('Ctrl Pts',(0.417057286598754,110.202951931274,10.8341947034181));
#42234=CARTESIAN_POINT('Ctrl Pts',(0.392798569153779,110.198661898692,10.8302750711374));
#42235=CARTESIAN_POINT('Ctrl Pts',(0.368466654843724,110.194375653523,10.826706696421));
#42236=CARTESIAN_POINT('Ctrl Pts',(0.282443181651797,110.179221987779,10.8140910023639));
#42237=CARTESIAN_POINT('Ctrl Pts',(0.19595745502032,110.164192193344,10.8059297038895));
#42238=CARTESIAN_POINT('Ctrl Pts',(0.109387378581065,110.149245055312,10.8021945677738));
#42239=CARTESIAN_POINT('Ctrl Pts',(0.0220758111051781,110.134169891877,
10.7984274394264));
#42240=CARTESIAN_POINT('Ctrl Pts',(-0.0653219079878356,110.119178777285,
10.7991625921094));
#42241=CARTESIAN_POINT('Ctrl Pts',(-0.152435635049384,110.104255973227,
10.8044063858373));
#42242=CARTESIAN_POINT('Ctrl Pts',(-0.238684278608216,110.089481360184,
10.8095981060334));
#42243=CARTESIAN_POINT('Ctrl Pts',(-0.324654979384985,110.074773830453,
10.8192092014915));
#42244=CARTESIAN_POINT('Ctrl Pts',(-0.409999891052358,110.060143180545,
10.8332816511376));
#42245=CARTESIAN_POINT('Ctrl Pts',(-0.4809571128161,110.047979007546,10.8449817268748));
#42246=CARTESIAN_POINT('Ctrl Pts',(-0.551482154344233,110.03586847296,10.8597662429117));
#42247=CARTESIAN_POINT('Ctrl Pts',(-0.621377267313918,110.023829482762,
10.877680368726));
#42248=CARTESIAN_POINT('Ctrl Pts',(-0.63996173885094,110.020628425332,10.8824435710039));
#42249=CARTESIAN_POINT('Ctrl Pts',(-0.658480264399054,110.017436224663,
10.8874226251331));
#42250=CARTESIAN_POINT('Ctrl Pts',(-0.676929533158853,110.014253319914,
10.8926171017569));
#42251=CARTESIAN_POINT('Ctrl Pts',(-0.759203825065035,110.000059194509,
10.9157818077194));
#42252=CARTESIAN_POINT('Ctrl Pts',(-0.840100886012136,109.986048767545,
10.9432268422863));
#42253=CARTESIAN_POINT('Ctrl Pts',(-0.919344599337146,109.972139976636,
10.974720389118));
#42254=CARTESIAN_POINT('Ctrl Pts',(-0.999967450718988,109.957989120558,
11.0067620418771));
#42255=CARTESIAN_POINT('Ctrl Pts',(-1.07887934449036,109.943943116139,11.0429950496292));
#42256=CARTESIAN_POINT('Ctrl Pts',(-1.1557750062517,109.929936373207,11.083214494394));
#42257=CARTESIAN_POINT('Ctrl Pts',(-1.23323378236241,109.915827057545,11.1237284700328));
#42258=CARTESIAN_POINT('Ctrl Pts',(-1.30864686734369,109.901757368578,11.1682879839491));
#42259=CARTESIAN_POINT('Ctrl Pts',(-1.38168314252135,109.887685442195,11.2167136948761));
#42260=CARTESIAN_POINT('Ctrl Pts',(-1.4264895574882,109.879052573509,11.2464219801574));
#42261=CARTESIAN_POINT('Ctrl Pts',(-1.4704010521126,109.870419374408,11.2775858824778));
#42262=CARTESIAN_POINT('Ctrl Pts',(-1.51333730239647,109.861781232391,11.3101686399619));
#42263=CARTESIAN_POINT('Ctrl Pts',(-1.58329352947783,109.847707068475,11.3632558743251));
#42264=CARTESIAN_POINT('Ctrl Pts',(-1.65029388636087,109.833693403166,11.419828104897));
#42265=CARTESIAN_POINT('Ctrl Pts',(-1.71407378502022,109.819743665232,11.4796389819029));
#42266=CARTESIAN_POINT('Ctrl Pts',(-1.77788889059502,109.805786226951,11.5394828748986));
#42267=CARTESIAN_POINT('Ctrl Pts',(-1.83848059659025,109.791893020877,11.6025689225187));
#42268=CARTESIAN_POINT('Ctrl Pts',(-1.89558038405761,109.778091251272,11.6686926200149));
#42269=CARTESIAN_POINT('Ctrl Pts',(-1.93576271336663,109.768378653802,11.7152252658578));
#42270=CARTESIAN_POINT('Ctrl Pts',(-1.97421575088245,109.758711851372,11.7632631138));
#42271=CARTESIAN_POINT('Ctrl Pts',(-2.01084182042605,109.749106280255,11.8127476638983));
#42272=CARTESIAN_POINT('Ctrl Pts',(-2.06270050352498,109.735505796372,11.8828126103645));
#42273=CARTESIAN_POINT('Ctrl Pts',(-2.11089855002028,109.722027164445,11.9557779476345));
#42274=CARTESIAN_POINT('Ctrl Pts',(-2.15524570805872,109.708587080166,12.0313151593601));
#42275=CARTESIAN_POINT('Ctrl Pts',(-2.15963214624348,109.707257703009,12.0387866485049));
#42276=CARTESIAN_POINT('Ctrl Pts',(-2.16398087591946,109.705928721963,12.0462833028258));
#42277=CARTESIAN_POINT('Ctrl Pts',(-2.16829169123313,109.704600069358,12.0538048056359));
#42278=CARTESIAN_POINT('Ctrl Pts',(-2.21145628653423,109.691296147059,12.1291183139242));
#42279=CARTESIAN_POINT('Ctrl Pts',(-2.25059811686777,109.678091178631,12.2065321513085));
#42280=CARTESIAN_POINT('Ctrl Pts',(-2.28561957442646,109.664932737475,12.2856685751055));
#42281=CARTESIAN_POINT('Ctrl Pts',(-2.32106659166802,109.651614402858,12.365766617115));
#42282=CARTESIAN_POINT('Ctrl Pts',(-2.35229235428514,109.638343638471,12.4476295826256));
#42283=CARTESIAN_POINT('Ctrl Pts',(-2.37917363327936,109.6250968897,12.5308869451382));
#42284=CARTESIAN_POINT('Ctrl Pts',(-2.40595432564599,109.611899708726,12.6138327682587));
#42285=CARTESIAN_POINT('Ctrl Pts',(-2.4284230937876,109.598726455936,12.6981626291549));
#42286=CARTESIAN_POINT('Ctrl Pts',(-2.4464367953254,109.585584108856,12.7835290813987));
#42287=CARTESIAN_POINT('Ctrl Pts',(-2.45800778408427,109.577142204232,12.8383636892235));
#42288=CARTESIAN_POINT('Ctrl Pts',(-2.46774018617838,109.568713666937,12.8936263828342));
#42289=CARTESIAN_POINT('Ctrl Pts',(-2.47559063569568,109.560306591779,12.9492290970707));
#42290=CARTESIAN_POINT('Ctrl Pts',(-2.47775855570292,109.557984958299,12.9645839167385));
#42291=CARTESIAN_POINT('Ctrl Pts',(-2.47978290586993,109.555664992123,12.9799646820784));
#42292=CARTESIAN_POINT('Ctrl Pts',(-2.4816630983293,109.553346874686,12.9953658093138));
#42293=CARTESIAN_POINT('Ctrl Pts',(-2.49395830740612,109.538187927313,13.0960789455856));
#42294=CARTESIAN_POINT('Ctrl Pts',(-2.50004583450027,109.523164566333,13.1972739658029));
#42295=CARTESIAN_POINT('Ctrl Pts',(-2.50004052090194,109.508185544341,13.2983771895099));
#42296=CARTESIAN_POINT('Origin',(0.,70.2,13.3));
#42297=CARTESIAN_POINT('',(-2.5,107.398963164072,13.3));
#42298=CARTESIAN_POINT('',(-2.5,108.597702566458,13.299999999993));
#42299=CARTESIAN_POINT('',(-2.5,70.2,13.3));
#42300=CARTESIAN_POINT('',(-2.49999996234878,108.597761318563,13.2995661151097));
#42301=CARTESIAN_POINT('Ctrl Pts',(-2.5,108.597702566458,13.2999999999859));
#42302=CARTESIAN_POINT('Ctrl Pts',(-2.5,108.597723045119,13.2998487659079));
#42303=CARTESIAN_POINT('Ctrl Pts',(-2.49999998745624,108.597742181868,13.2997074408026));
#42304=CARTESIAN_POINT('Ctrl Pts',(-2.4999999606093,108.597762660402,13.2995562055454));
#42305=CARTESIAN_POINT('Ctrl Pts',(-2.49999996234878,108.597761318563,13.2995661151097));
#42306=CARTESIAN_POINT('Ctrl Pts',(-2.49996127400753,108.627272326748,13.0816254657993));
#42307=CARTESIAN_POINT('Ctrl Pts',(-2.47142480948102,108.656429210505,12.8646035671895));
#42308=CARTESIAN_POINT('Ctrl Pts',(-2.35878302773443,108.715080836125,12.4434629014955));
#42309=CARTESIAN_POINT('Ctrl Pts',(-2.27515727800989,108.744218171731,12.2411369514137));
#42310=CARTESIAN_POINT('Ctrl Pts',(-2.00804038715987,108.815466700751,11.7773812837939));
#42311=CARTESIAN_POINT('Ctrl Pts',(-1.79885867136011,108.857325226278,11.5351391029824));
#42312=CARTESIAN_POINT('Ctrl Pts',(-1.41973717840134,108.921060982191,11.2355641456908));
#42313=CARTESIAN_POINT('Ctrl Pts',(-1.27957677521832,108.942797951022,11.1458790846607));
#42314=CARTESIAN_POINT('Ctrl Pts',(-0.986031723585365,108.986018769111,
10.9968767095871));
#42315=CARTESIAN_POINT('Ctrl Pts',(-0.833613895820597,109.007394625194,
10.9374322248134));
#42316=CARTESIAN_POINT('Ctrl Pts',(-0.518255591179365,109.050243261842,
10.8487906492423));
#42317=CARTESIAN_POINT('Ctrl Pts',(-0.356013778143492,109.071585227966,
10.8200251510171));
#42318=CARTESIAN_POINT('Ctrl Pts',(-0.0310359412977735,109.113974241321,
10.7949773096619));
#42319=CARTESIAN_POINT('Ctrl Pts',(0.130877516573796,109.134921306702,10.7982053575935));
#42320=CARTESIAN_POINT('Ctrl Pts',(0.623673653758929,109.199183677247,10.8560294543235));
#42321=CARTESIAN_POINT('Ctrl Pts',(0.94483595807269,109.241569698108,10.9613507794186));
#42322=CARTESIAN_POINT('Ctrl Pts',(1.37356403589125,109.304782593515,11.2051359347462));
#42323=CARTESIAN_POINT('Ctrl Pts',(1.50361457831467,109.325059272149,11.2964334774443));
#42324=CARTESIAN_POINT('Ctrl Pts',(1.87842726030939,109.388089661664,11.6167319908891));
#42325=CARTESIAN_POINT('Ctrl Pts',(2.08655389220884,109.430035043802,11.8828873049376));
#42326=CARTESIAN_POINT('Ctrl Pts',(2.30710833395787,109.492416408326,12.3240707169627));
#42327=CARTESIAN_POINT('Ctrl Pts',(2.36439699616986,109.512421640674,12.472463658104));
#42328=CARTESIAN_POINT('Ctrl Pts',(2.49719917562092,109.574437830974,12.9462728999172));
#42329=CARTESIAN_POINT('Ctrl Pts',(2.52207078606059,109.615761043397,13.2820615962384));
#42330=CARTESIAN_POINT('Ctrl Pts',(2.46015235542664,109.677429094164,13.772962846743));
#42331=CARTESIAN_POINT('Ctrl Pts',(2.42450068824604,109.697451690676,13.9307479769561));
#42332=CARTESIAN_POINT('Ctrl Pts',(2.26886088138479,109.759062269446,14.4020150172217));
#42333=CARTESIAN_POINT('Ctrl Pts',(2.10098182948669,109.800109140089,14.6957355776455));
#42334=CARTESIAN_POINT('Ctrl Pts',(1.68267620470091,109.878046746828,15.1730827795599));
#42335=CARTESIAN_POINT('Ctrl Pts',(1.44618714468181,109.914280049486,15.3611640261789));
#42336=CARTESIAN_POINT('Ctrl Pts',(1.03611523545117,109.97105894972,15.5812048451219));
#42337=CARTESIAN_POINT('Ctrl Pts',(0.882749733962537,109.991209696826,15.6448214532444));
#42338=CARTESIAN_POINT('Ctrl Pts',(0.577555683805002,110.029900944934,15.7371929611169));
#42339=CARTESIAN_POINT('Ctrl Pts',(0.427113075503393,110.048367266475,15.7680074854576));
#42340=CARTESIAN_POINT('Ctrl Pts',(0.116823992327557,110.085886237418,15.8023209407108));
#42341=CARTESIAN_POINT('Ctrl Pts',(-0.0424516464144428,110.104848827156,
15.8046874082007));
#42342=CARTESIAN_POINT('Ctrl Pts',(-0.534757737709349,110.163928021299,
15.7650022335554));
#42343=CARTESIAN_POINT('Ctrl Pts',(-0.859875376778409,110.203875710064,
15.6712549565493));
#42344=CARTESIAN_POINT('Ctrl Pts',(-1.43277381060917,110.280367266776,15.3722037298678));
#42345=CARTESIAN_POINT('Ctrl Pts',(-1.67938483606652,110.316287342787,15.1779110623556));
#42346=CARTESIAN_POINT('Ctrl Pts',(-2.09144447462872,110.390048498595,14.7055117149096));
#42347=CARTESIAN_POINT('Ctrl Pts',(-2.25203633660929,110.426789327045,14.4304877623833));
#42348=CARTESIAN_POINT('Ctrl Pts',(-2.40975463661823,110.481207127063,13.984080209621));
#42349=CARTESIAN_POINT('Ctrl Pts',(-2.44810946395696,110.499150595612,13.8307031217425));
#42350=CARTESIAN_POINT('Ctrl Pts',(-2.49060203845772,110.531575425718,13.5504203653099));
#42351=CARTESIAN_POINT('Ctrl Pts',(-2.5,110.545997076194,13.4251542520052));
#42352=CARTESIAN_POINT('Ctrl Pts',(-2.5,110.560415842511,13.3));
#42353=CARTESIAN_POINT('Ctrl Pts',(-2.49999946874101,109.50813782114,13.2983701856957));
#42354=CARTESIAN_POINT('Ctrl Pts',(-2.50014743099999,109.47470183367,13.5253319738356));
#42355=CARTESIAN_POINT('Ctrl Pts',(-2.46938886651776,109.440797156689,13.7512018334646));
#42356=CARTESIAN_POINT('Ctrl Pts',(-2.36318482247125,109.382484222952,14.1331322874585));
#42357=CARTESIAN_POINT('Ctrl Pts',(-2.30127816868861,109.358753517347,14.2914353476029));
#42358=CARTESIAN_POINT('Ctrl Pts',(-2.07118790625412,109.290656635913,14.7392882519759));
#42359=CARTESIAN_POINT('Ctrl Pts',(-1.86090928673608,109.247048972379,15.0024460208004));
#42360=CARTESIAN_POINT('Ctrl Pts',(-1.35980338407567,109.153226386204,15.4221056702417));
#42361=CARTESIAN_POINT('Ctrl Pts',(-1.07736098827051,109.104562298503,15.5784834082954));
#42362=CARTESIAN_POINT('Ctrl Pts',(-0.479117324911624,109.012092543446,
15.7730932116796));
#42363=CARTESIAN_POINT('Ctrl Pts',(-0.169891597185701,108.971233355369,
15.8133531162263));
#42364=CARTESIAN_POINT('Ctrl Pts',(0.297431111595153,108.906425226583,15.7873004866538));
#42365=CARTESIAN_POINT('Ctrl Pts',(0.454547365927925,108.884460358984,15.7634386301251));
#42366=CARTESIAN_POINT('Ctrl Pts',(0.767729463762711,108.840092224318,15.6848675151351));
#42367=CARTESIAN_POINT('Ctrl Pts',(0.922787692247484,108.817669590434,15.6292634571929));
#42368=CARTESIAN_POINT('Ctrl Pts',(1.2187766126299,108.772826789759,15.4888892061383));
#42369=CARTESIAN_POINT('Ctrl Pts',(1.35908275732209,108.750560573587,15.4046496363571));
#42370=CARTESIAN_POINT('Ctrl Pts',(1.75766305512708,108.682865954791,15.1087570784973));
#42371=CARTESIAN_POINT('Ctrl Pts',(1.9827987061679,108.638676048485,14.858694122639));
#42372=CARTESIAN_POINT('Ctrl Pts',(2.23407575843589,108.572044204741,14.4334636244901));
#42373=CARTESIAN_POINT('Ctrl Pts',(2.30231004488894,108.55030637558,14.2875230706927));
#42374=CARTESIAN_POINT('Ctrl Pts',(2.40924604020111,108.507167369673,13.9861680929474));
#42375=CARTESIAN_POINT('Ctrl Pts',(2.44801163505166,108.485966866797,13.8315454927465));
#42376=CARTESIAN_POINT('Ctrl Pts',(2.51860834899393,108.423068640535,13.3653015499732));
#42377=CARTESIAN_POINT('Ctrl Pts',(2.50705167997413,108.381664188897,13.0502553988117));
#42378=CARTESIAN_POINT('Ctrl Pts',(2.4005401620259,108.31816355143,12.5820011505177));
#42379=CARTESIAN_POINT('Ctrl Pts',(2.34699396469652,108.296160270614,12.4226532248292));
#42380=CARTESIAN_POINT('Ctrl Pts',(2.15206948111612,108.233728377247,11.9916235638509));
#42381=CARTESIAN_POINT('Ctrl Pts',(1.97630606161899,108.193578333358,11.7387499853495));
#42382=CARTESIAN_POINT('Ctrl Pts',(1.53221773170734,108.111950150126,11.2988824867021));
#42383=CARTESIAN_POINT('Ctrl Pts',(1.26407436406757,108.070456391872,11.1195683870759));
#42384=CARTESIAN_POINT('Ctrl Pts',(0.824114986157931,108.008260926605,10.9344777583247));
#42385=CARTESIAN_POINT('Ctrl Pts',(0.673313458835044,107.987932630849,10.8872181441702));
#42386=CARTESIAN_POINT('Ctrl Pts',(0.194063553655871,107.92465414115,10.7854985471525));
#42387=CARTESIAN_POINT('Ctrl Pts',(-0.141442500289415,107.882026430039,
10.7819903818547));
#42388=CARTESIAN_POINT('Ctrl Pts',(-0.627082419382444,107.818166943961,
10.8744986208313));
#42389=CARTESIAN_POINT('Ctrl Pts',(-0.783030632525979,107.797270221791,
10.9202620179646));
#42390=CARTESIAN_POINT('Ctrl Pts',(-1.13257268861168,107.748631656285,11.0609479751009));
#42391=CARTESIAN_POINT('Ctrl Pts',(-1.32058333814669,107.721062016685,11.1664198722666));
#42392=CARTESIAN_POINT('Ctrl Pts',(-1.60728945842999,107.675792686956,11.3798476374749));
#42393=CARTESIAN_POINT('Ctrl Pts',(-1.71426404682308,107.657941223723,11.4747135352435));
#42394=CARTESIAN_POINT('Ctrl Pts',(-1.90423831957223,107.623402092554,11.6747019854949));
#42395=CARTESIAN_POINT('Ctrl Pts',(-1.98805520560998,107.606773674294,11.7783719607084));
#42396=CARTESIAN_POINT('Ctrl Pts',(-2.14135866623276,107.572660840051,12.0024138083965));
#42397=CARTESIAN_POINT('Ctrl Pts',(-2.20987733010779,107.555228240195,12.1228920186611));
#42398=CARTESIAN_POINT('Ctrl Pts',(-2.40063239072227,107.497679759308,12.5343124453017));
#42399=CARTESIAN_POINT('Ctrl Pts',(-2.47793576315712,107.457483744812,12.8427016530759));
#42400=CARTESIAN_POINT('Ctrl Pts',(-2.49864139718994,107.41110563653,13.2048244838333));
#42401=CARTESIAN_POINT('Ctrl Pts',(-2.5,107.405028168214,13.252414849999));
#42402=CARTESIAN_POINT('Ctrl Pts',(-2.5,107.398963164072,13.3));
#42403=CARTESIAN_POINT('Origin',(0.,70.2,13.3));
#42404=CARTESIAN_POINT('',(-2.5,105.533497732924,13.3000000000002));
#42405=CARTESIAN_POINT('',(-2.50000333388702,106.437958303058,13.3001965898202));
#42406=CARTESIAN_POINT('',(-2.5,70.2,13.3));
#42407=CARTESIAN_POINT('',(1.45735612640718,107.079506406801,11.2679629878995));
#42408=CARTESIAN_POINT('Ctrl Pts',(-2.49999999227335,106.437958007126,13.3001965534331));
#42409=CARTESIAN_POINT('Ctrl Pts',(-2.50001798642019,106.465898559144,13.0713256237538));
#42410=CARTESIAN_POINT('Ctrl Pts',(-2.46860680580814,106.493594969784,12.8435143817534));
#42411=CARTESIAN_POINT('Ctrl Pts',(-2.34842960455445,106.547184092487,12.4162042342614));
#42412=CARTESIAN_POINT('Ctrl Pts',(-2.26377157410827,106.572863318266,12.2176117785873));
#42413=CARTESIAN_POINT('Ctrl Pts',(-2.07813421178431,106.616731300532,11.902077945352));
#42414=CARTESIAN_POINT('Ctrl Pts',(-1.98986892198254,106.63477730416,11.7790615650358));
#42415=CARTESIAN_POINT('Ctrl Pts',(-1.68153582826976,106.690900301041,11.4224960813028));
#42416=CARTESIAN_POINT('Ctrl Pts',(-1.42740292158903,106.728163934818,11.2227080745087));
#42417=CARTESIAN_POINT('Ctrl Pts',(-0.995223984362087,106.785184092776,
11.0006671495818));
#42418=CARTESIAN_POINT('Ctrl Pts',(-0.840824854642511,106.804547713125,
10.9398258010325));
#42419=CARTESIAN_POINT('Ctrl Pts',(-0.382829581973324,106.859949198179,
10.8100535828494));
#42420=CARTESIAN_POINT('Ctrl Pts',(-0.0709278463260396,106.895164958428,
10.781787400615));
#42421=CARTESIAN_POINT('Ctrl Pts',(0.465570512213512,106.956956057592,10.8331351265117));
#42422=CARTESIAN_POINT('Ctrl Pts',(0.688930644507382,106.98296512778,10.8859626872702));
#42423=CARTESIAN_POINT('Ctrl Pts',(1.09893413324957,107.032530831421,11.0445790864913));
#42424=CARTESIAN_POINT('Ctrl Pts',(1.2854182595164,107.05593391797,11.1454026727805));
#42425=CARTESIAN_POINT('Ctrl Pts',(1.45701176931329,107.079469279784,11.2684693691498));
#42426=CARTESIAN_POINT('Ctrl Pts',(1.45691314277681,107.080279081049,11.2683986379203));
#42427=CARTESIAN_POINT('Ctrl Pts',(1.62602378470569,107.115794291604,11.389672191585));
#42428=CARTESIAN_POINT('Ctrl Pts',(1.7793776066286,107.15046473624,11.5316147053649));
#42429=CARTESIAN_POINT('Ctrl Pts',(2.05462324138204,107.22120768442,11.8589364513814));
#42430=CARTESIAN_POINT('Ctrl Pts',(2.17314512138307,107.257330168275,12.0447646756983));
#42431=CARTESIAN_POINT('Ctrl Pts',(2.40216586590629,107.345457840436,12.5360399190128));
#42432=CARTESIAN_POINT('Ctrl Pts',(2.48063478144839,107.395677705901,12.8520967298161));
#42433=CARTESIAN_POINT('Ctrl Pts',(2.5130889845337,107.49750342118,13.4974568467129));
#42434=CARTESIAN_POINT('Ctrl Pts',(2.46650567299891,107.546631730194,13.8206323311975));
#42435=CARTESIAN_POINT('Ctrl Pts',(2.25539462242128,107.644707133605,14.4236686416826));
#42436=CARTESIAN_POINT('Ctrl Pts',(2.09580227720739,107.691798446146,14.6989862592695));
#42437=CARTESIAN_POINT('Ctrl Pts',(1.68105237624616,107.786334762015,15.1775017715823));
#42438=CARTESIAN_POINT('Ctrl Pts',(1.42903676626015,107.832842343291,15.375786349681));
#42439=CARTESIAN_POINT('Ctrl Pts',(0.849619493980127,107.928189837091,15.6748306721696));
#42440=CARTESIAN_POINT('Ctrl Pts',(0.524851876498055,107.97624700749,15.7670445384718));
#42441=CARTESIAN_POINT('Ctrl Pts',(-0.13419844394631,108.070733519944,15.8176769949132));
#42442=CARTESIAN_POINT('Ctrl Pts',(-0.461719755941352,108.117147165353,
15.7786256839406));
#42443=CARTESIAN_POINT('Ctrl Pts',(-1.08299346969568,108.209251354498,15.5767776770374));
#42444=CARTESIAN_POINT('Ctrl Pts',(-1.37080309473312,108.254946622623,15.4160212472238));
#42445=CARTESIAN_POINT('Ctrl Pts',(-1.74653250618216,108.323596181201,15.0964960092678));
#42446=CARTESIAN_POINT('Ctrl Pts',(-1.86238445182696,108.346567621202,14.9760981856762));
#42447=CARTESIAN_POINT('Ctrl Pts',(-2.13505286930052,108.407606029766,14.6292511053334));
#42448=CARTESIAN_POINT('Ctrl Pts',(-2.26803346760061,108.445269726053,14.386932257422));
#42449=CARTESIAN_POINT('Ctrl Pts',(-2.45230623455293,108.521241908179,13.8618389889636));
#42450=CARTESIAN_POINT('Ctrl Pts',(-2.50000000000159,108.559525276668,13.5819377266705));
#42451=CARTESIAN_POINT('Ctrl Pts',(-2.5,108.597702566458,13.2999999999859));
#42452=CARTESIAN_POINT('Ctrl Pts',(-2.5,107.398963164072,13.3));
#42453=CARTESIAN_POINT('Ctrl Pts',(-2.5,107.388587973973,13.3814022489794));
#42454=CARTESIAN_POINT('Ctrl Pts',(-2.49602417443423,107.378253537848,13.462789778904));
#42455=CARTESIAN_POINT('Ctrl Pts',(-2.47821031759599,107.355161879218,13.6445350202945));
#42456=CARTESIAN_POINT('Ctrl Pts',(-2.46224293867941,107.342441498577,13.7445140910394));
#42457=CARTESIAN_POINT('Ctrl Pts',(-2.41181399250324,107.313307970256,13.9710369640909));
#42458=CARTESIAN_POINT('Ctrl Pts',(-2.37337316566617,107.29695349493,14.0963916290613));
#42459=CARTESIAN_POINT('Ctrl Pts',(-2.2813654615178,107.265649596051,14.3294058349301));
#42460=CARTESIAN_POINT('Ctrl Pts',(-2.22951262688311,107.25074202421,14.4373561312345));
#42461=CARTESIAN_POINT('Ctrl Pts',(-2.07417327432608,107.211714841503,14.7089580026402));
#42462=CARTESIAN_POINT('Ctrl Pts',(-1.95907952149779,107.187708358492,14.865045300933));
#42463=CARTESIAN_POINT('Ctrl Pts',(-1.67039468351634,107.135041185485,15.1741757722895));
#42464=CARTESIAN_POINT('Ctrl Pts',(-1.49124220078996,107.106610164872,15.3196416303595));
#42465=CARTESIAN_POINT('Ctrl Pts',(-1.04993368060304,107.042470588755,15.5868208327022));
#42466=CARTESIAN_POINT('Ctrl Pts',(-0.781452470515746,107.00715018963,15.6919146642682));
#42467=CARTESIAN_POINT('Ctrl Pts',(-0.200041920490081,106.933773294451,
15.8108508768705));
#42468=CARTESIAN_POINT('Ctrl Pts',(0.10974706912583,106.896361534273,15.8164168905719));
#42469=CARTESIAN_POINT('Ctrl Pts',(0.716563545998488,106.820564402393,15.7148315686896));
#42470=CARTESIAN_POINT('Ctrl Pts',(1.00837663178938,106.782922632074,15.6082628215899));
#42471=CARTESIAN_POINT('Ctrl Pts',(1.55683602445739,106.70510839167,15.2836056075017));
#42472=CARTESIAN_POINT('Ctrl Pts',(1.804287188546,106.665485186369,15.0615259766754));
#42473=CARTESIAN_POINT('Ctrl Pts',(2.17104976337721,106.590690820608,14.5714349524458));
#42474=CARTESIAN_POINT('Ctrl Pts',(2.30089102815796,106.556612477708,14.3178170038338));
#42475=CARTESIAN_POINT('Ctrl Pts',(2.43296860039397,106.503752799261,13.8965039837913));
#42476=CARTESIAN_POINT('Ctrl Pts',(2.46590292276778,106.484922098114,13.7409956117158));
#42477=CARTESIAN_POINT('Ctrl Pts',(2.52171257568214,106.426112166352,13.251876296912));
#42478=CARTESIAN_POINT('Ctrl Pts',(2.49278335522221,106.386359418917,12.9160821442861));
#42479=CARTESIAN_POINT('Ctrl Pts',(2.31119325403085,106.309567356957,12.2974392628104));
#42480=CARTESIAN_POINT('Ctrl Pts',(2.16865671539812,106.27323487974,12.0179348538109));
#42481=CARTESIAN_POINT('Ctrl Pts',(1.87727006989814,106.216993599097,11.6406986597147));
#42482=CARTESIAN_POINT('Ctrl Pts',(1.76326224051283,106.197451366672,11.5200185245298));
#42483=CARTESIAN_POINT('Ctrl Pts',(1.4062358441955,106.141937833872,11.2103203415651));
#42484=CARTESIAN_POINT('Ctrl Pts',(1.13919984286605,106.106598416615,11.0535522118528));
#42485=CARTESIAN_POINT('Ctrl Pts',(0.705936943052217,106.053440846938,10.8968226522371));
#42486=CARTESIAN_POINT('Ctrl Pts',(0.556949731090647,106.035801919639,10.8579907344719));
#42487=CARTESIAN_POINT('Ctrl Pts',(0.0972717715450301,105.981491291937,
10.7824586441877));
#42488=CARTESIAN_POINT('Ctrl Pts',(-0.217687028212233,105.944831568633,
10.7899816313777));
#42489=CARTESIAN_POINT('Ctrl Pts',(-0.808106094379333,105.876435302433,
10.9163297644695));
#42490=CARTESIAN_POINT('Ctrl Pts',(-1.0801857468759,105.845039753081,11.0266526925972));
#42491=CARTESIAN_POINT('Ctrl Pts',(-1.61218472171108,105.774757757908,11.3598969928922));
#42492=CARTESIAN_POINT('Ctrl Pts',(-1.8583483329386,105.735794988364,11.5941963304945));
#42493=CARTESIAN_POINT('Ctrl Pts',(-2.21631095716883,105.666924364116,12.1076374659539));
#42494=CARTESIAN_POINT('Ctrl Pts',(-2.33932955088605,105.636981418308,12.3719473583166));
#42495=CARTESIAN_POINT('Ctrl Pts',(-2.47134358727144,105.582009656608,12.8633873336436));
#42496=CARTESIAN_POINT('Ctrl Pts',(-2.5,105.557440002256,13.0814498945321));
#42497=CARTESIAN_POINT('Ctrl Pts',(-2.5,105.533497732924,13.3000000000004));
#42498=CARTESIAN_POINT('Origin',(0.,70.2,13.3));
#42499=CARTESIAN_POINT('',(-2.50003871369437,103.603837493162,13.2999999833246));
#42500=CARTESIAN_POINT('',(-2.5,104.491842419534,13.3));
#42501=CARTESIAN_POINT('',(-2.5,70.2,13.3));
#42502=CARTESIAN_POINT('',(-0.0771081494294188,104.870757121609,10.8023559268293));
#42503=CARTESIAN_POINT('Ctrl Pts',(-2.5,104.491842419534,13.3));
#42504=CARTESIAN_POINT('Ctrl Pts',(-2.5,104.515014746024,13.0770988191812));
#42505=CARTESIAN_POINT('Ctrl Pts',(-2.47018808345436,104.537763921925,12.8547935006237));
#42506=CARTESIAN_POINT('Ctrl Pts',(-2.36817301427408,104.578231563052,12.4826513121143));
#42507=CARTESIAN_POINT('Ctrl Pts',(-2.31017230605444,104.595256815441,12.3307634735551));
#42508=CARTESIAN_POINT('Ctrl Pts',(-2.10833292898536,104.641830880163,11.9254613436518));
#42509=CARTESIAN_POINT('Ctrl Pts',(-1.93445262603939,104.669970953774,11.6899135363534));
#42510=CARTESIAN_POINT('Ctrl Pts',(-1.48578658328471,104.730245552284,11.262700707031));
#42511=CARTESIAN_POINT('Ctrl Pts',(-1.20518080907228,104.763270768522,11.0851054799438));
#42512=CARTESIAN_POINT('Ctrl Pts',(-0.635850580826999,104.820912496787,
10.8659274407985));
#42513=CARTESIAN_POINT('Ctrl Pts',(-0.358400677651412,104.84553105741,10.8099051765678));
#42514=CARTESIAN_POINT('Ctrl Pts',(-0.0774247329654312,104.870995320611,
10.8011992054737));
#42515=CARTESIAN_POINT('Ctrl Pts',(-0.0767123097838143,104.870816751188,
10.8022856266005));
#42516=CARTESIAN_POINT('Ctrl Pts',(-0.0223177348150291,104.878477929272,
10.8001035155528));
#42517=CARTESIAN_POINT('Ctrl Pts',(0.0320873656158203,104.886295266453,
10.7999829501676));
#42518=CARTESIAN_POINT('Ctrl Pts',(0.0863615600831533,104.894160010526,
10.8017387475656));
#42519=CARTESIAN_POINT('Ctrl Pts',(0.120678810323465,104.899132841409,10.8028489278138));
#42520=CARTESIAN_POINT('Ctrl Pts',(0.154944755651476,104.904124748766,10.8047090968772));
#42521=CARTESIAN_POINT('Ctrl Pts',(0.189134306212569,104.909109517031,10.8072718680335));
#42522=CARTESIAN_POINT('Ctrl Pts',(0.269346731325135,104.920804328593,10.8132844094704));
#42523=CARTESIAN_POINT('Ctrl Pts',(0.349139807491138,104.932459741272,10.8231604950264));
#42524=CARTESIAN_POINT('Ctrl Pts',(0.428273375004075,104.944050329601,10.8368704813559));
#42525=CARTESIAN_POINT('Ctrl Pts',(0.436481208700324,104.945252520081,10.8382924984759));
#42526=CARTESIAN_POINT('Ctrl Pts',(0.444681975098596,104.946454016347,10.8397557979769));
#42527=CARTESIAN_POINT('Ctrl Pts',(0.452875424696013,104.94765479224,10.8412603731459));
#42528=CARTESIAN_POINT('Ctrl Pts',(0.478581129502685,104.951422044393,10.8459807494289));
#42529=CARTESIAN_POINT('Ctrl Pts',(0.504214836405781,104.955182106315,10.8511071745682));
#42530=CARTESIAN_POINT('Ctrl Pts',(0.529769172972489,104.958933982361,10.8566393738351));
#42531=CARTESIAN_POINT('Ctrl Pts',(0.529797434998153,104.958938131779,10.8566454922158));
#42532=CARTESIAN_POINT('Ctrl Pts',(0.52982569692664,104.958942281187,10.8566516110931));
#42533=CARTESIAN_POINT('Ctrl Pts',(0.529853958757947,104.958946430585,10.8566577304671));
#42534=CARTESIAN_POINT('Ctrl Pts',(0.609649687591697,104.970662028134,10.8739354470389));
#42535=CARTESIAN_POINT('Ctrl Pts',(0.688673893735166,104.982299532234,10.8951699354422));
#42536=CARTESIAN_POINT('Ctrl Pts',(0.766635019018041,104.993914622409,10.9202985827422));
#42537=CARTESIAN_POINT('Ctrl Pts',(0.77264163974443,104.994809522799,10.9222346534845));
#42538=CARTESIAN_POINT('Ctrl Pts',(0.778641930049558,104.995704288225,10.9241938566037));
#42539=CARTESIAN_POINT('Ctrl Pts',(0.784635746401502,104.996598943195,10.926176171165));
#42540=CARTESIAN_POINT('Ctrl Pts',(0.826373752028617,105.002828882849,10.9399800402623));
#42541=CARTESIAN_POINT('Ctrl Pts',(0.867798332419425,105.009053175507,10.9549038079222));
#42542=CARTESIAN_POINT('Ctrl Pts',(0.908860953515595,105.015278002027,10.9709380285799));
#42543=CARTESIAN_POINT('Ctrl Pts',(0.991712109179066,105.027837698833,11.0032899261498));
#42544=CARTESIAN_POINT('Ctrl Pts',(1.07264720441223,105.040334468887,11.039989888498));
#42545=CARTESIAN_POINT('Ctrl Pts',(1.15131842734291,105.052799988542,11.0808198028244));
#42546=CARTESIAN_POINT('Ctrl Pts',(1.22998965027359,105.065265508198,11.1216497171509));
#42547=CARTESIAN_POINT('Ctrl Pts',(1.3063963941909,105.07769946929,11.1666090994476));
#42548=CARTESIAN_POINT('Ctrl Pts',(1.3802058218432,105.09010954104,11.2154881414483));
#42549=CARTESIAN_POINT('Ctrl Pts',(1.38021285402431,105.090110723407,11.215492798391));
#42550=CARTESIAN_POINT('Ctrl Pts',(1.38021988618185,105.090111905775,11.2154974553693));
#42551=CARTESIAN_POINT('Ctrl Pts',(1.38022691831581,105.090113088142,11.2155021123832));
#42552=CARTESIAN_POINT('Ctrl Pts',(1.45391807892792,105.102503353383,11.2643039077924));
#42553=CARTESIAN_POINT('Ctrl Pts',(1.52502286575103,105.114869774911,11.3170138546018));
#42554=CARTESIAN_POINT('Ctrl Pts',(1.59323035299045,105.127242949573,11.3734193901038));
#42555=CARTESIAN_POINT('Ctrl Pts',(1.64632972673284,105.136875437915,11.417330971251));
#42556=CARTESIAN_POINT('Ctrl Pts',(1.69767277560963,105.146511559921,11.4634822423969));
#42557=CARTESIAN_POINT('Ctrl Pts',(1.74710941870683,105.156157570951,11.5117740752752));
#42558=CARTESIAN_POINT('Ctrl Pts',(1.81048733976164,105.168523785306,11.5736843462808));
#42559=CARTESIAN_POINT('Ctrl Pts',(1.87039492239607,105.180841025181,11.6387822943887));
#42560=CARTESIAN_POINT('Ctrl Pts',(1.92662844542012,105.193108828271,11.7067719615592));
#42561=CARTESIAN_POINT('Ctrl Pts',(1.96714642331521,105.201948156624,11.7557606018463));
#42562=CARTESIAN_POINT('Ctrl Pts',(2.00575746861655,105.210761464845,11.8062510992187));
#42563=CARTESIAN_POINT('Ctrl Pts',(2.04238978974739,105.219544953973,11.8581462872837));
#42564=CARTESIAN_POINT('Ctrl Pts',(2.04240145913173,105.219547751992,11.8581628187203));
#42565=CARTESIAN_POINT('Ctrl Pts',(2.04241312831511,105.219550550007,11.8581793502997));
#42566=CARTESIAN_POINT('Ctrl Pts',(2.04242479729753,105.21955334802,11.8581958820219));
#42567=CARTESIAN_POINT('Ctrl Pts',(2.09087546388037,105.231170948197,11.9268370822175));
#42568=CARTESIAN_POINT('Ctrl Pts',(2.13586585416883,105.242737817032,11.9979391885498));
#42569=CARTESIAN_POINT('Ctrl Pts',(2.17721560855768,105.254298993246,12.0712284238331));
#42570=CARTESIAN_POINT('Ctrl Pts',(2.18047416711808,105.255210069268,12.0770039663617));
#42571=CARTESIAN_POINT('Ctrl Pts',(2.18371008994331,105.256121107944,12.082793091901));
#42572=CARTESIAN_POINT('Ctrl Pts',(2.18692327512376,105.257032130292,12.0885956662356));
#42573=CARTESIAN_POINT('Ctrl Pts',(2.23092026546228,105.269506432018,12.168048232023));
#42574=CARTESIAN_POINT('Ctrl Pts',(2.27065881057391,105.281977987509,12.2500219681585));
#42575=CARTESIAN_POINT('Ctrl Pts',(2.30589542182622,105.294478480049,12.3341511912473));
#42576=CARTESIAN_POINT('Ctrl Pts',(2.33996226830475,105.306563988421,12.4154875407277));
#42577=CARTESIAN_POINT('Ctrl Pts',(2.36964148514218,105.318612847026,12.4984093401656));
#42578=CARTESIAN_POINT('Ctrl Pts',(2.39485288630369,105.330634405139,12.5825331581062));
#42579=CARTESIAN_POINT('Ctrl Pts',(2.42034091503532,105.342787867638,12.6675800095266));
#42580=CARTESIAN_POINT('Ctrl Pts',(2.44126312560911,105.354913086582,12.7538544208005));
#42581=CARTESIAN_POINT('Ctrl Pts',(2.4575459223763,105.367004861023,12.8409935595597));
#42582=CARTESIAN_POINT('Ctrl Pts',(2.46751060912787,105.374404741172,12.8943206528073));
#42583=CARTESIAN_POINT('Ctrl Pts',(2.475737958404,105.381791826925,12.9479723280063));
#42584=CARTESIAN_POINT('Ctrl Pts',(2.48221055097361,105.389163087704,13.0018737295152));
#42585=CARTESIAN_POINT('Ctrl Pts',(2.48221345153975,105.389166390991,13.0018978843772));
#42586=CARTESIAN_POINT('Ctrl Pts',(2.4822163517532,105.389169694274,13.0019220392895));
#42587=CARTESIAN_POINT('Ctrl Pts',(2.48221925161395,105.389172997555,13.001946194252));
#42588=CARTESIAN_POINT('Ctrl Pts',(2.49200947540987,105.40032520752,13.083495795978));
#42589=CARTESIAN_POINT('Ctrl Pts',(2.49778328797554,105.411442318619,13.1656207611822));
#42590=CARTESIAN_POINT('Ctrl Pts',(2.49948722327461,105.422563640583,13.2480287371168));
#42591=CARTESIAN_POINT('Ctrl Pts',(2.4996162514713,105.423405787652,13.2542689696737));
#42592=CARTESIAN_POINT('Ctrl Pts',(2.49972192247862,105.424247957049,13.2605108108624));
#42593=CARTESIAN_POINT('Ctrl Pts',(2.49980420337392,105.425090164947,13.2667541264527));
#42594=CARTESIAN_POINT('Ctrl Pts',(2.49997792983122,105.426868388118,13.27993615486));
#42595=CARTESIAN_POINT('Ctrl Pts',(2.50004746740122,105.428646758056,13.2931247595324));
#42596=CARTESIAN_POINT('Ctrl Pts',(2.50001257456669,105.43042539916,13.3063186690347));
#42597=CARTESIAN_POINT('Ctrl Pts',(2.49978032346598,105.442264258336,13.3941389921994));
#42598=CARTESIAN_POINT('Ctrl Pts',(2.49492252226676,105.454055084379,13.4817379211726));
#42599=CARTESIAN_POINT('Ctrl Pts',(2.48551198524104,105.465824827408,13.5687387848905));
#42600=CARTESIAN_POINT('Ctrl Pts',(2.47598579827656,105.477739213622,13.6568088378094));
#42601=CARTESIAN_POINT('Ctrl Pts',(2.46179440573668,105.489631756767,13.7442651823317));
#42602=CARTESIAN_POINT('Ctrl Pts',(2.44301432508079,105.501514401093,13.8307279010647));
#42603=CARTESIAN_POINT('Ctrl Pts',(2.42427314145891,105.513372434257,13.9170115394533));
#42604=CARTESIAN_POINT('Ctrl Pts',(2.40096309316782,105.525220298167,14.0023050920439));
#42605=CARTESIAN_POINT('Ctrl Pts',(2.37315395086311,105.537058232586,14.0862526435496));
#42606=CARTESIAN_POINT('Ctrl Pts',(2.3585587874749,105.543271174544,14.13031111241));
#42607=CARTESIAN_POINT('Ctrl Pts',(2.34272417772455,105.549481216242,14.1739992488483));
#42608=CARTESIAN_POINT('Ctrl Pts',(2.32565797445764,105.555687556788,14.2172685452003));
#42609=CARTESIAN_POINT('Ctrl Pts',(2.32565424479426,105.555688913127,14.2172780013111));
#42610=CARTESIAN_POINT('Ctrl Pts',(2.32565051507209,105.555690269466,14.2172874574019));
#42611=CARTESIAN_POINT('Ctrl Pts',(2.32564678529104,105.555691625805,14.2172969134728));
#42612=CARTESIAN_POINT('Ctrl Pts',(2.3181041697723,105.558434506029,14.2364196196085));
#42613=CARTESIAN_POINT('Ctrl Pts',(2.3103209622381,105.56117666083,14.2554605617107));
#42614=CARTESIAN_POINT('Ctrl Pts',(2.30229812250341,105.563918672576,14.2744151213525));
#42615=CARTESIAN_POINT('Ctrl Pts',(2.26825350326511,105.575554296482,14.354848083642));
#42616=CARTESIAN_POINT('Ctrl Pts',(2.23006911326562,105.587128688416,14.4333113867564));
#42617=CARTESIAN_POINT('Ctrl Pts',(2.18795192015606,105.598676768125,14.5094947206022));
#42618=CARTESIAN_POINT('Ctrl Pts',(2.14520393250849,105.610397804888,14.5868190618925));
#42619=CARTESIAN_POINT('Ctrl Pts',(2.09840447483234,105.622091544948,14.6617935829058));
#42620=CARTESIAN_POINT('Ctrl Pts',(2.04777528699326,105.633778478258,14.7340913729177));
#42621=CARTESIAN_POINT('Ctrl Pts',(1.99706699511466,105.645483671462,14.8065021224197));
#42622=CARTESIAN_POINT('Ctrl Pts',(1.94251772866277,105.657181761271,14.8762271029557));
#42623=CARTESIAN_POINT('Ctrl Pts',(1.88434978160436,105.668880968815,14.9429486422004));
#42624=CARTESIAN_POINT('Ctrl Pts',(1.84060283042637,105.677679709137,14.9931285792183));
#42625=CARTESIAN_POINT('Ctrl Pts',(1.79480924101796,105.686478796312,15.0416099965999));
#42626=CARTESIAN_POINT('Ctrl Pts',(1.74705831743356,105.695278621781,15.0882638213829));
#42627=CARTESIAN_POINT('Ctrl Pts',(1.70289359002632,105.703417561593,15.1314138444479));
#42628=CARTESIAN_POINT('Ctrl Pts',(1.65721598349889,105.711527384435,15.1728430380111));
#42629=CARTESIAN_POINT('Ctrl Pts',(1.6101210606777,105.719607721275,15.2124907827542));
#42630=CARTESIAN_POINT('Ctrl Pts',(1.61009827249629,105.71961163117,15.2125099674125));
#42631=CARTESIAN_POINT('Ctrl Pts',(1.61007548398255,105.719615541058,15.2125291516533));
#42632=CARTESIAN_POINT('Ctrl Pts',(1.61005269513633,105.719619450939,15.2125483354769));
#42633=CARTESIAN_POINT('Ctrl Pts',(1.5467607321213,105.730478449014,15.2658279899057));
#42634=CARTESIAN_POINT('Ctrl Pts',(1.4809054610739,105.741285214015,15.3158927283671));
#42635=CARTESIAN_POINT('Ctrl Pts',(1.41273687818421,105.752072263208,15.3625790913589));
#42636=CARTESIAN_POINT('Ctrl Pts',(1.40908368282409,105.752650347662,15.3650810416332));
#42637=CARTESIAN_POINT('Ctrl Pts',(1.40542384247143,105.753228374396,15.3675732771162));
#42638=CARTESIAN_POINT('Ctrl Pts',(1.40175739531424,105.753806348042,15.3700557685084));
#42639=CARTESIAN_POINT('Ctrl Pts',(1.32696265084648,105.765596887837,15.4206980664509));
#42640=CARTESIAN_POINT('Ctrl Pts',(1.24941903782708,105.777365741811,15.4672896711794));
#42641=CARTESIAN_POINT('Ctrl Pts',(1.16947577736157,105.789139938805,15.5095991769402));
#42642=CARTESIAN_POINT('Ctrl Pts',(1.08953251689606,105.800914135799,15.5519086827011));
#42643=CARTESIAN_POINT('Ctrl Pts',(1.00719045863905,105.812693416674,15.5899352425771));
#42644=CARTESIAN_POINT('Ctrl Pts',(0.922814149414468,105.824492674449,15.6234487947611));
#42645=CARTESIAN_POINT('Ctrl Pts',(0.840494140845276,105.83600437732,15.656145601819));
#42646=CARTESIAN_POINT('Ctrl Pts',(0.756669532738083,105.847474872144,15.6843759250257));
#42647=CARTESIAN_POINT('Ctrl Pts',(0.671717354500609,105.858911300001,15.708074851585));
#42648=CARTESIAN_POINT('Ctrl Pts',(0.593676842397612,105.869417265889,15.7298456454992));
#42649=CARTESIAN_POINT('Ctrl Pts',(0.514684904131195,105.879894301432,15.7477928776352));
#42650=CARTESIAN_POINT('Ctrl Pts',(0.434999958783847,105.890345964829,15.7618732428008));
#42651=CARTESIAN_POINT('Ctrl Pts',(0.4272820147099,105.891358268386,15.7632370069398));
#42652=CARTESIAN_POINT('Ctrl Pts',(0.41955753635055,105.892370336641,15.7645644729712));
#42653=CARTESIAN_POINT('Ctrl Pts',(0.411826737618222,105.893382174577,15.7658555860788));
#42654=CARTESIAN_POINT('Ctrl Pts',(0.392933753176928,105.895854964135,15.7690108848645));
#42655=CARTESIAN_POINT('Ctrl Pts',(0.374003051985269,105.898326358889,15.7719492196747));
#42656=CARTESIAN_POINT('Ctrl Pts',(0.355037683276059,105.900796413385,15.7746699389306));
#42657=CARTESIAN_POINT('Ctrl Pts',(0.355009411215707,105.900800095545,15.7746739947621));
#42658=CARTESIAN_POINT('Ctrl Pts',(0.35498113907849,105.900803777703,15.7746780501095));
#42659=CARTESIAN_POINT('Ctrl Pts',(0.354952866863997,105.900807459857,15.7746821049729));
#42660=CARTESIAN_POINT('Ctrl Pts',(0.275362966415399,105.91117319594,15.7860970640957));
#42661=CARTESIAN_POINT('Ctrl Pts',(0.195159535661565,105.921516126916,15.7936796314266));
#42662=CARTESIAN_POINT('Ctrl Pts',(0.114613373662538,105.931860908419,15.7973747524082));
#42663=CARTESIAN_POINT('Ctrl Pts',(0.106607492758985,105.932889127351,15.7977420287348));
#42664=CARTESIAN_POINT('Ctrl Pts',(0.0985982516142945,105.933917360959,
15.798070866006));
#42665=CARTESIAN_POINT('Ctrl Pts',(0.0905859339165349,105.934945631065,
15.7983611885636));
#42666=CARTESIAN_POINT('Ctrl Pts',(0.0466598291122464,105.940582938786,
15.7999528302801));
#42667=CARTESIAN_POINT('Ctrl Pts',(0.00264108292224348,105.946221279131,
15.8003879064293));
#42668=CARTESIAN_POINT('Ctrl Pts',(-0.0414220991200776,105.951863558129,
15.7996569773884));
#42669=CARTESIAN_POINT('Ctrl Pts',(-0.129649252143588,105.963161022121,
15.7981934473992));
#42670=CARTESIAN_POINT('Ctrl Pts',(-0.217598499637906,105.974416486348,
15.7920619921095));
#42671=CARTESIAN_POINT('Ctrl Pts',(-0.304876011434223,105.985647005872,
15.7813383723747));
#42672=CARTESIAN_POINT('Ctrl Pts',(-0.393111830651169,105.997000836545,
15.7704970072533));
#42673=CARTESIAN_POINT('Ctrl Pts',(-0.480659965460766,106.00832890011,15.7549624067265));
#42674=CARTESIAN_POINT('Ctrl Pts',(-0.567127395333113,106.019642960363,
15.7348227819865));
#42675=CARTESIAN_POINT('Ctrl Pts',(-0.653120786905656,106.030894993817,
15.7147935682241));
#42676=CARTESIAN_POINT('Ctrl Pts',(-0.738044605572204,106.042132906577,
15.6902108041284));
#42677=CARTESIAN_POINT('Ctrl Pts',(-0.82153966473669,106.053366615165,15.661159983255));
#42678=CARTESIAN_POINT('Ctrl Pts',(-0.880797051696853,106.061339305087,
15.6405422874149));
#42679=CARTESIAN_POINT('Ctrl Pts',(-0.939335435527555,106.06930983994,15.6176741808237));
#42680=CARTESIAN_POINT('Ctrl Pts',(-0.997036660975464,106.077282331523,
15.5925799698115));
#42681=CARTESIAN_POINT('Ctrl Pts',(-1.00076673224388,106.077797709863,15.5909577651742));
#42682=CARTESIAN_POINT('Ctrl Pts',(-1.00449242144962,106.078312974203,15.5893266403852));
#42683=CARTESIAN_POINT('Ctrl Pts',(-1.00821370359685,106.078828125878,15.5876866136242));
#42684=CARTESIAN_POINT('Ctrl Pts',(-1.00822934511551,106.078830291195,15.5876797201643));
#42685=CARTESIAN_POINT('Ctrl Pts',(-1.00824498655625,106.07883245651,15.587672826547));
#42686=CARTESIAN_POINT('Ctrl Pts',(-1.00826062791905,106.078834621822,15.5876659327723));
#42687=CARTESIAN_POINT('Ctrl Pts',(-1.08779081575265,106.089844387037,15.5526137953467));
#42688=CARTESIAN_POINT('Ctrl Pts',(-1.16531048809033,106.100803409767,15.5134950297588));
#42689=CARTESIAN_POINT('Ctrl Pts',(-1.24053283900543,106.111734164408,15.4705020308001));
#42690=CARTESIAN_POINT('Ctrl Pts',(-1.31708027702335,106.122857470888,15.4267516842214));
#42691=CARTESIAN_POINT('Ctrl Pts',(-1.39124746951981,106.133951294818,15.378989002505));
#42692=CARTESIAN_POINT('Ctrl Pts',(-1.46271281470655,106.145032236782,15.3274294926996));
#42693=CARTESIAN_POINT('Ctrl Pts',(-1.53466997760064,106.156189436735,15.2755151552525));
#42694=CARTESIAN_POINT('Ctrl Pts',(-1.60388692214073,106.167333327671,15.2197519602795));
#42695=CARTESIAN_POINT('Ctrl Pts',(-1.67003393079078,106.178477253816,15.1603726532369));
#42696=CARTESIAN_POINT('Ctrl Pts',(-1.71410383774848,106.185901804047,15.1208116724761));
#42697=CARTESIAN_POINT('Ctrl Pts',(-1.75681112493626,106.193326301304,15.079645902846));
#42698=CARTESIAN_POINT('Ctrl Pts',(-1.79806070250911,106.200754649183,15.0369449333695));
#42699=CARTESIAN_POINT('Ctrl Pts',(-1.85480992413589,106.210974219538,14.978198955275));
#42700=CARTESIAN_POINT('Ctrl Pts',(-1.90852777793187,106.221152183826,14.9168293454672));
#42701=CARTESIAN_POINT('Ctrl Pts',(-1.95906553464639,106.231300987436,14.8530814438934));
#42702=CARTESIAN_POINT('Ctrl Pts',(-1.96366259469882,106.232224151872,14.8472827509794));
#42703=CARTESIAN_POINT('Ctrl Pts',(-1.96823334005503,106.233147077082,14.8414643440128));
#42704=CARTESIAN_POINT('Ctrl Pts',(-1.97277765705257,106.234069773669,14.835626386468));
#42705=CARTESIAN_POINT('Ctrl Pts',(-2.00522579949362,106.240658176343,14.7939411611458));
#42706=CARTESIAN_POINT('Ctrl Pts',(-2.03632730304487,106.247234868703,14.7512605436525));
#42707=CARTESIAN_POINT('Ctrl Pts',(-2.06604550345792,106.253804188614,14.7076421634946));
#42708=CARTESIAN_POINT('Ctrl Pts',(-2.06605822524938,106.253807000814,14.7076234913029));
#42709=CARTESIAN_POINT('Ctrl Pts',(-2.06607094678712,106.253809813013,14.707604818939));
#42710=CARTESIAN_POINT('Ctrl Pts',(-2.06608366807114,106.25381262521,14.707586146403));
#42711=CARTESIAN_POINT('Ctrl Pts',(-2.11184912614115,106.263929645628,14.6404107604048));
#42712=CARTESIAN_POINT('Ctrl Pts',(-2.15433513971328,106.27402966425,14.5710071336948));
#42713=CARTESIAN_POINT('Ctrl Pts',(-2.19338512292969,106.284124772629,14.4996089412343));
#42714=CARTESIAN_POINT('Ctrl Pts',(-2.19856502698409,106.285463869052,14.4901381103622));
#42715=CARTESIAN_POINT('Ctrl Pts',(-2.20368439823283,106.286802872529,14.4806321937328));
#42716=CARTESIAN_POINT('Ctrl Pts',(-2.2087428039534,106.288141805273,14.4710917482332));
#42717=CARTESIAN_POINT('Ctrl Pts',(-2.24920320147823,106.298851454537,14.3947811004121));
#42718=CARTESIAN_POINT('Ctrl Pts',(-2.28576704144237,106.309556811497,14.3162608832952));
#42719=CARTESIAN_POINT('Ctrl Pts',(-2.31823081051596,106.320268892542,14.2358441526627));
#42720=CARTESIAN_POINT('Ctrl Pts',(-2.32043139778229,106.320995021079,14.2303930285795));
#42721=CARTESIAN_POINT('Ctrl Pts',(-2.32261312579945,106.321721179361,14.2249331926951));
#42722=CARTESIAN_POINT('Ctrl Pts',(-2.32477592260554,106.322447370315,14.2194647439171));
#42723=CARTESIAN_POINT('Ctrl Pts',(-2.35733730491164,106.333380335086,14.1371360430508));
#42724=CARTESIAN_POINT('Ctrl Pts',(-2.38544381125838,106.344264515039,14.0532814442699));
#42725=CARTESIAN_POINT('Ctrl Pts',(-2.40901979147983,106.355112883126,13.9682972962322));
#42726=CARTESIAN_POINT('Ctrl Pts',(-2.43282223960327,106.366065459272,13.882496801153));
#42727=CARTESIAN_POINT('Ctrl Pts',(-2.45200715117387,106.376981311971,13.7955461667228));
#42728=CARTESIAN_POINT('Ctrl Pts',(-2.46651155076268,106.387878306611,13.707829504449));
#42729=CARTESIAN_POINT('Ctrl Pts',(-2.47985710950783,106.397904676971,13.627121036502));
#42730=CARTESIAN_POINT('Ctrl Pts',(-2.48924077358504,106.407915006875,13.5457643076491));
#42731=CARTESIAN_POINT('Ctrl Pts',(-2.49461608659223,106.417928770086,13.4640288581122));
#42732=CARTESIAN_POINT('Ctrl Pts',(-2.49505233826781,106.418741470849,13.4573953417444));
#42733=CARTESIAN_POINT('Ctrl Pts',(-2.49546216787465,106.419554196303,13.4507593110106));
#42734=CARTESIAN_POINT('Ctrl Pts',(-2.49584553938309,106.420366957959,13.4441208997767));
#42735=CARTESIAN_POINT('Ctrl Pts',(-2.49668113576872,106.42213845294,13.4296518213207));
#42736=CARTESIAN_POINT('Ctrl Pts',(-2.49739112856075,106.423910126733,13.4151714419338));
#42737=CARTESIAN_POINT('Ctrl Pts',(-2.4979752113352,106.425682110233,13.4006811231117));
#42738=CARTESIAN_POINT('Ctrl Pts',(-2.49797622340333,106.425685180634,13.400656015044));
#42739=CARTESIAN_POINT('Ctrl Pts',(-2.49797723509339,106.425688251035,13.4006309069463));
#42740=CARTESIAN_POINT('Ctrl Pts',(-2.49797824640536,106.425691321437,13.4006057988189));
#42741=CARTESIAN_POINT('Ctrl Pts',(-2.49932446808026,106.429778529246,13.3671827735883));
#42742=CARTESIAN_POINT('Ctrl Pts',(-2.50000082507155,106.433867394332,13.3337067595297));
#42743=CARTESIAN_POINT('Ctrl Pts',(-2.50000333388702,106.437958303058,13.3001965898202));
#42744=CARTESIAN_POINT('',(2.31220144791066,104.895136985459,14.2499282950331));
#42745=CARTESIAN_POINT('Ctrl Pts',(-2.5,105.533497732924,13.3000000000004));
#42746=CARTESIAN_POINT('Ctrl Pts',(-2.5,105.520804033348,13.4158707782706));
#42747=CARTESIAN_POINT('Ctrl Pts',(-2.49194405837885,105.508271404854,13.5318769342806));
#42748=CARTESIAN_POINT('Ctrl Pts',(-2.43550168616906,105.465234432574,13.9343938651791));
#42749=CARTESIAN_POINT('Ctrl Pts',(-2.3455711156717,105.436725695498,14.2123538901486));
#42750=CARTESIAN_POINT('Ctrl Pts',(-2.05347068002038,105.372146357901,14.764712314317));
#42751=CARTESIAN_POINT('Ctrl Pts',(-1.83899158460821,105.335631760271,15.0263806357197));
#42752=CARTESIAN_POINT('Ctrl Pts',(-1.35535144233529,105.273294634429,15.4204772199161));
#42753=CARTESIAN_POINT('Ctrl Pts',(-1.10166774143074,105.247108937262,15.562670083002));
#42754=CARTESIAN_POINT('Ctrl Pts',(-0.513772393234898,105.187016003129,
15.7693959782354));
#42755=CARTESIAN_POINT('Ctrl Pts',(-0.179028915558743,105.152249943282,
15.8159540487419));
#42756=CARTESIAN_POINT('Ctrl Pts',(0.437597169497571,105.09541965019,15.777623767016));
#42757=CARTESIAN_POINT('Ctrl Pts',(0.71488641944579,105.072598380658,15.712260395868));
#42758=CARTESIAN_POINT('Ctrl Pts',(1.28240255117051,105.020050748162,15.4717752588311));
#42759=CARTESIAN_POINT('Ctrl Pts',(1.56033530811733,104.988672482657,15.2815924355496));
#42760=CARTESIAN_POINT('Ctrl Pts',(2.01516254243393,104.936876652781,14.8135517832682));
#42761=CARTESIAN_POINT('Ctrl Pts',(2.19136165007833,104.91683004046,14.5447676063188));
#42762=CARTESIAN_POINT('Ctrl Pts',(2.31244118192445,104.894682621471,14.2500609349615));
#42763=CARTESIAN_POINT('Ctrl Pts',(2.31132717531622,104.894586489788,14.2495818126787));
#42764=CARTESIAN_POINT('Ctrl Pts',(2.31640301832098,104.893034510998,14.2382227802811));
#42765=CARTESIAN_POINT('Ctrl Pts',(2.32096538576457,104.891223989443,14.2271257782176));
#42766=CARTESIAN_POINT('Ctrl Pts',(2.325494703813,104.889232143616,14.2155903870854));
#42767=CARTESIAN_POINT('Ctrl Pts',(2.32796599272174,104.888145351643,14.2092964408758));
#42768=CARTESIAN_POINT('Ctrl Pts',(2.33045581922597,104.887039290589,14.2028797622965));
#42769=CARTESIAN_POINT('Ctrl Pts',(2.33288880610748,104.885944438163,14.1965283732465));
#42770=CARTESIAN_POINT('Ctrl Pts',(2.3547237778565,104.876118626125,14.139527490288));
#42771=CARTESIAN_POINT('Ctrl Pts',(2.37442302242763,104.866334600622,14.0819364577489));
#42772=CARTESIAN_POINT('Ctrl Pts',(2.39201877324852,104.856560092324,14.0237517623631));
#42773=CARTESIAN_POINT('Ctrl Pts',(2.39344183757104,104.855769574536,14.0190460487528));
#42774=CARTESIAN_POINT('Ctrl Pts',(2.39485111735034,104.854979119164,14.0143364410787));
#42775=CARTESIAN_POINT('Ctrl Pts',(2.39624661586076,104.854188709229,14.0096229320215));
#42776=CARTESIAN_POINT('Ctrl Pts',(2.40063533255731,104.851702941418,13.994799372022));
#42777=CARTESIAN_POINT('Ctrl Pts',(2.40488779415261,104.849217659616,13.9799372376659));
#42778=CARTESIAN_POINT('Ctrl Pts',(2.40900402591882,104.846732403914,13.9650362751071));
#42779=CARTESIAN_POINT('Ctrl Pts',(2.4324637763532,104.832568119238,13.8801108183507));
#42780=CARTESIAN_POINT('Ctrl Pts',(2.45142542935255,104.81844640189,13.7941923937425));
#42781=CARTESIAN_POINT('Ctrl Pts',(2.46583912706641,104.804367050333,13.7076472505981));
#42782=CARTESIAN_POINT('Ctrl Pts',(2.48028545759541,104.790255822925,13.6209061680276));
#42783=CARTESIAN_POINT('Ctrl Pts',(2.49016380420976,104.776187456513,13.53353550939));
#42784=CARTESIAN_POINT('Ctrl Pts',(2.49540428284792,104.762186058041,13.4458706150948));
#42785=CARTESIAN_POINT('Ctrl Pts',(2.50002756423327,104.749833673956,13.3685304517379));
#42786=CARTESIAN_POINT('Ctrl Pts',(2.50104126814055,104.737533941667,13.2909606583303));
#42787=CARTESIAN_POINT('Ctrl Pts',(2.49837750332954,104.725315874626,13.2133711356687));
#42788=CARTESIAN_POINT('Ctrl Pts',(2.498377401564,104.725315407851,13.2133681714659));
#42789=CARTESIAN_POINT('Ctrl Pts',(2.4983772997931,104.725314941076,13.2133652072631));
#42790=CARTESIAN_POINT('Ctrl Pts',(2.49837719801682,104.725314474302,13.2133622430602));
#42791=CARTESIAN_POINT('Ctrl Pts',(2.49631991527468,104.715879199737,13.153444513395));
#42792=CARTESIAN_POINT('Ctrl Pts',(2.49206892984282,104.706492629584,13.0935136045211));
#42793=CARTESIAN_POINT('Ctrl Pts',(2.48563118019984,104.697127684045,13.0336903597452));
#42794=CARTESIAN_POINT('Ctrl Pts',(2.47641510401865,104.68372112798,12.9480493187237));
#42795=CARTESIAN_POINT('Ctrl Pts',(2.4627635801708,104.670422904911,12.8630447898128));
#42796=CARTESIAN_POINT('Ctrl Pts',(2.44480596284123,104.657174972098,12.779027106201));
#42797=CARTESIAN_POINT('Ctrl Pts',(2.42644199360434,104.643627259939,12.6931082379634));
#42798=CARTESIAN_POINT('Ctrl Pts',(2.40357459222705,104.630132057815,12.6082215059131));
#42799=CARTESIAN_POINT('Ctrl Pts',(2.37631958811954,104.616658055251,12.5247395636468));
#42800=CARTESIAN_POINT('Ctrl Pts',(2.3633671507341,104.610254784357,12.4850663122411));
#42801=CARTESIAN_POINT('Ctrl Pts',(2.34942349741903,104.603856751717,12.44571028307));
#42802=CARTESIAN_POINT('Ctrl Pts',(2.33449942248738,104.597462983089,12.4067111690843));
#42803=CARTESIAN_POINT('Ctrl Pts',(2.33449551723172,104.597461310001,12.4067009639954));
#42804=CARTESIAN_POINT('Ctrl Pts',(2.33449161190891,104.597459636912,12.406690758931));
#42805=CARTESIAN_POINT('Ctrl Pts',(2.33448770651895,104.597457963824,12.406680553891));
#42806=CARTESIAN_POINT('Ctrl Pts',(2.30308731779963,104.584005884054,12.3246292797908));
#42807=CARTESIAN_POINT('Ctrl Pts',(2.26734814612602,104.570570846415,12.2441570905773));
#42808=CARTESIAN_POINT('Ctrl Pts',(2.22738543114158,104.557133161751,12.1656287552845));
#42809=CARTESIAN_POINT('Ctrl Pts',(2.22232079896839,104.555430151079,12.1556765502458));
#42810=CARTESIAN_POINT('Ctrl Pts',(2.21718830623773,104.553727135036,12.1457555765282));
#42811=CARTESIAN_POINT('Ctrl Pts',(2.21198816619355,104.552024105675,12.1358665851468));
#42812=CARTESIAN_POINT('Ctrl Pts',(2.1707674646652,104.53852445674,12.0574780881662));
#42813=CARTESIAN_POINT('Ctrl Pts',(2.125504413121,104.525088923967,11.9814918736891));
#42814=CARTESIAN_POINT('Ctrl Pts',(2.07641083093898,104.511727763851,11.908206254754));
#42815=CARTESIAN_POINT('Ctrl Pts',(2.03007312716373,104.499116635225,11.8390345392209));
#42816=CARTESIAN_POINT('Ctrl Pts',(1.98032290342944,104.486572082576,11.7722682983247));
#42817=CARTESIAN_POINT('Ctrl Pts',(1.92730470099957,104.474120826965,11.7081458826343));
#42818=CARTESIAN_POINT('Ctrl Pts',(1.92415675167142,104.473381535176,11.7043386219928));
#42819=CARTESIAN_POINT('Ctrl Pts',(1.92099726632121,104.472642571576,11.7005406836093));
#42820=CARTESIAN_POINT('Ctrl Pts',(1.91782626945823,104.471903941485,11.6967521182203));
#42821=CARTESIAN_POINT('Ctrl Pts',(1.91782098748062,104.471902711138,11.6967458075494));
#42822=CARTESIAN_POINT('Ctrl Pts',(1.91781570547112,104.471901480791,11.6967394969046));
#42823=CARTESIAN_POINT('Ctrl Pts',(1.91781042342962,104.471900250446,11.6967331862858));
#42824=CARTESIAN_POINT('Ctrl Pts',(1.86438918186872,104.459456844901,11.6329091713746));
#42825=CARTESIAN_POINT('Ctrl Pts',(1.8077021726804,104.447107763815,11.5717411172208));
#42826=CARTESIAN_POINT('Ctrl Pts',(1.74797526072607,104.434777066512,11.5134449880751));
#42827=CARTESIAN_POINT('Ctrl Pts',(1.74475125556711,104.434111466527,11.5102982152894));
#42828=CARTESIAN_POINT('Ctrl Pts',(1.741518389665,104.433445920956,11.5071598226906));
#42829=CARTESIAN_POINT('Ctrl Pts',(1.73827669757747,104.432780418149,11.504029848421));
#42830=CARTESIAN_POINT('Ctrl Pts',(1.70142992194142,104.425215963545,11.4684529162061));
#42831=CARTESIAN_POINT('Ctrl Pts',(1.66344318122168,104.417657370591,11.4339626861876));
#42832=CARTESIAN_POINT('Ctrl Pts',(1.6243690138553,104.410091315338,11.4006152189792));
#42833=CARTESIAN_POINT('Ctrl Pts',(1.55770811423271,104.397183553415,11.3437241240672));
#42834=CARTESIAN_POINT('Ctrl Pts',(1.48821400032916,104.384316116825,11.2904416042935));
#42835=CARTESIAN_POINT('Ctrl Pts',(1.41623247776679,104.371446188938,11.2409555225195));
#42836=CARTESIAN_POINT('Ctrl Pts',(1.34343741829754,104.358430804815,11.1909101478539));
#42837=CARTESIAN_POINT('Ctrl Pts',(1.26809865033967,104.345412964124,11.1447478606375));
#42838=CARTESIAN_POINT('Ctrl Pts',(1.19055875363133,104.332378863251,11.1026664096893));
#42839=CARTESIAN_POINT('Ctrl Pts',(1.11337774917425,104.319405090519,11.060779732107));
#42840=CARTESIAN_POINT('Ctrl Pts',(1.03401642885747,104.306415474085,11.0229360815388));
#42841=CARTESIAN_POINT('Ctrl Pts',(0.952792154383874,104.293423606679,10.9893319930855));
#42842=CARTESIAN_POINT('Ctrl Pts',(0.903417989526645,104.285526181835,10.9689049247747));
#42843=CARTESIAN_POINT('Ctrl Pts',(0.853355014458621,104.277628441397,10.9500444244177));
#42844=CARTESIAN_POINT('Ctrl Pts',(0.802669533287437,104.269737670569,10.9327957675765));
#42845=CARTESIAN_POINT('Ctrl Pts',(0.726683416410001,104.25790806926,10.9069371109271));
#42846=CARTESIAN_POINT('Ctrl Pts',(0.649647541024132,104.246147920313,10.8848185904926));
#42847=CARTESIAN_POINT('Ctrl Pts',(0.571791164490983,104.234490979685,10.8664973794054));
#42848=CARTESIAN_POINT('Ctrl Pts',(0.563722196810629,104.233282864417,10.864598584898));
#42849=CARTESIAN_POINT('Ctrl Pts',(0.5556443763029,104.232075854953,10.8627406008586));
#42850=CARTESIAN_POINT('Ctrl Pts',(0.547557931073244,104.230869986947,10.8609235080037));
#42851=CARTESIAN_POINT('Ctrl Pts',(0.54067397443229,104.229843436612,10.8593766245376));
#42852=CARTESIAN_POINT('Ctrl Pts',(0.533783769571032,104.228817722253,10.8578593633675));
#42853=CARTESIAN_POINT('Ctrl Pts',(0.526887455256306,104.227792869948,10.856371770479));
#42854=CARTESIAN_POINT('Ctrl Pts',(0.526880753065446,104.227791873945,10.8563703247601));
#42855=CARTESIAN_POINT('Ctrl Pts',(0.526874050868816,104.227790877942,10.8563688790693));
#42856=CARTESIAN_POINT('Ctrl Pts',(0.526867348666415,104.227789881939,10.8563674334065));
#42857=CARTESIAN_POINT('Ctrl Pts',(0.446620824989185,104.21586459042,10.8390582854445));
#42858=CARTESIAN_POINT('Ctrl Pts',(0.365545409459377,104.204054184164,10.8257640866501));
#42859=CARTESIAN_POINT('Ctrl Pts',(0.283937999466609,104.192283089781,10.8164921772243));
#42860=CARTESIAN_POINT('Ctrl Pts',(0.279486886488785,104.191641058978,10.8159864594668));
#42861=CARTESIAN_POINT('Ctrl Pts',(0.275034195464569,104.190999146129,10.8154927196941));
#42862=CARTESIAN_POINT('Ctrl Pts',(0.270579976289946,104.190357339318,10.8150109631338));
#42863=CARTESIAN_POINT('Ctrl Pts',(0.18293327300947,104.177728357924,10.8055313276145));
#42864=CARTESIAN_POINT('Ctrl Pts',(0.0946927161389826,104.165139746534,
10.8006875338495));
#42865=CARTESIAN_POINT('Ctrl Pts',(0.00625065803806539,104.152526195187,
10.8005145466055));
#42866=CARTESIAN_POINT('Ctrl Pts',(-0.0411532060176732,104.145765485563,
10.8004218275533));
#42867=CARTESIAN_POINT('Ctrl Pts',(-0.0886145178237575,104.138998111239,
10.8016712486707));
#42868=CARTESIAN_POINT('Ctrl Pts',(-0.136070138901457,104.13221754998,10.8042694897761));
#42869=CARTESIAN_POINT('Ctrl Pts',(-0.224250527438516,104.119618146311,
10.8090974512478));
#42870=CARTESIAN_POINT('Ctrl Pts',(-0.311967947992333,104.107034634962,
10.8185579744082));
#42871=CARTESIAN_POINT('Ctrl Pts',(-0.398827613518663,104.094448735194,
10.8325581551025));
#42872=CARTESIAN_POINT('Ctrl Pts',(-0.486276333258706,104.081777481916,
10.8466532805031));
#42873=CARTESIAN_POINT('Ctrl Pts',(-0.572855093604851,104.069104083644,
10.8653494072166));
#42874=CARTESIAN_POINT('Ctrl Pts',(-0.658183909257249,104.056437260993,
10.8885601179806));
#42875=CARTESIAN_POINT('Ctrl Pts',(-0.742515312981924,104.043918501337,
10.9114995178212));
#42876=CARTESIAN_POINT('Ctrl Pts',(-0.825625721850992,104.03140657265,10.9388476503207));
#42877=CARTESIAN_POINT('Ctrl Pts',(-0.907175381067747,104.0189312925,10.9705395440152));
#42878=CARTESIAN_POINT('Ctrl Pts',(-0.958033605417957,104.011151117785,
10.9903041077801));
#42879=CARTESIAN_POINT('Ctrl Pts',(-1.00828537816385,104.00338560235,11.0117585033029));
#42880=CARTESIAN_POINT('Ctrl Pts',(-1.05785344363349,103.995645155671,11.0348935660898));
#42881=CARTESIAN_POINT('Ctrl Pts',(-1.06777998612567,103.994095047307,11.0395266132269));
#42882=CARTESIAN_POINT('Ctrl Pts',(-1.07767292081435,103.992546915427,11.0442241955565));
#42883=CARTESIAN_POINT('Ctrl Pts',(-1.08753176128416,103.991000846838,11.0489860266477));
#42884=CARTESIAN_POINT('Ctrl Pts',(-1.087533256854,103.991000612302,11.0489867490096));
#42885=CARTESIAN_POINT('Ctrl Pts',(-1.08753475242305,103.991000377766,11.048987471373));
#42886=CARTESIAN_POINT('Ctrl Pts',(-1.08753624799132,103.99100014323,11.0489881937379));
#42887=CARTESIAN_POINT('Ctrl Pts',(-1.16515019883,103.978828674469,11.0864760125203));
#42888=CARTESIAN_POINT('Ctrl Pts',(-1.24065394406993,103.96678307826,11.1279448232097));
#42889=CARTESIAN_POINT('Ctrl Pts',(-1.31378826137423,103.95478369176,11.1731703264622));
#42890=CARTESIAN_POINT('Ctrl Pts',(-1.38825593575194,103.942565537006,11.2192203638989));
#42891=CARTESIAN_POINT('Ctrl Pts',(-1.46026623719515,103.930395143374,11.2691661804705));
#42892=CARTESIAN_POINT('Ctrl Pts',(-1.5295177582202,103.918214907366,11.3227748642695));
#42893=CARTESIAN_POINT('Ctrl Pts',(-1.59937234241708,103.905928602182,11.3768503886868));
#42894=CARTESIAN_POINT('Ctrl Pts',(-1.66641902509694,103.893632283652,11.4346530706847));
#42895=CARTESIAN_POINT('Ctrl Pts',(-1.7303331345939,103.881294620168,11.4959394971383));
#42896=CARTESIAN_POINT('Ctrl Pts',(-1.7639922823914,103.874797224804,11.5282148257351));
#42897=CARTESIAN_POINT('Ctrl Pts',(-1.79678247358277,103.868288827152,11.5614562326876));
#42898=CARTESIAN_POINT('Ctrl Pts',(-1.82865573339812,103.861767840413,11.5956277512324));
#42899=CARTESIAN_POINT('Ctrl Pts',(-1.88899623687624,103.849422707682,11.6603191773855));
#42900=CARTESIAN_POINT('Ctrl Pts',(-1.945743259724,103.83709370184,11.7280142267784));
#42901=CARTESIAN_POINT('Ctrl Pts',(-1.99868685669959,103.82478831317,11.7983868957619));
#42902=CARTESIAN_POINT('Ctrl Pts',(-2.04833708423673,103.813248384222,11.8643820156069));
#42903=CARTESIAN_POINT('Ctrl Pts',(-2.0946426725136,103.801729546487,11.9327316991028));
#42904=CARTESIAN_POINT('Ctrl Pts',(-2.1374460831665,103.790253046683,12.0031971503753));
#42905=CARTESIAN_POINT('Ctrl Pts',(-2.14033658080241,103.789478043125,12.0079556548311));
#42906=CARTESIAN_POINT('Ctrl Pts',(-2.14321110172861,103.788703231404,12.0127238265024));
#42907=CARTESIAN_POINT('Ctrl Pts',(-2.14606959460474,103.787928617525,12.0175015999515));
#42908=CARTESIAN_POINT('Ctrl Pts',(-2.18042621706528,103.77861842584,12.0749263218966));
#42909=CARTESIAN_POINT('Ctrl Pts',(-2.21246904706033,103.769337440822,12.1337357121099));
#42910=CARTESIAN_POINT('Ctrl Pts',(-2.24211581456284,103.760101711445,12.1938232382963));
#42911=CARTESIAN_POINT('Ctrl Pts',(-2.24211903410285,103.760100708475,12.1938297636011));
#42912=CARTESIAN_POINT('Ctrl Pts',(-2.24212225361458,103.760099705506,12.193836288921));
#42913=CARTESIAN_POINT('Ctrl Pts',(-2.24212547309804,103.760098702538,12.193842814256));
#42914=CARTESIAN_POINT('Ctrl Pts',(-2.27620049792537,103.749483282059,12.2629069839777));
#42915=CARTESIAN_POINT('Ctrl Pts',(-2.30711203979563,103.738926878711,12.3336636236315));
#42916=CARTESIAN_POINT('Ctrl Pts',(-2.3347431690348,103.728375426866,12.4059037896928));
#42917=CARTESIAN_POINT('Ctrl Pts',(-2.36583191082452,103.716503622457,12.4871837059092));
#42918=CARTESIAN_POINT('Ctrl Pts',(-2.39261160021939,103.704696711206,12.5699347703841));
#42919=CARTESIAN_POINT('Ctrl Pts',(-2.415018825915,103.692899317101,12.6537855449586));
#42920=CARTESIAN_POINT('Ctrl Pts',(-2.43777757189232,103.680916847728,12.738951754487));
#42921=CARTESIAN_POINT('Ctrl Pts',(-2.45602467618214,103.668944244274,12.825251955648));
#42922=CARTESIAN_POINT('Ctrl Pts',(-2.46968963992784,103.656949702055,12.9122873766021));
#42923=CARTESIAN_POINT('Ctrl Pts',(-2.48340027960736,103.644915067384,12.9996137184984));
#42924=CARTESIAN_POINT('Ctrl Pts',(-2.49249782364295,103.632858547501,13.0876793361628));
#42925=CARTESIAN_POINT('Ctrl Pts',(-2.49691617211707,103.620772247152,13.1760824234444));
#42926=CARTESIAN_POINT('Ctrl Pts',(-2.49897760899693,103.615133229445,13.2173280122618));
#42927=CARTESIAN_POINT('Ctrl Pts',(-2.50002056844956,103.609488051128,13.2586471582004));
#42928=CARTESIAN_POINT('Ctrl Pts',(-2.50003871369437,103.603837493162,13.2999999833247));
#42929=CARTESIAN_POINT('Origin',(0.,70.2,13.3));
#42930=CARTESIAN_POINT('',(-2.5,101.637207465761,13.3));
#42931=CARTESIAN_POINT('',(-2.49999999983267,102.618167926383,13.3000182966029));
#42932=CARTESIAN_POINT('',(-2.5,70.2,13.3));
#42933=CARTESIAN_POINT('Ctrl Pts',(-2.50000000000001,102.618170270812,13.3000000000108));
#42934=CARTESIAN_POINT('Ctrl Pts',(-2.50000000000002,102.640241818529,13.1277477261055));
#42935=CARTESIAN_POINT('Ctrl Pts',(-2.48219754881853,102.662175662565,12.9559557473048));
#42936=CARTESIAN_POINT('Ctrl Pts',(-2.41878394951985,102.701806833258,12.6532752530091));
#42937=CARTESIAN_POINT('Ctrl Pts',(-2.37971848431703,102.719380382371,12.5217291795141));
#42938=CARTESIAN_POINT('Ctrl Pts',(-2.24627692491632,102.766817117034,12.1785203162223));
#42939=CARTESIAN_POINT('Ctrl Pts',(-2.13297412252146,102.796604688506,11.9756503729151));
#42940=CARTESIAN_POINT('Ctrl Pts',(-1.83035194125583,102.861030204594,11.5758152281744));
#42941=CARTESIAN_POINT('Ctrl Pts',(-1.63342316382879,102.894998152686,11.3882017433834));
#42942=CARTESIAN_POINT('Ctrl Pts',(-1.15105626067604,102.968551686843,11.0586572424382));
#42943=CARTESIAN_POINT('Ctrl Pts',(-0.860793368550738,103.007629514266,
10.9319652280881));
#42944=CARTESIAN_POINT('Ctrl Pts',(-0.333393964031027,103.075601944804,
10.8119578523735));
#42945=CARTESIAN_POINT('Ctrl Pts',(-0.106267156973827,103.103980854947,
10.7919692630349));
#42946=CARTESIAN_POINT('Ctrl Pts',(0.454543715130937,103.174286282485,10.8190159216283));
#42947=CARTESIAN_POINT('Ctrl Pts',(0.782084388962346,103.215561131113,10.9020257305053));
#42948=CARTESIAN_POINT('Ctrl Pts',(1.37852094509146,103.297314979055,11.1888903374276));
#42949=CARTESIAN_POINT('Ctrl Pts',(1.64277116966911,103.336961893884,11.3872937983161));
#42950=CARTESIAN_POINT('Ctrl Pts',(2.06252832963449,103.413649002816,11.855411703839));
#42951=CARTESIAN_POINT('Ctrl Pts',(2.22153308461144,103.450236068805,12.1143937399292));
#42952=CARTESIAN_POINT('Ctrl Pts',(2.44745506784865,103.526009143805,12.6964692631386));
#42953=CARTESIAN_POINT('Ctrl Pts',(2.50488005028318,103.564342939622,13.017348411793));
#42954=CARTESIAN_POINT('Ctrl Pts',(2.49428563828586,103.643210285286,13.6747076658831));
#42955=CARTESIAN_POINT('Ctrl Pts',(2.42183817645359,103.68304824667,14.004707900806));
#42956=CARTESIAN_POINT('Ctrl Pts',(2.168328900386,103.757209567566,14.5782519913845));
#42957=CARTESIAN_POINT('Ctrl Pts',(2.00401103259475,103.79118499957,14.8229973609931));
#42958=CARTESIAN_POINT('Ctrl Pts',(1.68844924596043,103.844936016636,15.1508213560995));
#42959=CARTESIAN_POINT('Ctrl Pts',(1.56461454068236,103.864070384638,15.2566270723523));
#42960=CARTESIAN_POINT('Ctrl Pts',(1.18864626693842,103.917695431997,15.5191834086683));
#42961=CARTESIAN_POINT('Ctrl Pts',(0.917703892648551,103.951315705915,15.6442495189771));
#42962=CARTESIAN_POINT('Ctrl Pts',(0.307417210611317,104.023796487592,15.8034880093659));
#42963=CARTESIAN_POINT('Ctrl Pts',(-0.030061686814792,104.062479500167,
15.8221220763861));
#42964=CARTESIAN_POINT('Ctrl Pts',(-0.67340724325193,104.136138283098,15.7281808403738));
#42965=CARTESIAN_POINT('Ctrl Pts',(-0.974166239719262,104.170745060693,
15.6239078966338));
#42966=CARTESIAN_POINT('Ctrl Pts',(-1.3875139716866,104.224606338278,15.3858760299509));
#42967=CARTESIAN_POINT('Ctrl Pts',(-1.51932294290106,104.242802123662,15.291919144752));
#42968=CARTESIAN_POINT('Ctrl Pts',(-1.86263044979247,104.293459772383,14.9931640649498));
#42969=CARTESIAN_POINT('Ctrl Pts',(-2.04844768197224,104.324808370143,14.7629080256152));
#42970=CARTESIAN_POINT('Ctrl Pts',(-2.35110813356646,104.392648284681,14.2131243018626));
#42971=CARTESIAN_POINT('Ctrl Pts',(-2.45193861624832,104.429337759002,13.8912436478308));
#42972=CARTESIAN_POINT('Ctrl Pts',(-2.49552480648441,104.4738137519,13.4728195719713));
#42973=CARTESIAN_POINT('Ctrl Pts',(-2.5,104.482864048722,13.3863654953521));
#42974=CARTESIAN_POINT('Ctrl Pts',(-2.5,104.491842419534,13.3));
#42975=CARTESIAN_POINT('',(-2.49999935789722,103.603575436303,13.3017917905773));
#42976=CARTESIAN_POINT('Ctrl Pts',(-2.50003871369437,103.603837493162,13.2999999833247));
#42977=CARTESIAN_POINT('Ctrl Pts',(-2.50003897610844,103.60375577556,13.3005980222681));
#42978=CARTESIAN_POINT('Ctrl Pts',(-2.50003902414661,103.603674056831,13.3011960682681));
#42979=CARTESIAN_POINT('Ctrl Pts',(-2.50003885778613,103.603592336976,13.3017941212051));
#42980=CARTESIAN_POINT('Ctrl Pts',(-2.49999935789722,103.603575436303,13.3017917905773));
#42981=CARTESIAN_POINT('Ctrl Pts',(-2.49987384567273,103.579612808251,13.4769129708106));
#42982=CARTESIAN_POINT('Ctrl Pts',(-2.48134822948507,103.55566875521,13.6515591459021));
#42983=CARTESIAN_POINT('Ctrl Pts',(-2.40206796913163,103.504501247821,14.022253028833));
#42984=CARTESIAN_POINT('Ctrl Pts',(-2.33517777320684,103.477508758949,14.2157209686054));
#42985=CARTESIAN_POINT('Ctrl Pts',(-2.10502101028616,103.407673700546,14.6860208714818));
#42986=CARTESIAN_POINT('Ctrl Pts',(-1.91075366020395,103.365019951847,14.9435301765248));
#42987=CARTESIAN_POINT('Ctrl Pts',(-1.42414626749157,103.277997202902,15.3818808592167));
#42988=CARTESIAN_POINT('Ctrl Pts',(-1.13238691184991,103.234822206233,15.5539218284624));
#42989=CARTESIAN_POINT('Ctrl Pts',(-0.662935492327526,103.169600803758,
15.715888693799));
#42990=CARTESIAN_POINT('Ctrl Pts',(-0.50576891308823,103.148428990443,15.7536098285557));
#42991=CARTESIAN_POINT('Ctrl Pts',(-0.0383727463709212,103.086589344291,
15.818938681796));
#42992=CARTESIAN_POINT('Ctrl Pts',(0.274691269532586,103.046981194232,15.8042209450093));
#42993=CARTESIAN_POINT('Ctrl Pts',(0.898423530583375,102.964585598428,15.6562504400845));
#42994=CARTESIAN_POINT('Ctrl Pts',(1.20151545297683,102.922364417971,15.5170816790616));
#42995=CARTESIAN_POINT('Ctrl Pts',(1.6012205823757,102.859086283876,15.2268823182098));
#42996=CARTESIAN_POINT('Ctrl Pts',(1.72389772965701,102.838265461855,15.1179560911702));
#42997=CARTESIAN_POINT('Ctrl Pts',(2.0570403779814,102.775777062402,14.7578862647492));
#42998=CARTESIAN_POINT('Ctrl Pts',(2.22984811558075,102.734636828213,14.4767125247071));
#42999=CARTESIAN_POINT('Ctrl Pts',(2.45981529442251,102.651181647567,13.8573876576525));
#43000=CARTESIAN_POINT('Ctrl Pts',(2.51217994755866,102.60966780587,13.5243963862876));
#43001=CARTESIAN_POINT('Ctrl Pts',(2.48301168831486,102.525953791866,12.8563736488223));
#43002=CARTESIAN_POINT('Ctrl Pts',(2.40132308282432,102.484624019053,12.5280985190173));
#43003=CARTESIAN_POINT('Ctrl Pts',(2.18792875470781,102.423077012594,12.0797160517702));
#43004=CARTESIAN_POINT('Ctrl Pts',(2.10447650457136,102.403142545388,11.940843048404));
#43005=CARTESIAN_POINT('Ctrl Pts',(1.81921790746521,102.344073768843,11.5561181098551));
#43006=CARTESIAN_POINT('Ctrl Pts',(1.5834170617546,102.305532688792,11.3395174198834));
#43007=CARTESIAN_POINT('Ctrl Pts',(1.02873179768248,102.225802055474,10.9970361940603));
#43008=CARTESIAN_POINT('Ctrl Pts',(0.711624302200728,102.185327693338,10.8801721773681));
#43009=CARTESIAN_POINT('Ctrl Pts',(0.227552725347762,102.126239798956,10.8055471516363));
#43010=CARTESIAN_POINT('Ctrl Pts',(0.0723278330722858,102.107652599778,
10.7962332615171));
#43011=CARTESIAN_POINT('Ctrl Pts',(-0.417079563898204,102.048926960579,
10.8124438502513));
#43012=CARTESIAN_POINT('Ctrl Pts',(-0.745819897061609,102.008947356071,
10.8905043375096));
#43013=CARTESIAN_POINT('Ctrl Pts',(-1.32291415776129,101.933310958461,11.1574142746825));
#43014=CARTESIAN_POINT('Ctrl Pts',(-1.57128153623215,101.898363766591,11.3322930818985));
#43015=CARTESIAN_POINT('Ctrl Pts',(-2.018280835674,101.823342126679,11.7868652511051));
#43016=CARTESIAN_POINT('Ctrl Pts',(-2.20328270803896,101.783936534117,12.0717320386843));
#43017=CARTESIAN_POINT('Ctrl Pts',(-2.44116137868579,101.708842047491,12.6763330895868));
#43018=CARTESIAN_POINT('Ctrl Pts',(-2.5,101.673389006817,12.986866730166));
#43019=CARTESIAN_POINT('Ctrl Pts',(-2.5,101.637207465761,13.3));
#43020=CARTESIAN_POINT('Origin',(0.,70.2,13.3));
#43021=CARTESIAN_POINT('',(2.49284186651808,100.7945130522,13.1110770588995));
#43022=CARTESIAN_POINT('Ctrl Pts',(-2.5,101.637207465761,13.3));
#43023=CARTESIAN_POINT('Ctrl Pts',(-2.5,101.635397107763,13.3156677494368));
#43024=CARTESIAN_POINT('Ctrl Pts',(-2.4998527135231,101.633586332796,13.3313421699356));
#43025=CARTESIAN_POINT('Ctrl Pts',(-2.49397575294634,101.597501416344,13.6437498288163));
#43026=CARTESIAN_POINT('Ctrl Pts',(-2.43559995242375,101.563958202291,13.9371851059678));
#43027=CARTESIAN_POINT('Ctrl Pts',(-2.26975677891009,101.513235154397,14.3596381439182));
#43028=CARTESIAN_POINT('Ctrl Pts',(-2.19878289690343,101.495853589453,14.4999917288581));
#43029=CARTESIAN_POINT('Ctrl Pts',(-1.93995342605789,101.441357413942,14.9107605021292));
#43030=CARTESIAN_POINT('Ctrl Pts',(-1.71162696691703,101.404443533433,15.1515939579269));
#43031=CARTESIAN_POINT('Ctrl Pts',(-1.177653286629,101.333066457237,15.5291010900195));
#43032=CARTESIAN_POINT('Ctrl Pts',(-0.877994267335959,101.298563133645,
15.6632353312194));
#43033=CARTESIAN_POINT('Ctrl Pts',(-0.272708342417149,101.230749095566,
15.8026397347157));
#43034=CARTESIAN_POINT('Ctrl Pts',(0.0252665497621781,101.199320408508,
15.8173478379036));
#43035=CARTESIAN_POINT('Ctrl Pts',(0.476193706233752,101.152163356072,15.75934411446));
#43036=CARTESIAN_POINT('Ctrl Pts',(0.631147494318057,101.135950172377,15.7242077588106));
#43037=CARTESIAN_POINT('Ctrl Pts',(1.09075440636581,101.085495612883,15.5729065029533));
#43038=CARTESIAN_POINT('Ctrl Pts',(1.37712231785397,101.051274244471,15.4117616857425));
#43039=CARTESIAN_POINT('Ctrl Pts',(1.86579795875028,100.98715374067,14.9939624038972));
#43040=CARTESIAN_POINT('Ctrl Pts',(2.06556533212102,100.956976682237,14.7436608799853));
#43041=CARTESIAN_POINT('Ctrl Pts',(2.32950750604381,100.900678241366,14.2412607707093));
#43042=CARTESIAN_POINT('Ctrl Pts',(2.41199748374071,100.876406442244,14.0035179645452));
#43043=CARTESIAN_POINT('Ctrl Pts',(2.49744258256006,100.833213788839,13.5443911621765));
#43044=CARTESIAN_POINT('Ctrl Pts',(2.50922496440789,100.814139396728,13.3271443744556));
#43045=CARTESIAN_POINT('Ctrl Pts',(2.49285252681543,100.794505242158,13.1110918753734));
#43046=CARTESIAN_POINT('',(-2.5,99.7536786153901,13.299999999524));
#43047=CARTESIAN_POINT('Ctrl Pts',(2.49285672356711,100.794015874192,13.11114726434));
#43048=CARTESIAN_POINT('Ctrl Pts',(2.47466985079183,100.759178937447,12.8710804846872));
#43049=CARTESIAN_POINT('Ctrl Pts',(2.42189355944945,100.724522436754,12.6348159025486));
#43050=CARTESIAN_POINT('Ctrl Pts',(2.23933715036676,100.652368551319,12.1557982714085));
#43051=CARTESIAN_POINT('Ctrl Pts',(2.10182163062156,100.615009546234,11.9193494988057));
#43052=CARTESIAN_POINT('Ctrl Pts',(1.73674877950707,100.534417987845,11.4765436645856));
#43053=CARTESIAN_POINT('Ctrl Pts',(1.50385865512308,100.491692324512,11.2801668860126));
#43054=CARTESIAN_POINT('Ctrl Pts',(0.950019201125868,100.403244092737,10.9632725006471));
#43055=CARTESIAN_POINT('Ctrl Pts',(0.627745662968607,100.358727928871,10.8568762769735));
#43056=CARTESIAN_POINT('Ctrl Pts',(-0.00524379688189826,100.271984632209,
10.7819049015937));
#43057=CARTESIAN_POINT('Ctrl Pts',(-0.308510598960716,100.230841405672,
10.8008641585676));
#43058=CARTESIAN_POINT('Ctrl Pts',(-0.926964154886148,100.145111588349,
10.9540581475074));
#43059=CARTESIAN_POINT('Ctrl Pts',(-1.23330514807368,100.101369766984,11.099607941249));
#43060=CARTESIAN_POINT('Ctrl Pts',(-1.74232012171602,100.016726577802,11.4820747650571));
#43061=CARTESIAN_POINT('Ctrl Pts',(-1.94829914608007,99.9768076775756,11.7047881115834));
#43062=CARTESIAN_POINT('Ctrl Pts',(-2.19621809152953,99.9161437038351,12.0947622126472));
#43063=CARTESIAN_POINT('Ctrl Pts',(-2.26933440606012,99.8952175210238,12.2388200231824));
#43064=CARTESIAN_POINT('Ctrl Pts',(-2.44169468599849,99.8337959262168,12.6792526037952));
#43065=CARTESIAN_POINT('Ctrl Pts',(-2.49999999988129,99.7937512872206,12.9882722440034));
#43066=CARTESIAN_POINT('Ctrl Pts',(-2.5,99.7536786153901,13.299999999048));
#43067=CARTESIAN_POINT('',(-2.5,100.556030878907,13.3000000000001));
#43068=CARTESIAN_POINT('',(-2.5,70.2,13.3));
#43069=CARTESIAN_POINT('',(-1.18065793506841,100.775168925174,11.0950388653619));
#43070=CARTESIAN_POINT('Ctrl Pts',(-2.5,100.556030878907,13.3000000000002));
#43071=CARTESIAN_POINT('Ctrl Pts',(-2.5,100.575712858969,13.0805393351909));
#43072=CARTESIAN_POINT('Ctrl Pts',(-2.47110612339189,100.593966114938,12.8617403493646));
#43073=CARTESIAN_POINT('Ctrl Pts',(-2.32687792948211,100.640854367325,12.3267623410781));
#43074=CARTESIAN_POINT('Ctrl Pts',(-2.17625108057745,100.672093072887,12.0250388790023));
#43075=CARTESIAN_POINT('Ctrl Pts',(-1.85782227860843,100.714049821671,11.6171010726225));
#43076=CARTESIAN_POINT('Ctrl Pts',(-1.72936686120991,100.727548384298,11.4853389758269));
#43077=CARTESIAN_POINT('Ctrl Pts',(-1.46093464308142,100.751543479388,11.2646786927412));
#43078=CARTESIAN_POINT('Ctrl Pts',(-1.32443223706636,100.762177989808,11.1733302526813));
#43079=CARTESIAN_POINT('Ctrl Pts',(-1.17998685155049,100.773580099726,11.0959965902549));
#43080=CARTESIAN_POINT('Ctrl Pts',(-1.18027058595304,100.77645823042,11.0961485204456));
#43081=CARTESIAN_POINT('Ctrl Pts',(-0.938059961197377,100.81973254846,10.9664328482887));
#43082=CARTESIAN_POINT('Ctrl Pts',(-0.67611969418476,100.863378555888,10.8775428772392));
#43083=CARTESIAN_POINT('Ctrl Pts',(-0.104371428946291,100.955455344403,
10.7836577628089));
#43084=CARTESIAN_POINT('Ctrl Pts',(0.20286109498074,101.001180411669,10.7896541673622));
#43085=CARTESIAN_POINT('Ctrl Pts',(0.800542765702973,101.09424520677,10.9120623848384));
#43086=CARTESIAN_POINT('Ctrl Pts',(1.08576786172926,101.14129542265,11.0275030476426));
#43087=CARTESIAN_POINT('Ctrl Pts',(1.62644534730514,101.237426863056,11.3719205629185));
#43088=CARTESIAN_POINT('Ctrl Pts',(1.87054137050352,101.284952813534,11.607661578119));
#43089=CARTESIAN_POINT('Ctrl Pts',(2.15217581987885,101.358294704342,12.017738384329));
#43090=CARTESIAN_POINT('Ctrl Pts',(2.23045716296475,101.38221229061,12.1593346989988));
#43091=CARTESIAN_POINT('Ctrl Pts',(2.4225117340961,101.453320984913,12.6033369942959));
#43092=CARTESIAN_POINT('Ctrl Pts',(2.49208268306385,101.498027246709,12.9211553592237));
#43093=CARTESIAN_POINT('Ctrl Pts',(2.5062718767786,101.587230943087,13.5495308111175));
#43094=CARTESIAN_POINT('Ctrl Pts',(2.45694119476446,101.631158355497,13.8541715994227));
#43095=CARTESIAN_POINT('Ctrl Pts',(2.29943054260782,101.696909554085,14.2943245697655));
#43096=CARTESIAN_POINT('Ctrl Pts',(2.23042958462874,101.719162545749,14.4407293777322));
#43097=CARTESIAN_POINT('Ctrl Pts',(2.06791841338335,101.763145315154,14.7135286666381));
#43098=CARTESIAN_POINT('Ctrl Pts',(1.975686937057,101.78476497561,14.8398065251242));
#43099=CARTESIAN_POINT('Ctrl Pts',(1.65122715615705,101.853115961513,15.2065003343976));
#43100=CARTESIAN_POINT('Ctrl Pts',(1.38230114422013,101.899447507771,15.4096596098744));
#43101=CARTESIAN_POINT('Ctrl Pts',(0.937253820472456,101.966521739436,15.6231650612652));
#43102=CARTESIAN_POINT('Ctrl Pts',(0.786868930602964,101.98811492698,15.6783138108469));
#43103=CARTESIAN_POINT('Ctrl Pts',(0.33232613258465,102.052110240557,15.7971308868413));
#43104=CARTESIAN_POINT('Ctrl Pts',(0.0204033351471258,102.094634362746,
15.8190696730077));
#43105=CARTESIAN_POINT('Ctrl Pts',(-0.619763219661474,102.1816384624,15.7449368552534));
#43106=CARTESIAN_POINT('Ctrl Pts',(-0.940905829217929,102.225509644986,
15.6402058495464));
#43107=CARTESIAN_POINT('Ctrl Pts',(-1.37113130501076,102.291810297129,15.3965651763402));
#43108=CARTESIAN_POINT('Ctrl Pts',(-1.50243774962431,102.313262476999,15.3045623869997));
#43109=CARTESIAN_POINT('Ctrl Pts',(-1.87849937890772,102.379344657656,14.983226876065));
#43110=CARTESIAN_POINT('Ctrl Pts',(-2.08673312877407,102.422754265075,14.7168978275346));
#43111=CARTESIAN_POINT('Ctrl Pts',(-2.31214659148409,102.489286959397,14.2657781400346));
#43112=CARTESIAN_POINT('Ctrl Pts',(-2.37231105861528,102.511632157536,14.1067798584379));
#43113=CARTESIAN_POINT('Ctrl Pts',(-2.47172208006199,102.562390571945,13.7332170211324));
#43114=CARTESIAN_POINT('Ctrl Pts',(-2.49999602821008,102.590349238264,13.5171226284436));
#43115=CARTESIAN_POINT('Ctrl Pts',(-2.49999999958163,102.61816441031,13.300045736922));
#43116=CARTESIAN_POINT('Origin',(0.,70.2,13.3));
#43117=CARTESIAN_POINT('',(-2.5,97.6537365388727,13.300000000061));
#43118=CARTESIAN_POINT('',(-2.5,98.7897650553754,13.3000000423409));
#43119=CARTESIAN_POINT('',(-2.5,70.2,13.3));
#43120=CARTESIAN_POINT('Ctrl Pts',(-2.5,98.7897650605138,13.3000000429739));
#43121=CARTESIAN_POINT('Ctrl Pts',(-2.50000000214343,98.8051272660355,13.1753065631474));
#43122=CARTESIAN_POINT('Ctrl Pts',(-2.4906708580659,98.8204518455014,13.0507235054539));
#43123=CARTESIAN_POINT('Ctrl Pts',(-2.44826568409266,98.855360827728,12.7694578365237));
#43124=CARTESIAN_POINT('Ctrl Pts',(-2.40940571355738,98.8748469893923,12.6142545421071));
#43125=CARTESIAN_POINT('Ctrl Pts',(-2.30198530466049,98.9141082339661,12.3115894708146));
#43126=CARTESIAN_POINT('Ctrl Pts',(-2.23333073527477,98.9338116246053,12.1649550451765));
#43127=CARTESIAN_POINT('Ctrl Pts',(-1.99098648642878,98.9918312786834,11.7557924829878));
#43128=CARTESIAN_POINT('Ctrl Pts',(-1.78147653231448,99.0295221164529,11.5181582930845));
#43129=CARTESIAN_POINT('Ctrl Pts',(-1.40529604856019,99.0873156968289,11.226000277956));
#43130=CARTESIAN_POINT('Ctrl Pts',(-1.26774449724101,99.1069517428578,11.1391760757682));
#43131=CARTESIAN_POINT('Ctrl Pts',(-0.841826558727321,99.1644754720802,
10.9250932985549));
#43132=CARTESIAN_POINT('Ctrl Pts',(-0.536762726704051,99.2017539995856,
10.8381397520154));
#43133=CARTESIAN_POINT('Ctrl Pts',(0.090611532668975,99.277260929085,10.781805010844));
#43134=CARTESIAN_POINT('Ctrl Pts',(0.407349129855685,99.3145103836881,10.8133136781569));
#43135=CARTESIAN_POINT('Ctrl Pts',(0.86206129970444,99.3707717314157,10.947970020182));
#43136=CARTESIAN_POINT('Ctrl Pts',(1.00962443647151,99.3894664737536,11.0074343217137));
#43137=CARTESIAN_POINT('Ctrl Pts',(1.44812432265774,99.4476893050727,11.2347451963873));
#43138=CARTESIAN_POINT('Ctrl Pts',(1.7116809425071,99.4870872328887,11.447291758789));
#43139=CARTESIAN_POINT('Ctrl Pts',(2.12328411387118,99.5622800556226,11.9443326462106));
#43140=CARTESIAN_POINT('Ctrl Pts',(2.27491957300927,99.5974259474615,12.2179098821064));
#43141=CARTESIAN_POINT('Ctrl Pts',(2.47778820378074,99.6717334494876,12.8289243550386));
#43142=CARTESIAN_POINT('Ctrl Pts',(2.51848056897162,99.7111296876756,13.1634850240867));
#43143=CARTESIAN_POINT('Ctrl Pts',(2.47008131417638,99.7815387857339,13.7783123624695));
#43144=CARTESIAN_POINT('Ctrl Pts',(2.40013715673431,99.8123662283287,14.0546164279131));
#43145=CARTESIAN_POINT('Ctrl Pts',(2.1502067743619,99.8811201682489,14.6182859862622));
#43146=CARTESIAN_POINT('Ctrl Pts',(1.9553652950623,99.9198991317864,14.8930460892253));
#43147=CARTESIAN_POINT('Ctrl Pts',(1.50949062916033,99.9882133066538,15.3122017106855));
#43148=CARTESIAN_POINT('Ctrl Pts',(1.27619852477342,100.017630055568,15.467689370579));
#43149=CARTESIAN_POINT('Ctrl Pts',(0.717247206038844,100.083273518722,15.7180768763258));
#43150=CARTESIAN_POINT('Ctrl Pts',(0.388176065348154,100.119902847992,15.7921610004401));
#43151=CARTESIAN_POINT('Ctrl Pts',(-0.271248184284303,100.19020796814,15.8064786470139));
#43152=CARTESIAN_POINT('Ctrl Pts',(-0.595071393621657,100.22463495625,15.749887798597));
#43153=CARTESIAN_POINT('Ctrl Pts',(-1.05125249761847,100.275694322305,15.5740946185112));
#43154=CARTESIAN_POINT('Ctrl Pts',(-1.19744680120775,100.292753612668,15.5006286895925));
#43155=CARTESIAN_POINT('Ctrl Pts',(-1.59818476697444,100.341714161852,15.2474094550559));
#43156=CARTESIAN_POINT('Ctrl Pts',(-1.82772321634462,100.37297117758,15.0338042070319));
#43157=CARTESIAN_POINT('Ctrl Pts',(-2.1933156268446,100.434384186937,14.5379426114997));
#43158=CARTESIAN_POINT('Ctrl Pts',(-2.32794606981634,100.463422938872,14.2611769303796));
#43159=CARTESIAN_POINT('Ctrl Pts',(-2.45202071822513,100.508032718833,13.8129609280056));
#43160=CARTESIAN_POINT('Ctrl Pts',(-2.47979654466681,100.523353891658,13.6551931589905));
#43161=CARTESIAN_POINT('Ctrl Pts',(-2.49744451782718,100.544218754017,13.4305894947812));
#43162=CARTESIAN_POINT('Ctrl Pts',(-2.5,100.550177730551,13.3652645630937));
#43163=CARTESIAN_POINT('Ctrl Pts',(-2.5,100.556030878907,13.3000000000002));
#43164=CARTESIAN_POINT('',(1.85693809316476,98.5858197253477,11.6266881416021));
#43165=CARTESIAN_POINT('Ctrl Pts',(-2.5,99.7536786153901,13.299999999048));
#43166=CARTESIAN_POINT('Ctrl Pts',(-2.50000000000205,99.7529871031884,13.3053793145855));
#43167=CARTESIAN_POINT('Ctrl Pts',(-2.49998263778621,99.7522955829396,13.3107594365981));
#43168=CARTESIAN_POINT('Ctrl Pts',(-2.49886417546877,99.7300314983695,13.4839966483087));
#43169=CARTESIAN_POINT('Ctrl Pts',(-2.48087730636317,99.708595350066,13.6513255859644));
#43170=CARTESIAN_POINT('Ctrl Pts',(-2.4130122730618,99.6665343858624,13.9733155581015));
#43171=CARTESIAN_POINT('Ctrl Pts',(-2.36459163132424,99.6460111796206,14.1274611634218));
#43172=CARTESIAN_POINT('Ctrl Pts',(-2.17142198877263,99.5830262880744,14.5830657591208));
#43173=CARTESIAN_POINT('Ctrl Pts',(-1.98097237446091,99.5413281492994,14.8611303351601));
#43174=CARTESIAN_POINT('Ctrl Pts',(-1.50488730504586,99.4580955184984,15.3233915873593));
#43175=CARTESIAN_POINT('Ctrl Pts',(-1.22506645736199,99.4173386990936,15.5040984827822));
#43176=CARTESIAN_POINT('Ctrl Pts',(-0.770752212604174,99.356807626939,15.6835012772582));
#43177=CARTESIAN_POINT('Ctrl Pts',(-0.618072616570848,99.3372697100055,
15.7275767246838));
#43178=CARTESIAN_POINT('Ctrl Pts',(-0.140620197266651,99.2774807068649,
15.8174051103642));
#43179=CARTESIAN_POINT('Ctrl Pts',(0.189803133257262,99.2378372422568,15.8141821376149));
#43180=CARTESIAN_POINT('Ctrl Pts',(0.665595919586561,99.1787152582534,15.7149884669689));
#43181=CARTESIAN_POINT('Ctrl Pts',(0.817533069576632,99.1595297038779,15.6678752431131));
#43182=CARTESIAN_POINT('Ctrl Pts',(1.1118761690379,99.1210583390881,15.544866071418));
#43183=CARTESIAN_POINT('Ctrl Pts',(1.25348934389529,99.101862958593,15.4689770455246));
#43184=CARTESIAN_POINT('Ctrl Pts',(1.66685831342957,99.0423367829859,15.1933650357196));
#43185=CARTESIAN_POINT('Ctrl Pts',(1.90632908056946,99.0025134688997,14.9520317040624));
#43186=CARTESIAN_POINT('Ctrl Pts',(2.179981716146,98.9436737025004,14.5345489450462));
#43187=CARTESIAN_POINT('Ctrl Pts',(2.25563508912969,98.9246597486341,14.3902042183656));
#43188=CARTESIAN_POINT('Ctrl Pts',(2.43966574363723,98.8672341310013,13.9364148628871));
#43189=CARTESIAN_POINT('Ctrl Pts',(2.5019341340693,98.8293628637644,13.6120529936428));
#43190=CARTESIAN_POINT('Ctrl Pts',(2.49903474331672,98.7742921815908,13.1329263785518));
#43191=CARTESIAN_POINT('Ctrl Pts',(2.48426450572032,98.7569600705699,12.9813778565468));
#43192=CARTESIAN_POINT('Ctrl Pts',(2.41162109407947,98.712498421881,12.6000940934995));
#43193=CARTESIAN_POINT('Ctrl Pts',(2.33475495555389,98.6855918690322,12.3754851169304));
#43194=CARTESIAN_POINT('Ctrl Pts',(2.12817714561673,98.6342832714491,11.9700655205455));
#43195=CARTESIAN_POINT('Ctrl Pts',(2.00368739954201,98.6100544090427,11.7890026644713));
#43196=CARTESIAN_POINT('Ctrl Pts',(1.85721457609527,98.5856828656957,11.6264546560253));
#43197=CARTESIAN_POINT('',(-2.49956101882259,97.6535864963121,13.298861354865));
#43198=CARTESIAN_POINT('Ctrl Pts',(1.85690960710508,98.5856773324862,11.6267152159055));
#43199=CARTESIAN_POINT('Ctrl Pts',(1.8077250499098,98.5731300683111,11.5720968634514));
#43200=CARTESIAN_POINT('Ctrl Pts',(1.75634066847637,98.560755922621,11.5196760589334));
#43201=CARTESIAN_POINT('Ctrl Pts',(1.70281770841323,98.5483499926756,11.4697088541542));
#43202=CARTESIAN_POINT('Ctrl Pts',(1.69221343839639,98.5458920600277,11.4598090703821));
#43203=CARTESIAN_POINT('Ctrl Pts',(1.68152525336647,98.5434329006297,11.4500057589624));
#43204=CARTESIAN_POINT('Ctrl Pts',(1.67075368875989,98.5409709520606,11.4403011455887));
#43205=CARTESIAN_POINT('Ctrl Pts',(1.60526395387986,98.5260026196997,11.3812983377171));
#43206=CARTESIAN_POINT('Ctrl Pts',(1.53678119562569,98.5111050743696,11.3258301785802));
#43207=CARTESIAN_POINT('Ctrl Pts',(1.46555679140617,98.4962988036746,11.2741434922838));
#43208=CARTESIAN_POINT('Ctrl Pts',(1.39433238718665,98.4814925329796,11.2224568059874));
#43209=CARTESIAN_POINT('Ctrl Pts',(1.32036646695919,98.466777901265,11.1745506420625));
#43210=CARTESIAN_POINT('Ctrl Pts',(1.24386760259586,98.4521967174326,11.1306839680054));
#43211=CARTESIAN_POINT('Ctrl Pts',(1.24384665438821,98.4521927245672,11.1306719556938));
#43212=CARTESIAN_POINT('Ctrl Pts',(1.24382570599033,98.4521887317119,11.1306599436852));
#43213=CARTESIAN_POINT('Ctrl Pts',(1.24380475740234,98.4521847388666,11.1306479319799));
#43214=CARTESIAN_POINT('Ctrl Pts',(1.18362787507212,98.4407148975493,11.0961431253399));
#43215=CARTESIAN_POINT('Ctrl Pts',(1.12188171434896,98.4293278778844,11.0641378362799));
#43216=CARTESIAN_POINT('Ctrl Pts',(1.05873497356869,98.4179752887785,11.034710939003));
#43217=CARTESIAN_POINT('Ctrl Pts',(0.980190438086826,98.4038544675482,10.9981085435549));
#43218=CARTESIAN_POINT('Ctrl Pts',(0.899887840407072,98.3898595702403,10.9656844771038));
#43219=CARTESIAN_POINT('Ctrl Pts',(0.81820808033838,98.3759192694801,10.9374911360008));
#43220=CARTESIAN_POINT('Ctrl Pts',(0.735155417917374,98.3617446552048,10.9088239112295));
#43221=CARTESIAN_POINT('Ctrl Pts',(0.650678671048983,98.3476263482223,10.8845311962933));
#43222=CARTESIAN_POINT('Ctrl Pts',(0.56516518123011,98.3335200054256,10.8646907338479));
#43223=CARTESIAN_POINT('Ctrl Pts',(0.479335393357447,98.3193614859631,10.8447768853243));
#43224=CARTESIAN_POINT('Ctrl Pts',(0.392461224071964,98.305215056977,10.8293484093262));
#43225=CARTESIAN_POINT('Ctrl Pts',(0.304922580453783,98.2910671650078,10.8185025756208));
#43226=CARTESIAN_POINT('Ctrl Pts',(0.23434772347413,98.2796609401565,10.8097585155012));
#43227=CARTESIAN_POINT('Ctrl Pts',(0.163340782647186,98.2682544039755,10.803993323425));
#43228=CARTESIAN_POINT('Ctrl Pts',(0.0920946306619685,98.2568545880395,
10.8012672213045));
#43229=CARTESIAN_POINT('Ctrl Pts',(0.0087673670571682,98.2435217210554,
10.7980788578116));
#43230=CARTESIAN_POINT('Ctrl Pts',(-0.0744698003503501,98.230263849956,
10.7990633229069));
#43231=CARTESIAN_POINT('Ctrl Pts',(-0.157327380642784,98.2171110235674,
10.8042089214701));
#43232=CARTESIAN_POINT('Ctrl Pts',(-0.162465995246597,98.2162953190112,
10.8045280382948));
#43233=CARTESIAN_POINT('Ctrl Pts',(-0.167603159750644,98.2154800177744,
10.8048631728795));
#43234=CARTESIAN_POINT('Ctrl Pts',(-0.172738808847055,98.2146651267462,
10.8052143278411));
#43235=CARTESIAN_POINT('Ctrl Pts',(-0.231902192624619,98.2052774700482,
10.8092596812852));
#43236=CARTESIAN_POINT('Ctrl Pts',(-0.290863988911329,98.1959448621742,
10.8154295879729));
#43237=CARTESIAN_POINT('Ctrl Pts',(-0.349529404896252,98.186682902991,10.8237293448082));
#43238=CARTESIAN_POINT('Ctrl Pts',(-0.349566423542153,98.1866770585734,
10.8237345820635));
#43239=CARTESIAN_POINT('Ctrl Pts',(-0.349603442069974,98.1866712141838,
10.8237398201674));
#43240=CARTESIAN_POINT('Ctrl Pts',(-0.349640460479707,98.1866653698222,
10.8237450591199));
#43241=CARTESIAN_POINT('Ctrl Pts',(-0.435420835414029,98.173122607364,10.8358849460904));
#43242=CARTESIAN_POINT('Ctrl Pts',(-0.520569872626937,98.1597297385198,
10.8525773729019));
#43243=CARTESIAN_POINT('Ctrl Pts',(-0.604757739420849,98.1463938881941,
10.8737062199925));
#43244=CARTESIAN_POINT('Ctrl Pts',(-0.690177587505622,98.1328628848288,
10.8951442606201));
#43245=CARTESIAN_POINT('Ctrl Pts',(-0.774608104153329,98.1193902428782,
10.9211504533214));
#43246=CARTESIAN_POINT('Ctrl Pts',(-0.857675979165781,98.1059045094002,
10.9516283315024));
#43247=CARTESIAN_POINT('Ctrl Pts',(-0.867543590611796,98.1043025425988,
10.95524879079));
#43248=CARTESIAN_POINT('Ctrl Pts',(-0.877391939972514,98.1027004235435,
10.9589323693656));
#43249=CARTESIAN_POINT('Ctrl Pts',(-0.8872203744183,98.1010980591305,10.9626789196573));
#43250=CARTESIAN_POINT('Ctrl Pts',(-0.969282088609672,98.0877192477634,
10.9939604366615));
#43251=CARTESIAN_POINT('Ctrl Pts',(-1.04952459558973,98.0743905233542,11.0294665444871));
#43252=CARTESIAN_POINT('Ctrl Pts',(-1.12761912194777,98.0610745687717,11.0689869248279));
#43253=CARTESIAN_POINT('Ctrl Pts',(-1.20649254011099,98.0476258047801,11.1089014698024));
#43254=CARTESIAN_POINT('Ctrl Pts',(-1.28317473152672,98.0341901899186,11.1529106546193));
#43255=CARTESIAN_POINT('Ctrl Pts',(-1.35733332410368,98.0207589852649,11.2008200181214));
#43256=CARTESIAN_POINT('Ctrl Pts',(-1.43093441808567,98.0074287517525,11.2483692156344));
#43257=CARTESIAN_POINT('Ctrl Pts',(-1.50204983803708,97.9941031558961,11.2997597484355));
#43258=CARTESIAN_POINT('Ctrl Pts',(-1.57036148504395,97.9807995009096,11.3548272860642));
#43259=CARTESIAN_POINT('Ctrl Pts',(-1.62464458227933,97.9702278981324,11.3985860977835));
#43260=CARTESIAN_POINT('Ctrl Pts',(-1.6771575261111,97.9596707221894,11.4446671003648));
#43261=CARTESIAN_POINT('Ctrl Pts',(-1.72774177335385,97.9491463647847,11.4930030452226));
#43262=CARTESIAN_POINT('Ctrl Pts',(-1.75106323781302,97.9442941935941,11.5152879477672));
#43263=CARTESIAN_POINT('Ctrl Pts',(-1.77392982658307,97.9394584790718,11.5380094279285));
#43264=CARTESIAN_POINT('Ctrl Pts',(-1.79633105271662,97.9346413679592,11.56115692621));
#43265=CARTESIAN_POINT('Ctrl Pts',(-1.79633402503211,97.934640728799,11.5611599975449));
#43266=CARTESIAN_POINT('Ctrl Pts',(-1.79633699733939,97.934640089639,11.5611630688873));
#43267=CARTESIAN_POINT('Ctrl Pts',(-1.79633996963847,97.9346394504794,11.5611661402372));
#43268=CARTESIAN_POINT('Ctrl Pts',(-1.85648744176362,97.9217054101724,11.6233180056473));
#43269=CARTESIAN_POINT('Ctrl Pts',(-1.91328231390543,97.908903295095,11.6885410519733));
#43270=CARTESIAN_POINT('Ctrl Pts',(-1.96654495350802,97.8961492911077,11.7565102147902));
#43271=CARTESIAN_POINT('Ctrl Pts',(-2.02072536299437,97.8831755225567,11.8256505559625));
#43272=CARTESIAN_POINT('Ctrl Pts',(-2.07125007841324,97.8702513400781,11.8976329408409));
#43273=CARTESIAN_POINT('Ctrl Pts',(-2.11790735285553,97.8573194023268,11.9721188703281));
#43274=CARTESIAN_POINT('Ctrl Pts',(-2.16480499076845,97.8443208433362,12.046988527685));
#43275=CARTESIAN_POINT('Ctrl Pts',(-2.20779465421926,97.8313144343512,12.1243875209184));
#43276=CARTESIAN_POINT('Ctrl Pts',(-2.24664854939422,97.8182743953918,12.2039727074303));
#43277=CARTESIAN_POINT('Ctrl Pts',(-2.26366933039734,97.8125619270177,12.2388367030377));
#43278=CARTESIAN_POINT('Ctrl Pts',(-2.27989631894334,97.8068434236944,12.2741202603897));
#43279=CARTESIAN_POINT('Ctrl Pts',(-2.29530993377528,97.8011186409183,12.3097947551504));
#43280=CARTESIAN_POINT('Ctrl Pts',(-2.33044684477994,97.7880684132385,12.391118413566));
#43281=CARTESIAN_POINT('Ctrl Pts',(-2.3611719920498,97.7750529178162,12.4740419297995));
#43282=CARTESIAN_POINT('Ctrl Pts',(-2.38739168035197,97.7620898280361,12.5581907883444));
#43283=CARTESIAN_POINT('Ctrl Pts',(-2.41181656453723,97.7500140946059,12.6365794442504));
#43284=CARTESIAN_POINT('Ctrl Pts',(-2.43233211720112,97.7379841771657,12.7160315578295));
#43285=CARTESIAN_POINT('Ctrl Pts',(-2.44886153498619,97.7260327698438,12.7962804586082));
#43286=CARTESIAN_POINT('Ctrl Pts',(-2.45007079496971,97.7251584281816,12.8021513117559));
#43287=CARTESIAN_POINT('Ctrl Pts',(-2.4512587063564,97.7242845053269,12.8080264474667));
#43288=CARTESIAN_POINT('Ctrl Pts',(-2.45242523195955,97.7234110134226,12.8139057696976));
#43289=CARTESIAN_POINT('Ctrl Pts',(-2.46681732935069,97.7126342413359,12.8864423500451));
#43290=CARTESIAN_POINT('Ctrl Pts',(-2.47795721570267,97.7019238513227,12.9596138246261));
#43291=CARTESIAN_POINT('Ctrl Pts',(-2.48577639666548,97.6913126183989,13.033253105027));
#43292=CARTESIAN_POINT('Ctrl Pts',(-2.48577675208907,97.6913121360617,13.0332564523261));
#43293=CARTESIAN_POINT('Ctrl Pts',(-2.48577710750579,97.6913116537246,13.0332597996261));
#43294=CARTESIAN_POINT('Ctrl Pts',(-2.48577746291565,97.6913111713877,13.0332631469272));
#43295=CARTESIAN_POINT('Ctrl Pts',(-2.49401981843078,97.680125235194,13.110890833956));
#43296=CARTESIAN_POINT('Ctrl Pts',(-2.49857267927591,97.6690489749956,13.1890433458736));
#43297=CARTESIAN_POINT('Ctrl Pts',(-2.49941994343173,97.6580017020404,13.2674859930955));
#43298=CARTESIAN_POINT('Ctrl Pts',(-2.49946891720529,97.6573631448202,13.2720201545092));
#43299=CARTESIAN_POINT('Ctrl Pts',(-2.49950549973951,97.6567246856369,13.2765552753999));
#43300=CARTESIAN_POINT('Ctrl Pts',(-2.49952968419203,97.6560863093464,13.2810913066838));
#43301=CARTESIAN_POINT('Ctrl Pts',(-2.49956126834484,97.6552526095017,13.2870152243378));
#43302=CARTESIAN_POINT('Ctrl Pts',(-2.49957170282008,97.6544193477551,13.2929386213973));
#43303=CARTESIAN_POINT('Ctrl Pts',(-2.49956101882259,97.6535864963121,13.298861354865));
#43304=CARTESIAN_POINT('Ctrl Pts',(-2.49999975973186,97.6538889287948,13.2989039431398));
#43305=CARTESIAN_POINT('Ctrl Pts',(-2.49999991991164,97.6538381304678,13.2992692977425));
#43306=CARTESIAN_POINT('Ctrl Pts',(-2.50000000000002,97.6537873338306,13.2996346500787));
#43307=CARTESIAN_POINT('Ctrl Pts',(-2.5,97.6537365388727,13.3000000001219));
#43308=CARTESIAN_POINT('Origin',(0.,70.2,13.3));
#43309=CARTESIAN_POINT('',(-2.5,95.5986983740631,13.2999999999961));
#43310=CARTESIAN_POINT('',(-2.5,96.7549279855909,13.2999999999447));
#43311=CARTESIAN_POINT('',(-2.5,70.2,13.3));
#43312=CARTESIAN_POINT('',(-2.49999986066494,96.7550430853858,13.2991653292544));
#43313=CARTESIAN_POINT('Ctrl Pts',(-2.5,96.7549279855909,13.2999999998894));
#43314=CARTESIAN_POINT('Ctrl Pts',(-2.49999999999999,96.7549668066987,13.2997184759693));
#43315=CARTESIAN_POINT('Ctrl Pts',(-2.499999954658,96.7550042625919,13.2994468565905));
#43316=CARTESIAN_POINT('Ctrl Pts',(-2.49999986066494,96.7550430853858,13.2991653292544));
#43317=CARTESIAN_POINT('Ctrl Pts',(-2.49999986066494,96.7550430853858,13.2991653292544));
#43318=CARTESIAN_POINT('Ctrl Pts',(-2.4999048220303,96.7942977431784,13.0145062890155));
#43319=CARTESIAN_POINT('Ctrl Pts',(-2.45119641016012,96.8342362093599,12.7319672350244));
#43320=CARTESIAN_POINT('Ctrl Pts',(-2.24580299791176,96.9182776615934,12.1533329620363));
#43321=CARTESIAN_POINT('Ctrl Pts',(-2.07536145657939,96.961638181301,11.867721059664));
#43322=CARTESIAN_POINT('Ctrl Pts',(-1.70534736711559,97.0370430385601,11.4584834123906));
#43323=CARTESIAN_POINT('Ctrl Pts',(-1.53496590298137,97.0676330581365,11.3142279371448));
#43324=CARTESIAN_POINT('Ctrl Pts',(-1.06376103659421,97.1429442871494,11.0126211563722));
#43325=CARTESIAN_POINT('Ctrl Pts',(-0.745874945772812,97.1864051895193,
10.890136629139));
#43326=CARTESIAN_POINT('Ctrl Pts',(-0.2614463808509,97.2520668212153,10.808950743721));
#43327=CARTESIAN_POINT('Ctrl Pts',(-0.107656360007522,97.2727323842445,
10.7975835750841));
#43328=CARTESIAN_POINT('Ctrl Pts',(0.368999568794703,97.3366120753734,10.8063924363503));
#43329=CARTESIAN_POINT('Ctrl Pts',(0.687640674119482,97.3784385152547,10.8748312297851));
#43330=CARTESIAN_POINT('Ctrl Pts',(1.12953003033371,97.4416803229475,11.0641423801631));
#43331=CARTESIAN_POINT('Ctrl Pts',(1.26836582571434,97.4624317716116,11.1398730102519));
#43332=CARTESIAN_POINT('Ctrl Pts',(1.53637440812764,97.5047924201444,11.320864607133));
#43333=CARTESIAN_POINT('Ctrl Pts',(1.66407019271966,97.5262914635495,11.4269549133227));
#43334=CARTESIAN_POINT('Ctrl Pts',(1.89442578477539,97.5691004210316,11.6606219903953));
#43335=CARTESIAN_POINT('Ctrl Pts',(1.99695763875969,97.5903017820097,11.7871985510204));
#43336=CARTESIAN_POINT('Ctrl Pts',(2.26999867043505,97.6550460335004,12.2008667524305));
#43337=CARTESIAN_POINT('Ctrl Pts',(2.396117148237,97.6975554606845,12.5128257932262));
#43338=CARTESIAN_POINT('Ctrl Pts',(2.48662776819297,97.7612196066646,12.9967060763603));
#43339=CARTESIAN_POINT('Ctrl Pts',(2.50088558516876,97.7817796272842,13.1555073472334));
#43340=CARTESIAN_POINT('Ctrl Pts',(2.49900506359339,97.8233510810348,13.4778209951536));
#43341=CARTESIAN_POINT('Ctrl Pts',(2.48206732363548,97.844233587277,13.6405767748455));
#43342=CARTESIAN_POINT('Ctrl Pts',(2.38754758700351,97.9048166049424,14.1031239518931));
#43343=CARTESIAN_POINT('Ctrl Pts',(2.27016509505655,97.9442452537162,14.3916775207734));
#43344=CARTESIAN_POINT('Ctrl Pts',(2.01166848824739,98.0052587730919,14.7939351977878));
#43345=CARTESIAN_POINT('Ctrl Pts',(1.90593033739705,98.0267429784756,14.9266787869341));
#43346=CARTESIAN_POINT('Ctrl Pts',(1.67387596686174,98.0690202143734,15.1640275240825));
#43347=CARTESIAN_POINT('Ctrl Pts',(1.54907843914706,98.0897042238692,15.268963261203));
#43348=CARTESIAN_POINT('Ctrl Pts',(1.28379776255734,98.1306363590377,15.4510883205238));
#43349=CARTESIAN_POINT('Ctrl Pts',(1.14431833258083,98.1507581395254,15.5284202670932));
#43350=CARTESIAN_POINT('Ctrl Pts',(0.695788205789993,98.21269066934,15.7238097878825));
#43351=CARTESIAN_POINT('Ctrl Pts',(0.369995281367472,98.2540823150316,15.7944124734551));
#43352=CARTESIAN_POINT('Ctrl Pts',(-0.124078022263904,98.3163559804903,
15.8022990562058));
#43353=CARTESIAN_POINT('Ctrl Pts',(-0.287921324138257,98.3369323485032,
15.7887747607542));
#43354=CARTESIAN_POINT('Ctrl Pts',(-0.777776827461194,98.3994949808555,
15.6992892043637));
#43355=CARTESIAN_POINT('Ctrl Pts',(-1.09097785132098,98.4409096251606,15.5740518226424));
#43356=CARTESIAN_POINT('Ctrl Pts',(-1.62791708018648,98.5211033674332,15.2221710225551));
#43357=CARTESIAN_POINT('Ctrl Pts',(-1.85212484969452,98.5591586581678,15.0071914751938));
#43358=CARTESIAN_POINT('Ctrl Pts',(-2.12518501545708,98.6174049447581,14.626411606301));
#43359=CARTESIAN_POINT('Ctrl Pts',(-2.20596720111262,98.6372923791233,14.4872196738139));
#43360=CARTESIAN_POINT('Ctrl Pts',(-2.40442423974478,98.696314506151,14.0540238557462));
#43361=CARTESIAN_POINT('Ctrl Pts',(-2.48038171310186,98.7349138964142,13.7444405524168));
#43362=CARTESIAN_POINT('Ctrl Pts',(-2.49889197968721,98.7791722189695,13.3859597485197));
#43363=CARTESIAN_POINT('Ctrl Pts',(-2.49999999926131,98.7844707629695,13.3429733245846));
#43364=CARTESIAN_POINT('Ctrl Pts',(-2.5,98.7897650605139,13.3000000429739));
#43365=CARTESIAN_POINT('Ctrl Pts',(-2.5,97.6537365388727,13.3000000001219));
#43366=CARTESIAN_POINT('Ctrl Pts',(-2.49999999999076,97.627401975356,13.4894151372761));
#43367=CARTESIAN_POINT('Ctrl Pts',(-2.4784747780135,97.6014402125008,13.67820302557));
#43368=CARTESIAN_POINT('Ctrl Pts',(-2.40177725317404,97.5536409027924,14.0101859651423));
#43369=CARTESIAN_POINT('Ctrl Pts',(-2.35441017643867,97.5321493679576,14.1541811575294));
#43370=CARTESIAN_POINT('Ctrl Pts',(-2.192399226816,97.4733058212946,14.5285183068175));
#43371=CARTESIAN_POINT('Ctrl Pts',(-2.05480027994648,97.4355934204874,14.7469513949122));
#43372=CARTESIAN_POINT('Ctrl Pts',(-1.67493578681359,97.3527118660193,15.1837187278098));
#43373=CARTESIAN_POINT('Ctrl Pts',(-1.41852849998166,97.3100120024059,15.3836717135531));
#43374=CARTESIAN_POINT('Ctrl Pts',(-0.836152786389093,97.2206086767106,
15.6791168348764));
#43375=CARTESIAN_POINT('Ctrl Pts',(-0.514540246449376,97.174495855927,15.7687012573328));
#43376=CARTESIAN_POINT('Ctrl Pts',(0.0509460299849206,97.0952246912926,
15.8106474016969));
#43377=CARTESIAN_POINT('Ctrl Pts',(0.288229664456515,97.0630785404824,15.7945929786411));
#43378=CARTESIAN_POINT('Ctrl Pts',(0.847849911368506,96.9875772773639,15.6756260792212));
#43379=CARTESIAN_POINT('Ctrl Pts',(1.15847714094599,96.9444677987102,15.540619152968));
#43380=CARTESIAN_POINT('Ctrl Pts',(1.70390832761623,96.8557277708046,15.1589874242792));
#43381=CARTESIAN_POINT('Ctrl Pts',(1.93442436709792,96.8112368601696,14.9177806471101));
#43382=CARTESIAN_POINT('Ctrl Pts',(2.19482873235114,96.747557840951,14.5070674152662));
#43383=CARTESIAN_POINT('Ctrl Pts',(2.26579713673052,96.7274806900131,14.3679232083318));
#43384=CARTESIAN_POINT('Ctrl Pts',(2.43940956666114,96.6667595832406,13.9309409165425));
#43385=CARTESIAN_POINT('Ctrl Pts',(2.49932457427662,96.6263279190135,13.6195785155601));
#43386=CARTESIAN_POINT('Ctrl Pts',(2.50071024216123,96.5409121595066,12.9694116703955));
#43387=CARTESIAN_POINT('Ctrl Pts',(2.43371445754413,96.4970067633686,12.6367081648662));
#43388=CARTESIAN_POINT('Ctrl Pts',(2.17706364847366,96.412042208916,12.0291557188249));
#43389=CARTESIAN_POINT('Ctrl Pts',(1.99451233046105,96.3711267612373,11.7583759989667));
#43390=CARTESIAN_POINT('Ctrl Pts',(1.53615472367558,96.2884946343016,11.3012299239407));
#43391=CARTESIAN_POINT('Ctrl Pts',(1.26461108592141,96.2475172110001,11.1192575230292));
#43392=CARTESIAN_POINT('Ctrl Pts',(0.659213540111815,96.1644262521489,10.8656613387087));
#43393=CARTESIAN_POINT('Ctrl Pts',(0.329919297730919,96.1231293188218,10.7996487205787));
#43394=CARTESIAN_POINT('Ctrl Pts',(-0.271650992945435,96.0477807689548,
10.8002866753478));
#43395=CARTESIAN_POINT('Ctrl Pts',(-0.53886072686419,96.0143725009609,10.8439866649088));
#43396=CARTESIAN_POINT('Ctrl Pts',(-0.930947777987851,95.9628533577763,
10.9753046607155));
#43397=CARTESIAN_POINT('Ctrl Pts',(-1.06370987554998,95.9449175566548,11.0329764389628));
#43398=CARTESIAN_POINT('Ctrl Pts',(-1.4856031535675,95.8853573127292,11.2615121404549));
#43399=CARTESIAN_POINT('Ctrl Pts',(-1.74536023738308,95.8443779661622,11.4789526737075));
#43400=CARTESIAN_POINT('Ctrl Pts',(-2.12607564347549,95.7696574029082,11.9563022019608));
#43401=CARTESIAN_POINT('Ctrl Pts',(-2.26097034795487,95.7363966300211,12.1983000332855));
#43402=CARTESIAN_POINT('Ctrl Pts',(-2.40424892457855,95.6845807834732,12.5985295102163));
#43403=CARTESIAN_POINT('Ctrl Pts',(-2.44198066924691,95.6663679720158,12.7439353615846));
#43404=CARTESIAN_POINT('Ctrl Pts',(-2.48878040304612,95.6316250583232,13.0267460608703));
#43405=CARTESIAN_POINT('Ctrl Pts',(-2.49999999999958,95.6151461118388,13.1632543090288));
#43406=CARTESIAN_POINT('Ctrl Pts',(-2.5,95.5986983740631,13.2999999999923));
#43407=CARTESIAN_POINT('Origin',(0.,70.2,13.3));
#43408=CARTESIAN_POINT('',(-2.49986749706851,93.5355013981268,13.3002300840465));
#43409=CARTESIAN_POINT('',(-2.5,94.5443074868315,13.3));
#43410=CARTESIAN_POINT('',(-2.5,70.2,13.3));
#43411=CARTESIAN_POINT('',(1.26263430499969,95.0979194610116,11.1414618660017));
#43412=CARTESIAN_POINT('Ctrl Pts',(-2.5,94.5443074868315,13.3000000000001));
#43413=CARTESIAN_POINT('Ctrl Pts',(-2.5,94.5644680475081,13.1186486447222));
#43414=CARTESIAN_POINT('Ctrl Pts',(-2.48026874018247,94.5847545601826,12.9374339113955));
#43415=CARTESIAN_POINT('Ctrl Pts',(-2.37654233467327,94.6386548782938,12.4689486065813));
#43416=CARTESIAN_POINT('Ctrl Pts',(-2.26079321829323,94.6713476130852,12.1920715749935));
#43417=CARTESIAN_POINT('Ctrl Pts',(-2.01323785574154,94.7204442407306,11.8094242032686));
#43418=CARTESIAN_POINT('Ctrl Pts',(-1.91508090445217,94.7372444910322,11.6852537477538));
#43419=CARTESIAN_POINT('Ctrl Pts',(-1.5772741532493,94.7899797268026,11.3323920717047));
#43420=CARTESIAN_POINT('Ctrl Pts',(-1.30348816183964,94.8259667526053,11.1412239424654));
#43421=CARTESIAN_POINT('Ctrl Pts',(-0.708934834990189,94.8936466630685,
10.8816245350023));
#43422=CARTESIAN_POINT('Ctrl Pts',(-0.395859301737226,94.9254859523938,
10.8111388947139));
#43423=CARTESIAN_POINT('Ctrl Pts',(0.17199246902843,94.9845464046267,10.7934137226392));
#43424=CARTESIAN_POINT('Ctrl Pts',(0.42181962795496,95.0100858075626,10.8231668857346));
#43425=CARTESIAN_POINT('Ctrl Pts',(0.87298920622079,95.0561559175267,10.9472851876794));
#43426=CARTESIAN_POINT('Ctrl Pts',(1.07440374312525,95.0767567093663,11.0321747618983));
#43427=CARTESIAN_POINT('Ctrl Pts',(1.26227923984204,95.0978944889888,11.142072494113));
#43428=CARTESIAN_POINT('Ctrl Pts',(1.26203730190332,95.0995873533355,11.1419309907687));
#43429=CARTESIAN_POINT('Ctrl Pts',(1.46842430378966,95.1476613657154,11.262625970352));
#43430=CARTESIAN_POINT('Ctrl Pts',(1.65668516861459,95.1947410746065,11.4124842588553));
#43431=CARTESIAN_POINT('Ctrl Pts',(2.01414687277796,95.2959850342644,11.7923979876296));
#43432=CARTESIAN_POINT('Ctrl Pts',(2.17133982784043,95.3467602996658,12.0291119103098));
#43433=CARTESIAN_POINT('Ctrl Pts',(2.40258858417271,95.4497714527187,12.5511821660518));
#43434=CARTESIAN_POINT('Ctrl Pts',(2.47302861188947,95.5011569869884,12.8334108037426));
#43435=CARTESIAN_POINT('Ctrl Pts',(2.51582245316482,95.6026152339085,13.4321460196188));
#43436=CARTESIAN_POINT('Ctrl Pts',(2.47984647037667,95.6545025759123,13.7441960487413));
#43437=CARTESIAN_POINT('Ctrl Pts',(2.34060727965609,95.7315276322284,14.1924901756862));
#43438=CARTESIAN_POINT('Ctrl Pts',(2.27953083918698,95.7565976643406,14.3386250518416));
#43439=CARTESIAN_POINT('Ctrl Pts',(2.0632840803951,95.8295088394741,14.7433714554592));
#43440=CARTESIAN_POINT('Ctrl Pts',(1.87477882323332,95.8775947323833,14.9810074047945));
#43441=CARTESIAN_POINT('Ctrl Pts',(1.52582791384189,95.9494024363869,15.2870786508213));
#43442=CARTESIAN_POINT('Ctrl Pts',(1.39287000270935,95.9741138758102,15.3824433696164));
#43443=CARTESIAN_POINT('Ctrl Pts',(0.962236362152568,96.0499931698765,15.6314762132584));
#43444=CARTESIAN_POINT('Ctrl Pts',(0.64220285034896,96.100642312423,15.7391436704674));
#43445=CARTESIAN_POINT('Ctrl Pts',(-0.0128182161629909,96.1981843631053,
15.8210933592527));
#43446=CARTESIAN_POINT('Ctrl Pts',(-0.340864458137898,96.246576201709,15.7979887443412));
#43447=CARTESIAN_POINT('Ctrl Pts',(-0.978260935330136,96.3424149658101,
15.6248722001714));
#43448=CARTESIAN_POINT('Ctrl Pts',(-1.2804779668322,96.3894533056691,15.4731330420803));
#43449=CARTESIAN_POINT('Ctrl Pts',(-1.80705279880308,96.4856715391894,15.0596972143874));
#43450=CARTESIAN_POINT('Ctrl Pts',(-2.02611260905865,96.5323773074924,14.8022897964918));
#43451=CARTESIAN_POINT('Ctrl Pts',(-2.28083439937312,96.6072885286814,14.3414471807324));
#43452=CARTESIAN_POINT('Ctrl Pts',(-2.35405458842808,96.6344178644481,14.1633121593938));
#43453=CARTESIAN_POINT('Ctrl Pts',(-2.46842584453599,96.6924053719844,13.757701351164));
#43454=CARTESIAN_POINT('Ctrl Pts',(-2.50000000001015,96.7232936431479,13.5294067478282));
#43455=CARTESIAN_POINT('Ctrl Pts',(-2.5,96.7549279855909,13.2999999998894));
#43456=CARTESIAN_POINT('',(-2.49999982739251,95.5985866352558,13.3009289980743));
#43457=CARTESIAN_POINT('Ctrl Pts',(-2.5,95.5986983740631,13.2999999999923));
#43458=CARTESIAN_POINT('Ctrl Pts',(-2.5,95.5986607295953,13.3003129742643));
#43459=CARTESIAN_POINT('Ctrl Pts',(-2.49999994369443,95.5986242794474,13.3006160213367));
#43460=CARTESIAN_POINT('Ctrl Pts',(-2.49999982739251,95.5985866352558,13.3009289980743));
#43461=CARTESIAN_POINT('',(1.16384208806484,94.4245814674342,11.0879031093561));
#43462=CARTESIAN_POINT('Ctrl Pts',(-2.49999982739251,95.5985866352558,13.3009289980743));
#43463=CARTESIAN_POINT('Ctrl Pts',(-2.49991594077752,95.5714345148425,13.5266738395382));
#43464=CARTESIAN_POINT('Ctrl Pts',(-2.46925785809366,95.544573295601,13.7513636778397));
#43465=CARTESIAN_POINT('Ctrl Pts',(-2.34196456797705,95.4874583805173,14.2097856729491));
#43466=CARTESIAN_POINT('Ctrl Pts',(-2.2393043135814,95.4576130445069,14.4393195495366));
#43467=CARTESIAN_POINT('Ctrl Pts',(-1.94095249925456,95.392167000552,14.9044377699575));
#43468=CARTESIAN_POINT('Ctrl Pts',(-1.73274263558696,95.3572435285814,15.1273299475365));
#43469=CARTESIAN_POINT('Ctrl Pts',(-1.35662187133884,95.3021398289391,15.4064365280348));
#43470=CARTESIAN_POINT('Ctrl Pts',(-1.21394946922444,95.2826120965141,15.4917637903386));
#43471=CARTESIAN_POINT('Ctrl Pts',(-0.762885317374347,95.2242495326819,
15.703879635277));
#43472=CARTESIAN_POINT('Ctrl Pts',(-0.436626489655097,95.1865739351268,
15.7839558464747));
#43473=CARTESIAN_POINT('Ctrl Pts',(0.0537123919130964,95.1303100478708,
15.8044169864406));
#43474=CARTESIAN_POINT('Ctrl Pts',(0.211919055482687,95.1120638801406,15.796011968289));
#43475=CARTESIAN_POINT('Ctrl Pts',(0.694474064943877,95.055886535,15.7241452126201));
#43476=CARTESIAN_POINT('Ctrl Pts',(1.00792883989179,95.019068419798,15.6114805376621));
#43477=CARTESIAN_POINT('Ctrl Pts',(1.57641306123172,94.9452865667945,15.2688456076683));
#43478=CARTESIAN_POINT('Ctrl Pts',(1.82493765431576,94.9078033833975,15.04099045924));
#43479=CARTESIAN_POINT('Ctrl Pts',(2.19572368194789,94.8381420569224,14.5314986521421));
#43480=CARTESIAN_POINT('Ctrl Pts',(2.32610993023979,94.80677869421,14.2628269382608));
#43481=CARTESIAN_POINT('Ctrl Pts',(2.4968400964955,94.7389319078162,13.6564681884161));
#43482=CARTESIAN_POINT('Ctrl Pts',(2.52209192413947,94.7024607771091,13.3204391869547));
#43483=CARTESIAN_POINT('Ctrl Pts',(2.4417562244427,94.6346841393199,12.6790173972034));
#43484=CARTESIAN_POINT('Ctrl Pts',(2.34501599305682,94.6034267524288,12.378746960768));
#43485=CARTESIAN_POINT('Ctrl Pts',(2.12961663849431,94.5565354597433,11.9833175548818));
#43486=CARTESIAN_POINT('Ctrl Pts',(2.05395544128919,94.54222843125,11.868149916199));
#43487=CARTESIAN_POINT('Ctrl Pts',(1.85605096969357,94.5093535416532,11.6151254287725));
#43488=CARTESIAN_POINT('Ctrl Pts',(1.72729025550136,94.4910953114638,11.4833471580103));
#43489=CARTESIAN_POINT('Ctrl Pts',(1.45461349282513,94.456731209407,11.2597487954932));
#43490=CARTESIAN_POINT('Ctrl Pts',(1.31350356515208,94.4406468431525,11.1661698056949));
#43491=CARTESIAN_POINT('Ctrl Pts',(1.16404056044746,94.424229722102,11.0875331474499));
#43492=CARTESIAN_POINT('Ctrl Pts',(1.16347235681021,94.4241522805232,11.0886093503689));
#43493=CARTESIAN_POINT('Ctrl Pts',(1.09886931445663,94.4095786870534,11.0546714886086));
#43494=CARTESIAN_POINT('Ctrl Pts',(1.03286394719834,94.3949382050941,11.0237518795221));
#43495=CARTESIAN_POINT('Ctrl Pts',(0.965698223793783,94.3804123520948,10.9957715840715));
#43496=CARTESIAN_POINT('Ctrl Pts',(0.954625997705913,94.3780177746172,10.9911590504527));
#43497=CARTESIAN_POINT('Ctrl Pts',(0.943522128381032,94.3756263044254,10.9866264249625));
#43498=CARTESIAN_POINT('Ctrl Pts',(0.932387570777659,94.3732387453768,10.9821733941901));
#43499=CARTESIAN_POINT('Ctrl Pts',(0.852355593053961,94.3560776618925,10.9501662977006));
#43500=CARTESIAN_POINT('Ctrl Pts',(0.770739886231872,94.3391183146964,10.9222676418242));
#43501=CARTESIAN_POINT('Ctrl Pts',(0.687895202432596,94.3223048946047,10.898563720722));
#43502=CARTESIAN_POINT('Ctrl Pts',(0.604906261470646,94.3054621973625,10.8748185240635));
#43503=CARTESIAN_POINT('Ctrl Pts',(0.520683550444595,94.2887658382801,10.8552826098449));
#43504=CARTESIAN_POINT('Ctrl Pts',(0.435566099291187,94.2721823223814,10.8400796637549));
#43505=CARTESIAN_POINT('Ctrl Pts',(0.362494535345656,94.2579457184182,10.8270282502984));
#43506=CARTESIAN_POINT('Ctrl Pts',(0.288763106090426,94.2437926396513,10.8171706621563));
#43507=CARTESIAN_POINT('Ctrl Pts',(0.214580045610659,94.2297157102005,10.8106081683442));
#43508=CARTESIAN_POINT('Ctrl Pts',(0.127661799560024,94.2132221601941,10.8029190753331));
#43509=CARTESIAN_POINT('Ctrl Pts',(0.040587175047819,94.1969195527311,10.799794064794));
#43510=CARTESIAN_POINT('Ctrl Pts',(-0.046315175775073,94.1808216686268,
10.8012845181134));
#43511=CARTESIAN_POINT('Ctrl Pts',(-0.0895357882538338,94.172815436298,
10.8020257904118));
#43512=CARTESIAN_POINT('Ctrl Pts',(-0.132714256012658,94.1648601554613,
10.8039093396504));
#43513=CARTESIAN_POINT('Ctrl Pts',(-0.175812361638747,94.1569592270527,
10.8069454866206));
#43514=CARTESIAN_POINT('Ctrl Pts',(-0.175818529435711,94.1569580963459,
10.8069459211255));
#43515=CARTESIAN_POINT('Ctrl Pts',(-0.175824697231117,94.1569569656401,
10.806946355654));
#43516=CARTESIAN_POINT('Ctrl Pts',(-0.175830865024881,94.1569558349355,
10.8069467902062));
#43517=CARTESIAN_POINT('Ctrl Pts',(-0.260944759189729,94.1413524153915,
10.8129434927071));
#43518=CARTESIAN_POINT('Ctrl Pts',(-0.345746873428532,94.1259600022047,
10.8234327177893));
#43519=CARTESIAN_POINT('Ctrl Pts',(-0.429909388036926,94.1106936244754,
10.8382787893713));
#43520=CARTESIAN_POINT('Ctrl Pts',(-0.51533239086428,94.0951986047032,10.8533472081399));
#43521=CARTESIAN_POINT('Ctrl Pts',(-0.600097272709715,94.0798330160529,
10.8729045032887));
#43522=CARTESIAN_POINT('Ctrl Pts',(-0.683848059130618,94.0645257074691,
10.8968512447243));
#43523=CARTESIAN_POINT('Ctrl Pts',(-0.712115171912877,94.0593592674078,
10.904933619468));
#43524=CARTESIAN_POINT('Ctrl Pts',(-0.740266604201373,94.0541996398609,
10.9135163387467));
#43525=CARTESIAN_POINT('Ctrl Pts',(-0.768288134706657,94.0490446490367,
10.9225964879163));
#43526=CARTESIAN_POINT('Ctrl Pts',(-0.851089486853107,94.0338120688441,
10.9494275929764));
#43527=CARTESIAN_POINT('Ctrl Pts',(-0.932321208706402,94.018697261967,10.9804584999919));
#43528=CARTESIAN_POINT('Ctrl Pts',(-1.01165869703274,94.0036631570407,11.0155028541458));
#43529=CARTESIAN_POINT('Ctrl Pts',(-1.09159427871556,93.9885157160553,11.0508113935651));
#43530=CARTESIAN_POINT('Ctrl Pts',(-1.16960731629625,93.9734501950163,11.0901942032906));
#43531=CARTESIAN_POINT('Ctrl Pts',(-1.24536692198904,93.9584541936714,11.1335007446988));
#43532=CARTESIAN_POINT('Ctrl Pts',(-1.32029170007773,93.9436234397001,11.176330072744));
#43533=CARTESIAN_POINT('Ctrl Pts',(-1.39301295184137,93.9288608246002,11.2229971636614));
#43534=CARTESIAN_POINT('Ctrl Pts',(-1.46320530897308,93.914178040055,11.2733945537142));
#43535=CARTESIAN_POINT('Ctrl Pts',(-1.52151896162447,93.9019800339911,11.3152631561969));
#43536=CARTESIAN_POINT('Ctrl Pts',(-1.57808737847907,93.8898376016107,11.3597069807771));
#43537=CARTESIAN_POINT('Ctrl Pts',(-1.63271644490332,93.8777688222159,11.4066848110243));
#43538=CARTESIAN_POINT('Ctrl Pts',(-1.64362384817868,93.8753591335187,11.4160645455329));
#43539=CARTESIAN_POINT('Ctrl Pts',(-1.65444449801962,93.8729545265953,11.4255372421034));
#43540=CARTESIAN_POINT('Ctrl Pts',(-1.66517723864454,93.8705551820243,11.4351021586842));
#43541=CARTESIAN_POINT('Ctrl Pts',(-1.66517859425571,93.8705548789724,11.435103366792));
#43542=CARTESIAN_POINT('Ctrl Pts',(-1.66517994986548,93.8705545759205,11.4351045749013));
#43543=CARTESIAN_POINT('Ctrl Pts',(-1.66518130547384,93.8705542728687,11.4351057830121));
#43544=CARTESIAN_POINT('Ctrl Pts',(-1.72884031212494,93.8563230407208,11.4918383411191));
#43545=CARTESIAN_POINT('Ctrl Pts',(-1.78940844538948,93.8422753331869,11.5518122614757));
#43546=CARTESIAN_POINT('Ctrl Pts',(-1.84671790514911,93.8283371097907,11.6146958222387));
#43547=CARTESIAN_POINT('Ctrl Pts',(-1.90503232073465,93.8141544712689,11.6786820840393));
#43548=CARTESIAN_POINT('Ctrl Pts',(-1.95997290070592,93.8000848809414,11.745681602123));
#43549=CARTESIAN_POINT('Ctrl Pts',(-2.01133759587612,93.7860740938722,11.8153752450508));
#43550=CARTESIAN_POINT('Ctrl Pts',(-2.06307838930044,93.7719607181954,11.8855791929135));
#43551=CARTESIAN_POINT('Ctrl Pts',(-2.11119079150021,93.7579068496475,11.9585172775703));
#43552=CARTESIAN_POINT('Ctrl Pts',(-2.15544179716195,93.7438844347746,12.0338854754219));
#43553=CARTESIAN_POINT('Ctrl Pts',(-2.16356185472066,93.741311322273,12.0477155363549));
#43554=CARTESIAN_POINT('Ctrl Pts',(-2.17155181739915,93.7387393459551,12.0616274759162));
#43555=CARTESIAN_POINT('Ctrl Pts',(-2.17941014585818,93.7361684369155,12.0756194824366));
#43556=CARTESIAN_POINT('Ctrl Pts',(-2.17941197753976,93.7361678376677,12.0756227438045));
#43557=CARTESIAN_POINT('Ctrl Pts',(-2.17941380921418,93.7361672384198,12.0756260051768));
#43558=CARTESIAN_POINT('Ctrl Pts',(-2.17941564088145,93.7361666391721,12.0756292665535));
#43559=CARTESIAN_POINT('Ctrl Pts',(-2.20057589852894,93.7292438549686,12.1133061804977));
#43560=CARTESIAN_POINT('Ctrl Pts',(-2.22078186132525,93.7223287096649,12.1515636262624));
#43561=CARTESIAN_POINT('Ctrl Pts',(-2.24000847350861,93.7154167765929,12.1903652844855));
#43562=CARTESIAN_POINT('Ctrl Pts',(-2.27868382590507,93.7015130558151,12.2684168825014));
#43563=CARTESIAN_POINT('Ctrl Pts',(-2.31319724593064,93.687694207725,12.3482620836716));
#43564=CARTESIAN_POINT('Ctrl Pts',(-2.34345309249078,93.6739428144898,12.4295605374583));
#43565=CARTESIAN_POINT('Ctrl Pts',(-2.37395208550431,93.6600809102998,12.5115123337541));
#43566=CARTESIAN_POINT('Ctrl Pts',(-2.4001251281991,93.64628764271,12.5949410687129));
#43567=CARTESIAN_POINT('Ctrl Pts',(-2.42184839166118,93.6325683170609,12.6795286142253));
#43568=CARTESIAN_POINT('Ctrl Pts',(-2.43619340691957,93.6235087235926,12.7353862266492));
#43569=CARTESIAN_POINT('Ctrl Pts',(-2.4485975138681,93.6144818559146,12.7917497827169));
#43570=CARTESIAN_POINT('Ctrl Pts',(-2.45901752505367,93.6054942738369,12.8485340711388));
#43571=CARTESIAN_POINT('Ctrl Pts',(-2.45901797260607,93.6054938878092,12.8485365100944));
#43572=CARTESIAN_POINT('Ctrl Pts',(-2.4590184201548,93.6054935017815,12.8485389490507));
#43573=CARTESIAN_POINT('Ctrl Pts',(-2.45901886769987,93.6054931157538,12.8485413880079));
#43574=CARTESIAN_POINT('Ctrl Pts',(-2.47477860185115,93.5918996400528,12.9344261810042));
#43575=CARTESIAN_POINT('Ctrl Pts',(-2.4860015256015,93.5783948820527,13.0212750778943));
#43576=CARTESIAN_POINT('Ctrl Pts',(-2.49264976786009,93.5649076679167,13.1087174910619));
#43577=CARTESIAN_POINT('Ctrl Pts',(-2.49364658064142,93.5628854450626,13.1218282821078));
#43578=CARTESIAN_POINT('Ctrl Pts',(-2.49454047246715,93.5608636596275,13.1349523938354));
#43579=CARTESIAN_POINT('Ctrl Pts',(-2.49533116854958,93.5588423848586,13.1480868187036));
#43580=CARTESIAN_POINT('Ctrl Pts',(-2.49838372369694,93.5510390672033,13.1987934772166));
#43581=CARTESIAN_POINT('Ctrl Pts',(-2.4998915056308,93.5432607996176,13.249540054876));
#43582=CARTESIAN_POINT('Ctrl Pts',(-2.49986749706851,93.5355013981268,13.3002300840465));
#43583=CARTESIAN_POINT('Origin',(0.,70.2,13.3));
#43584=CARTESIAN_POINT('',(-2.5,91.3980900981106,13.3));
#43585=CARTESIAN_POINT('',(-2.5,92.6061264662692,13.2999999996171));
#43586=CARTESIAN_POINT('',(-2.5,70.2,13.3));
#43587=CARTESIAN_POINT('',(-2.49999761486117,92.6065892681553,13.296546640986));
#43588=CARTESIAN_POINT('Ctrl Pts',(-2.5,92.6061264662692,13.2999999992341));
#43589=CARTESIAN_POINT('Ctrl Pts',(-2.49999999999965,92.6062811709464,13.2988456033981));
#43590=CARTESIAN_POINT('Ctrl Pts',(-2.49999920955526,92.6064345527048,13.2977010913065));
#43591=CARTESIAN_POINT('Ctrl Pts',(-2.49999761486117,92.6065892681553,13.2965466409861));
#43592=CARTESIAN_POINT('Ctrl Pts',(-2.49999761486117,92.6065892681554,13.296546640986));
#43593=CARTESIAN_POINT('Ctrl Pts',(-2.49974231312978,92.6313583587562,13.1117255097472));
#43594=CARTESIAN_POINT('Ctrl Pts',(-2.47899380873915,92.6561286709599,12.9275123025644));
#43595=CARTESIAN_POINT('Ctrl Pts',(-2.39276586348267,92.708439349742,12.5471553898367));
#43596=CARTESIAN_POINT('Ctrl Pts',(-2.32292262850757,92.735726442814,12.3533322714901));
#43597=CARTESIAN_POINT('Ctrl Pts',(-2.07920141723139,92.8061179400166,11.872248794433));
#43598=CARTESIAN_POINT('Ctrl Pts',(-1.87007179557902,92.8484792603454,11.6075450979363));
#43599=CARTESIAN_POINT('Ctrl Pts',(-1.38183916875315,92.9319131617122,11.1943129302899));
#43600=CARTESIAN_POINT('Ctrl Pts',(-1.11433355745884,92.9719818863433,11.0413153212106));
#43601=CARTESIAN_POINT('Ctrl Pts',(-0.551537143215495,93.049648231513,10.8443344521761));
#43602=CARTESIAN_POINT('Ctrl Pts',(-0.262503619937133,93.086277995738,10.7968748032867));
#43603=CARTESIAN_POINT('Ctrl Pts',(0.339914036160982,93.1628043721513,10.8036806691249));
#43604=CARTESIAN_POINT('Ctrl Pts',(0.648180826792544,93.202181931772,10.8654578372114));
#43605=CARTESIAN_POINT('Ctrl Pts',(1.15749934761066,93.2723831415024,11.0713900277499));
#43606=CARTESIAN_POINT('Ctrl Pts',(1.36406727805913,93.3026013245646,11.1914822077757));
#43607=CARTESIAN_POINT('Ctrl Pts',(1.81248982774957,93.3748889939285,11.5460405876667));
#43608=CARTESIAN_POINT('Ctrl Pts',(2.03031177981672,93.4163034018027,11.8035488170692));
#43609=CARTESIAN_POINT('Ctrl Pts',(2.34680804312831,93.4984737524834,12.379648598209));
#43610=CARTESIAN_POINT('Ctrl Pts',(2.44605820800887,93.5383907596061,12.6905942134514));
#43611=CARTESIAN_POINT('Ctrl Pts',(2.52108852552984,93.6191936511323,13.3371554665366));
#43612=CARTESIAN_POINT('Ctrl Pts',(2.49454822643192,93.6593295731743,13.6667888607161));
#43613=CARTESIAN_POINT('Ctrl Pts',(2.36211807527856,93.7188889609086,14.1338678288279));
#43614=CARTESIAN_POINT('Ctrl Pts',(2.30474237838344,93.7381450405329,14.2813787102134));
#43615=CARTESIAN_POINT('Ctrl Pts',(2.0864230926269,93.7974474462361,14.7158477760113));
#43616=CARTESIAN_POINT('Ctrl Pts',(1.88265177494184,93.837158538839,14.9773285460213));
#43617=CARTESIAN_POINT('Ctrl Pts',(1.51509361740658,93.8959651658159,15.2948053030737));
#43618=CARTESIAN_POINT('Ctrl Pts',(1.38656789723429,93.9148813552297,15.3861908873483));
#43619=CARTESIAN_POINT('Ctrl Pts',(1.11642368411619,93.9523260924595,15.5422084446643));
#43620=CARTESIAN_POINT('Ctrl Pts',(0.975663561710984,93.9707753732465,15.606942167965));
#43621=CARTESIAN_POINT('Ctrl Pts',(0.514260502639939,94.0293900601284,15.76930134143));
#43622=CARTESIAN_POINT('Ctrl Pts',(0.179556580620323,94.0692542741921,15.8158937237312));
#43623=CARTESIAN_POINT('Ctrl Pts',(-0.477623044706271,94.1469936864816,
15.7752256425953));
#43624=CARTESIAN_POINT('Ctrl Pts',(-0.793897270724776,94.1844054736309,
15.6926131546135));
#43625=CARTESIAN_POINT('Ctrl Pts',(-1.22976491031325,94.2414202920349,15.482495961809));
#43626=CARTESIAN_POINT('Ctrl Pts',(-1.36692753001275,94.26019774854,15.3993159874602));
#43627=CARTESIAN_POINT('Ctrl Pts',(-1.73569019541523,94.3138047017912,15.1241221320101));
#43628=CARTESIAN_POINT('Ctrl Pts',(-1.94192177052931,94.347720696045,14.9028112140539));
#43629=CARTESIAN_POINT('Ctrl Pts',(-2.2853474559415,94.4207917580665,14.3676691921534));
#43630=CARTESIAN_POINT('Ctrl Pts',(-2.40795052875896,94.4594073953375,14.0513863627676));
#43631=CARTESIAN_POINT('Ctrl Pts',(-2.48815000607631,94.5130391481474,13.5811380584742));
#43632=CARTESIAN_POINT('Ctrl Pts',(-2.5,94.5286845898386,13.4405334697025));
#43633=CARTESIAN_POINT('Ctrl Pts',(-2.5,94.5443074868315,13.3000000000001));
#43634=CARTESIAN_POINT('Ctrl Pts',(-2.49999998683747,93.5356742584249,13.3002565397127));
#43635=CARTESIAN_POINT('Ctrl Pts',(-2.4999789695336,93.5044243811101,13.5050718444085));
#43636=CARTESIAN_POINT('Ctrl Pts',(-2.47478881885302,93.473058246009,13.7091015875136));
#43637=CARTESIAN_POINT('Ctrl Pts',(-2.37018635660125,93.4074962166809,14.1264723750432));
#43638=CARTESIAN_POINT('Ctrl Pts',(-2.28604298265964,93.3743391483411,14.3367685729446));
#43639=CARTESIAN_POINT('Ctrl Pts',(-2.09910870413749,93.3182242719682,14.666488622868));
#43640=CARTESIAN_POINT('Ctrl Pts',(-2.0112932659589,93.295470102,14.7927312450222));
#43641=CARTESIAN_POINT('Ctrl Pts',(-1.70571042301175,93.225223893868,15.1556957769451));
#43642=CARTESIAN_POINT('Ctrl Pts',(-1.45356321019058,93.1798227443927,15.3591995454538));
#43643=CARTESIAN_POINT('Ctrl Pts',(-1.02913288799724,93.1107249653846,15.5838978624607));
#43644=CARTESIAN_POINT('Ctrl Pts',(-0.881759653757164,93.0877777099911,
15.644740430157));
#43645=CARTESIAN_POINT('Ctrl Pts',(-0.407882395044307,93.0169384538345,
15.789331411237));
#43646=CARTESIAN_POINT('Ctrl Pts',(-0.0695863349327156,92.9706330455138,
15.8215770818348));
#43647=CARTESIAN_POINT('Ctrl Pts',(0.586698011167412,92.8775518437506,15.7516272646382));
#43648=CARTESIAN_POINT('Ctrl Pts',(0.898782601217875,92.8334217271977,15.6551959751661));
#43649=CARTESIAN_POINT('Ctrl Pts',(1.44938353103509,92.7469448940478,15.3591678880462));
#43650=CARTESIAN_POINT('Ctrl Pts',(1.68695879439215,92.7054565987242,15.1695231302102));
#43651=CARTESIAN_POINT('Ctrl Pts',(2.0931268316993,92.6213899195092,14.7032713845275));
#43652=CARTESIAN_POINT('Ctrl Pts',(2.25393486896684,92.5783071985329,14.4269993422804));
#43653=CARTESIAN_POINT('Ctrl Pts',(2.41344537190869,92.5131072267778,13.972630544522));
#43654=CARTESIAN_POINT('Ctrl Pts',(2.45252514690124,92.491087068295,13.8121318364526));
#43655=CARTESIAN_POINT('Ctrl Pts',(2.4983191341392,92.4469569051383,13.4872558846521));
#43656=CARTESIAN_POINT('Ctrl Pts',(2.50521404251146,92.4249607365414,13.3237244353476));
#43657=CARTESIAN_POINT('Ctrl Pts',(2.47773093742526,92.358445213497,12.8312603077648));
#43658=CARTESIAN_POINT('Ctrl Pts',(2.3943083060055,92.3152377297702,12.5086723216436));
#43659=CARTESIAN_POINT('Ctrl Pts',(2.18178654562703,92.2502850745213,12.0692238051173));
#43660=CARTESIAN_POINT('Ctrl Pts',(2.09959281497549,92.2292337984681,11.9337219735002));
#43661=CARTESIAN_POINT('Ctrl Pts',(1.80543284066672,92.1639854018535,11.5386840176256));
#43662=CARTESIAN_POINT('Ctrl Pts',(1.55390552563549,92.120684412765,11.3132384200328));
#43663=CARTESIAN_POINT('Ctrl Pts',(0.977159926933571,92.0325181691515,10.9747194087218));
#43664=CARTESIAN_POINT('Ctrl Pts',(0.657777013696649,91.9894311947502,10.8650191560993));
#43665=CARTESIAN_POINT('Ctrl Pts',(0.168672586084107,91.924970656387,10.8006368228099));
#43666=CARTESIAN_POINT('Ctrl Pts',(0.00945374552732607,91.9042037078517,
10.7949691397534));
#43667=CARTESIAN_POINT('Ctrl Pts',(-0.482974831005797,91.8399479630952,
10.8244147096595));
#43668=CARTESIAN_POINT('Ctrl Pts',(-0.809373468747169,91.797310972374,10.9111249870723));
#43669=CARTESIAN_POINT('Ctrl Pts',(-1.40949449292844,91.7106124885981,11.2081802334211));
#43670=CARTESIAN_POINT('Ctrl Pts',(-1.67699636792964,91.6680289632479,11.4158307318775));
#43671=CARTESIAN_POINT('Ctrl Pts',(-2.0000838690445,91.6043552699173,11.7915732168463));
#43672=CARTESIAN_POINT('Ctrl Pts',(-2.09265142535013,91.5837847170907,11.9228658205572));
#43673=CARTESIAN_POINT('Ctrl Pts',(-2.33749113353084,91.5203917769293,12.3524654527532));
#43674=CARTESIAN_POINT('Ctrl Pts',(-2.44308933652245,91.4783101504844,12.6730853904379));
#43675=CARTESIAN_POINT('Ctrl Pts',(-2.49419079729861,91.423136710787,13.1030884670158));
#43676=CARTESIAN_POINT('Ctrl Pts',(-2.5,91.4105921947178,13.2016002889944));
#43677=CARTESIAN_POINT('Ctrl Pts',(-2.5,91.3980900981106,13.3));
#43678=CARTESIAN_POINT('Origin',(0.,70.2,13.3));
#43679=CARTESIAN_POINT('',(-2.5,90.4307847167281,13.2999999999841));
#43680=CARTESIAN_POINT('',(0.400974295891035,90.9332096597013,10.8309447386746));
#43681=CARTESIAN_POINT('Ctrl Pts',(-2.49999999944397,90.430791038424,13.2999472726946));
#43682=CARTESIAN_POINT('Ctrl Pts',(-2.49999398616684,90.4649743170265,13.0148351718446));
#43683=CARTESIAN_POINT('Ctrl Pts',(-2.45121672545614,90.4988744454463,12.7317974299723));
#43684=CARTESIAN_POINT('Ctrl Pts',(-2.26557142946895,90.5645414565702,12.209239581071));
#43685=CARTESIAN_POINT('Ctrl Pts',(-2.13494258436756,90.5959008943449,11.9716138177145));
#43686=CARTESIAN_POINT('Ctrl Pts',(-1.86512631626832,90.6472524747142,11.6267783216932));
#43687=CARTESIAN_POINT('Ctrl Pts',(-1.7481912546364,90.6669116085519,11.5049506339109));
#43688=CARTESIAN_POINT('Ctrl Pts',(-1.37991318202436,90.7230418962365,11.1916588423971));
#43689=CARTESIAN_POINT('Ctrl Pts',(-1.1034811920457,90.7587209515757,11.0346917762158));
#43690=CARTESIAN_POINT('Ctrl Pts',(-0.604712400799047,90.8190948670444,
10.8650145562887));
#43691=CARTESIAN_POINT('Ctrl Pts',(-0.396384515693903,90.8431506187802,
10.8225555507897));
#43692=CARTESIAN_POINT('Ctrl Pts',(0.0104683070707311,90.8890917529299,
10.79233544841));
#43693=CARTESIAN_POINT('Ctrl Pts',(0.207159199743011,90.9108543330795,10.8008836601677));
#43694=CARTESIAN_POINT('Ctrl Pts',(0.400828488760919,90.9327222859085,10.8323418951164));
#43695=CARTESIAN_POINT('Ctrl Pts',(0.400506739468218,90.9349782296111,10.8322896540233));
#43696=CARTESIAN_POINT('Ctrl Pts',(0.621120297389946,90.9723564264929,10.868094997592));
#43697=CARTESIAN_POINT('Ctrl Pts',(0.835904576484284,91.0101623910831,10.9333148711372));
#43698=CARTESIAN_POINT('Ctrl Pts',(1.27168608214601,91.090069164932,11.1324708489373));
#43699=CARTESIAN_POINT('Ctrl Pts',(1.48652387690573,91.1303415091947,11.2737468407469));
#43700=CARTESIAN_POINT('Ctrl Pts',(1.90760374097452,91.2207085299562,11.654329613527));
#43701=CARTESIAN_POINT('Ctrl Pts',(2.09775190589845,91.2708175203025,11.904784414362));
#43702=CARTESIAN_POINT('Ctrl Pts',(2.38675839750348,91.3723506393853,12.483941804229));
#43703=CARTESIAN_POINT('Ctrl Pts',(2.4746364372273,91.4213334522488,12.8112648400754));
#43704=CARTESIAN_POINT('Ctrl Pts',(2.51293821602994,91.5162567229141,13.4331618947545));
#43705=CARTESIAN_POINT('Ctrl Pts',(2.48102245615064,91.5605504977297,13.7210305117836));
#43706=CARTESIAN_POINT('Ctrl Pts',(2.35523589392042,91.6271019915223,14.1541369467785));
#43707=CARTESIAN_POINT('Ctrl Pts',(2.29439915178092,91.6506768742613,14.3062005804627));
#43708=CARTESIAN_POINT('Ctrl Pts',(2.070561381475,91.7213524525443,14.7376635081236));
#43709=CARTESIAN_POINT('Ctrl Pts',(1.8679142149634,91.7687807293572,14.9926178470517));
#43710=CARTESIAN_POINT('Ctrl Pts',(1.36693704679103,91.8645588470098,15.4199816748156));
#43711=CARTESIAN_POINT('Ctrl Pts',(1.0700285034486,91.9109157335291,15.5842830755364));
#43712=CARTESIAN_POINT('Ctrl Pts',(0.432339885058854,92.0063423998576,15.7846688280913));
#43713=CARTESIAN_POINT('Ctrl Pts',(0.0983981470253122,92.0538541595564,
15.8201114951091));
#43714=CARTESIAN_POINT('Ctrl Pts',(-0.394684796713186,92.1225632368531,
15.7739974665974));
#43715=CARTESIAN_POINT('Ctrl Pts',(-0.554718205591719,92.1449255734657,
15.7430981435197));
#43716=CARTESIAN_POINT('Ctrl Pts',(-1.005229486078,92.2101441446002,15.6095322692099));
#43717=CARTESIAN_POINT('Ctrl Pts',(-1.281214846687,92.2532119422054,15.4686190485525));
#43718=CARTESIAN_POINT('Ctrl Pts',(-1.79048026572708,92.3419207642284,15.0766916589386));
#43719=CARTESIAN_POINT('Ctrl Pts',(-2.01242440125496,92.386502596009,14.8207462284203));
#43720=CARTESIAN_POINT('Ctrl Pts',(-2.27816469537492,92.4603043242833,14.3498147510431));
#43721=CARTESIAN_POINT('Ctrl Pts',(-2.35665279172611,92.4883709713848,14.1592674280451));
#43722=CARTESIAN_POINT('Ctrl Pts',(-2.47004890104903,92.5465142950431,13.7458294206398));
#43723=CARTESIAN_POINT('Ctrl Pts',(-2.50000000006845,92.576184132504,13.5234276683856));
#43724=CARTESIAN_POINT('Ctrl Pts',(-2.5,92.6061264662693,13.2999999992341));
#43725=CARTESIAN_POINT('',(-2.5,89.5119815300394,13.3));
#43726=CARTESIAN_POINT('Ctrl Pts',(-2.5,91.3980900981106,13.3));
#43727=CARTESIAN_POINT('Ctrl Pts',(-2.5,91.368530213291,13.5326557068775));
#43728=CARTESIAN_POINT('Ctrl Pts',(-2.46751960634584,91.3392038081443,13.7646842113909));
#43729=CARTESIAN_POINT('Ctrl Pts',(-2.35870962296507,91.2892893951694,14.1440491200089));
#43730=CARTESIAN_POINT('Ctrl Pts',(-2.29946141539159,91.2689712778199,14.294187482627));
#43731=CARTESIAN_POINT('Ctrl Pts',(-2.15320190902688,91.228398632862,14.5804091252095));
#43732=CARTESIAN_POINT('Ctrl Pts',(-2.06663970281822,91.2082547569972,14.7158846723123));
#43733=CARTESIAN_POINT('Ctrl Pts',(-1.7693061928053,91.1476526070444,15.0952690068056));
#43734=CARTESIAN_POINT('Ctrl Pts',(-1.52391373605851,91.1076480466686,15.3077696040993));
#43735=CARTESIAN_POINT('Ctrl Pts',(-1.09880992681705,91.0463439344429,15.5518957636767));
#43736=CARTESIAN_POINT('Ctrl Pts',(-0.944503984613686,91.0253561873975,
15.6208474375327));
#43737=CARTESIAN_POINT('Ctrl Pts',(-0.510700700564446,90.9684073479455,
15.7642031784739));
#43738=CARTESIAN_POINT('Ctrl Pts',(-0.223365419072312,90.9328095634411,
15.8066368307339));
#43739=CARTESIAN_POINT('Ctrl Pts',(0.222638075959661,90.8773771355885,15.795064762925));
#43740=CARTESIAN_POINT('Ctrl Pts',(0.379695990862955,90.8578382908325,15.7760351590646));
#43741=CARTESIAN_POINT('Ctrl Pts',(0.815486743500037,90.8026557974328,15.680767658675));
#43742=CARTESIAN_POINT('Ctrl Pts',(1.08431846596642,90.7674865422745,15.5709778776648));
#43743=CARTESIAN_POINT('Ctrl Pts',(1.61292582457286,90.6907519849497,15.2393819932704));
#43744=CARTESIAN_POINT('Ctrl Pts',(1.8585328820173,90.6497316053036,15.0054664287502));
#43745=CARTESIAN_POINT('Ctrl Pts',(2.23051708143503,90.5704271973385,14.4720539524885));
#43746=CARTESIAN_POINT('Ctrl Pts',(2.36013642592417,90.5327665798079,14.1824274811899));
#43747=CARTESIAN_POINT('Ctrl Pts',(2.46991719189685,90.4748120053061,13.7190918867424));
#43748=CARTESIAN_POINT('Ctrl Pts',(2.4918439325536,90.4551884526585,13.5585498160198));
#43749=CARTESIAN_POINT('Ctrl Pts',(2.50939685205833,90.4004998753436,13.1065462481498));
#43750=CARTESIAN_POINT('Ctrl Pts',(2.46993224947177,90.3661374484165,12.8163155338604));
#43751=CARTESIAN_POINT('Ctrl Pts',(2.27992584186872,90.2914072336011,12.2214092042317));
#43752=CARTESIAN_POINT('Ctrl Pts',(2.1157069097961,90.2511386130339,11.9269655469924));
#43753=CARTESIAN_POINT('Ctrl Pts',(1.71056651076189,90.1770821018749,11.4540824290684));
#43754=CARTESIAN_POINT('Ctrl Pts',(1.48600950333078,90.1437499762508,11.2689315344893));
#43755=CARTESIAN_POINT('Ctrl Pts',(0.944518588190801,90.0705024688197,10.9613368573605));
#43756=CARTESIAN_POINT('Ctrl Pts',(0.624138639742351,90.0303394185647,10.8562509154152));
#43757=CARTESIAN_POINT('Ctrl Pts',(0.0186310933730435,89.9586948956865,
10.7848971646399));
#43758=CARTESIAN_POINT('Ctrl Pts',(-0.258796694907511,89.9274633674728,
10.7981706303626));
#43759=CARTESIAN_POINT('Ctrl Pts',(-0.854485046668086,89.8576522359491,
10.9270035879568));
#43760=CARTESIAN_POINT('Ctrl Pts',(-1.16308185270574,89.8183984118701,11.0620356140602));
#43761=CARTESIAN_POINT('Ctrl Pts',(-1.6640759599315,89.748234413936,11.4136213894974));
#43762=CARTESIAN_POINT('Ctrl Pts',(-1.86374161376017,89.7176791650614,11.610597051237));
#43763=CARTESIAN_POINT('Ctrl Pts',(-2.22196856512738,89.6497716042869,12.1067014844785));
#43764=CARTESIAN_POINT('Ctrl Pts',(-2.36107557540821,89.6112869974941,12.4132200524645));
#43765=CARTESIAN_POINT('Ctrl Pts',(-2.46887032142857,89.5576028964703,12.8804083992387));
#43766=CARTESIAN_POINT('Ctrl Pts',(-2.48918706775228,89.5415776841612,13.0255115769856));
#43767=CARTESIAN_POINT('Ctrl Pts',(-2.49890211709861,89.5211630832979,13.2144071673686));
#43768=CARTESIAN_POINT('Ctrl Pts',(-2.5,89.516563021389,13.2572235679475));
#43769=CARTESIAN_POINT('Ctrl Pts',(-2.5,89.5119815300394,13.3));
#43770=CARTESIAN_POINT('',(-2.5,70.2,13.3));
#43771=CARTESIAN_POINT('Origin',(0.,70.2,13.3));
#43772=CARTESIAN_POINT('',(-2.5,87.6157001716672,13.3000000000001));
#43773=CARTESIAN_POINT('',(-2.5,88.464609916907,13.2999999999998));
#43774=CARTESIAN_POINT('',(-2.5,70.2,13.3));
#43775=CARTESIAN_POINT('',(-1.18108807079192,88.7245239333106,11.0963559860755));
#43776=CARTESIAN_POINT('Ctrl Pts',(-2.5,88.464609916907,13.2999999999997));
#43777=CARTESIAN_POINT('Ctrl Pts',(-2.49999999999999,88.4763169599804,13.1863620604698));
#43778=CARTESIAN_POINT('Ctrl Pts',(-2.49225149769818,88.4878609695849,13.0725943974306));
#43779=CARTESIAN_POINT('Ctrl Pts',(-2.43361199552928,88.5308384828477,12.6460598539817));
#43780=CARTESIAN_POINT('Ctrl Pts',(-2.33139820322754,88.5609011878374,12.3436028049079));
#43781=CARTESIAN_POINT('Ctrl Pts',(-2.05119861166652,88.6173290833032,11.8487106482045));
#43782=CARTESIAN_POINT('Ctrl Pts',(-1.89432399303536,88.6418420705692,11.6491554750665));
#43783=CARTESIAN_POINT('Ctrl Pts',(-1.55107956884997,88.6853869978468,11.3272581236237));
#43784=CARTESIAN_POINT('Ctrl Pts',(-1.3731860005449,88.7045813073607,11.1995430462422));
#43785=CARTESIAN_POINT('Ctrl Pts',(-1.1809717498647,88.7243316451192,11.096524171673));
#43786=CARTESIAN_POINT('Ctrl Pts',(-1.18100228905586,88.7246337621387,11.0965405396866));
#43787=CARTESIAN_POINT('Ctrl Pts',(-0.912279497684443,88.768490042615,10.9525114629338));
#43788=CARTESIAN_POINT('Ctrl Pts',(-0.619420463177039,88.8119324096701,
10.8588259010574));
#43789=CARTESIAN_POINT('Ctrl Pts',(0.0110562175630186,88.9019754116573,
10.7782565527367));
#43790=CARTESIAN_POINT('Ctrl Pts',(0.344128588636148,88.9474058964649,10.8018106969851));
#43791=CARTESIAN_POINT('Ctrl Pts',(0.985082241119456,89.0399859110188,10.9781053204488));
#43792=CARTESIAN_POINT('Ctrl Pts',(1.28619087413887,89.0858470553435,11.1303608395587));
#43793=CARTESIAN_POINT('Ctrl Pts',(1.76740341983592,89.1703846349364,11.5100161694327));
#43794=CARTESIAN_POINT('Ctrl Pts',(1.95593217319766,89.2087799324138,11.7181829468283));
#43795=CARTESIAN_POINT('Ctrl Pts',(2.28641800458696,89.2915244201812,12.2350168643086));
#43796=CARTESIAN_POINT('Ctrl Pts',(2.40826581514484,89.3349110408818,12.5501922024444));
#43797=CARTESIAN_POINT('Ctrl Pts',(2.51969689321026,89.4234811092858,13.2041022431543));
#43798=CARTESIAN_POINT('Ctrl Pts',(2.5104565071361,89.4676960780469,13.535874451767));
#43799=CARTESIAN_POINT('Ctrl Pts',(2.37940547667574,89.5470239663889,14.1100374774523));
#43800=CARTESIAN_POINT('Ctrl Pts',(2.28221157497402,89.5812808781357,14.3532486116256));
#43801=CARTESIAN_POINT('Ctrl Pts',(2.06661474240068,89.6359562540811,14.716058017857));
#43802=CARTESIAN_POINT('Ctrl Pts',(1.97077728174789,89.6567147310476,14.8466599521433));
#43803=CARTESIAN_POINT('Ctrl Pts',(1.76006132626174,89.6975160446304,15.0821379882182));
#43804=CARTESIAN_POINT('Ctrl Pts',(1.64668519347369,89.7174882555832,15.1873941516935));
#43805=CARTESIAN_POINT('Ctrl Pts',(1.25926540288717,89.7807712394764,15.4854270935864));
#43806=CARTESIAN_POINT('Ctrl Pts',(0.955928569384893,89.8230556129854,15.6341153718328));
#43807=CARTESIAN_POINT('Ctrl Pts',(0.47588115623038,89.8862569233562,15.7596088273576));
#43808=CARTESIAN_POINT('Ctrl Pts',(0.315858414766504,89.9067645785581,15.7852316710863));
#43809=CARTESIAN_POINT('Ctrl Pts',(-0.178758489715751,89.9695384933718,
15.8158534419732));
#43810=CARTESIAN_POINT('Ctrl Pts',(-0.5128089107048,90.0110951020614,15.7695224754184));
#43811=CARTESIAN_POINT('Ctrl Pts',(-0.980914054595601,90.0731649428838,
15.6052339635061));
#43812=CARTESIAN_POINT('Ctrl Pts',(-1.12834413828788,90.093352382921,15.536770055282));
#43813=CARTESIAN_POINT('Ctrl Pts',(-1.41087701492271,90.1341263072552,15.3704759451092));
#43814=CARTESIAN_POINT('Ctrl Pts',(-1.54494897055453,90.1546113378598,15.2724561154334));
#43815=CARTESIAN_POINT('Ctrl Pts',(-1.9010443501359,90.2136559253285,14.9533779167191));
#43816=CARTESIAN_POINT('Ctrl Pts',(-2.09262623372159,90.2516155141937,14.7030592156736));
#43817=CARTESIAN_POINT('Ctrl Pts',(-2.32357225104417,90.3143298066315,14.2441900446282));
#43818=CARTESIAN_POINT('Ctrl Pts',(-2.39200606433039,90.3387228604655,14.0541889532507));
#43819=CARTESIAN_POINT('Ctrl Pts',(-2.47883854408009,90.3857630654534,13.6749938333432));
#43820=CARTESIAN_POINT('Ctrl Pts',(-2.5000000000012,90.4082684462306,13.4878011326208));
#43821=CARTESIAN_POINT('Ctrl Pts',(-2.5,90.4307847167281,13.2999999999841));
#43822=CARTESIAN_POINT('',(2.49380022861477,88.7482468790765,13.1242986243742));
#43823=CARTESIAN_POINT('Ctrl Pts',(-2.5,89.5119815300394,13.3));
#43824=CARTESIAN_POINT('Ctrl Pts',(-2.5,89.4810423796734,13.5888724134592));
#43825=CARTESIAN_POINT('Ctrl Pts',(-2.44993209699204,89.4503589471884,13.8758588946447));
#43826=CARTESIAN_POINT('Ctrl Pts',(-2.25550598041351,89.386723099465,14.4149652188788));
#43827=CARTESIAN_POINT('Ctrl Pts',(-2.1145205937211,89.3558894266671,14.6636012356151));
#43828=CARTESIAN_POINT('Ctrl Pts',(-1.72695518427293,89.2925059282761,15.1371816758764));
#43829=CARTESIAN_POINT('Ctrl Pts',(-1.4712854181974,89.2600761614001,15.347657900266));
#43830=CARTESIAN_POINT('Ctrl Pts',(-1.0437449082664,89.2082805972365,15.5771293245674));
#43831=CARTESIAN_POINT('Ctrl Pts',(-0.898470128396195,89.1915201595237,
15.6382673932665));
#43832=CARTESIAN_POINT('Ctrl Pts',(-0.489441669287295,89.1472260303795,
15.7665965143056));
#43833=CARTESIAN_POINT('Ctrl Pts',(-0.218986886119816,89.1213352670832,
15.8051510850134));
#43834=CARTESIAN_POINT('Ctrl Pts',(0.386695141988435,89.0641691849577,15.7924291495129));
#43835=CARTESIAN_POINT('Ctrl Pts',(0.716050772460616,89.0303875130934,15.7184560611734));
#43836=CARTESIAN_POINT('Ctrl Pts',(1.26825396004202,88.9727120554833,15.4713748099971));
#43837=CARTESIAN_POINT('Ctrl Pts',(1.49584007436802,88.9494664761161,15.321362199537));
#43838=CARTESIAN_POINT('Ctrl Pts',(1.80937824712612,88.9140270927264,15.0321509241068));
#43839=CARTESIAN_POINT('Ctrl Pts',(1.91357251849696,88.9011856658873,14.9163063922395));
#43840=CARTESIAN_POINT('Ctrl Pts',(2.19258967471724,88.8598586562317,14.5409534548794));
#43841=CARTESIAN_POINT('Ctrl Pts',(2.33049526736143,88.8312407626482,14.2574036472055));
#43842=CARTESIAN_POINT('Ctrl Pts',(2.48608381650137,88.7854658454611,13.6848348898527));
#43843=CARTESIAN_POINT('Ctrl Pts',(2.513521888597,88.7677049407441,13.4039429441296));
#43844=CARTESIAN_POINT('Ctrl Pts',(2.49381725504168,88.7482160582468,13.1242857477141));
#43845=CARTESIAN_POINT('Ctrl Pts',(2.49381566113763,88.7484607548506,13.12426312776));
#43846=CARTESIAN_POINT('Ctrl Pts',(2.47565534574513,88.7070000631215,12.8665569425994));
#43847=CARTESIAN_POINT('Ctrl Pts',(2.41765147496816,88.6651844459182,12.6132136321295));
#43848=CARTESIAN_POINT('Ctrl Pts',(2.21301696079434,88.5761995865008,12.1004754446969));
#43849=CARTESIAN_POINT('Ctrl Pts',(2.05689746380474,88.5315830003039,11.8489259991677));
#43850=CARTESIAN_POINT('Ctrl Pts',(1.65040665773457,88.4384387277635,11.3960303305365));
#43851=CARTESIAN_POINT('Ctrl Pts',(1.39802601746336,88.3896655340998,11.2037090144886));
#43852=CARTESIAN_POINT('Ctrl Pts',(0.819588758961109,88.2914320737367,10.9149417394812));
#43853=CARTESIAN_POINT('Ctrl Pts',(0.495955679782436,88.2444147965749,10.8272734506959));
#43854=CARTESIAN_POINT('Ctrl Pts',(0.00453787822132061,88.1721718799112,
10.7948703357809));
#43855=CARTESIAN_POINT('Ctrl Pts',(-0.156050830368948,88.148541850119,10.799732329503));
#43856=CARTESIAN_POINT('Ctrl Pts',(-0.635349229729586,88.0774445711616,
10.8606198763144));
#43857=CARTESIAN_POINT('Ctrl Pts',(-0.944788939378858,88.0320309903952,
10.962969055852));
#43858=CARTESIAN_POINT('Ctrl Pts',(-1.48429869501355,87.9435592292897,11.2666467041139));
#43859=CARTESIAN_POINT('Ctrl Pts',(-1.71448532938947,87.9008458484831,11.4565718891768));
#43860=CARTESIAN_POINT('Ctrl Pts',(-2.1228309313702,87.8120499511084,11.93772816208));
#43861=CARTESIAN_POINT('Ctrl Pts',(-2.28605336365111,87.768145174016,12.2340625425692));
#43862=CARTESIAN_POINT('Ctrl Pts',(-2.46172645703544,87.6871063806446,12.7958318505116));
#43863=CARTESIAN_POINT('Ctrl Pts',(-2.5,87.6515555495105,13.0474641705025));
#43864=CARTESIAN_POINT('Ctrl Pts',(-2.5,87.6157001716673,13.3000000000002));
#43865=CARTESIAN_POINT('Origin',(0.,70.2,13.3));
#43866=CARTESIAN_POINT('',(-2.49999998851479,85.6233212596494,13.299784549362));
#43867=CARTESIAN_POINT('',(-2.5,86.6193069507268,13.3));
#43868=CARTESIAN_POINT('',(-2.5,70.2,13.3));
#43869=CARTESIAN_POINT('Ctrl Pts',(-2.5,86.6193069507268,13.3));
#43870=CARTESIAN_POINT('Ctrl Pts',(-2.5,86.6466224285355,13.0882700909667));
#43871=CARTESIAN_POINT('Ctrl Pts',(-2.47310162020712,86.6739408747903,12.8769977869022));
#43872=CARTESIAN_POINT('Ctrl Pts',(-2.33717304474614,86.7432060272066,12.3538430071535));
#43873=CARTESIAN_POINT('Ctrl Pts',(-2.19299741241983,86.7842030767294,12.0556505314509));
#43874=CARTESIAN_POINT('Ctrl Pts',(-1.89845883436738,86.8458435419989,11.665464747059));
#43875=CARTESIAN_POINT('Ctrl Pts',(-1.78943257350458,86.8660433988868,11.5467786512888));
#43876=CARTESIAN_POINT('Ctrl Pts',(-1.42031476505742,86.9283745224802,11.215522845001));
#43877=CARTESIAN_POINT('Ctrl Pts',(-1.12835965609482,86.9698982400417,11.0440809091017));
#43878=CARTESIAN_POINT('Ctrl Pts',(-0.660044278587822,87.0316091782384,
10.8834095432661));
#43879=CARTESIAN_POINT('Ctrl Pts',(-0.504163353457166,87.0514528251636,
10.8461478125476));
#43880=CARTESIAN_POINT('Ctrl Pts',(-0.0148979909304198,87.1127595257338,
10.7778177517056));
#43881=CARTESIAN_POINT('Ctrl Pts',(0.321954960890778,87.1535939154995,10.7983984756532));
#43882=CARTESIAN_POINT('Ctrl Pts',(0.796401612334706,87.2137847940213,10.925055463053));
#43883=CARTESIAN_POINT('Ctrl Pts',(0.943848795692934,87.2329188398661,10.9797050512545));
#43884=CARTESIAN_POINT('Ctrl Pts',(1.38639000358212,87.2929515301836,11.1929405664258));
#43885=CARTESIAN_POINT('Ctrl Pts',(1.65545708382981,87.3334111575162,11.3970342209617));
#43886=CARTESIAN_POINT('Ctrl Pts',(2.09063920004624,87.4129023369536,11.8913397762962));
#43887=CARTESIAN_POINT('Ctrl Pts',(2.2555061197234,87.4513297701916,12.1740337493058));
#43888=CARTESIAN_POINT('Ctrl Pts',(2.4142692291858,87.5095085883815,12.631487104091));
#43889=CARTESIAN_POINT('Ctrl Pts',(2.45210320271859,87.5286452993377,12.7873574458279));
#43890=CARTESIAN_POINT('Ctrl Pts',(2.51725670542116,87.5833614208896,13.2425587142243));
#43891=CARTESIAN_POINT('Ctrl Pts',(2.50600923919744,87.6181536114473,13.5445853195605));
#43892=CARTESIAN_POINT('Ctrl Pts',(2.36975068982988,87.6926827888213,14.1636264460045));
#43893=CARTESIAN_POINT('Ctrl Pts',(2.23328414475215,87.7318659425395,14.4722059293934));
#43894=CARTESIAN_POINT('Ctrl Pts',(1.85248841510107,87.8080604517333,15.0099025973434));
#43895=CARTESIAN_POINT('Ctrl Pts',(1.61491793120646,87.8447442584537,15.2358519541843));
#43896=CARTESIAN_POINT('Ctrl Pts',(1.08764544573736,87.9168828566478,15.5709007560183));
#43897=CARTESIAN_POINT('Ctrl Pts',(0.807547217265582,87.9508570739586,15.6849329705292));
#43898=CARTESIAN_POINT('Ctrl Pts',(0.360424704205339,88.0019452544041,15.7788475805645));
#43899=CARTESIAN_POINT('Ctrl Pts',(0.204268234737293,88.0193065650425,15.7965704328218));
#43900=CARTESIAN_POINT('Ctrl Pts',(-0.287258966713611,88.0743739751298,
15.8059084464013));
#43901=CARTESIAN_POINT('Ctrl Pts',(-0.619978172706541,88.1120388035939,
15.7449568493119));
#43902=CARTESIAN_POINT('Ctrl Pts',(-1.23105190151795,88.1839341142793,15.4998057128026));
#43903=CARTESIAN_POINT('Ctrl Pts',(-1.50506596143497,88.2181948120678,15.322228590379));
#43904=CARTESIAN_POINT('Ctrl Pts',(-1.95150383951295,88.2859948112912,14.8906373921834));
#43905=CARTESIAN_POINT('Ctrl Pts',(-2.12682915700285,88.3176526285759,14.6472925207583));
#43906=CARTESIAN_POINT('Ctrl Pts',(-2.32365163721931,88.3649981698067,14.2358180576044));
#43907=CARTESIAN_POINT('Ctrl Pts',(-2.37828215497575,88.3812051966122,14.0866910105076));
#43908=CARTESIAN_POINT('Ctrl Pts',(-2.47269020647712,88.4200082290749,13.7262271340283));
#43909=CARTESIAN_POINT('Ctrl Pts',(-2.50000000000002,88.4426309223165,13.5133457306453));
#43910=CARTESIAN_POINT('Ctrl Pts',(-2.5,88.464609916907,13.2999999999997));
#43911=CARTESIAN_POINT('Ctrl Pts',(-2.5,87.6157001716673,13.3000000000002));
#43912=CARTESIAN_POINT('Ctrl Pts',(-2.5,87.6048906897737,13.3761331114224));
#43913=CARTESIAN_POINT('Ctrl Pts',(-2.4965224112813,87.5940677933037,13.452350368579));
#43914=CARTESIAN_POINT('Ctrl Pts',(-2.46510757798474,87.5454743782036,13.7947448174624));
#43915=CARTESIAN_POINT('Ctrl Pts',(-2.39809759648182,87.5092925209849,14.0554947378149));
#43916=CARTESIAN_POINT('Ctrl Pts',(-2.16102875337192,87.4299927646321,14.5981855066975));
#43917=CARTESIAN_POINT('Ctrl Pts',(-1.97446098492741,87.3867291938527,14.8674059211297));
#43918=CARTESIAN_POINT('Ctrl Pts',(-1.50179762651519,87.2964549886563,15.3264396930274));
#43919=CARTESIAN_POINT('Ctrl Pts',(-1.21741653480531,87.2508484855315,15.5090665624559));
#43920=CARTESIAN_POINT('Ctrl Pts',(-0.594089858313682,87.163389292783,15.751238717163));
#43921=CARTESIAN_POINT('Ctrl Pts',(-0.261716373756765,87.121006090775,15.8085929817085));
#43922=CARTESIAN_POINT('Ctrl Pts',(0.369495063987766,87.0383197382512,15.7903782250777));
#43923=CARTESIAN_POINT('Ctrl Pts',(0.662968954884288,86.999087228789,15.7287824581235));
#43924=CARTESIAN_POINT('Ctrl Pts',(1.24884474031079,86.9165904250011,15.4914280926614));
#43925=CARTESIAN_POINT('Ctrl Pts',(1.53065417503801,86.8746009812092,15.3047763718407));
#43926=CARTESIAN_POINT('Ctrl Pts',(1.95169418101603,86.7983425328552,14.8839200494221));
#43927=CARTESIAN_POINT('Ctrl Pts',(2.10605889778836,86.7649315937189,14.6720095011498));
#43928=CARTESIAN_POINT('Ctrl Pts',(2.29093548057867,86.7125650457084,14.3112312392637));
#43929=CARTESIAN_POINT('Ctrl Pts',(2.34566095004559,86.693892675126,14.1768424648627));
#43930=CARTESIAN_POINT('Ctrl Pts',(2.48729441704505,86.6323240198447,13.7187538256714));
#43931=CARTESIAN_POINT('Ctrl Pts',(2.52096433896476,86.590453325082,13.3823820847822));
#43932=CARTESIAN_POINT('Ctrl Pts',(2.47170635126602,86.5285024519331,12.8935881743819));
#43933=CARTESIAN_POINT('Ctrl Pts',(2.44141781072855,86.5088471240641,12.7396567590519));
#43934=CARTESIAN_POINT('Ctrl Pts',(2.30300644825099,86.4476390572762,12.2726692707813));
#43935=CARTESIAN_POINT('Ctrl Pts',(2.14715563849133,86.4065960985094,11.9775063735307));
#43936=CARTESIAN_POINT('Ctrl Pts',(1.74658059918022,86.3273664067261,11.4856900616074));
#43937=CARTESIAN_POINT('Ctrl Pts',(1.51341345441157,86.2898878339531,11.2870727723557));
#43938=CARTESIAN_POINT('Ctrl Pts',(1.01354676556786,86.2186284722799,10.9983712063086));
#43939=CARTESIAN_POINT('Ctrl Pts',(0.755899027584269,86.1853458203392,10.9013730834781));
#43940=CARTESIAN_POINT('Ctrl Pts',(0.164164177956732,86.111639338047,10.7836844551613));
#43941=CARTESIAN_POINT('Ctrl Pts',(-0.168912606911206,86.0716259537327,
10.783994787668));
#43942=CARTESIAN_POINT('Ctrl Pts',(-0.783423096808428,85.9955451571676,
10.9074267337659));
#43943=CARTESIAN_POINT('Ctrl Pts',(-1.06181458238947,85.9602116328655,11.0172961032343));
#43944=CARTESIAN_POINT('Ctrl Pts',(-1.59892393627267,85.8845224624073,11.3492801308928));
#43945=CARTESIAN_POINT('Ctrl Pts',(-1.8452892123725,85.8446071613234,11.5804625622087));
#43946=CARTESIAN_POINT('Ctrl Pts',(-2.18010727624499,85.7760126044956,12.0523224408078));
#43947=CARTESIAN_POINT('Ctrl Pts',(-2.2914420907559,85.7475533148643,12.2709867692661));
#43948=CARTESIAN_POINT('Ctrl Pts',(-2.45582760355662,85.6868482894876,12.7592485550244));
#43949=CARTESIAN_POINT('Ctrl Pts',(-2.49997107572636,85.6548921126602,13.0285721308173));
#43950=CARTESIAN_POINT('Ctrl Pts',(-2.49999998579136,85.6233272066706,13.2997334606593));
#43951=CARTESIAN_POINT('Origin',(0.,70.2,13.3));
#43952=CARTESIAN_POINT('',(-2.50006911666048,83.7560733610116,13.3003763888455));
#43953=CARTESIAN_POINT('',(-2.5,84.5087322051727,13.3000000000001));
#43954=CARTESIAN_POINT('',(-2.5,70.2,13.3));
#43955=CARTESIAN_POINT('',(-2.03459967169508,84.6272597203354,11.8472323735682));
#43956=CARTESIAN_POINT('Ctrl Pts',(-2.5,84.5087322051727,13.3000000000002));
#43957=CARTESIAN_POINT('Ctrl Pts',(-2.5,84.5296744575748,13.0655280982184));
#43958=CARTESIAN_POINT('Ctrl Pts',(-2.46699906006975,84.5500080722109,12.8315998676825));
#43959=CARTESIAN_POINT('Ctrl Pts',(-2.32292977670388,84.5897770551703,12.3335388726652));
#43960=CARTESIAN_POINT('Ctrl Pts',(-2.19886900509429,84.6076007678664,12.0773365066594));
#43961=CARTESIAN_POINT('Ctrl Pts',(-2.03458002190507,84.6272882767454,11.8472494589694));
#43962=CARTESIAN_POINT('Ctrl Pts',(-2.03458055730488,84.627288638924,11.8472502087982));
#43963=CARTESIAN_POINT('Ctrl Pts',(-1.89450969771275,84.6662409459504,11.6510805384963));
#43964=CARTESIAN_POINT('Ctrl Pts',(-1.72676167686059,84.70488524973,11.4761414012548));
#43965=CARTESIAN_POINT('Ctrl Pts',(-1.33323554888588,84.7839203668059,11.1695331444189));
#43966=CARTESIAN_POINT('Ctrl Pts',(-1.10663251548048,84.824181403158,11.043490787527));
#43967=CARTESIAN_POINT('Ctrl Pts',(-0.713279434127413,84.8891603374553,
10.8984823803338));
#43968=CARTESIAN_POINT('Ctrl Pts',(-0.556769167311561,84.9137340255325,
10.8574444566412));
#43969=CARTESIAN_POINT('Ctrl Pts',(-0.0920359549528423,84.9854951466048,
10.7826265481142));
#43970=CARTESIAN_POINT('Ctrl Pts',(0.219863619697767,85.0323990958273,10.7905367664575));
#43971=CARTESIAN_POINT('Ctrl Pts',(0.829912779101551,85.1254292919659,10.9209057582261));
#43972=CARTESIAN_POINT('Ctrl Pts',(1.12231417855182,85.1718960945836,11.0440446262694));
#43973=CARTESIAN_POINT('Ctrl Pts',(1.6507300087735,85.2648134431928,11.3953957464715));
#43974=CARTESIAN_POINT('Ctrl Pts',(1.88082541594596,85.3108255938684,11.6222047214489));
#43975=CARTESIAN_POINT('Ctrl Pts',(2.154729054646,85.3805730708179,12.0216790741474));
#43976=CARTESIAN_POINT('Ctrl Pts',(2.23401550940231,85.4037764216242,12.1659173450706));
#43977=CARTESIAN_POINT('Ctrl Pts',(2.36216169616374,85.4501613860974,12.4655396180094));
#43978=CARTESIAN_POINT('Ctrl Pts',(2.41115940395367,85.4734047411207,12.6199789466383));
#43979=CARTESIAN_POINT('Ctrl Pts',(2.50542927385025,85.5380651617574,13.0615369731934));
#43980=CARTESIAN_POINT('Ctrl Pts',(2.51620520654007,85.5771720580018,13.3534227472839));
#43981=CARTESIAN_POINT('Ctrl Pts',(2.43286997623803,85.660417934164,13.9590573673342));
#43982=CARTESIAN_POINT('Ctrl Pts',(2.32815364430273,85.7046699769092,14.2658043051374));
#43983=CARTESIAN_POINT('Ctrl Pts',(2.04326879523016,85.7853727884209,14.7622662765919));
#43984=CARTESIAN_POINT('Ctrl Pts',(1.88594571676374,85.8206545389477,14.9602761163235));
#43985=CARTESIAN_POINT('Ctrl Pts',(1.45672746521806,85.8996631696703,15.3590473678497));
#43986=CARTESIAN_POINT('Ctrl Pts',(1.16867617371516,85.9429996836769,15.5351669355018));
#43987=CARTESIAN_POINT('Ctrl Pts',(0.567290294484066,86.0294344701491,15.7538890334455));
#43988=CARTESIAN_POINT('Ctrl Pts',(0.263389568511162,86.0713280760463,15.80479544449));
#43989=CARTESIAN_POINT('Ctrl Pts',(-0.347063720854757,86.153708880797,15.7945044066049));
#43990=CARTESIAN_POINT('Ctrl Pts',(-0.648508246571967,86.1927479533828,
15.7336233250396));
#43991=CARTESIAN_POINT('Ctrl Pts',(-1.22704950937592,86.2739753109181,15.5012940046377));
#43992=CARTESIAN_POINT('Ctrl Pts',(-1.49705895641803,86.3156531362169,15.3273375546511));
#43993=CARTESIAN_POINT('Ctrl Pts',(-1.90384652058772,86.3902653546794,14.9386270062663));
#43994=CARTESIAN_POINT('Ctrl Pts',(-2.05487870899703,86.4223406009384,14.744737410521));
#43995=CARTESIAN_POINT('Ctrl Pts',(-2.33984399672216,86.4969198229823,14.2415511770626));
#43996=CARTESIAN_POINT('Ctrl Pts',(-2.44450868436423,86.5389635819673,13.9211140722652));
#43997=CARTESIAN_POINT('Ctrl Pts',(-2.49440148476151,86.5943813575555,13.4932888285128));
#43998=CARTESIAN_POINT('Ctrl Pts',(-2.5,86.6068448891404,13.3965969251772));
#43999=CARTESIAN_POINT('Ctrl Pts',(-2.5,86.6193069507268,13.3));
#44000=CARTESIAN_POINT('',(2.14925682029349,84.6483054938945,12.0236057114313));
#44001=CARTESIAN_POINT('Ctrl Pts',(-2.5,85.6232961799494,13.299999999995));
#44002=CARTESIAN_POINT('Ctrl Pts',(-2.50000000000055,85.5917227576639,13.5712372036452));
#44003=CARTESIAN_POINT('Ctrl Pts',(-2.45585968378062,85.560975556195,13.8406868646292));
#44004=CARTESIAN_POINT('Ctrl Pts',(-2.27504200781115,85.4958832560464,14.3776917079628));
#44005=CARTESIAN_POINT('Ctrl Pts',(-2.13192098994924,85.4617229481704,14.6387221943466));
#44006=CARTESIAN_POINT('Ctrl Pts',(-1.75410765777896,85.3933213928303,15.1075309435492));
#44007=CARTESIAN_POINT('Ctrl Pts',(-1.51934906495187,85.3597252797142,15.3088945812207));
#44008=CARTESIAN_POINT('Ctrl Pts',(-1.10894810382751,85.3063223822594,15.5468531123579));
#44009=CARTESIAN_POINT('Ctrl Pts',(-0.955788647789875,85.2873824496154,
15.6161583606504));
#44010=CARTESIAN_POINT('Ctrl Pts',(-0.480112309063621,85.231316508119,15.7761164643413));
#44011=CARTESIAN_POINT('Ctrl Pts',(-0.145206934044905,85.1957537821981,
15.8180608233535));
#44012=CARTESIAN_POINT('Ctrl Pts',(0.347176162967513,85.1423661766384,15.7809117293853));
#44013=CARTESIAN_POINT('Ctrl Pts',(0.504742999838479,85.1248905459983,15.7537076929526));
#44014=CARTESIAN_POINT('Ctrl Pts',(0.940608188461335,85.0756692072896,15.6346732045655));
#44015=CARTESIAN_POINT('Ctrl Pts',(1.20697524144371,85.0448924842423,15.5087888422649));
#44016=CARTESIAN_POINT('Ctrl Pts',(1.57582668150888,84.9981323686656,15.2473704104133));
#44017=CARTESIAN_POINT('Ctrl Pts',(1.69691114033394,84.9817729703862,15.1428161339116));
#44018=CARTESIAN_POINT('Ctrl Pts',(2.02477759993649,84.9321002195505,14.7998083454098));
#44019=CARTESIAN_POINT('Ctrl Pts',(2.19749443666729,84.8992477097675,14.5330108934588));
#44020=CARTESIAN_POINT('Ctrl Pts',(2.37516628231922,84.8523744181851,14.0957358404697));
#44021=CARTESIAN_POINT('Ctrl Pts',(2.42041100154623,84.8371809870098,13.9451571559582));
#44022=CARTESIAN_POINT('Ctrl Pts',(2.51630609195442,84.7896560808508,13.4667250924553));
#44023=CARTESIAN_POINT('Ctrl Pts',(2.51626066285438,84.7563533960887,13.132390406575));
#44024=CARTESIAN_POINT('Ctrl Pts',(2.39548609200373,84.6982962618345,12.5310518927434));
#44025=CARTESIAN_POINT('Ctrl Pts',(2.29349171899702,84.6735589749346,12.2658148578631));
#44026=CARTESIAN_POINT('Ctrl Pts',(2.14935917264751,84.64798408829,12.0231855471698));
#44027=CARTESIAN_POINT('Ctrl Pts',(2.14849826856341,84.6481217304052,12.0232892114969));
#44028=CARTESIAN_POINT('Ctrl Pts',(2.11917051097377,84.6398957178875,11.9731483588035));
#44029=CARTESIAN_POINT('Ctrl Pts',(2.0879409562537,84.6315456703781,11.9242313897563));
#44030=CARTESIAN_POINT('Ctrl Pts',(2.05503530279454,84.6231699387726,11.8765751353672));
#44031=CARTESIAN_POINT('Ctrl Pts',(2.03758851112758,84.6187290713526,11.8513074790665));
#44032=CARTESIAN_POINT('Ctrl Pts',(2.01967012324788,84.6142808813125,11.8263934597074));
#44033=CARTESIAN_POINT('Ctrl Pts',(2.0013105791726,84.6098393338709,11.8018336082256));
#44034=CARTESIAN_POINT('Ctrl Pts',(1.95360166998468,84.598297577568,11.7380126484452));
#44035=CARTESIAN_POINT('Ctrl Pts',(1.90291702693478,84.5868009686769,11.6765816365097));
#44036=CARTESIAN_POINT('Ctrl Pts',(1.84940702252334,84.5753758491209,11.617721034844));
#44037=CARTESIAN_POINT('Ctrl Pts',(1.84334032278039,84.5740805255522,11.6110477108381));
#44038=CARTESIAN_POINT('Ctrl Pts',(1.83723725127936,84.5727861170242,11.6044074219133));
#44039=CARTESIAN_POINT('Ctrl Pts',(1.83109798478322,84.571492658943,11.597800428888));
#44040=CARTESIAN_POINT('Ctrl Pts',(1.81083540127987,84.5672236143602,11.5759941189706));
#44041=CARTESIAN_POINT('Ctrl Pts',(1.79017879691286,84.5629650561677,11.554550327143));
#44042=CARTESIAN_POINT('Ctrl Pts',(1.76913427802234,84.5587185485681,11.5334779347543));
#44043=CARTESIAN_POINT('Ctrl Pts',(1.76912118729655,84.5587159070315,11.5334648266898));
#44044=CARTESIAN_POINT('Ctrl Pts',(1.76910809642049,84.5587132654995,11.5334517187691));
#44045=CARTESIAN_POINT('Ctrl Pts',(1.76909500539423,84.5587106239721,11.5334386109921));
#44046=CARTESIAN_POINT('Ctrl Pts',(1.71326467222136,84.5474450935846,11.4775368399679));
#44047=CARTESIAN_POINT('Ctrl Pts',(1.65470244751872,84.5362629238947,11.4242464012593));
#44048=CARTESIAN_POINT('Ctrl Pts',(1.5935912865466,84.5251013315194,11.3737476542726));
#44049=CARTESIAN_POINT('Ctrl Pts',(1.58663034186001,84.5238299561126,11.3679955301282));
#44050=CARTESIAN_POINT('Ctrl Pts',(1.57963632720324,84.5225588525222,11.362279682546));
#44051=CARTESIAN_POINT('Ctrl Pts',(1.57260951578204,84.5212879316989,11.3566004206128));
#44052=CARTESIAN_POINT('Ctrl Pts',(1.54114987390819,84.5155979093606,11.3311738742295));
#44053=CARTESIAN_POINT('Ctrl Pts',(1.50903308308831,84.5099117604085,11.306480011195));
#44054=CARTESIAN_POINT('Ctrl Pts',(1.47628533748555,84.5042229325365,11.2825462510708));
#44055=CARTESIAN_POINT('Ctrl Pts',(1.40560170972749,84.4919440112159,11.2308869700934));
#44056=CARTESIAN_POINT('Ctrl Pts',(1.33234814011117,84.4797149402549,11.1830393232752));
#44057=CARTESIAN_POINT('Ctrl Pts',(1.25688466188294,84.4674885153415,11.1391740063337));
#44058=CARTESIAN_POINT('Ctrl Pts',(1.18024233305996,84.4550710956764,11.0946234485819));
#44059=CARTESIAN_POINT('Ctrl Pts',(1.10132102455115,84.4426565425067,11.0541814524054));
#44060=CARTESIAN_POINT('Ctrl Pts',(1.02050057260668,84.4302220882334,11.0180230316069));
#44061=CARTESIAN_POINT('Ctrl Pts',(0.939565585508334,84.417770012404,10.9818133687009));
#44062=CARTESIAN_POINT('Ctrl Pts',(0.856727000365074,84.4052982698638,10.9498996271201));
#44063=CARTESIAN_POINT('Ctrl Pts',(0.772357774959221,84.3928072041311,10.9224457497855));
#44064=CARTESIAN_POINT('Ctrl Pts',(0.705646887261843,84.3829304975559,10.9007379230404));
#44065=CARTESIAN_POINT('Ctrl Pts',(0.637979060749295,84.3730422331464,10.8818180164808));
#44066=CARTESIAN_POINT('Ctrl Pts',(0.569528632595271,84.3631508286921,10.8657628186098));
#44067=CARTESIAN_POINT('Ctrl Pts',(0.492890482829709,84.3520762604768,10.8477871726987));
#44068=CARTESIAN_POINT('Ctrl Pts',(0.415633948246713,84.3410498064073,10.8334872949032));
#44069=CARTESIAN_POINT('Ctrl Pts',(0.337996328823612,84.3300902367718,10.8228666141398));
#44070=CARTESIAN_POINT('Ctrl Pts',(0.327737236966226,84.3286420312183,10.82146318961));
#44071=CARTESIAN_POINT('Ctrl Pts',(0.317471425880949,84.3271949884746,10.820124044175));
#44072=CARTESIAN_POINT('Ctrl Pts',(0.307199384886591,84.3257491472112,10.8188492206551));
#44073=CARTESIAN_POINT('Ctrl Pts',(0.241293251306034,84.3164725285242,10.8106698637737));
#44074=CARTESIAN_POINT('Ctrl Pts',(0.17513263978019,84.3072459085532,10.8051360337245));
#44075=CARTESIAN_POINT('Ctrl Pts',(0.108833704360324,84.2980823991264,10.8022584452339));
#44076=CARTESIAN_POINT('Ctrl Pts',(0.108796485092262,84.2980772548642,10.8022568297971));
#44077=CARTESIAN_POINT('Ctrl Pts',(0.108759265780064,84.2980721106215,10.8022552151983));
#44078=CARTESIAN_POINT('Ctrl Pts',(0.108722046423735,84.2980669663986,10.8022536014376));
#44079=CARTESIAN_POINT('Ctrl Pts',(0.0315282094793017,84.2873977248123,
10.798906622949));
#44080=CARTESIAN_POINT('Ctrl Pts',(-0.0458583482863662,84.2768127737701,
10.7991611830844));
#44081=CARTESIAN_POINT('Ctrl Pts',(-0.123206969103929,84.2662556267233,
10.8030205706221));
#44082=CARTESIAN_POINT('Ctrl Pts',(-0.134614841424897,84.2646985907437,
10.8035897779305));
#44083=CARTESIAN_POINT('Ctrl Pts',(-0.146021823490824,84.2631421683135,
10.8042374633925));
#44084=CARTESIAN_POINT('Ctrl Pts',(-0.157427105394915,84.2615861873139,
10.8049637018818));
#44085=CARTESIAN_POINT('Ctrl Pts',(-0.238209670080459,84.2505653167376,
10.8101075824304));
#44086=CARTESIAN_POINT('Ctrl Pts',(-0.318910181397317,84.2395660218492,
10.8191901541463));
#44087=CARTESIAN_POINT('Ctrl Pts',(-0.399221905405393,84.2285423329785,
10.832224058259));
#44088=CARTESIAN_POINT('Ctrl Pts',(-0.40716638935307,84.2274518630582,10.8335133798777));
#44089=CARTESIAN_POINT('Ctrl Pts',(-0.415107035160441,84.2263611579551,
10.8348413913814));
#44090=CARTESIAN_POINT('Ctrl Pts',(-0.423043523069841,84.2252701754968,
10.8362081206935));
#44091=CARTESIAN_POINT('Ctrl Pts',(-0.509827441306192,84.2133404991037,
10.8511530341395));
#44092=CARTESIAN_POINT('Ctrl Pts',(-0.595661334196555,84.2014396006435,
10.8706460978654));
#44093=CARTESIAN_POINT('Ctrl Pts',(-0.680151385509904,84.1895334035807,
10.8945522574904));
#44094=CARTESIAN_POINT('Ctrl Pts',(-0.765810754833279,84.1774624281748,
10.918789271489));
#44095=CARTESIAN_POINT('Ctrl Pts',(-0.850087656711938,84.1653862403638,
10.9475623001945));
#44096=CARTESIAN_POINT('Ctrl Pts',(-0.932579965822,84.1532917784,10.980718122263));
#44097=CARTESIAN_POINT('Ctrl Pts',(-1.01489871165712,84.1412227631045,11.0138041847003));
#44098=CARTESIAN_POINT('Ctrl Pts',(-1.0954395486111,84.1291359036723,11.0512537216435));
#44099=CARTESIAN_POINT('Ctrl Pts',(-1.17382631390194,84.117035886723,11.0929096144844));
#44100=CARTESIAN_POINT('Ctrl Pts',(-1.23349316200181,84.1078255325178,11.1246174649281));
#44101=CARTESIAN_POINT('Ctrl Pts',(-1.29191246367207,84.0986079596607,11.158762141708));
#44102=CARTESIAN_POINT('Ctrl Pts',(-1.34893047897793,84.0893901288936,11.1952788927209));
#44103=CARTESIAN_POINT('Ctrl Pts',(-1.41374684242227,84.0789115763525,11.2367900360457));
#44104=CARTESIAN_POINT('Ctrl Pts',(-1.47645562641417,84.0684804861339,11.2811758377148));
#44105=CARTESIAN_POINT('Ctrl Pts',(-1.53690793086315,84.0581102114262,11.3282811495333));
#44106=CARTESIAN_POINT('Ctrl Pts',(-1.54661344555603,84.0564452814544,11.3358438272531));
#44107=CARTESIAN_POINT('Ctrl Pts',(-1.55626083141933,84.0547819109094,11.3434767058554));
#44108=CARTESIAN_POINT('Ctrl Pts',(-1.56584950640497,84.0531201457002,11.3511792634875));
#44109=CARTESIAN_POINT('Ctrl Pts',(-1.58076085088466,84.050535935315,11.3631575076555));
#44110=CARTESIAN_POINT('Ctrl Pts',(-1.5955302851023,84.0479556411926,11.3753041619004));
#44111=CARTESIAN_POINT('Ctrl Pts',(-1.61015577184586,84.0453794715716,11.3876173081328));
#44112=CARTESIAN_POINT('Ctrl Pts',(-1.61017318706277,84.0453764040119,11.3876319699432));
#44113=CARTESIAN_POINT('Ctrl Pts',(-1.61019060207545,84.0453733364582,11.3876466319895));
#44114=CARTESIAN_POINT('Ctrl Pts',(-1.61020801688417,84.0453702689102,11.387661294272));
#44115=CARTESIAN_POINT('Ctrl Pts',(-1.6702222848764,84.0347989989563,11.4381899084481));
#44116=CARTESIAN_POINT('Ctrl Pts',(-1.72781534394189,84.0242960017743,11.491523535541));
#44117=CARTESIAN_POINT('Ctrl Pts',(-1.78281861963694,84.0138159666427,11.5474935888694));
#44118=CARTESIAN_POINT('Ctrl Pts',(-1.78873192186358,84.0126892771083,11.5535108276027));
#44119=CARTESIAN_POINT('Ctrl Pts',(-1.79461524224577,84.0115628577759,11.5595585424526));
#44120=CARTESIAN_POINT('Ctrl Pts',(-1.80046833598367,84.01043665582,11.5656365256758));
#44121=CARTESIAN_POINT('Ctrl Pts',(-1.85778274524969,83.9994087101373,11.6251530879525));
#44122=CARTESIAN_POINT('Ctrl Pts',(-1.91220264883735,83.9884010673625,11.6875723068517));
#44123=CARTESIAN_POINT('Ctrl Pts',(-1.96349678520254,83.9773768953035,11.7526753058382));
#44124=CARTESIAN_POINT('Ctrl Pts',(-1.96727297368631,83.9765653142043,11.7574680796805));
#44125=CARTESIAN_POINT('Ctrl Pts',(-1.97103219826863,83.975753645517,11.7622753979488));
#44126=CARTESIAN_POINT('Ctrl Pts',(-1.97477435558608,83.974941875499,11.7670971725773));
#44127=CARTESIAN_POINT('Ctrl Pts',(-2.00390860505308,83.9686219086436,11.8046366913581));
#44128=CARTESIAN_POINT('Ctrl Pts',(-2.03200944070001,83.9622959963989,11.8430519541797));
#44129=CARTESIAN_POINT('Ctrl Pts',(-2.05903053186209,83.9559594509966,11.8822977714207));
#44130=CARTESIAN_POINT('Ctrl Pts',(-2.10927629639763,83.9441766341466,11.9552754346937));
#44131=CARTESIAN_POINT('Ctrl Pts',(-2.15552457366351,83.9324176323788,12.0307431773993));
#44132=CARTESIAN_POINT('Ctrl Pts',(-2.19760450671408,83.9206653708732,12.1083180328222));
#44133=CARTESIAN_POINT('Ctrl Pts',(-2.24010370136137,83.9087960162172,12.1866658019689));
#44134=CARTESIAN_POINT('Ctrl Pts',(-2.27835082976822,83.8969338428497,12.2671617205543));
#44135=CARTESIAN_POINT('Ctrl Pts',(-2.31219177387408,83.8850748620298,12.3494225010224));
#44136=CARTESIAN_POINT('Ctrl Pts',(-2.34577947277736,83.8733046266654,12.431067691454));
#44137=CARTESIAN_POINT('Ctrl Pts',(-2.37502734172382,83.8615378834169,12.5144502354414));
#44138=CARTESIAN_POINT('Ctrl Pts',(-2.39980300275635,83.8497790893336,12.5992242626934));
#44139=CARTESIAN_POINT('Ctrl Pts',(-2.41793252873578,83.8411746221292,12.661257438213));
#44140=CARTESIAN_POINT('Ctrl Pts',(-2.43366789394612,83.8325746030936,12.7240362618047));
#44141=CARTESIAN_POINT('Ctrl Pts',(-2.44695834901582,83.8239824445497,12.7874374646912));
#44142=CARTESIAN_POINT('Ctrl Pts',(-2.460347233552,83.8153266522494,12.8513082185857));
#44143=CARTESIAN_POINT('Ctrl Pts',(-2.471204606091,83.8067116911319,12.9155681000887));
#44144=CARTESIAN_POINT('Ctrl Pts',(-2.47953240888263,83.7981397773589,12.9801030274514));
#44145=CARTESIAN_POINT('Ctrl Pts',(-2.47954663266533,83.7981251366377,12.9802132522978));
#44146=CARTESIAN_POINT('Ctrl Pts',(-2.4795608490606,83.7981104960407,12.9803234779527));
#44147=CARTESIAN_POINT('Ctrl Pts',(-2.47957505806789,83.7980958555679,12.980433704416));
#44148=CARTESIAN_POINT('Ctrl Pts',(-2.48978104680403,83.7875799554521,13.0596067261839));
#44149=CARTESIAN_POINT('Ctrl Pts',(-2.49617918219035,83.7771276545593,13.1391989483178));
#44150=CARTESIAN_POINT('Ctrl Pts',(-2.49876087430341,83.7667036850347,13.2189438316804));
#44151=CARTESIAN_POINT('Ctrl Pts',(-2.49899788354894,83.7657467246211,13.2262647180652));
#44152=CARTESIAN_POINT('Ctrl Pts',(-2.49920269802926,83.7647900065606,13.2335868711549));
#44153=CARTESIAN_POINT('Ctrl Pts',(-2.49937529352148,83.763833505736,13.240910072088));
#44154=CARTESIAN_POINT('Ctrl Pts',(-2.49984232063202,83.7612453047894,13.2607259625703));
#44155=CARTESIAN_POINT('Ctrl Pts',(-2.50007366146133,83.7586587303504,13.2805495321041));
#44156=CARTESIAN_POINT('Ctrl Pts',(-2.50006911666048,83.7560733610116,13.3003763888455));
#44157=CARTESIAN_POINT('Origin',(0.,70.2,13.3));
#44158=CARTESIAN_POINT('',(-2.49945695676299,81.6745745895027,13.3008703539627));
#44159=CARTESIAN_POINT('',(-2.5,82.7842705339798,13.3000000461456));
#44160=CARTESIAN_POINT('',(-2.5,70.2,13.3));
#44161=CARTESIAN_POINT('Ctrl Pts',(-2.5,82.7842705395179,13.30000004682));
#44162=CARTESIAN_POINT('Ctrl Pts',(-2.50000000474803,82.8151486489161,13.0464743231556));
#44163=CARTESIAN_POINT('Ctrl Pts',(-2.46143312520029,82.8456950881806,12.7942093261388));
#44164=CARTESIAN_POINT('Ctrl Pts',(-2.29559019350917,82.913307429788,12.2653750201076));
#44165=CARTESIAN_POINT('Ctrl Pts',(-2.15481793884933,82.9496162619464,11.9973154498993));
#44166=CARTESIAN_POINT('Ctrl Pts',(-1.77133732543768,83.0243684274161,11.5065918089598));
#44167=CARTESIAN_POINT('Ctrl Pts',(-1.52552718495303,83.0624000292781,11.2933314358174));
#44168=CARTESIAN_POINT('Ctrl Pts',(-0.978817042207699,83.1380165311215,
10.979029248912));
#44169=CARTESIAN_POINT('Ctrl Pts',(-0.685479661821654,83.1744000363931,
10.876129893064));
#44170=CARTESIAN_POINT('Ctrl Pts',(-0.230925991395841,83.2286768540928,
10.8060729843433));
#44171=CARTESIAN_POINT('Ctrl Pts',(-0.0792523874947042,83.246459573482,
10.7966588088363));
#44172=CARTESIAN_POINT('Ctrl Pts',(0.40597672983133,83.3037729097049,10.8107043539447));
#44173=CARTESIAN_POINT('Ctrl Pts',(0.734341271195505,83.343726567668,10.887079955444));
#44174=CARTESIAN_POINT('Ctrl Pts',(1.29290248867132,83.415501730351,11.1420161353982));
#44175=CARTESIAN_POINT('Ctrl Pts',(1.52642631860712,83.4470317637685,11.3003642432778));
#44176=CARTESIAN_POINT('Ctrl Pts',(1.96977200461063,83.5172201949765,11.7248012931862));
#44177=CARTESIAN_POINT('Ctrl Pts',(2.16210557071182,83.5565757583034,12.0013363632263));
#44178=CARTESIAN_POINT('Ctrl Pts',(2.40434668893103,83.6266132227551,12.5613249417336));
#44179=CARTESIAN_POINT('Ctrl Pts',(2.47128925112929,83.6569863242284,12.8317076339978));
#44180=CARTESIAN_POINT('Ctrl Pts',(2.51847633634278,83.7249975186905,13.4430164826046));
#44181=CARTESIAN_POINT('Ctrl Pts',(2.47639648335978,83.7638242349361,13.7801922505863));
#44182=CARTESIAN_POINT('Ctrl Pts',(2.32211632612132,83.8179195687182,14.2376694798723));
#44183=CARTESIAN_POINT('Ctrl Pts',(2.26320478544772,83.8339892328385,14.3720869380744));
#44184=CARTESIAN_POINT('Ctrl Pts',(2.03327647388433,83.8857476511911,14.7920409828922));
#44185=CARTESIAN_POINT('Ctrl Pts',(1.8172110944513,83.9206614450298,15.0487405805084));
#44186=CARTESIAN_POINT('Ctrl Pts',(1.33675906134119,83.988904671192,15.4313357697943));
#44187=CARTESIAN_POINT('Ctrl Pts',(1.08792744616513,84.0195314593032,15.5684976495056));
#44188=CARTESIAN_POINT('Ctrl Pts',(0.512447306626639,84.0825800153206,15.7686752409219));
#44189=CARTESIAN_POINT('Ctrl Pts',(0.18549286044068,84.1148658541091,15.8144637113446));
#44190=CARTESIAN_POINT('Ctrl Pts',(-0.297842385271882,84.1663760915718,
15.7871608483506));
#44191=CARTESIAN_POINT('Ctrl Pts',(-0.453540252969198,84.183059015621,15.7635344772117));
#44192=CARTESIAN_POINT('Ctrl Pts',(-0.87086652634696,84.2273370307914,15.659261624922));
#44193=CARTESIAN_POINT('Ctrl Pts',(-1.12309700629158,84.2532555468506,15.5501672836693));
#44194=CARTESIAN_POINT('Ctrl Pts',(-1.63403978386678,84.3106087880742,15.2213979897503));
#44195=CARTESIAN_POINT('Ctrl Pts',(-1.87603810873575,84.3447079772851,14.9858870711083));
#44196=CARTESIAN_POINT('Ctrl Pts',(-2.2161326393584,84.4028897048695,14.4878602816455));
#44197=CARTESIAN_POINT('Ctrl Pts',(-2.33095487771852,84.4263308146894,14.2428805823425));
#44198=CARTESIAN_POINT('Ctrl Pts',(-2.44762140903683,84.4620722812837,13.8328188645868));
#44199=CARTESIAN_POINT('Ctrl Pts',(-2.47628360372299,84.4751148756247,13.677856235399));
#44200=CARTESIAN_POINT('Ctrl Pts',(-2.49673874376048,84.4955310389552,13.447508993848));
#44201=CARTESIAN_POINT('Ctrl Pts',(-2.5,84.502147214964,13.3737263188229));
#44202=CARTESIAN_POINT('Ctrl Pts',(-2.5,84.5087322051727,13.3000000000002));
#44203=CARTESIAN_POINT('',(0.920533865651003,82.4393565600724,10.9761000835092));
#44204=CARTESIAN_POINT('Ctrl Pts',(-2.49999997190418,83.756061301239,13.3003748053845));
#44205=CARTESIAN_POINT('Ctrl Pts',(-2.49997053707063,83.7304625818255,13.4967089193153));
#44206=CARTESIAN_POINT('Ctrl Pts',(-2.47681278101998,83.7050876939534,13.6923701395223));
#44207=CARTESIAN_POINT('Ctrl Pts',(-2.386442493329,83.6549243393185,14.0689985510949));
#44208=CARTESIAN_POINT('Ctrl Pts',(-2.3207540989909,83.6303163479419,14.2489869525319));
#44209=CARTESIAN_POINT('Ctrl Pts',(-2.17540180662083,83.588603526226,14.5391361695074));
#44210=CARTESIAN_POINT('Ctrl Pts',(-2.10611992772313,83.5715210295465,14.6535483090943));
#44211=CARTESIAN_POINT('Ctrl Pts',(-1.84384754758448,83.5141396907722,15.0173918612513));
#44212=CARTESIAN_POINT('Ctrl Pts',(-1.61301034700003,83.4742903313108,15.2358304578918));
#44213=CARTESIAN_POINT('Ctrl Pts',(-1.06657348378726,83.3921894241131,15.5855651570229));
#44214=CARTESIAN_POINT('Ctrl Pts',(-0.752239937707715,83.3507172289968,
15.7073982634096));
#44215=CARTESIAN_POINT('Ctrl Pts',(-0.100607888244321,83.2681416610412,
15.8193341419016));
#44216=CARTESIAN_POINT('Ctrl Pts',(0.229826195854046,83.2278622845284,15.8108536590563));
#44217=CARTESIAN_POINT('Ctrl Pts',(0.854323629728798,83.1489218889708,15.6702154373954));
#44218=CARTESIAN_POINT('Ctrl Pts',(1.14383932493661,83.1109645118561,15.544872369784));
#44219=CARTESIAN_POINT('Ctrl Pts',(1.53687818274458,83.0530562323332,15.278451413705));
#44220=CARTESIAN_POINT('Ctrl Pts',(1.6618751448833,83.0333993710254,15.1746844222207));
#44221=CARTESIAN_POINT('Ctrl Pts',(1.99964754439797,82.9753386868527,14.8337623860049));
#44222=CARTESIAN_POINT('Ctrl Pts',(2.17826535959274,82.9375944425982,14.567362465926));
#44223=CARTESIAN_POINT('Ctrl Pts',(2.42372800150795,82.8622912527412,13.9875530584655));
#44224=CARTESIAN_POINT('Ctrl Pts',(2.49051521068362,82.8256643283977,13.6802215306031));
#44225=CARTESIAN_POINT('Ctrl Pts',(2.50820308507383,82.749883453198,13.0350558370635));
#44226=CARTESIAN_POINT('Ctrl Pts',(2.45051170429726,82.7110712531846,12.7030768183537));
#44227=CARTESIAN_POINT('Ctrl Pts',(2.21264451975073,82.6353142833311,12.0927269729288));
#44228=CARTESIAN_POINT('Ctrl Pts',(2.03926080643865,82.5989342728309,11.8185321005017));
#44229=CARTESIAN_POINT('Ctrl Pts',(1.68967717139366,82.5407258716454,11.4478785655612));
#44230=CARTESIAN_POINT('Ctrl Pts',(1.54561286613422,82.5194619873994,11.3260548274809));
#44231=CARTESIAN_POINT('Ctrl Pts',(1.24219839653513,82.4785013781746,11.1232543168828));
#44232=CARTESIAN_POINT('Ctrl Pts',(1.08514199867268,82.4588978683154,11.0408518241034));
#44233=CARTESIAN_POINT('Ctrl Pts',(0.920701682247921,82.439197125928,10.9757133541007));
#44234=CARTESIAN_POINT('Ctrl Pts',(0.920507210407054,82.4391691851521,10.9761469785899));
#44235=CARTESIAN_POINT('Ctrl Pts',(0.84976445037318,82.426381971998,10.948000104283));
#44236=CARTESIAN_POINT('Ctrl Pts',(0.777916166713806,82.4135085909658,10.9232354764272));
#44237=CARTESIAN_POINT('Ctrl Pts',(0.705230255075198,82.4006744273682,10.9018091529748));
#44238=CARTESIAN_POINT('Ctrl Pts',(0.694119454342045,82.398712591421,10.8985339156563));
#44239=CARTESIAN_POINT('Ctrl Pts',(0.6829889829655,82.3967516629018,10.8953366906903));
#44240=CARTESIAN_POINT('Ctrl Pts',(0.671839691847331,82.3947920799437,10.8922173334976));
#44241=CARTESIAN_POINT('Ctrl Pts',(0.586872667320551,82.3798584010672,10.8684451944179));
#44242=CARTESIAN_POINT('Ctrl Pts',(0.500815373266157,82.3650031047442,10.8491915008198));
#44243=CARTESIAN_POINT('Ctrl Pts',(0.413984558834269,82.3502424772814,10.8345517612444));
#44244=CARTESIAN_POINT('Ctrl Pts',(0.327154114489939,82.3354819127309,10.8199120840661));
#44245=CARTESIAN_POINT('Ctrl Pts',(0.239549777812097,82.3208163506725,10.8098854974778));
#44246=CARTESIAN_POINT('Ctrl Pts',(0.151457802439923,82.3062793032402,10.804602088381));
#44247=CARTESIAN_POINT('Ctrl Pts',(0.151457426975483,82.3062792412806,10.8046020658621));
#44248=CARTESIAN_POINT('Ctrl Pts',(0.151457051511035,82.306279179321,10.8046020433433));
#44249=CARTESIAN_POINT('Ctrl Pts',(0.151456676046577,82.3062791173614,10.8046020208246));
#44250=CARTESIAN_POINT('Ctrl Pts',(0.0822104397887709,82.2948520186583,
10.800448936811));
#44251=CARTESIAN_POINT('Ctrl Pts',(0.0126607245485073,82.2835043155213,
10.7992276341647));
#44252=CARTESIAN_POINT('Ctrl Pts',(-0.0570059073669244,82.2721873246359,
10.8009360103044));
#44253=CARTESIAN_POINT('Ctrl Pts',(-0.14371378961836,82.258102069096,10.8030622746734));
#44254=CARTESIAN_POINT('Ctrl Pts',(-0.230151663471033,82.2441367908506,
10.8097146479824));
#44255=CARTESIAN_POINT('Ctrl Pts',(-0.315952706456719,82.2302199268284,
10.8207744957541));
#44256=CARTESIAN_POINT('Ctrl Pts',(-0.403178153725669,82.2160720255131,
10.8320179507872));
#44257=CARTESIAN_POINT('Ctrl Pts',(-0.489745485313005,82.2019740268762,
10.8478168688112));
#44258=CARTESIAN_POINT('Ctrl Pts',(-0.575270617001006,82.1878816168917,
10.8680721652291));
#44259=CARTESIAN_POINT('Ctrl Pts',(-0.661074709200265,82.173743241168,10.8883935291027));
#44260=CARTESIAN_POINT('Ctrl Pts',(-0.745829681226131,82.1596105377005,
10.9132004739449));
#44261=CARTESIAN_POINT('Ctrl Pts',(-0.829149800122876,82.1454701158155,
10.9424143426831));
#44262=CARTESIAN_POINT('Ctrl Pts',(-0.896122525388783,82.1341040423798,
10.9658964551772));
#44263=CARTESIAN_POINT('Ctrl Pts',(-0.96216825856647,82.1227336268377,10.9922261462949));
#44264=CARTESIAN_POINT('Ctrl Pts',(-1.02708814866811,82.1113658868256,11.0213733111377));
#44265=CARTESIAN_POINT('Ctrl Pts',(-1.10336977519159,82.0980086599932,11.0556215690949));
#44266=CARTESIAN_POINT('Ctrl Pts',(-1.17771424808106,82.0847211261591,11.0935876798491));
#44267=CARTESIAN_POINT('Ctrl Pts',(-1.24986448583372,82.0715335632568,11.1351336081243));
#44268=CARTESIAN_POINT('Ctrl Pts',(-1.25422160535989,82.0707371724254,11.1376425475396));
#44269=CARTESIAN_POINT('Ctrl Pts',(-1.25857072555773,82.0699411455125,11.1401645576712));
#44270=CARTESIAN_POINT('Ctrl Pts',(-1.26291179071775,82.0691454889291,11.1426996141131));
#44271=CARTESIAN_POINT('Ctrl Pts',(-1.31412432639877,82.0597589467627,11.1726062530819));
#44272=CARTESIAN_POINT('Ctrl Pts',(-1.36421607654112,82.0504245494676,11.2043270087693));
#44273=CARTESIAN_POINT('Ctrl Pts',(-1.41309955253088,82.0411578054689,11.2378252182875));
#44274=CARTESIAN_POINT('Ctrl Pts',(-1.41310394086109,82.0411569735818,11.2378282254633));
#44275=CARTESIAN_POINT('Ctrl Pts',(-1.41310832918156,82.0411561416953,11.2378312326534));
#44276=CARTESIAN_POINT('Ctrl Pts',(-1.41311271749229,82.0411553098093,11.2378342398578));
#44277=CARTESIAN_POINT('Ctrl Pts',(-1.48469698971785,82.0275851782536,11.2868892303627));
#44278=CARTESIAN_POINT('Ctrl Pts',(-1.5536938241786,82.0141586954001,11.3397565966466));
#44279=CARTESIAN_POINT('Ctrl Pts',(-1.61985078000212,82.0007828283404,11.3961809425237));
#44280=CARTESIAN_POINT('Ctrl Pts',(-1.68693280121697,81.987219928012,11.4533942637844));
#44281=CARTESIAN_POINT('Ctrl Pts',(-1.75109465428362,81.9737087318884,11.5142656241143));
#44282=CARTESIAN_POINT('Ctrl Pts',(-1.81203792615991,81.9601793605005,11.5785368018034));
#44283=CARTESIAN_POINT('Ctrl Pts',(-1.81926383290583,81.958575213349,11.5861572908605));
#44284=CARTESIAN_POINT('Ctrl Pts',(-1.82644445540145,81.956970844803,11.593825576645));
#44285=CARTESIAN_POINT('Ctrl Pts',(-1.8335792678427,81.9553661663048,11.6015412284807));
#44286=CARTESIAN_POINT('Ctrl Pts',(-1.89327644268047,81.9419397765216,11.666098302744));
#44287=CARTESIAN_POINT('Ctrl Pts',(-1.94945332063817,81.9285591200788,11.7336311899609));
#44288=CARTESIAN_POINT('Ctrl Pts',(-2.00190495204929,81.915190002813,11.8037989156827));
#44289=CARTESIAN_POINT('Ctrl Pts',(-2.05486837504321,81.9016904377135,11.8746512960177));
#44290=CARTESIAN_POINT('Ctrl Pts',(-2.1040333896945,81.8882027779552,11.9481899398141));
#44291=CARTESIAN_POINT('Ctrl Pts',(-2.14918746491882,81.8747225855896,12.0240873143052));
#44292=CARTESIAN_POINT('Ctrl Pts',(-2.19396401610349,81.8613550983708,12.0993501262838));
#44293=CARTESIAN_POINT('Ctrl Pts',(-2.23479676132122,81.84799526694,12.1769320227064));
#44294=CARTESIAN_POINT('Ctrl Pts',(-2.27147531358765,81.8346653241564,12.2565413372964));
#44295=CARTESIAN_POINT('Ctrl Pts',(-2.30066318307058,81.8240576909174,12.3198924277921));
#44296=CARTESIAN_POINT('Ctrl Pts',(-2.32722053987198,81.813469572234,12.384527860221));
#44297=CARTESIAN_POINT('Ctrl Pts',(-2.35103612877134,81.8029222000041,12.4503155687124));
#44298=CARTESIAN_POINT('Ctrl Pts',(-2.36200624994732,81.798063787645,12.4806192129805));
#44299=CARTESIAN_POINT('Ctrl Pts',(-2.37237341924686,81.7932235389059,12.5111090934759));
#44300=CARTESIAN_POINT('Ctrl Pts',(-2.38213316408953,81.7884038266734,12.5417713279222));
#44301=CARTESIAN_POINT('Ctrl Pts',(-2.38213497126972,81.788402934223,12.5417770055484));
#44302=CARTESIAN_POINT('Ctrl Pts',(-2.38213677842907,81.7884020417733,12.5417826831804));
#44303=CARTESIAN_POINT('Ctrl Pts',(-2.38213858556761,81.7884011493242,12.5417883608184));
#44304=CARTESIAN_POINT('Ctrl Pts',(-2.40822063813608,81.7755206192219,12.6237325227086));
#44305=CARTESIAN_POINT('Ctrl Pts',(-2.42996705299851,81.7627848366969,12.7069088786412));
#44306=CARTESIAN_POINT('Ctrl Pts',(-2.44737300812834,81.7501066243246,12.7909657542522));
#44307=CARTESIAN_POINT('Ctrl Pts',(-2.46525102449264,81.7370845702879,12.8773023089828));
#44308=CARTESIAN_POINT('Ctrl Pts',(-2.4785491035503,81.724122963737,12.9645680884214));
#44309=CARTESIAN_POINT('Ctrl Pts',(-2.48723432530795,81.7111558284396,13.0523726633709));
#44310=CARTESIAN_POINT('Ctrl Pts',(-2.49539167600486,81.698976810666,13.1348406452648));
#44311=CARTESIAN_POINT('Ctrl Pts',(-2.49947918835398,81.6867931450403,13.2177836784269));
#44312=CARTESIAN_POINT('Ctrl Pts',(-2.49945695676299,81.6745745895027,13.3008703539627));
#44313=CARTESIAN_POINT('Origin',(0.,70.2,13.3));
#44314=CARTESIAN_POINT('',(-2.5,79.5915676097122,13.3));
#44315=CARTESIAN_POINT('',(-2.49999989869882,80.7678846556286,13.3006754269486));
#44316=CARTESIAN_POINT('',(-2.5,70.2,13.3));
#44317=CARTESIAN_POINT('Ctrl Pts',(-2.5,80.7679766722356,13.2999999999636));
#44318=CARTESIAN_POINT('Ctrl Pts',(-2.49999999999743,80.7919940503135,13.1237066736875));
#44319=CARTESIAN_POINT('Ctrl Pts',(-2.48135257898582,80.8160657376386,12.9479000631705));
#44320=CARTESIAN_POINT('Ctrl Pts',(-2.40449147928125,80.8656754101913,12.5896891044419));
#44321=CARTESIAN_POINT('Ctrl Pts',(-2.34355439399043,80.8910969426707,12.4089970768672));
#44322=CARTESIAN_POINT('Ctrl Pts',(-2.1323483554941,80.9578859740607,11.9594402169915));
#44323=CARTESIAN_POINT('Ctrl Pts',(-1.95200779379245,80.9986680773843,11.7082328251797));
#44324=CARTESIAN_POINT('Ctrl Pts',(-1.50005750782899,81.0816867594947,11.2746672404786));
#44325=CARTESIAN_POINT('Ctrl Pts',(-1.22910592695524,81.1239888242985,11.0996727640186));
#44326=CARTESIAN_POINT('Ctrl Pts',(-0.622132238241597,81.2105497801797,
10.85563754211));
#44327=CARTESIAN_POINT('Ctrl Pts',(-0.289742232557924,81.2537155668831,
10.7943997868315));
#44328=CARTESIAN_POINT('Ctrl Pts',(0.378906709372972,81.3416969560312,10.8063952796647));
#44329=CARTESIAN_POINT('Ctrl Pts',(0.708421464602578,81.3847548048629,10.8792982086031));
#44330=CARTESIAN_POINT('Ctrl Pts',(1.15920293187042,81.4492114126598,11.0792950433409));
#44331=CARTESIAN_POINT('Ctrl Pts',(1.29806394747014,81.46999271598,11.1574981473877));
#44332=CARTESIAN_POINT('Ctrl Pts',(1.56092802817003,81.5117258795864,11.3405303600909));
#44333=CARTESIAN_POINT('Ctrl Pts',(1.68407459372433,81.5325267391818,11.4452989666089));
#44334=CARTESIAN_POINT('Ctrl Pts',(2.01344849481162,81.593772627866,11.7855611220864));
#44335=CARTESIAN_POINT('Ctrl Pts',(2.18668992149707,81.6339977394226,12.0486394497486));
#44336=CARTESIAN_POINT('Ctrl Pts',(2.37206751090576,81.6959212714359,12.4926489676096));
#44337=CARTESIAN_POINT('Ctrl Pts',(2.42117567545926,81.7175292392572,12.6546859991923));
#44338=CARTESIAN_POINT('Ctrl Pts',(2.51301675488385,81.7790396248975,13.1245661496585));
#44339=CARTESIAN_POINT('Ctrl Pts',(2.51540170769641,81.8185577968828,13.4371340404721));
#44340=CARTESIAN_POINT('Ctrl Pts',(2.40386216979899,81.8990292788653,14.0578293187524));
#44341=CARTESIAN_POINT('Ctrl Pts',(2.28691982456896,81.9396181738109,14.3596549603516));
#44342=CARTESIAN_POINT('Ctrl Pts',(2.02796594347174,82.0014185968546,14.7713185529014));
#44343=CARTESIAN_POINT('Ctrl Pts',(1.92607653879892,82.0223329024532,14.9023909362485));
#44344=CARTESIAN_POINT('Ctrl Pts',(1.70024326424352,82.0638260203644,15.1399653104941));
#44345=CARTESIAN_POINT('Ctrl Pts',(1.57733880143946,82.0843029246184,15.2463562682276));
#44346=CARTESIAN_POINT('Ctrl Pts',(1.17233692727742,82.1470572328373,15.5332193050472));
#44347=CARTESIAN_POINT('Ctrl Pts',(0.863690510392055,82.1886808319658,15.6697476837293));
#44348=CARTESIAN_POINT('Ctrl Pts',(0.379503208853912,82.250929777162,15.7763067879642));
#44349=CARTESIAN_POINT('Ctrl Pts',(0.218669114029323,82.2711547840977,15.7956570620044));
#44350=CARTESIAN_POINT('Ctrl Pts',(-0.109131336955512,82.3122024257939,
15.8031451044184));
#44351=CARTESIAN_POINT('Ctrl Pts',(-0.275325575811793,82.332920868852,15.7903501656056));
#44352=CARTESIAN_POINT('Ctrl Pts',(-0.600564073168092,82.3741292333048,
15.7323342732206));
#44353=CARTESIAN_POINT('Ctrl Pts',(-0.75888333096764,82.3945175299687,15.6876819955936));
#44354=CARTESIAN_POINT('Ctrl Pts',(-1.21607316545537,82.4556116920922,15.5086263790366));
#44355=CARTESIAN_POINT('Ctrl Pts',(-1.49415858908143,82.4958887774955,15.3308551159289));
#44356=CARTESIAN_POINT('Ctrl Pts',(-1.94913799063012,82.5738694127342,14.8946466969535));
#44357=CARTESIAN_POINT('Ctrl Pts',(-2.12809954443533,82.6108546906218,14.646566811081));
#44358=CARTESIAN_POINT('Ctrl Pts',(-2.40253056499088,82.6895940267774,14.0687282670974));
#44359=CARTESIAN_POINT('Ctrl Pts',(-2.48404468206299,82.7306970300942,13.738917591953));
#44360=CARTESIAN_POINT('Ctrl Pts',(-2.49929532159507,82.7759165854465,13.3685641927628));
#44361=CARTESIAN_POINT('Ctrl Pts',(-2.49999999935818,82.780096565306,13.3342705981348));
#44362=CARTESIAN_POINT('Ctrl Pts',(-2.5,82.7842705395179,13.30000004682));
#44363=CARTESIAN_POINT('Ctrl Pts',(-2.4999998261115,81.6749952458184,13.3009324389811));
#44364=CARTESIAN_POINT('Ctrl Pts',(-2.49991253633163,81.6405605469028,13.5349685946262));
#44365=CARTESIAN_POINT('Ctrl Pts',(-2.46696346326491,81.6058284433278,13.7678210047342));
#44366=CARTESIAN_POINT('Ctrl Pts',(-2.32746234213115,81.5318384401283,14.2515934989957));
#44367=CARTESIAN_POINT('Ctrl Pts',(-2.21144212941816,81.4940422500614,14.4967445953751));
#44368=CARTESIAN_POINT('Ctrl Pts',(-1.87818185910071,81.4105339024537,14.9802831866022));
#44369=CARTESIAN_POINT('Ctrl Pts',(-1.64970720082521,81.3649212471221,15.2050888306269));
#44370=CARTESIAN_POINT('Ctrl Pts',(-1.10617480949064,81.2723301938908,15.5668922268197));
#44371=CARTESIAN_POINT('Ctrl Pts',(-0.792482881520969,81.2269863668739,
15.694674443377));
#44372=CARTESIAN_POINT('Ctrl Pts',(-0.305885222944733,81.1579877356795,
15.7863540338617));
#44373=CARTESIAN_POINT('Ctrl Pts',(-0.14641747304618,81.1356671061898,15.8008166872527));
#44374=CARTESIAN_POINT('Ctrl Pts',(0.33631647022864,81.068466064175,15.7982413847432));
#44375=CARTESIAN_POINT('Ctrl Pts',(0.655951788470225,81.025363460793,15.7339520439778));
#44376=CARTESIAN_POINT('Ctrl Pts',(1.23977630781376,80.9396868701814,15.4927558358357));
#44377=CARTESIAN_POINT('Ctrl Pts',(1.50071189510592,80.8976116253231,15.3231388991448));
#44378=CARTESIAN_POINT('Ctrl Pts',(1.9671157445643,80.8107550473978,14.8789293715332));
#44379=CARTESIAN_POINT('Ctrl Pts',(2.16104664137428,80.7670092557745,14.6009593608744));
#44380=CARTESIAN_POINT('Ctrl Pts',(2.39439141454417,80.6886729004306,14.0618027257703));
#44381=CARTESIAN_POINT('Ctrl Pts',(2.45894886565495,80.6550316744386,13.8167865804675));
#44382=CARTESIAN_POINT('Ctrl Pts',(2.52138635184131,80.5782689387822,13.2338126945466));
#44383=CARTESIAN_POINT('Ctrl Pts',(2.48995284914939,80.5358865949142,12.8975853572706));
#44384=CARTESIAN_POINT('Ctrl Pts',(2.30089390179739,80.4505903893889,12.2713312541675));
#44385=CARTESIAN_POINT('Ctrl Pts',(2.15057778183786,80.4086501158078,11.9857418823028));
#44386=CARTESIAN_POINT('Ctrl Pts',(1.74537905123426,80.32403380283,11.4803167972005));
#44387=CARTESIAN_POINT('Ctrl Pts',(1.49180752192044,80.2827027831265,11.2672255635697));
#44388=CARTESIAN_POINT('Ctrl Pts',(1.07427192245701,80.2218625597934,11.0377125497692));
#44389=CARTESIAN_POINT('Ctrl Pts',(0.938178420999734,80.20293185114,10.9779699547945));
#44390=CARTESIAN_POINT('Ctrl Pts',(0.524495277091662,80.1470038199357,10.8387113041414));
#44391=CARTESIAN_POINT('Ctrl Pts',(0.237531674435638,80.1101825354509,10.7946798827699));
#44392=CARTESIAN_POINT('Ctrl Pts',(-0.358844376929671,80.0341640202705,
10.8067514790922));
#44393=CARTESIAN_POINT('Ctrl Pts',(-0.663334875007,79.9957531567254,10.8699603612868));
#44394=CARTESIAN_POINT('Ctrl Pts',(-1.24016568033655,79.9176729412342,11.1065420209301));
#44395=CARTESIAN_POINT('Ctrl Pts',(-1.50647293035896,79.8787046039393,11.2801417129448));
#44396=CARTESIAN_POINT('Ctrl Pts',(-1.8363841577928,79.8217387609598,11.5976268567848));
#44397=CARTESIAN_POINT('Ctrl Pts',(-1.93058492742045,79.8040343036143,11.7052509341366));
#44398=CARTESIAN_POINT('Ctrl Pts',(-2.21401866602675,79.744612481632,12.0912436803229));
#44399=CARTESIAN_POINT('Ctrl Pts',(-2.3563070459151,79.7034678779596,12.3995407202117));
#44400=CARTESIAN_POINT('Ctrl Pts',(-2.47774027658423,79.6385375323126,12.9150157743823));
#44401=CARTESIAN_POINT('Ctrl Pts',(-2.5,79.6150595569346,13.1073924341113));
#44402=CARTESIAN_POINT('Ctrl Pts',(-2.5,79.5915676097122,13.3));
#44403=CARTESIAN_POINT('Origin',(0.,70.2,13.3));
#44404=CARTESIAN_POINT('',(0.0622069118415443,78.2779999202659,10.8008522795397));
#44405=CARTESIAN_POINT('Ctrl Pts',(-2.5,79.5915676097122,13.3));
#44406=CARTESIAN_POINT('Ctrl Pts',(-2.5,79.5765893471849,13.4228049194608));
#44407=CARTESIAN_POINT('Ctrl Pts',(-2.49095183244887,79.5615902451076,13.5457018584579));
#44408=CARTESIAN_POINT('Ctrl Pts',(-2.42905647899425,79.5103106867224,13.9619631225716));
#44409=CARTESIAN_POINT('Ctrl Pts',(-2.33311627520834,79.4745828864616,14.2461061930075));
#44410=CARTESIAN_POINT('Ctrl Pts',(-2.11483283458189,79.4203135727282,14.6421625210424));
#44411=CARTESIAN_POINT('Ctrl Pts',(-2.02777490876142,79.4018575879159,14.7703903323516));
#44412=CARTESIAN_POINT('Ctrl Pts',(-1.71700853519764,79.3432769354389,15.1475574324335));
#44413=CARTESIAN_POINT('Ctrl Pts',(-1.45502808785973,79.3035168530704,15.3602269930674));
#44414=CARTESIAN_POINT('Ctrl Pts',(-0.870536320458681,79.2257575529658,
15.6660382611492));
#44415=CARTESIAN_POINT('Ctrl Pts',(-0.555372805189541,79.1881784743964,
15.7591739433774));
#44416=CARTESIAN_POINT('Ctrl Pts',(0.0689547438071552,79.1144225712145,
15.8171677303455));
#44417=CARTESIAN_POINT('Ctrl Pts',(0.37177162559577,79.0795738596712,15.7905292092738));
#44418=CARTESIAN_POINT('Ctrl Pts',(0.813737634667213,79.0270165160454,15.6690525947261));
#44419=CARTESIAN_POINT('Ctrl Pts',(0.960662794940438,79.0091851413643,15.6133751578383));
#44420=CARTESIAN_POINT('Ctrl Pts',(1.39918978441872,78.9530842841364,15.3981666218593));
#44421=CARTESIAN_POINT('Ctrl Pts',(1.66500041743212,78.9150325480588,15.1941727241333));
#44422=CARTESIAN_POINT('Ctrl Pts',(2.0978478448116,78.8411758699274,14.6983952064093));
#44423=CARTESIAN_POINT('Ctrl Pts',(2.26227010865142,78.8054826369546,14.4129268163996));
#44424=CARTESIAN_POINT('Ctrl Pts',(2.46292419306783,78.7354421192179,13.8221142684528));
#44425=CARTESIAN_POINT('Ctrl Pts',(2.50756858043878,78.7028085987227,13.5253606679568));
#44426=CARTESIAN_POINT('Ctrl Pts',(2.49438845861115,78.6537286585241,13.0699291846091));
#44427=CARTESIAN_POINT('Ctrl Pts',(2.47489621447307,78.6369255806952,12.9129704408489));
#44428=CARTESIAN_POINT('Ctrl Pts',(2.36985034709022,78.5844124596717,12.4391366042795));
#44429=CARTESIAN_POINT('Ctrl Pts',(2.23677091053079,78.5487737055021,12.1362737650858));
#44430=CARTESIAN_POINT('Ctrl Pts',(1.86562405784736,78.4811260038381,11.6053326362498));
#44431=CARTESIAN_POINT('Ctrl Pts',(1.633539081042,78.4489573179972,11.3806244304195));
#44432=CARTESIAN_POINT('Ctrl Pts',(1.15875266219343,78.3898965509339,11.0710637806197));
#44433=CARTESIAN_POINT('Ctrl Pts',(0.933219124018623,78.3646789547675,10.9676100711174));
#44434=CARTESIAN_POINT('Ctrl Pts',(0.489884079549194,78.319165331666,10.8390810709257));
#44435=CARTESIAN_POINT('Ctrl Pts',(0.276813594715694,78.298799748681,10.8061106932887));
#44436=CARTESIAN_POINT('Ctrl Pts',(0.0621484015592424,78.2779284766691,
10.8007726041467));
#44437=CARTESIAN_POINT('',(-2.5,77.5741002924676,13.3000000003379));
#44438=CARTESIAN_POINT('Ctrl Pts',(0.0619821551910609,78.2789454186495,
10.8007684756234));
#44439=CARTESIAN_POINT('Ctrl Pts',(-0.104887459920181,78.2455091533278,
10.7966300281528));
#44440=CARTESIAN_POINT('Ctrl Pts',(-0.271922990360639,78.2128217158413,
10.8092189380874));
#44441=CARTESIAN_POINT('Ctrl Pts',(-0.614414187643506,78.1449976468288,
10.8699487483443));
#44442=CARTESIAN_POINT('Ctrl Pts',(-0.788656239572891,78.1101407315737,
10.920744664503));
#44443=CARTESIAN_POINT('Ctrl Pts',(-1.24864492292068,78.0183993180752,11.1111327255881));
#44444=CARTESIAN_POINT('Ctrl Pts',(-1.51604373609959,77.9626022477322,11.2869701050732));
#44445=CARTESIAN_POINT('Ctrl Pts',(-1.96838320015796,77.8511640306151,11.7271156654777));
#44446=CARTESIAN_POINT('Ctrl Pts',(-2.15010403125278,77.7996110206432,11.986333026704));
#44447=CARTESIAN_POINT('Ctrl Pts',(-2.34743372797686,77.7191456011658,12.4241322392309));
#44448=CARTESIAN_POINT('Ctrl Pts',(-2.40044283594966,77.6913034022843,12.582023844553));
#44449=CARTESIAN_POINT('Ctrl Pts',(-2.47898775590883,77.6335137307816,12.9263758145357));
#44450=CARTESIAN_POINT('Ctrl Pts',(-2.5000000000506,77.6039710225773,13.1128609741768));
#44451=CARTESIAN_POINT('Ctrl Pts',(-2.5,77.5741002924676,13.3000000006759));
#44452=CARTESIAN_POINT('',(-2.5,78.5257776763231,13.3));
#44453=CARTESIAN_POINT('',(-2.5,70.2,13.3));
#44454=CARTESIAN_POINT('',(0.171877485205294,78.9529403329783,10.8041890652845));
#44455=CARTESIAN_POINT('Ctrl Pts',(-2.5,78.5257776763231,13.2999999999999));
#44456=CARTESIAN_POINT('Ctrl Pts',(-2.5,78.5374921201612,13.192701393122));
#44457=CARTESIAN_POINT('Ctrl Pts',(-2.49309211256744,78.5491001278162,13.08530859238));
#44458=CARTESIAN_POINT('Ctrl Pts',(-2.45895306334767,78.5776320699999,12.8220488663969));
#44459=CARTESIAN_POINT('Ctrl Pts',(-2.42390357232428,78.5944012804548,12.6678797589494));
#44460=CARTESIAN_POINT('Ctrl Pts',(-2.27266321667134,78.6466887304271,12.2086072991207));
#44461=CARTESIAN_POINT('Ctrl Pts',(-2.11120649888306,78.6820619745369,11.9219325597868));
#44462=CARTESIAN_POINT('Ctrl Pts',(-1.69032400712601,78.7495267532703,11.4302392127342));
#44463=CARTESIAN_POINT('Ctrl Pts',(-1.43630710763509,78.7818015743182,11.2287147601134));
#44464=CARTESIAN_POINT('Ctrl Pts',(-0.934258717810192,78.8406692098519,
10.9682936273892));
#44465=CARTESIAN_POINT('Ctrl Pts',(-0.70198902852392,78.8655951332596,10.8881584393048));
#44466=CARTESIAN_POINT('Ctrl Pts',(-0.252925044443173,78.9105886366888,
10.8037701643773));
#44467=CARTESIAN_POINT('Ctrl Pts',(-0.0399939993924468,78.9307258166804,
10.7913084605993));
#44468=CARTESIAN_POINT('Ctrl Pts',(0.171947635724521,78.9513559607842,10.805920207658));
#44469=CARTESIAN_POINT('Ctrl Pts',(0.171303481418846,78.9553621611337,10.8058758817465));
#44470=CARTESIAN_POINT('Ctrl Pts',(0.505867271394403,79.0245516761969,10.8288546667877));
#44471=CARTESIAN_POINT('Ctrl Pts',(0.831929165199084,79.0863319292476,10.9187702898156));
#44472=CARTESIAN_POINT('Ctrl Pts',(1.23052217204385,79.1735020953802,11.1209408397906));
#44473=CARTESIAN_POINT('Ctrl Pts',(1.32665033278514,79.1958273401737,11.1780930678944));
#44474=CARTESIAN_POINT('Ctrl Pts',(1.63536937636204,79.2662723917822,11.3908566956994));
#44475=CARTESIAN_POINT('Ctrl Pts',(1.82722107710317,79.3063688325274,11.5735409813187));
#44476=CARTESIAN_POINT('Ctrl Pts',(2.18172934994433,79.3983318517819,12.0378802394338));
#44477=CARTESIAN_POINT('Ctrl Pts',(2.32519576174729,79.450561402491,12.327446655297));
#44478=CARTESIAN_POINT('Ctrl Pts',(2.48050030556733,79.5526871729,12.8911251762962));
#44479=CARTESIAN_POINT('Ctrl Pts',(2.50992648690821,79.6001223886286,13.1561574926153));
#44480=CARTESIAN_POINT('Ctrl Pts',(2.4817442154734,79.6944068751355,13.736713999312));
#44481=CARTESIAN_POINT('Ctrl Pts',(2.4067385701941,79.7409703630377,14.0470738747417));
#44482=CARTESIAN_POINT('Ctrl Pts',(2.14174192637851,79.8388252292017,14.6293068551095));
#44483=CARTESIAN_POINT('Ctrl Pts',(1.95245057245882,79.8890169503679,14.8943553326399));
#44484=CARTESIAN_POINT('Ctrl Pts',(1.47484138064917,79.9899104232987,15.3462248317479));
#44485=CARTESIAN_POINT('Ctrl Pts',(1.18771380609895,80.0383247134631,15.5252268585384));
#44486=CARTESIAN_POINT('Ctrl Pts',(0.726853310411885,80.111607156897,15.6971359724758));
#44487=CARTESIAN_POINT('Ctrl Pts',(0.575091912529377,80.1348851208563,15.7380072204676));
#44488=CARTESIAN_POINT('Ctrl Pts',(0.255105968301367,80.1821333282104,15.7926001852218));
#44489=CARTESIAN_POINT('Ctrl Pts',(0.0873214593971162,80.2061723419182,
15.8041013366678));
#44490=CARTESIAN_POINT('Ctrl Pts',(-0.239383543702946,80.2533509862687,
15.7935933724892));
#44491=CARTESIAN_POINT('Ctrl Pts',(-0.397551125899607,80.2763502649642,
15.7733109938813));
#44492=CARTESIAN_POINT('Ctrl Pts',(-0.879279426513901,80.3473941635615,
15.6641045728957));
#44493=CARTESIAN_POINT('Ctrl Pts',(-1.18767938229527,80.3936092227799,15.5252178632953));
#44494=CARTESIAN_POINT('Ctrl Pts',(-1.58750127644831,80.4632663793177,15.2376943353219));
#44495=CARTESIAN_POINT('Ctrl Pts',(-1.70645156282528,80.4855189044681,15.1338111519495));
#44496=CARTESIAN_POINT('Ctrl Pts',(-1.92132795902574,80.5289745915201,14.9070061206651));
#44497=CARTESIAN_POINT('Ctrl Pts',(-2.01714654831655,80.5502304891351,14.7849571867929));
#44498=CARTESIAN_POINT('Ctrl Pts',(-2.22411274682521,80.6029904129379,14.4639924109367));
#44499=CARTESIAN_POINT('Ctrl Pts',(-2.32059410452609,80.6344752592051,14.2572888175016));
#44500=CARTESIAN_POINT('Ctrl Pts',(-2.46210955022574,80.7001052591825,13.8008974785368));
#44501=CARTESIAN_POINT('Ctrl Pts',(-2.49992465432316,80.7337057411103,13.5515590982602));
#44502=CARTESIAN_POINT('Ctrl Pts',(-2.49999988752857,80.7678745091697,13.300749904748));
#44503=CARTESIAN_POINT('Origin',(0.,70.2,13.3));
#44504=CARTESIAN_POINT('',(-2.5,75.3973313149984,13.3000000121208));
#44505=CARTESIAN_POINT('',(-2.5,76.6135035584265,13.2999999999132));
#44506=CARTESIAN_POINT('',(-2.5,70.2,13.3));
#44507=CARTESIAN_POINT('Ctrl Pts',(-2.5,76.6135035584265,13.2999999998264));
#44508=CARTESIAN_POINT('Ctrl Pts',(-2.49999999998539,76.640902869312,13.0895322308419));
#44509=CARTESIAN_POINT('Ctrl Pts',(-2.47342120095586,76.6677737652282,12.8798774831044));
#44510=CARTESIAN_POINT('Ctrl Pts',(-2.3781118132781,76.7170204228158,12.5100973809186));
#44511=CARTESIAN_POINT('Ctrl Pts',(-2.31840169439709,76.7391589961369,12.3490188539065));
#44512=CARTESIAN_POINT('Ctrl Pts',(-2.12608432661687,76.7959052654627,11.9585769422093));
#44513=CARTESIAN_POINT('Ctrl Pts',(-1.97271400315806,76.8304637746989,11.7417801334845));
#44514=CARTESIAN_POINT('Ctrl Pts',(-1.55432352359324,76.9084499187077,11.3135007781829));
#44515=CARTESIAN_POINT('Ctrl Pts',(-1.2745885757433,76.9505294341588,11.1233999946634));
#44516=CARTESIAN_POINT('Ctrl Pts',(-0.665469047182266,77.0347972873928,
10.8683177235145));
#44517=CARTESIAN_POINT('Ctrl Pts',(-0.343592375749612,77.0761912654679,
10.8024294587727));
#44518=CARTESIAN_POINT('Ctrl Pts',(0.224305597109283,77.1489271621091,10.7983050157087));
#44519=CARTESIAN_POINT('Ctrl Pts',(0.465768942230109,77.1796327922307,10.8318265258157));
#44520=CARTESIAN_POINT('Ctrl Pts',(1.01810755224723,77.2521309194086,10.992584925399));
#44521=CARTESIAN_POINT('Ctrl Pts',(1.31585192842238,77.2933169768907,11.1484246196224));
#44522=CARTESIAN_POINT('Ctrl Pts',(1.80560651333131,77.3719347136821,11.5454611603937));
#44523=CARTESIAN_POINT('Ctrl Pts',(2.0015333900107,77.4086412486526,11.772746904296));
#44524=CARTESIAN_POINT('Ctrl Pts',(2.23186471364254,77.4647845442123,12.1629328237427));
#44525=CARTESIAN_POINT('Ctrl Pts',(2.29820690462181,77.4839667178163,12.3038123258275));
#44526=CARTESIAN_POINT('Ctrl Pts',(2.46448498400187,77.5443102571003,12.7636937113607));
#44527=CARTESIAN_POINT('Ctrl Pts',(2.51399035998698,77.5848542874368,13.0970293775363));
#44528=CARTESIAN_POINT('Ctrl Pts',(2.4792250272564,77.6663169874103,13.7633551740978));
#44529=CARTESIAN_POINT('Ctrl Pts',(2.39535655664669,77.7065267839996,14.0896555908775));
#44530=CARTESIAN_POINT('Ctrl Pts',(2.11692598939642,77.7836716415707,14.664438237422));
#44531=CARTESIAN_POINT('Ctrl Pts',(1.93478729252063,77.819908957663,14.9123521587681));
#44532=CARTESIAN_POINT('Ctrl Pts',(1.48376859601782,77.8942561289083,15.3364222407047));
#44533=CARTESIAN_POINT('Ctrl Pts',(1.21650442379957,77.9315662180476,15.5065256145283));
#44534=CARTESIAN_POINT('Ctrl Pts',(0.616914435544194,78.0076284594651,15.7452344837372));
#44535=CARTESIAN_POINT('Ctrl Pts',(0.287797030902772,78.045956589178,15.8053804108854));
#44536=CARTESIAN_POINT('Ctrl Pts',(-0.340078085170195,78.1198400621924,
15.7944661472727));
#44537=CARTESIAN_POINT('Ctrl Pts',(-0.633483617053071,78.1540624494793,
15.7365500538306));
#44538=CARTESIAN_POINT('Ctrl Pts',(-1.05594351327345,78.2059808555621,15.5714678825535));
#44539=CARTESIAN_POINT('Ctrl Pts',(-1.19628421432258,78.223787946904,15.5007919969388));
#44540=CARTESIAN_POINT('Ctrl Pts',(-1.60741510921896,78.2795230211215,15.2427330232083));
#44541=CARTESIAN_POINT('Ctrl Pts',(-1.84865373409124,78.3171641432396,15.0148046712996));
#44542=CARTESIAN_POINT('Ctrl Pts',(-2.22847037713956,78.390763227938,14.4795104962304));
#44543=CARTESIAN_POINT('Ctrl Pts',(-2.36369876141874,78.4266339789996,14.1776392558598));
#44544=CARTESIAN_POINT('Ctrl Pts',(-2.47888946444884,78.4844613579317,13.6748672499996));
#44545=CARTESIAN_POINT('Ctrl Pts',(-2.5,78.5052984944755,13.4875793432979));
#44546=CARTESIAN_POINT('Ctrl Pts',(-2.5,78.5257776763231,13.2999999999999));
#44547=CARTESIAN_POINT('',(-2.49999942824129,77.573830409475,13.3016907966184));
#44548=CARTESIAN_POINT('Ctrl Pts',(-2.5,77.5741002924675,13.3000000006759));
#44549=CARTESIAN_POINT('Ctrl Pts',(-2.49999999999985,77.5740103330377,13.300563593198));
#44550=CARTESIAN_POINT('Ctrl Pts',(-2.49999980941778,77.5739203720443,13.301127191876));
#44551=CARTESIAN_POINT('Ctrl Pts',(-2.49999942824129,77.573830409475,13.3016907966182));
#44552=CARTESIAN_POINT('Ctrl Pts',(-2.49999942824129,77.573830409475,13.3016907966184));
#44553=CARTESIAN_POINT('Ctrl Pts',(-2.4998505811012,77.5387005635294,13.5217750817969));
#44554=CARTESIAN_POINT('Ctrl Pts',(-2.47064091555273,77.5033825159943,13.740893541864));
#44555=CARTESIAN_POINT('Ctrl Pts',(-2.3483376565198,77.429789750783,14.192603555114));
#44556=CARTESIAN_POINT('Ctrl Pts',(-2.24832776289067,77.3922965656205,14.4209456127892));
#44557=CARTESIAN_POINT('Ctrl Pts',(-2.03244148026049,77.3297355802073,14.7642416633179));
#44558=CARTESIAN_POINT('Ctrl Pts',(-1.93614254553577,77.3053765968394,14.8893973342427));
#44559=CARTESIAN_POINT('Ctrl Pts',(-1.71980881159253,77.2570344446502,15.1214711922229));
#44560=CARTESIAN_POINT('Ctrl Pts',(-1.59998907477998,77.2333548279477,15.2275763340365));
#44561=CARTESIAN_POINT('Ctrl Pts',(-1.21985180740028,77.1633293695089,15.5041530681793));
#44562=CARTESIAN_POINT('Ctrl Pts',(-0.937023136788006,77.1167539272231,
15.6384551993766));
#44563=CARTESIAN_POINT('Ctrl Pts',(-0.325696562787157,77.0237243318469,
15.7994850398668));
#44564=CARTESIAN_POINT('Ctrl Pts',(-0.00157318768005031,76.9774958228247,
15.8206327412019));
#44565=CARTESIAN_POINT('Ctrl Pts',(0.63174975682301,76.8851664667259,15.7394987781402));
#44566=CARTESIAN_POINT('Ctrl Pts',(0.935374303226106,76.8404184465601,15.6399543789379));
#44567=CARTESIAN_POINT('Ctrl Pts',(1.3028941703547,76.7808548813591,15.4361609030548));
#44568=CARTESIAN_POINT('Ctrl Pts',(1.39009367686082,76.7665074340061,15.3804588353565));
#44569=CARTESIAN_POINT('Ctrl Pts',(1.50535157950659,76.7463205190376,15.2963636060073));
#44570=CARTESIAN_POINT('Ctrl Pts',(1.53659892243022,76.7406681422641,15.2724126513246));
#44571=CARTESIAN_POINT('Ctrl Pts',(1.81904613870801,76.6889073900605,15.0451420920796));
#44572=CARTESIAN_POINT('Ctrl Pts',(2.02897514010295,76.6484341445869,14.7959177014732));
#44573=CARTESIAN_POINT('Ctrl Pts',(2.3044125404054,76.5736698642684,14.2996769558068));
#44574=CARTESIAN_POINT('Ctrl Pts',(2.39094677284079,76.5407430138779,14.0700120180514));
#44575=CARTESIAN_POINT('Ctrl Pts',(2.47192341580842,76.4874477557849,13.6978860278733));
#44576=CARTESIAN_POINT('Ctrl Pts',(2.48998737661861,76.4680577676827,13.5620527966633));
#44577=CARTESIAN_POINT('Ctrl Pts',(2.50731994501945,76.4191333719729,13.2170661773746));
#44578=CARTESIAN_POINT('Ctrl Pts',(2.49167006960422,76.3900369387755,13.0080606890604));
#44579=CARTESIAN_POINT('Ctrl Pts',(2.38327009156406,76.3168584472652,12.4733323875626));
#44580=CARTESIAN_POINT('Ctrl Pts',(2.25040410413921,76.2732649774488,12.160223554131));
#44581=CARTESIAN_POINT('Ctrl Pts',(1.88165383932843,76.1858267344357,11.6243497016782));
#44582=CARTESIAN_POINT('Ctrl Pts',(1.65673297807875,76.143246252331,11.4016782761849));
#44583=CARTESIAN_POINT('Ctrl Pts',(1.27826868862348,76.081701869475,11.1467762890589));
#44584=CARTESIAN_POINT('Ctrl Pts',(1.15331478493064,76.0627282967789,11.0773335725986));
#44585=CARTESIAN_POINT('Ctrl Pts',(0.880737790828388,76.0240851784733,10.9550845003908));
#44586=CARTESIAN_POINT('Ctrl Pts',(0.732726750098576,76.0044524348387,10.9047007074389));
#44587=CARTESIAN_POINT('Ctrl Pts',(0.454796393228603,75.9683176029859,10.8382959519578));
#44588=CARTESIAN_POINT('Ctrl Pts',(0.32649122453168,75.9519074811869,10.8180203891146));
#44589=CARTESIAN_POINT('Ctrl Pts',(0.0277475536918095,75.913455920915,10.7943811013704));
#44590=CARTESIAN_POINT('Ctrl Pts',(-0.142584306677741,75.8913396507178,
10.7982939050615));
#44591=CARTESIAN_POINT('Ctrl Pts',(-0.623538156815243,75.8270074461982,
10.8586237557184));
#44592=CARTESIAN_POINT('Ctrl Pts',(-0.925689021952383,75.7841518592404,
10.9564564924502));
#44593=CARTESIAN_POINT('Ctrl Pts',(-1.31863331537763,75.7247675861707,11.1718601340145));
#44594=CARTESIAN_POINT('Ctrl Pts',(-1.43023064939628,75.7075147965054,11.2451938153252));
#44595=CARTESIAN_POINT('Ctrl Pts',(-1.68474483337432,75.6661869413406,11.4432798817047));
#44596=CARTESIAN_POINT('Ctrl Pts',(-1.82034970448806,75.6423350379601,11.576019380759));
#44597=CARTESIAN_POINT('Ctrl Pts',(-2.07068845605139,75.5917233173125,11.8838908761042));
#44598=CARTESIAN_POINT('Ctrl Pts',(-2.18108506264707,75.56510243921,12.0606627621888));
#44599=CARTESIAN_POINT('Ctrl Pts',(-2.327449747465,75.5198200222404,12.3765606150119));
#44600=CARTESIAN_POINT('Ctrl Pts',(-2.37568238161733,75.5014569409713,12.5088664258353));
#44601=CARTESIAN_POINT('Ctrl Pts',(-2.46990638762609,75.4544805658895,12.8556620039472));
#44602=CARTESIAN_POINT('Ctrl Pts',(-2.49932241759073,75.4261114405848,13.0734822739441));
#44603=CARTESIAN_POINT('Ctrl Pts',(-2.49999614356494,75.3979755132803,13.2949294639965));
#44604=CARTESIAN_POINT('Ctrl Pts',(-2.50000000001249,75.3976534070846,13.2974647744158));
#44605=CARTESIAN_POINT('Ctrl Pts',(-2.5,75.3973313165138,13.3000000123134));
#44606=CARTESIAN_POINT('Origin',(0.,70.2,13.3));
#44607=CARTESIAN_POINT('',(-2.5,73.4944230382101,13.2999999999644));
#44608=CARTESIAN_POINT('',(-2.49999273450874,74.4211783466184,13.3001428234969));
#44609=CARTESIAN_POINT('',(-2.5,70.2,13.3));
#44610=CARTESIAN_POINT('',(-0.733503873481175,74.78666297405,10.9114679132036));
#44611=CARTESIAN_POINT('Ctrl Pts',(-2.49999999591027,74.4211798314431,13.3001429987339));
#44612=CARTESIAN_POINT('Ctrl Pts',(-2.50000751449558,74.436651893318,13.1686980360196));
#44613=CARTESIAN_POINT('Ctrl Pts',(-2.48964837222459,74.4520432857278,13.0374544083168));
#44614=CARTESIAN_POINT('Ctrl Pts',(-2.44723124009369,74.4837556590281,12.7705393309274));
#44615=CARTESIAN_POINT('Ctrl Pts',(-2.41406352581613,74.5000213738019,12.6354931731809));
#44616=CARTESIAN_POINT('Ctrl Pts',(-2.28678011758541,74.5466895483705,12.256593581168));
#44617=CARTESIAN_POINT('Ctrl Pts',(-2.16549504303506,74.5765971772256,12.0237856397495));
#44618=CARTESIAN_POINT('Ctrl Pts',(-1.84691883962062,74.6380215390291,11.5928048072836));
#44619=CARTESIAN_POINT('Ctrl Pts',(-1.64806494295363,74.669433844371,11.4001236101956));
#44620=CARTESIAN_POINT('Ctrl Pts',(-1.21099616275154,74.7296273166173,11.0979110585496));
#44621=CARTESIAN_POINT('Ctrl Pts',(-0.978969412809463,74.7580078043688,
10.9854055233531));
#44622=CARTESIAN_POINT('Ctrl Pts',(-0.733888726014597,74.7865824538561,
10.9101449127973));
#44623=CARTESIAN_POINT('',(-2.5002953309371,76.6131570886756,13.3019903645843));
#44624=CARTESIAN_POINT('Ctrl Pts',(-0.733451012361657,74.7865480661225,
10.9113467541027));
#44625=CARTESIAN_POINT('Ctrl Pts',(-0.673432073149203,74.7969027271255,
10.8925765472324));
#44626=CARTESIAN_POINT('Ctrl Pts',(-0.61279267897203,74.8074995342543,10.8762898556838));
#44627=CARTESIAN_POINT('Ctrl Pts',(-0.55172135071725,74.8181371867223,10.8623636258165));
#44628=CARTESIAN_POINT('Ctrl Pts',(-0.527242737521253,74.8224009711776,
10.8567817135846));
#44629=CARTESIAN_POINT('Ctrl Pts',(-0.502694159786421,74.8266713837145,
10.8515789143186));
#44630=CARTESIAN_POINT('Ctrl Pts',(-0.478085440360247,74.830935728438,10.8467469881344));
#44631=CARTESIAN_POINT('Ctrl Pts',(-0.391690881824103,74.8459066894804,
10.8297834020844));
#44632=CARTESIAN_POINT('Ctrl Pts',(-0.304556382645288,74.8608026951908,
10.8173866950697));
#44633=CARTESIAN_POINT('Ctrl Pts',(-0.217002215176073,74.8756018342364,
10.8096373887802));
#44634=CARTESIAN_POINT('Ctrl Pts',(-0.130399267725503,74.8902401901037,
10.8019722737461));
#44635=CARTESIAN_POINT('Ctrl Pts',(-0.0433852286454588,74.9047833866685,
10.7988533364698));
#44636=CARTESIAN_POINT('Ctrl Pts',(0.043758486802499,74.91919374792,10.8003936725185));
#44637=CARTESIAN_POINT('Ctrl Pts',(0.0566968067092791,74.9213332695468,
10.8006223678462));
#44638=CARTESIAN_POINT('Ctrl Pts',(0.0696380283409227,74.9234698394944,
10.8009538476554));
#44639=CARTESIAN_POINT('Ctrl Pts',(0.0825812731339249,74.9256033117317,
10.8013885670833));
#44640=CARTESIAN_POINT('Ctrl Pts',(0.0825820740862332,74.925603443755,10.8013885939845));
#44641=CARTESIAN_POINT('Ctrl Pts',(0.0825828750384656,74.9256035757782,
10.8013886208862));
#44642=CARTESIAN_POINT('Ctrl Pts',(0.0825836759907892,74.9256037078014,
10.8013886477882));
#44643=CARTESIAN_POINT('Ctrl Pts',(0.139654244730043,74.9350108117913,10.80330550976));
#44644=CARTESIAN_POINT('Ctrl Pts',(0.19676461313113,74.944358023619,10.8072290409036));
#44645=CARTESIAN_POINT('Ctrl Pts',(0.25380981250971,74.9536749586842,10.8131490801754));
#44646=CARTESIAN_POINT('Ctrl Pts',(0.339677955557163,74.9676994151093,10.8220603081942));
#44647=CARTESIAN_POINT('Ctrl Pts',(0.424954184620481,74.9815844407113,10.8354479249586));
#44648=CARTESIAN_POINT('Ctrl Pts',(0.50928181401435,74.995410860137,10.8531618287097));
#44649=CARTESIAN_POINT('Ctrl Pts',(0.595136153633828,75.0094876000813,10.8711964339697));
#44650=CARTESIAN_POINT('Ctrl Pts',(0.680007269306105,75.0235037767173,10.8937159352084));
#44651=CARTESIAN_POINT('Ctrl Pts',(0.76351528770202,75.0375128666789,10.9205871965277));
#44652=CARTESIAN_POINT('Ctrl Pts',(0.847496371018082,75.0516013167924,10.9476106809668));
#44653=CARTESIAN_POINT('Ctrl Pts',(0.93009870104371,75.0656826032932,10.979035547205));
#44654=CARTESIAN_POINT('Ctrl Pts',(1.01093371845271,75.0797779001705,11.0147460566196));
#44655=CARTESIAN_POINT('Ctrl Pts',(1.07649638558958,75.0912101394027,11.0437096953629));
#44656=CARTESIAN_POINT('Ctrl Pts',(1.14089641483889,75.1026509275967,11.0754928204192));
#44657=CARTESIAN_POINT('Ctrl Pts',(1.20392643847574,75.1140960024377,11.1100433369972));
#44658=CARTESIAN_POINT('Ctrl Pts',(1.27764029228284,75.1274810612552,11.1504502983314));
#44659=CARTESIAN_POINT('Ctrl Pts',(1.34910819872983,75.1408056987181,11.1944383492081));
#44660=CARTESIAN_POINT('Ctrl Pts',(1.41807234911295,75.1540415193412,11.2418370124753));
#44661=CARTESIAN_POINT('Ctrl Pts',(1.42188026116491,75.1547723460184,11.2444541684919));
#44662=CARTESIAN_POINT('Ctrl Pts',(1.42568054105983,75.1555029024436,11.2470817358406));
#44663=CARTESIAN_POINT('Ctrl Pts',(1.42947314570352,75.1562331840236,11.2497196904154));
#44664=CARTESIAN_POINT('Ctrl Pts',(1.48821328401066,75.1675438385859,11.2905765239462));
#44665=CARTESIAN_POINT('Ctrl Pts',(1.5451127816376,75.178787796999,11.3339221191132));
#44666=CARTESIAN_POINT('Ctrl Pts',(1.60001966060966,75.1899372720086,11.3796743104618));
#44667=CARTESIAN_POINT('Ctrl Pts',(1.60003342207554,75.189940066433,11.3796857774625));
#44668=CARTESIAN_POINT('Ctrl Pts',(1.60004718341631,75.1899428608514,11.3796972446146));
#44669=CARTESIAN_POINT('Ctrl Pts',(1.60006094463184,75.1899456552639,11.3797087119179));
#44670=CARTESIAN_POINT('Ctrl Pts',(1.6673443291717,75.2036085130715,11.4357763595104));
#44671=CARTESIAN_POINT('Ctrl Pts',(1.73163979777147,75.2171305775013,11.4954600813728));
#44672=CARTESIAN_POINT('Ctrl Pts',(1.79271504775094,75.2306050483382,11.5584796061301));
#44673=CARTESIAN_POINT('Ctrl Pts',(1.85244431910617,75.243782568287,11.6201103042635));
#44674=CARTESIAN_POINT('Ctrl Pts',(1.90909317913172,75.2569147376254,11.6849322179067));
#44675=CARTESIAN_POINT('Ctrl Pts',(1.96241051268122,75.270064831468,11.7526874122898));
#44676=CARTESIAN_POINT('Ctrl Pts',(2.01669904148912,75.2834544592096,11.8216767929899));
#44677=CARTESIAN_POINT('Ctrl Pts',(2.06724717224374,75.2967928725989,11.8933439766623));
#44678=CARTESIAN_POINT('Ctrl Pts',(2.1138843007413,75.3101179829707,11.9673353415709));
#44679=CARTESIAN_POINT('Ctrl Pts',(2.16101009854242,75.3235827154123,12.0421019966811));
#44680=CARTESIAN_POINT('Ctrl Pts',(2.20414236768937,75.3370337554537,12.1192416034528));
#44681=CARTESIAN_POINT('Ctrl Pts',(2.24309946485785,75.3504800299476,12.198411352111));
#44682=CARTESIAN_POINT('Ctrl Pts',(2.28179120955321,75.3638347164523,12.2770418437369));
#44683=CARTESIAN_POINT('Ctrl Pts',(2.31636476395523,75.377184419459,12.357674599306));
#44684=CARTESIAN_POINT('Ctrl Pts',(2.34663557544729,75.390511346333,12.4399993181984));
#44685=CARTESIAN_POINT('Ctrl Pts',(2.37076686222032,75.4011353064566,12.505626941053));
#44686=CARTESIAN_POINT('Ctrl Pts',(2.39216386483685,75.4117442086223,12.5723302337242));
#44687=CARTESIAN_POINT('Ctrl Pts',(2.41072662863896,75.4223188535665,12.6399658222181));
#44688=CARTESIAN_POINT('Ctrl Pts',(2.42243215395167,75.4289871372007,12.6826162648782));
#44689=CARTESIAN_POINT('Ctrl Pts',(2.43297973302564,75.435623911314,12.7255250621973));
#44690=CARTESIAN_POINT('Ctrl Pts',(2.44236065948483,75.4422232969214,12.7686548293934));
#44691=CARTESIAN_POINT('Ctrl Pts',(2.44236584688118,75.4422269462016,12.7686786789778));
#44692=CARTESIAN_POINT('Ctrl Pts',(2.44237103392073,75.4422305954703,12.7687025286298));
#44693=CARTESIAN_POINT('Ctrl Pts',(2.44237622060347,75.4422342447276,12.7687263783495));
#44694=CARTESIAN_POINT('Ctrl Pts',(2.46072654712334,75.4551452065906,12.853105964497));
#44695=CARTESIAN_POINT('Ctrl Pts',(2.47461400085036,75.4679150002155,12.9383338657672));
#44696=CARTESIAN_POINT('Ctrl Pts',(2.48406042479723,75.4806324337433,13.0240546792843));
#44697=CARTESIAN_POINT('Ctrl Pts',(2.49367121346562,75.4935711465014,13.1112670072327));
#44698=CARTESIAN_POINT('Ctrl Pts',(2.49868415566037,75.5064559074555,13.1989897404089));
#44699=CARTESIAN_POINT('Ctrl Pts',(2.49909641203807,75.5193519910899,13.2868352131255));
#44700=CARTESIAN_POINT('Ctrl Pts',(2.49951140053525,75.5323335400882,13.3752628583458));
#44701=CARTESIAN_POINT('Ctrl Pts',(2.495263900863,75.5453266418256,13.4638146101252));
#44702=CARTESIAN_POINT('Ctrl Pts',(2.48633709196862,75.5583670927344,13.5520823114472));
#44703=CARTESIAN_POINT('Ctrl Pts',(2.48364724855088,75.5622964667646,13.5786793068808));
#44704=CARTESIAN_POINT('Ctrl Pts',(2.4805324830723,75.5662299259216,13.6052504431002));
#44705=CARTESIAN_POINT('Ctrl Pts',(2.47699218299231,75.5701678989593,13.6317844060255));
#44706=CARTESIAN_POINT('Ctrl Pts',(2.46528649345273,75.5831884590115,13.7195166109914));
#44707=CARTESIAN_POINT('Ctrl Pts',(2.44899149821608,75.5961919028125,13.806378913221));
#44708=CARTESIAN_POINT('Ctrl Pts',(2.42822322194485,75.6091743378299,13.8919968916897));
#44709=CARTESIAN_POINT('Ctrl Pts',(2.40740031121669,75.6221909253344,13.9778401027052));
#44710=CARTESIAN_POINT('Ctrl Pts',(2.38208137503915,75.6351860176116,14.0624323536811));
#44711=CARTESIAN_POINT('Ctrl Pts',(2.35236220815066,75.6481314832766,14.1454285113532));
#44712=CARTESIAN_POINT('Ctrl Pts',(2.32489555181246,75.6600957707647,14.2221341252329));
#44713=CARTESIAN_POINT('Ctrl Pts',(2.29367077963975,75.6720172721161,14.2974769611409));
#44714=CARTESIAN_POINT('Ctrl Pts',(2.25873663231306,75.6838596094595,14.3712075534845));
#44715=CARTESIAN_POINT('Ctrl Pts',(2.25685841419233,75.6844963071977,14.375171644358));
#44716=CARTESIAN_POINT('Ctrl Pts',(2.25496946130733,75.6851327769405,14.3791310771119));
#44717=CARTESIAN_POINT('Ctrl Pts',(2.25306977696079,75.6857690133209,14.3830858136331));
#44718=CARTESIAN_POINT('Ctrl Pts',(2.25306658016676,75.6857700839812,14.3830924686746));
#44719=CARTESIAN_POINT('Ctrl Pts',(2.25306338334234,75.6857711546408,14.3830991237028));
#44720=CARTESIAN_POINT('Ctrl Pts',(2.25306018648752,75.6857722252999,14.3831057787176));
#44721=CARTESIAN_POINT('Ctrl Pts',(2.22243593725604,75.6960285960637,14.4468574490815));
#44722=CARTESIAN_POINT('Ctrl Pts',(2.18902432755426,75.7062241969384,14.5093912418138));
#44723=CARTESIAN_POINT('Ctrl Pts',(2.15290592708741,75.7164060231917,14.5705373831612));
#44724=CARTESIAN_POINT('Ctrl Pts',(2.10866139269601,75.7288786176589,14.6454405493805));
#44725=CARTESIAN_POINT('Ctrl Pts',(2.06058442629697,75.741267291856,14.7178723154643));
#44726=CARTESIAN_POINT('Ctrl Pts',(2.00893945857773,75.7536364929604,14.78756381264));
#44727=CARTESIAN_POINT('Ctrl Pts',(1.95648556985937,75.7661994342675,14.8583468956568));
#44728=CARTESIAN_POINT('Ctrl Pts',(1.90035073741023,75.7787423214424,14.9263025021805));
#44729=CARTESIAN_POINT('Ctrl Pts',(1.84080541521727,75.7913032226803,14.9911382774124));
#44730=CARTESIAN_POINT('Ctrl Pts',(1.78111316121511,75.8038951187281,15.0561340389775));
#44731=CARTESIAN_POINT('Ctrl Pts',(1.71799383596212,75.8165049741781,15.117994034378));
#44732=CARTESIAN_POINT('Ctrl Pts',(1.6517134736397,75.8291427017163,15.1764225844277));
#44733=CARTESIAN_POINT('Ctrl Pts',(1.5990675273059,75.8391807446968,15.2228319008903));
#44734=CARTESIAN_POINT('Ctrl Pts',(1.54442734183659,75.8492357618664,15.2670763422543));
#44735=CARTESIAN_POINT('Ctrl Pts',(1.4879202749969,75.8593011931669,15.3090092861084));
#44736=CARTESIAN_POINT('Ctrl Pts',(1.42231117942937,75.8709879410563,15.3576966923855));
#44737=CARTESIAN_POINT('Ctrl Pts',(1.3545068213907,75.8826320789913,15.4030297515981));
#44738=CARTESIAN_POINT('Ctrl Pts',(1.28475077245473,75.8942095722137,15.444881694988));
#44739=CARTESIAN_POINT('Ctrl Pts',(1.27871108705053,75.8952119858811,15.4485053602541));
#44740=CARTESIAN_POINT('Ctrl Pts',(1.27265673912055,75.8962139017588,15.4521029219175));
#44741=CARTESIAN_POINT('Ctrl Pts',(1.26658786902862,75.8972153052834,15.4556742931523));
#44742=CARTESIAN_POINT('Ctrl Pts',(1.21572309807101,75.9056083274014,15.4856068797972));
#44743=CARTESIAN_POINT('Ctrl Pts',(1.16383977803469,75.9139648112094,15.5137008071853));
#44744=CARTESIAN_POINT('Ctrl Pts',(1.11101530300954,75.9222723589206,15.5399090451328));
#44745=CARTESIAN_POINT('Ctrl Pts',(1.11099275017228,75.9222759057381,15.539920234456));
#44746=CARTESIAN_POINT('Ctrl Pts',(1.11097019716324,75.9222794525467,15.5399314234353));
#44747=CARTESIAN_POINT('Ctrl Pts',(1.1109476439824,75.9222829993466,15.5399426120706));
#44748=CARTESIAN_POINT('Ctrl Pts',(1.03849226736117,75.933677610141,15.5758877317773));
#44749=CARTESIAN_POINT('Ctrl Pts',(0.964263053763198,75.9449815130845,15.6082870623993));
#44750=CARTESIAN_POINT('Ctrl Pts',(0.888522792730374,75.9562620121927,15.6370424190572));
#44751=CARTESIAN_POINT('Ctrl Pts',(0.882729811883871,75.9571247992281,15.6392417675686));
#44752=CARTESIAN_POINT('Ctrl Pts',(0.876927997441459,75.9579874472851,15.6414197746847));
#44753=CARTESIAN_POINT('Ctrl Pts',(0.871117470341167,75.9588499854481,15.6435763845172));
#44754=CARTESIAN_POINT('Ctrl Pts',(0.788277248438114,75.9711471233134,15.6743229990672));
#44755=CARTESIAN_POINT('Ctrl Pts',(0.703664325561586,75.983422613545,15.7007248351678));
#44756=CARTESIAN_POINT('Ctrl Pts',(0.617648796075465,75.995736457179,15.7226245731082));
#44757=CARTESIAN_POINT('Ctrl Pts',(0.608067858723901,75.9971080486244,15.7250639002678));
#44758=CARTESIAN_POINT('Ctrl Pts',(0.598469549791323,75.9984800870089,15.7274473540847));
#44759=CARTESIAN_POINT('Ctrl Pts',(0.588854403214788,75.9998526334047,15.729774706648));
#44760=CARTESIAN_POINT('Ctrl Pts',(0.503102455857692,76.0120935831757,15.7505310219989));
#44761=CARTESIAN_POINT('Ctrl Pts',(0.416463419919644,76.0243127067554,15.766715883117));
#44762=CARTESIAN_POINT('Ctrl Pts',(0.32934856527692,76.03653712927,15.7783111241274));
#44763=CARTESIAN_POINT('Ctrl Pts',(0.241430789949471,76.0488742219112,15.7900132362207));
#44764=CARTESIAN_POINT('Ctrl Pts',(0.153029212895176,76.0612164676254,15.7970407405293));
#44765=CARTESIAN_POINT('Ctrl Pts',(0.0645493278428554,76.0735649869199,
15.7993796972489));
#44766=CARTESIAN_POINT('Ctrl Pts',(-0.0230985086592275,76.0857973830122,
15.80169665885));
#44767=CARTESIAN_POINT('Ctrl Pts',(-0.110822535722874,76.0980355546637,
15.7994135583182));
#44768=CARTESIAN_POINT('Ctrl Pts',(-0.198256686777905,76.1102592735339,
15.7925159596017));
#44769=CARTESIAN_POINT('Ctrl Pts',(-0.269506223325971,76.1202203047086,
15.7868951500448));
#44770=CARTESIAN_POINT('Ctrl Pts',(-0.340563746673898,76.1301712481095,
15.7782104512091));
#44771=CARTESIAN_POINT('Ctrl Pts',(-0.411248703774869,76.1400932863411,
15.7664465105473));
#44772=CARTESIAN_POINT('Ctrl Pts',(-0.44133857644335,76.1443169978527,15.7614387197653));
#44773=CARTESIAN_POINT('Ctrl Pts',(-0.471306198061353,76.1485276771993,
15.755881959445));
#44774=CARTESIAN_POINT('Ctrl Pts',(-0.501139789789567,76.1527237137163,
15.7497803106777));
#44775=CARTESIAN_POINT('Ctrl Pts',(-0.501197011215927,76.1527317617984,
15.7497686075932));
#44776=CARTESIAN_POINT('Ctrl Pts',(-0.501254232148938,76.1527398098271,
15.7497569025029));
#44777=CARTESIAN_POINT('Ctrl Pts',(-0.501311452588403,76.1527478578024,
15.7497451954068));
#44778=CARTESIAN_POINT('Ctrl Pts',(-0.580947228216661,76.1639485190249,
15.7334520021067));
#44779=CARTESIAN_POINT('Ctrl Pts',(-0.659630015256989,76.1750462039147,
15.7132769711695));
#44780=CARTESIAN_POINT('Ctrl Pts',(-0.737114781406418,76.1861013148928,
15.6893371215363));
#44781=CARTESIAN_POINT('Ctrl Pts',(-0.741951721823921,76.186791423617,15.687842690669));
#44782=CARTESIAN_POINT('Ctrl Pts',(-0.746783982146367,76.1874813649855,
15.6863335770746));
#44783=CARTESIAN_POINT('Ctrl Pts',(-0.751611498013482,76.1881711531107,
15.684809804654));
#44784=CARTESIAN_POINT('Ctrl Pts',(-0.835239102038435,76.2001204309129,
15.6584133224633));
#44785=CARTESIAN_POINT('Ctrl Pts',(-0.917446329446927,76.2120243199748,
15.6276207561274));
#44786=CARTESIAN_POINT('Ctrl Pts',(-0.997890138365169,76.2239362109078,
15.5925692869216));
#44787=CARTESIAN_POINT('Ctrl Pts',(-1.0789228246198,76.2359353011256,15.5572612284754));
#44788=CARTESIAN_POINT('Ctrl Pts',(-1.15816533534941,76.2479424786977,15.5176311885102));
#44789=CARTESIAN_POINT('Ctrl Pts',(-1.23524624877195,76.2599888541402,15.4738223576914));
#44790=CARTESIAN_POINT('Ctrl Pts',(-1.27100436126527,76.2655772109601,15.4534992837804));
#44791=CARTESIAN_POINT('Ctrl Pts',(-1.30629707352708,76.2711736775701,15.4322769955763));
#44792=CARTESIAN_POINT('Ctrl Pts',(-1.34108657282719,76.2767797302698,15.4101702111085));
#44793=CARTESIAN_POINT('Ctrl Pts',(-1.415759134045,76.2888126230056,15.3627199675086));
#44794=CARTESIAN_POINT('Ctrl Pts',(-1.48771758185659,76.300827454443,15.3114463334864));
#44795=CARTESIAN_POINT('Ctrl Pts',(-1.55667988000077,76.3128244045749,15.2566116217886));
#44796=CARTESIAN_POINT('Ctrl Pts',(-1.62213921269428,76.3242119651859,15.2045622595606));
#44797=CARTESIAN_POINT('Ctrl Pts',(-1.68489918208202,76.3355831139414,15.1493048957895));
#44798=CARTESIAN_POINT('Ctrl Pts',(-1.74474088032925,76.3469255124351,15.0910409012296));
#44799=CARTESIAN_POINT('Ctrl Pts',(-1.74812837979167,76.3475675792535,15.0877427119062));
#44800=CARTESIAN_POINT('Ctrl Pts',(-1.75150652690978,76.3482095547653,15.0844348742236));
#44801=CARTESIAN_POINT('Ctrl Pts',(-1.75487528148195,76.3488514370288,15.0811174197373));
#44802=CARTESIAN_POINT('Ctrl Pts',(-1.80561391389885,76.358519172545,15.0311514456266));
#44803=CARTESIAN_POINT('Ctrl Pts',(-1.85422289573364,76.3681651830346,14.9790071471326));
#44804=CARTESIAN_POINT('Ctrl Pts',(-1.90057536777064,76.3777775107188,14.9247866797692));
#44805=CARTESIAN_POINT('Ctrl Pts',(-1.90062224681902,76.3777872322451,14.924731843343));
#44806=CARTESIAN_POINT('Ctrl Pts',(-1.90066912355759,76.3777969537375,14.9246770047901));
#44807=CARTESIAN_POINT('Ctrl Pts',(-1.9007159979862,76.3778066751962,14.9246221641105));
#44808=CARTESIAN_POINT('Ctrl Pts',(-1.95231041277473,76.3885070289554,14.8642593424878));
#44809=CARTESIAN_POINT('Ctrl Pts',(-2.00111051102113,76.3991667756396,14.8013195262346));
#44810=CARTESIAN_POINT('Ctrl Pts',(-2.04691567528589,76.4098334589787,14.7360005086112));
#44811=CARTESIAN_POINT('Ctrl Pts',(-2.05012799429443,76.4105815141423,14.7314196818573));
#44812=CARTESIAN_POINT('Ctrl Pts',(-2.05332556257768,76.4113296017097,14.7268271568184));
#44813=CARTESIAN_POINT('Ctrl Pts',(-2.05650830149135,76.4120777373028,14.7222230034536));
#44814=CARTESIAN_POINT('Ctrl Pts',(-2.10629072825319,76.4237796099294,14.6502076940295));
#44815=CARTESIAN_POINT('Ctrl Pts',(-2.1521892024876,76.4354331050823,14.5757230003587));
#44816=CARTESIAN_POINT('Ctrl Pts',(-2.19403695991354,76.4470776657862,14.4991364969011));
#44817=CARTESIAN_POINT('Ctrl Pts',(-2.23643541816,76.4588754645494,14.4215421437309));
#44818=CARTESIAN_POINT('Ctrl Pts',(-2.27467494882356,76.4706638994492,14.341791060917));
#44819=CARTESIAN_POINT('Ctrl Pts',(-2.30859138972386,76.4824603329568,14.2602705222529));
#44820=CARTESIAN_POINT('Ctrl Pts',(-2.34239086443858,76.4942160846065,14.1790311199994));
#44821=CARTESIAN_POINT('Ctrl Pts',(-2.37189690399192,76.5059794565488,14.0960355989326));
#44822=CARTESIAN_POINT('Ctrl Pts',(-2.39696388450254,76.5177482893823,14.0116574646967));
#44823=CARTESIAN_POINT('Ctrl Pts',(-2.41650145088532,76.5269210875434,13.9458919291074));
#44824=CARTESIAN_POINT('Ctrl Pts',(-2.4333428481211,76.5360967607975,13.8792864653539));
#44825=CARTESIAN_POINT('Ctrl Pts',(-2.4474244211088,76.5452678718641,13.8120084540209));
#44826=CARTESIAN_POINT('Ctrl Pts',(-2.46306349950581,76.5554533621558,13.7372890959951));
#44827=CARTESIAN_POINT('Ctrl Pts',(-2.47522838680595,76.5655876315513,13.6620766505065));
#44828=CARTESIAN_POINT('Ctrl Pts',(-2.48392759067115,76.5756563141987,13.5865868434683));
#44829=CARTESIAN_POINT('Ctrl Pts',(-2.48540853634816,76.5773703988748,13.5737355176317));
#44830=CARTESIAN_POINT('Ctrl Pts',(-2.48678898196702,76.5790825920282,13.5608760472049));
#44831=CARTESIAN_POINT('Ctrl Pts',(-2.48806889087532,76.5807928342119,13.5480093684867));
#44832=CARTESIAN_POINT('Ctrl Pts',(-2.49254950722509,76.5867799314504,13.502966591881));
#44833=CARTESIAN_POINT('Ctrl Pts',(-2.49579901758045,76.5927428739485,13.4578359689247));
#44834=CARTESIAN_POINT('Ctrl Pts',(-2.49781663356568,76.59867840509,13.412654387648));
#44835=CARTESIAN_POINT('Ctrl Pts',(-2.49782108997901,76.5986915152062,13.4125545927402));
#44836=CARTESIAN_POINT('Ctrl Pts',(-2.49782554038138,76.5987046251887,13.4124547975822));
#44837=CARTESIAN_POINT('Ctrl Pts',(-2.49782998477221,76.5987177350374,13.4123550021743));
#44838=CARTESIAN_POINT('Ctrl Pts',(-2.49946714175907,76.6035469413954,13.3755938901972));
#44839=CARTESIAN_POINT('Ctrl Pts',(-2.50028876863852,76.6083580330503,13.3387986941934));
#44840=CARTESIAN_POINT('Ctrl Pts',(-2.5002953309371,76.6131570886756,13.3019903645843));
#44841=CARTESIAN_POINT('Ctrl Pts',(-2.49999919892924,76.6132430042317,13.3020013378422));
#44842=CARTESIAN_POINT('Ctrl Pts',(-2.49999973298295,76.613329861406,13.3013342171668));
#44843=CARTESIAN_POINT('Ctrl Pts',(-2.50000000000005,76.6134167127929,13.3006671044415));
#44844=CARTESIAN_POINT('Ctrl Pts',(-2.5,76.6135035584265,13.2999999998264));
#44845=CARTESIAN_POINT('',(-2.4999999270496,73.494492116903,13.2993960529866));
#44846=CARTESIAN_POINT('Ctrl Pts',(-2.5,75.3973313165138,13.3000000123134));
#44847=CARTESIAN_POINT('Ctrl Pts',(-2.49999999930815,75.3794855759421,13.4404673277535));
#44848=CARTESIAN_POINT('Ctrl Pts',(-2.48816179457868,75.3615006572095,13.5806882486726));
#44849=CARTESIAN_POINT('Ctrl Pts',(-2.45095445436725,75.3332520774929,13.7994517894063));
#44850=CARTESIAN_POINT('Ctrl Pts',(-2.43338834493185,75.3229050248894,13.8790088385834));
#44851=CARTESIAN_POINT('Ctrl Pts',(-2.36938303214634,75.2919598298753,14.1137818437225));
#44852=CARTESIAN_POINT('Ctrl Pts',(-2.31171814593751,75.2714156745673,14.2654938052394));
#44853=CARTESIAN_POINT('Ctrl Pts',(-2.0948220817595,75.2094987503269,14.7029305970115));
#44854=CARTESIAN_POINT('Ctrl Pts',(-1.89399762693792,75.1686958122473,14.9641156730433));
#44855=CARTESIAN_POINT('Ctrl Pts',(-1.39769529827426,75.085326161972,15.3995014584683));
#44856=CARTESIAN_POINT('Ctrl Pts',(-1.10513603679065,75.0437866196789,15.5671908650294));
#44857=CARTESIAN_POINT('Ctrl Pts',(-0.635224349127472,74.9816679945857,
15.7233247668668));
#44858=CARTESIAN_POINT('Ctrl Pts',(-0.477601342132093,74.96149582157,15.759250211776));
#44859=CARTESIAN_POINT('Ctrl Pts',(0.00557082576147318,74.9005214840376,
15.8211373284657));
#44860=CARTESIAN_POINT('Ctrl Pts',(0.333770523264666,74.8602562950338,15.7989557265504));
#44861=CARTESIAN_POINT('Ctrl Pts',(0.806534464814458,74.7993341183018,15.6719796575195));
#44862=CARTESIAN_POINT('Ctrl Pts',(0.960047577135318,74.7790364042287,15.6141079638523));
#44863=CARTESIAN_POINT('Ctrl Pts',(1.25098845094371,74.7387396892959,15.470457553408));
#44864=CARTESIAN_POINT('Ctrl Pts',(1.38797483721028,74.7188438722729,15.3855183534228));
#44865=CARTESIAN_POINT('Ctrl Pts',(1.64125378238698,74.6794328915327,15.1923936235826));
#44866=CARTESIAN_POINT('Ctrl Pts',(1.75732842027187,74.6600066475558,15.0851237520893));
#44867=CARTESIAN_POINT('Ctrl Pts',(2.08631059955819,74.5991786079486,14.7176946522855));
#44868=CARTESIAN_POINT('Ctrl Pts',(2.25752652155513,74.5582589250647,14.4252330328735));
#44869=CARTESIAN_POINT('Ctrl Pts',(2.41834594181126,74.4973362844201,13.9541606773706));
#44870=CARTESIAN_POINT('Ctrl Pts',(2.45569313558712,74.4775627525761,13.7958778664999));
#44871=CARTESIAN_POINT('Ctrl Pts',(2.49926677107777,74.4377923045067,13.473728490575));
#44872=CARTESIAN_POINT('Ctrl Pts',(2.50527587115069,74.4179256063479,13.3106077671179));
#44873=CARTESIAN_POINT('Ctrl Pts',(2.48591052115193,74.3791271198315,12.9925618485189));
#44874=CARTESIAN_POINT('Ctrl Pts',(2.46192808661686,74.3602767894519,12.8382814999868));
#44875=CARTESIAN_POINT('Ctrl Pts',(2.3429262047644,74.3015459577404,12.3675809227022));
#44876=CARTESIAN_POINT('Ctrl Pts',(2.19966323029684,74.2621185759085,12.0670280133111));
#44877=CARTESIAN_POINT('Ctrl Pts',(1.91062036874315,74.2042817750153,11.6804578957822));
#44878=CARTESIAN_POINT('Ctrl Pts',(1.80800134049828,74.1860362191448,11.5666463778398));
#44879=CARTESIAN_POINT('Ctrl Pts',(1.48995679492643,74.1339292109434,11.2730881712845));
#44880=CARTESIAN_POINT('Ctrl Pts',(1.25382301214976,74.1001662766046,11.119104232612));
#44881=CARTESIAN_POINT('Ctrl Pts',(0.737991110913591,74.0333338360369,10.8947554316624));
#44882=CARTESIAN_POINT('Ctrl Pts',(0.461640395918053,74.0007827039911,10.8267945107951));
#44883=CARTESIAN_POINT('Ctrl Pts',(-0.152956009339652,73.9287428698101,
10.7824824854762));
#44884=CARTESIAN_POINT('Ctrl Pts',(-0.487134590031164,73.8888815077343,
10.8253330033193));
#44885=CARTESIAN_POINT('Ctrl Pts',(-1.06689216198579,73.8171841973809,11.0219812491073));
#44886=CARTESIAN_POINT('Ctrl Pts',(-1.31395600857547,73.7857292972642,11.1549625923103));
#44887=CARTESIAN_POINT('Ctrl Pts',(-1.79978338394291,73.7154979029411,11.5324961074332));
#44888=CARTESIAN_POINT('Ctrl Pts',(-2.02110396006483,73.675917157806,11.7905658659855));
#44889=CARTESIAN_POINT('Ctrl Pts',(-2.28838954888656,73.6126840262612,12.2710378854155));
#44890=CARTESIAN_POINT('Ctrl Pts',(-2.36781510497411,73.5888336856356,12.4699536848605));
#44891=CARTESIAN_POINT('Ctrl Pts',(-2.47342243415319,73.5417658505072,12.8800744979288));
#44892=CARTESIAN_POINT('Ctrl Pts',(-2.49994917427196,73.518521429244,13.0893081850669));
#44893=CARTESIAN_POINT('Ctrl Pts',(-2.4999999270496,73.494492116903,13.2993960529866));
#44894=CARTESIAN_POINT('Ctrl Pts',(-2.4999999270496,73.494492116903,13.2993960529867));
#44895=CARTESIAN_POINT('Ctrl Pts',(-2.49999997648352,73.4944687120149,13.2996006815233));
#44896=CARTESIAN_POINT('Ctrl Pts',(-2.49999999999999,73.4944464433691,13.2997953736906));
#44897=CARTESIAN_POINT('Ctrl Pts',(-2.5,73.4944230382101,13.2999999999289));
#44898=CARTESIAN_POINT('Origin',(0.,70.2,13.3));
#44899=CARTESIAN_POINT('',(-2.50070443670409,71.6262534957662,13.2983067811559));
#44900=CARTESIAN_POINT('',(-2.5,72.4321658751541,13.2999999555149));
#44901=CARTESIAN_POINT('',(-2.5,70.2,13.3));
#44902=CARTESIAN_POINT('',(-2.03416539392586,72.5775385913636,11.8488729526678));
#44903=CARTESIAN_POINT('Ctrl Pts',(-2.5,72.4321658707887,13.2999999550827));
#44904=CARTESIAN_POINT('Ctrl Pts',(-2.49999999988434,72.4328037665143,13.2935626169879));
#44905=CARTESIAN_POINT('Ctrl Pts',(-2.49997513620357,72.4334420042849,13.2871241387266));
#44906=CARTESIAN_POINT('Ctrl Pts',(-2.49779794714823,72.4613839629548,13.0053373066117));
#44907=CARTESIAN_POINT('Ctrl Pts',(-2.45019055606489,72.4884964690398,12.7321056106144));
#44908=CARTESIAN_POINT('Ctrl Pts',(-2.28095458285056,72.5360659243848,12.2499098292762));
#44909=CARTESIAN_POINT('Ctrl Pts',(-2.171990881226,72.556756728809,12.0398803308066));
#44910=CARTESIAN_POINT('Ctrl Pts',(-2.03524748958403,72.5780861924427,11.8481847031589));
#44911=CARTESIAN_POINT('Ctrl Pts',(-2.03353780881959,72.5776812861837,11.8479182461381));
#44912=CARTESIAN_POINT('Ctrl Pts',(-2.00233517851855,72.5853459213617,11.8033339758466));
#44913=CARTESIAN_POINT('Ctrl Pts',(-1.96948569089566,72.593167016327,11.7599905332146));
#44914=CARTESIAN_POINT('Ctrl Pts',(-1.93522193281923,72.6010356435396,11.717886377818));
#44915=CARTESIAN_POINT('Ctrl Pts',(-1.91356637909698,72.6060088131185,11.6912754965163));
#44916=CARTESIAN_POINT('Ctrl Pts',(-1.89134540088026,72.6110010933063,11.665158731078));
#44917=CARTESIAN_POINT('Ctrl Pts',(-1.86861172784556,72.6159862597669,11.6395268720491));
#44918=CARTESIAN_POINT('Ctrl Pts',(-1.81493788397145,72.6277561592409,11.5790104567026));
#44919=CARTESIAN_POINT('Ctrl Pts',(-1.75840840698191,72.6394863199071,11.5211937322117));
#44920=CARTESIAN_POINT('Ctrl Pts',(-1.69919068199487,72.6511529581679,11.466250439536));
#44921=CARTESIAN_POINT('Ctrl Pts',(-1.69344502147043,72.6522849257152,11.4609195101922));
#44922=CARTESIAN_POINT('Ctrl Pts',(-1.6876740131914,72.6534162979526,11.4556156325558));
#44923=CARTESIAN_POINT('Ctrl Pts',(-1.68187778389141,72.6545470548966,11.4503389668807));
#44924=CARTESIAN_POINT('Ctrl Pts',(-1.6625817125446,72.6583114274805,11.4327725608484));
#44925=CARTESIAN_POINT('Ctrl Pts',(-1.64300627854001,72.6620688900243,11.4155075965675));
#44926=CARTESIAN_POINT('Ctrl Pts',(-1.62315600409785,72.665818536364,11.3985497211438));
#44927=CARTESIAN_POINT('Ctrl Pts',(-1.62315110236485,72.665819462284,11.3985455336461));
#44928=CARTESIAN_POINT('Ctrl Pts',(-1.62314620061507,72.6658203882035,11.3985413461672));
#44929=CARTESIAN_POINT('Ctrl Pts',(-1.62314129884852,72.6658213141225,11.3985371587071));
#44930=CARTESIAN_POINT('Ctrl Pts',(-1.56082317157978,72.6775928945893,11.3453002953787));
#44931=CARTESIAN_POINT('Ctrl Pts',(-1.4957944859709,72.6892892859298,11.2950882784085));
#44932=CARTESIAN_POINT('Ctrl Pts',(-1.42828733292841,72.7009656441407,11.248104005016));
#44933=CARTESIAN_POINT('Ctrl Pts',(-1.42332600423477,72.7018237791445,11.2446509720673));
#44934=CARTESIAN_POINT('Ctrl Pts',(-1.41835128774641,72.7026818042154,11.2412153962897));
#44935=CARTESIAN_POINT('Ctrl Pts',(-1.41336327554541,72.7035397404235,11.2377973692778));
#44936=CARTESIAN_POINT('Ctrl Pts',(-1.37712182632814,72.7097732559532,11.2129629768617));
#44937=CARTESIAN_POINT('Ctrl Pts',(-1.34017883736149,72.7160017706803,11.1890540941832));
#44938=CARTESIAN_POINT('Ctrl Pts',(-1.30257161362189,72.7222311870257,11.1661042373544));
#44939=CARTESIAN_POINT('Ctrl Pts',(-1.22666037836876,72.7348054385303,11.1197793080582));
#44940=CARTESIAN_POINT('Ctrl Pts',(-1.14844789582755,72.7473182678509,11.0776095001034));
#44941=CARTESIAN_POINT('Ctrl Pts',(-1.06832128165793,72.7597986771855,11.0397427669342));
#44942=CARTESIAN_POINT('Ctrl Pts',(-0.988194667488308,72.77227908652,11.0018760337651));
#44943=CARTESIAN_POINT('Ctrl Pts',(-0.906154741620227,72.7847267457644,
10.9683124889373));
#44944=CARTESIAN_POINT('Ctrl Pts',(-0.822570907356569,72.797146478726,10.9391908917457));
#44945=CARTESIAN_POINT('Ctrl Pts',(-0.822568759051828,72.7971467979429,
10.9391901432509));
#44946=CARTESIAN_POINT('Ctrl Pts',(-0.822566610745908,72.7971471171598,
10.939189394759));
#44947=CARTESIAN_POINT('Ctrl Pts',(-0.822564462439122,72.7971474363766,
10.9391886462701));
#44948=CARTESIAN_POINT('Ctrl Pts',(-0.739122321522642,72.8095461018663,
10.9101166724656));
#44949=CARTESIAN_POINT('Ctrl Pts',(-0.654138804942838,72.8219169139849,
10.8854698603914));
#44950=CARTESIAN_POINT('Ctrl Pts',(-0.567970639269384,72.834291747492,10.8653654129984));
#44951=CARTESIAN_POINT('Ctrl Pts',(-0.500847214011987,72.843931516489,10.8497044161397));
#44952=CARTESIAN_POINT('Ctrl Pts',(-0.433005218202936,72.8535732672548,
10.8368000881515));
#44953=CARTESIAN_POINT('Ctrl Pts',(-0.364614729086927,72.8632238157735,
10.8267114737518));
#44954=CARTESIAN_POINT('Ctrl Pts',(-0.277028957441099,72.8755830012354,
10.8137912696642));
#44955=CARTESIAN_POINT('Ctrl Pts',(-0.18900998836863,72.8878915084906,10.8055572567933));
#44956=CARTESIAN_POINT('Ctrl Pts',(-0.10091689812988,72.9001498719571,10.801991568242));
#44957=CARTESIAN_POINT('Ctrl Pts',(-0.0373380391023907,72.9089970217237,
10.7994181267937));
#44958=CARTESIAN_POINT('Ctrl Pts',(0.0262801750454052,72.9178176922334,
10.799276294681));
#44959=CARTESIAN_POINT('Ctrl Pts',(0.0898160120563695,72.9266083378267,
10.8015639694048));
#44960=CARTESIAN_POINT('Ctrl Pts',(0.0898329310713154,72.9266106786955,
10.8015645785917));
#44961=CARTESIAN_POINT('Ctrl Pts',(0.089849850080472,72.9266130195624,10.8015651879512));
#44962=CARTESIAN_POINT('Ctrl Pts',(0.0898667690838388,72.9266153604271,
10.801565797483));
#44963=CARTESIAN_POINT('Ctrl Pts',(0.173797377113533,72.9382277583191,10.8045895205693));
#44964=CARTESIAN_POINT('Ctrl Pts',(0.257587847717748,72.949789154405,10.8118537130972));
#44965=CARTESIAN_POINT('Ctrl Pts',(0.340913817027985,72.961344531577,10.8233359098749));
#44966=CARTESIAN_POINT('Ctrl Pts',(0.347489815953519,72.9622564699379,10.8242420729151));
#44967=CARTESIAN_POINT('Ctrl Pts',(0.354062906104864,72.9631683688201,10.825174528162));
#44968=CARTESIAN_POINT('Ctrl Pts',(0.360632919580723,72.9640802493081,10.8261332753483));
#44969=CARTESIAN_POINT('Ctrl Pts',(0.450469841210252,72.9765491028715,10.8392429738528));
#44970=CARTESIAN_POINT('Ctrl Pts',(0.539734065831612,72.9890148357778,10.8572646821544));
#44971=CARTESIAN_POINT('Ctrl Pts',(0.627990142466835,73.0015094525903,10.880171520626));
#44972=CARTESIAN_POINT('Ctrl Pts',(0.713329773984111,73.0135911815249,10.9023213966338));
#44973=CARTESIAN_POINT('Ctrl Pts',(0.797276335746133,73.0256362234166,10.9289218151932));
#44974=CARTESIAN_POINT('Ctrl Pts',(0.879477830991702,73.0376544768961,10.9598058078935));
#44975=CARTESIAN_POINT('Ctrl Pts',(0.962586973041719,73.0498054326986,10.9910308133356));
#44976=CARTESIAN_POINT('Ctrl Pts',(1.04391188025697,73.0619286698602,11.0266334838925));
#44977=CARTESIAN_POINT('Ctrl Pts',(1.12311984382727,73.0740196943337,11.0664543810062));
#44978=CARTESIAN_POINT('Ctrl Pts',(1.17162970886691,73.0814246816476,11.0908421604374));
#44979=CARTESIAN_POINT('Ctrl Pts',(1.21934622802924,73.0888173197235,11.1168123983187));
#44980=CARTESIAN_POINT('Ctrl Pts',(1.26619905011251,73.0961947466003,11.144333929718));
#44981=CARTESIAN_POINT('Ctrl Pts',(1.2662122340189,73.096196822533,11.1443416739963));
#44982=CARTESIAN_POINT('Ctrl Pts',(1.26622541785702,73.0961988984646,11.1443494183977));
#44983=CARTESIAN_POINT('Ctrl Pts',(1.26623860162657,73.0962009743949,11.1443571629219));
#44984=CARTESIAN_POINT('Ctrl Pts',(1.33721083186637,73.1073763371073,11.1860482858601));
#44985=CARTESIAN_POINT('Ctrl Pts',(1.40620421057854,73.118517965937,11.2313013178963));
#44986=CARTESIAN_POINT('Ctrl Pts',(1.47294802842284,73.129664939284,11.2799795122737));
#44987=CARTESIAN_POINT('Ctrl Pts',(1.47787170560366,73.1304872491259,11.2835704922715));
#44988=CARTESIAN_POINT('Ctrl Pts',(1.48278311839773,73.1313095863343,11.2871801191278));
#44989=CARTESIAN_POINT('Ctrl Pts',(1.48768214735287,73.1321319657744,11.2908083410286));
#44990=CARTESIAN_POINT('Ctrl Pts',(1.49825461608264,73.1339067217503,11.2986383136501));
#44991=CARTESIAN_POINT('Ctrl Pts',(1.50876946429231,73.1356816487118,11.3065548228557));
#44992=CARTESIAN_POINT('Ctrl Pts',(1.51922552872597,73.1374568675363,11.3145572867525));
#44993=CARTESIAN_POINT('Ctrl Pts',(1.58901016748647,73.1493048247839,11.367966392614));
#44994=CARTESIAN_POINT('Ctrl Pts',(1.6558133367778,73.1611056721388,11.4249265632611));
#44995=CARTESIAN_POINT('Ctrl Pts',(1.71937633086119,73.1728854036747,11.4851486463954));
#44996=CARTESIAN_POINT('Ctrl Pts',(1.78370884880155,73.1848077462468,11.5460998067287));
#44997=CARTESIAN_POINT('Ctrl Pts',(1.84472166146891,73.1967082083627,11.6103916638963));
#44998=CARTESIAN_POINT('Ctrl Pts',(1.90215787333205,73.2085975648045,11.6777304363509));
#44999=CARTESIAN_POINT('Ctrl Pts',(1.95944319604363,73.2204556870329,11.7448923048993));
#45000=CARTESIAN_POINT('Ctrl Pts',(2.01317077029276,73.2323024404982,11.8150840358726));
#45001=CARTESIAN_POINT('Ctrl Pts',(2.06310091360915,73.2441369028791,11.8880333691187));
#45002=CARTESIAN_POINT('Ctrl Pts',(2.08930829682315,73.2503485872474,11.9263230876054));
#45003=CARTESIAN_POINT('Ctrl Pts',(2.11446974771244,73.2565567214177,11.9653729420136));
#45004=CARTESIAN_POINT('Ctrl Pts',(2.13855173663704,73.2627603494946,12.0051473198796));
#45005=CARTESIAN_POINT('Ctrl Pts',(2.13855545002762,73.2627613060806,12.0051534530026));
#45006=CARTESIAN_POINT('Ctrl Pts',(2.13855916339253,73.2627622626665,12.0051595861428));
#45007=CARTESIAN_POINT('Ctrl Pts',(2.13856287673177,73.2627632192523,12.0051657193003));
#45008=CARTESIAN_POINT('Ctrl Pts',(2.14921639855088,73.2655076514524,12.0227616679975));
#45009=CARTESIAN_POINT('Ctrl Pts',(2.15965867181997,73.2682511993657,12.0404994742902));
#45010=CARTESIAN_POINT('Ctrl Pts',(2.16988667557105,73.2709944723947,12.0583756525207));
#45011=CARTESIAN_POINT('Ctrl Pts',(2.21320796727965,73.2826137613602,12.134091222304));
#45012=CARTESIAN_POINT('Ctrl Pts',(2.25246284353253,73.2941696184544,12.2119000238158));
#45013=CARTESIAN_POINT('Ctrl Pts',(2.28753354557419,73.3056990189531,12.2914562562454));
#45014=CARTESIAN_POINT('Ctrl Pts',(2.32315205883524,73.3174085109408,12.3722551725723));
#45015=CARTESIAN_POINT('Ctrl Pts',(2.35445375262732,73.3290905463094,12.4548560009577));
#45016=CARTESIAN_POINT('Ctrl Pts',(2.38131295547122,73.3407678264489,12.5388879834489));
#45017=CARTESIAN_POINT('Ctrl Pts',(2.4082565505562,73.3524817968746,12.6231839963867));
#45018=CARTESIAN_POINT('Ctrl Pts',(2.43072946898995,73.3641907263945,12.7089192493945));
#45019=CARTESIAN_POINT('Ctrl Pts',(2.44861131043191,73.3759047830073,12.7957222680304));
#45020=CARTESIAN_POINT('Ctrl Pts',(2.46205090276032,73.384708806122,12.8609614765945));
#45021=CARTESIAN_POINT('Ctrl Pts',(2.47289742868133,73.3935154323392,12.9268037870214));
#45022=CARTESIAN_POINT('Ctrl Pts',(2.48110148774651,73.4023256647204,12.9930975741823));
#45023=CARTESIAN_POINT('Ctrl Pts',(2.48868454997462,73.410469016671,13.0543733291939));
#45024=CARTESIAN_POINT('Ctrl Pts',(2.4939825627341,73.4185856930003,13.1158109652438));
#45025=CARTESIAN_POINT('Ctrl Pts',(2.49700513073167,73.4266755909545,13.1772949549708));
#45026=CARTESIAN_POINT('Ctrl Pts',(2.49700633378398,73.4266788109219,13.1773194270277));
#45027=CARTESIAN_POINT('Ctrl Pts',(2.49700753647547,73.4266820308852,13.1773438990924));
#45028=CARTESIAN_POINT('Ctrl Pts',(2.49700873880609,73.4266852508442,13.1773683711644));
#45029=CARTESIAN_POINT('Ctrl Pts',(2.50129482405442,73.4381638064985,13.2646067605123));
#45030=CARTESIAN_POINT('Ctrl Pts',(2.50099985775013,73.4495894794228,13.351942076957));
#45031=CARTESIAN_POINT('Ctrl Pts',(2.49614920214244,73.4609924753731,13.4390156985328));
#45032=CARTESIAN_POINT('Ctrl Pts',(2.49123082008854,73.4725546836968,13.5273050706022));
#45033=CARTESIAN_POINT('Ctrl Pts',(2.48162827059325,73.4840933815966,13.615324511331));
#45034=CARTESIAN_POINT('Ctrl Pts',(2.46736827501081,73.4956279218977,13.7026915579614));
#45035=CARTESIAN_POINT('Ctrl Pts',(2.45828319561121,73.5029766068162,13.758353325243));
#45036=CARTESIAN_POINT('Ctrl Pts',(2.44730774964432,73.5103233663213,13.8137501608377));
#45037=CARTESIAN_POINT('Ctrl Pts',(2.43444902403012,73.5176713013572,13.8687838814702));
#45038=CARTESIAN_POINT('Ctrl Pts',(2.43444379905134,73.5176742870967,13.868806243719));
#45039=CARTESIAN_POINT('Ctrl Pts',(2.43443857376157,73.5176772728363,13.8688286059079));
#45040=CARTESIAN_POINT('Ctrl Pts',(2.4344333481608,73.5176802585762,13.8688509680369));
#45041=CARTESIAN_POINT('Ctrl Pts',(2.42629390065555,73.5223308765159,13.9036824415316));
#45042=CARTESIAN_POINT('Ctrl Pts',(2.41740001942849,73.5269819505898,13.9383685490922));
#45043=CARTESIAN_POINT('Ctrl Pts',(2.40775379177636,73.5316350026151,13.97288380081));
#45044=CARTESIAN_POINT('Ctrl Pts',(2.3841740531368,73.5430091640584,14.0572546703289));
#45045=CARTESIAN_POINT('Ctrl Pts',(2.35622043358093,73.5543371678204,14.1401690110613));
#45046=CARTESIAN_POINT('Ctrl Pts',(2.32406085243493,73.5656353612939,14.2212942630802));
#45047=CARTESIAN_POINT('Ctrl Pts',(2.2913907848197,73.5771128971186,14.3037072602124));
#45048=CARTESIAN_POINT('Ctrl Pts',(2.25438096393225,73.5885594153825,14.3842733082134));
#45049=CARTESIAN_POINT('Ctrl Pts',(2.21319922707366,73.5999856891628,14.4626643216925));
#45050=CARTESIAN_POINT('Ctrl Pts',(2.20371695763857,73.6026166371239,14.480714184758));
#45051=CARTESIAN_POINT('Ctrl Pts',(2.19401343862176,73.605246494746,14.4986488374847));
#45052=CARTESIAN_POINT('Ctrl Pts',(2.18409057163531,73.6078753689123,14.5164644639377));
#45053=CARTESIAN_POINT('Ctrl Pts',(2.1840784998516,73.607878567101,14.5164861377533));
#45054=CARTESIAN_POINT('Ctrl Pts',(2.18406642774296,73.6078817652882,14.5165078113925));
#45055=CARTESIAN_POINT('Ctrl Pts',(2.18405435530939,73.607884963474,14.5165294848555));
#45056=CARTESIAN_POINT('Ctrl Pts',(2.14099860687478,73.619291137893,14.5938268385608));
#45057=CARTESIAN_POINT('Ctrl Pts',(2.09381259199541,73.6306795804414,14.6688854275725));
#45058=CARTESIAN_POINT('Ctrl Pts',(2.04266511848951,73.6420734746669,14.7413688003259));
#45059=CARTESIAN_POINT('Ctrl Pts',(2.01737742112873,73.6477067020619,14.7772051274842));
#45060=CARTESIAN_POINT('Ctrl Pts',(1.99112157182045,73.6533411159011,14.8124116242157));
#45061=CARTESIAN_POINT('Ctrl Pts',(1.96391898866646,73.6589787854801,14.8469461788497));
#45062=CARTESIAN_POINT('Ctrl Pts',(1.90940688591095,73.6702762869583,14.9161510473789));
#45063=CARTESIAN_POINT('Ctrl Pts',(1.85137529467586,73.6815288812977,14.9822992683596));
#45064=CARTESIAN_POINT('Ctrl Pts',(1.79010475237028,73.6927498506299,15.0451480084304));
#45065=CARTESIAN_POINT('Ctrl Pts',(1.78185427612238,73.6942608269893,15.0536109992519));
#45066=CARTESIAN_POINT('Ctrl Pts',(1.77354504249908,73.6957712246937,15.0620141917625));
#45067=CARTESIAN_POINT('Ctrl Pts',(1.76517770766173,73.69728107206,15.0703570203222));
#45068=CARTESIAN_POINT('Ctrl Pts',(1.76516281634345,73.6972837591304,15.0703718680267));
#45069=CARTESIAN_POINT('Ctrl Pts',(1.76514792484096,73.6972864461991,15.0703867155399));
#45070=CARTESIAN_POINT('Ctrl Pts',(1.76513303315425,73.697289133266,15.0704015628617));
#45071=CARTESIAN_POINT('Ctrl Pts',(1.7025265980138,73.7085858846769,15.1328214825145));
#45072=CARTESIAN_POINT('Ctrl Pts',(1.63666761921622,73.7198522934615,15.191861541058));
#45073=CARTESIAN_POINT('Ctrl Pts',(1.56784913211618,73.7311046927559,15.2472707152904));
#45074=CARTESIAN_POINT('Ctrl Pts',(1.49913127904375,73.7423406375436,15.3025988640804));
#45075=CARTESIAN_POINT('Ctrl Pts',(1.42746360530328,73.7535623546263,15.3543065322117));
#45076=CARTESIAN_POINT('Ctrl Pts',(1.35312935194537,73.7647828589483,15.4021541708615));
#45077=CARTESIAN_POINT('Ctrl Pts',(1.3098499907358,73.7713157322547,15.4300123269955));
#45078=CARTESIAN_POINT('Ctrl Pts',(1.26566646222046,73.7778481545506,15.4565622280442));
#45079=CARTESIAN_POINT('Ctrl Pts',(1.22063096628485,73.7843827064178,15.4817579816506));
#45080=CARTESIAN_POINT('Ctrl Pts',(1.21708536945061,73.7848971647563,15.4837416166116));
#45081=CARTESIAN_POINT('Ctrl Pts',(1.21353533127665,73.7854115143304,15.4857163878051));
#45082=CARTESIAN_POINT('Ctrl Pts',(1.20998088303043,73.7859257565345,15.4876822852714));
#45083=CARTESIAN_POINT('Ctrl Pts',(1.20995800480846,73.7859290664568,15.4876949387792));
#45084=CARTESIAN_POINT('Ctrl Pts',(1.20993512640368,73.7859323763746,15.487707591919));
#45085=CARTESIAN_POINT('Ctrl Pts',(1.20991224781601,73.7859356862879,15.4877202446908));
#45086=CARTESIAN_POINT('Ctrl Pts',(1.13371903175926,73.796958785634,15.5298581332995));
#45087=CARTESIAN_POINT('Ctrl Pts',(1.05549763345003,73.8079332466301,15.5679199945778));
#45088=CARTESIAN_POINT('Ctrl Pts',(0.975580932636508,73.8188805221497,15.6017912055059));
#45089=CARTESIAN_POINT('Ctrl Pts',(0.894288616358889,73.8300162343958,15.6362454455264));
#45090=CARTESIAN_POINT('Ctrl Pts',(0.81124264483813,73.8411236031648,15.666362331274));
#45091=CARTESIAN_POINT('Ctrl Pts',(0.726813507581337,73.8522184547178,15.6920161130511));
#45092=CARTESIAN_POINT('Ctrl Pts',(0.641886281410767,73.8633787602448,15.7178212390764));
#45093=CARTESIAN_POINT('Ctrl Pts',(0.55556052045207,73.874526150366,15.7391099440483));
#45094=CARTESIAN_POINT('Ctrl Pts',(0.46822177286561,73.8856735115328,15.7557622194446));
#45095=CARTESIAN_POINT('Ctrl Pts',(0.410327112081077,73.8930628170957,15.7668005943011));
#45096=CARTESIAN_POINT('Ctrl Pts',(0.351987503949557,73.9004520504417,15.7758019757087));
#45097=CARTESIAN_POINT('Ctrl Pts',(0.293313731830431,73.9078450103692,15.7827337846194));
#45098=CARTESIAN_POINT('Ctrl Pts',(0.212594966547678,73.9180156637221,15.7922700226392));
#45099=CARTESIAN_POINT('Ctrl Pts',(0.1316293840294,73.9281449406435,15.7978439249359));
#45100=CARTESIAN_POINT('Ctrl Pts',(0.050695235931738,73.938245163729,15.7994858904266));
#45101=CARTESIAN_POINT('Ctrl Pts',(0.0428563290129143,73.9392234245804,
15.7996449236029));
#45102=CARTESIAN_POINT('Ctrl Pts',(0.0350176857552271,73.9402014153011,
15.7997670460444));
#45103=CARTESIAN_POINT('Ctrl Pts',(0.0271795394711455,73.9411791486449,
15.7998522684778));
#45104=CARTESIAN_POINT('Ctrl Pts',(-0.0255788911773204,73.9477602553177,
15.8004258992424));
#45105=CARTESIAN_POINT('Ctrl Pts',(-0.0783141785358755,73.9543296457411,
15.7993291913896));
#45106=CARTESIAN_POINT('Ctrl Pts',(-0.130959639856642,73.9608916989189,
15.796567664907));
#45107=CARTESIAN_POINT('Ctrl Pts',(-0.13098453186807,73.9608948016119,15.7965663591924));
#45108=CARTESIAN_POINT('Ctrl Pts',(-0.131009423859538,73.9608979043032,
15.7965650531051));
#45109=CARTESIAN_POINT('Ctrl Pts',(-0.131034315831042,73.9609010069929,
15.7965637466453));
#45110=CARTESIAN_POINT('Ctrl Pts',(-0.211918936036267,73.9709829677021,
15.7923185018661));
#45111=CARTESIAN_POINT('Ctrl Pts',(-0.292595669761997,73.9810480981651,
15.7841419162165));
#45112=CARTESIAN_POINT('Ctrl Pts',(-0.372786814204804,73.9911084885637,
15.772049757157));
#45113=CARTESIAN_POINT('Ctrl Pts',(-0.383722757406466,73.9924804587326,
15.7704007076818));
#45114=CARTESIAN_POINT('Ctrl Pts',(-0.394649613821351,73.9938523337729,
15.7686787817984));
#45115=CARTESIAN_POINT('Ctrl Pts',(-0.405566624343431,73.9952241377399,
15.76688396919));
#45116=CARTESIAN_POINT('Ctrl Pts',(-0.490543523113661,74.0059021201968,
15.7529133305225));
#45117=CARTESIAN_POINT('Ctrl Pts',(-0.574926649123603,74.0165760349966,
15.7345293361135));
#45118=CARTESIAN_POINT('Ctrl Pts',(-0.658346101382832,74.0272568189175,
15.7117584487786));
#45119=CARTESIAN_POINT('Ctrl Pts',(-0.664252883748156,74.0280131061431,
15.7101460829322));
#45120=CARTESIAN_POINT('Ctrl Pts',(-0.670154819025069,74.0287694265211,
15.708511706861));
#45121=CARTESIAN_POINT('Ctrl Pts',(-0.676051768597265,74.0295257833444,
15.7068553232257));
#45122=CARTESIAN_POINT('Ctrl Pts',(-0.761266198022221,74.0404555893987,
15.682919594309));
#45123=CARTESIAN_POINT('Ctrl Pts',(-0.845001135821688,74.0513368367019,
15.6545158815446));
#45124=CARTESIAN_POINT('Ctrl Pts',(-0.926893964906226,74.0621824056608,
15.6218235710098));
#45125=CARTESIAN_POINT('Ctrl Pts',(-1.0095880665815,74.0731340920568,15.5888113856745));
#45126=CARTESIAN_POINT('Ctrl Pts',(-1.09040311035051,74.0840491747836,15.551427350259));
#45127=CARTESIAN_POINT('Ctrl Pts',(-1.16899335196819,74.0949453898928,15.5098545427027));
#45128=CARTESIAN_POINT('Ctrl Pts',(-1.2413646583252,74.1049793750996,15.4715714387212));
#45129=CARTESIAN_POINT('Ctrl Pts',(-1.31184946361676,74.1149972811528,15.4297368908981));
#45130=CARTESIAN_POINT('Ctrl Pts',(-1.38020314453495,74.1250185438341,15.3844786621361));
#45131=CARTESIAN_POINT('Ctrl Pts',(-1.38570105997187,74.1258245875476,15.3808383912507));
#45132=CARTESIAN_POINT('Ctrl Pts',(-1.39118519146044,74.1266306550172,15.3771759430737));
#45133=CARTESIAN_POINT('Ctrl Pts',(-1.39665541301641,74.1274367574286,15.3734913694022));
#45134=CARTESIAN_POINT('Ctrl Pts',(-1.40873566158579,74.1292169261846,15.3653544840187));
#45135=CARTESIAN_POINT('Ctrl Pts',(-1.42074812250748,74.1309972723805,15.3571097738254));
#45136=CARTESIAN_POINT('Ctrl Pts',(-1.43269150113015,74.1327779285501,15.3487578372105));
#45137=CARTESIAN_POINT('Ctrl Pts',(-1.43270814395231,74.1327804098533,15.3487461989798));
#45138=CARTESIAN_POINT('Ctrl Pts',(-1.4327247866403,74.1327828911572,15.3487345605409));
#45139=CARTESIAN_POINT('Ctrl Pts',(-1.43274142919412,74.1327853724616,15.3487229218937));
#45140=CARTESIAN_POINT('Ctrl Pts',(-1.46975856779551,74.1383044046323,15.3228357039874));
#45141=CARTESIAN_POINT('Ctrl Pts',(-1.5061123792386,74.1438264387456,15.2959182353033));
#45142=CARTESIAN_POINT('Ctrl Pts',(-1.54175964813545,74.1493524052715,15.2679911113879));
#45143=CARTESIAN_POINT('Ctrl Pts',(-1.6106533329589,74.1600321630191,15.2140177627249));
#45144=CARTESIAN_POINT('Ctrl Pts',(-1.67655905716899,74.1706724236108,15.1565460532155));
#45145=CARTESIAN_POINT('Ctrl Pts',(-1.73922926765431,74.181279657172,15.0958498312479));
#45146=CARTESIAN_POINT('Ctrl Pts',(-1.8028790531229,74.1920526884952,15.0342048889847));
#45147=CARTESIAN_POINT('Ctrl Pts',(-1.86319023395297,74.2027913948432,14.9692341759712));
#45148=CARTESIAN_POINT('Ctrl Pts',(-1.91989961078423,74.2135052070296,14.901238251256));
#45149=CARTESIAN_POINT('Ctrl Pts',(-1.97679002714856,74.2242532220879,14.833025255729));
#45150=CARTESIAN_POINT('Ctrl Pts',(-2.03005504931108,74.2349759582558,14.761768665622));
#45151=CARTESIAN_POINT('Ctrl Pts',(-2.07943829573419,74.2456892501053,14.6877755540771));
#45152=CARTESIAN_POINT('Ctrl Pts',(-2.11265888379711,74.2528961852727,14.6379996714415));
#45153=CARTESIAN_POINT('Ctrl Pts',(-2.14412311571905,74.2600989861902,14.5869855056616));
#45154=CARTESIAN_POINT('Ctrl Pts',(-2.17375607155748,74.2673047803565,14.5348235657417));
#45155=CARTESIAN_POINT('Ctrl Pts',(-2.21313294035364,74.2768799848351,14.4655097289588));
#45156=CARTESIAN_POINT('Ctrl Pts',(-2.24909377318838,74.2864160170156,14.3944911231243));
#45157=CARTESIAN_POINT('Ctrl Pts',(-2.28156343766963,74.2959360987337,14.3220077550171));
#45158=CARTESIAN_POINT('Ctrl Pts',(-2.28538296352163,74.2970559809011,14.313481270289));
#45159=CARTESIAN_POINT('Ctrl Pts',(-2.28915416434354,74.2981756461493,14.3049344595523));
#45160=CARTESIAN_POINT('Ctrl Pts',(-2.29287690406189,74.2992951353138,14.2963676683204));
#45161=CARTESIAN_POINT('Ctrl Pts',(-2.29532894250337,74.3000325036698,14.2907250225784));
#45162=CARTESIAN_POINT('Ctrl Pts',(-2.29775996884127,74.3007697977115,14.2850737138729));
#45163=CARTESIAN_POINT('Ctrl Pts',(-2.30016994868297,74.3015070301832,14.2794138407622));
#45164=CARTESIAN_POINT('Ctrl Pts',(-2.30017588511715,74.3015088461868,14.2793998989592));
#45165=CARTESIAN_POINT('Ctrl Pts',(-2.30018182142352,74.30151066219,14.2793859571042));
#45166=CARTESIAN_POINT('Ctrl Pts',(-2.30018775760206,74.3015124781928,14.2793720151971));
#45167=CARTESIAN_POINT('Ctrl Pts',(-2.33233849075179,74.3113480687414,14.2038617303245));
#45168=CARTESIAN_POINT('Ctrl Pts',(-2.36074405274654,74.3211725286144,14.1268246655189));
#45169=CARTESIAN_POINT('Ctrl Pts',(-2.38530971244953,74.3309847983196,14.0485327517548));
#45170=CARTESIAN_POINT('Ctrl Pts',(-2.38694554546875,74.3316381996519,14.0433192749249));
#45171=CARTESIAN_POINT('Ctrl Pts',(-2.38856433300727,74.3322915452213,14.0381002387581));
#45172=CARTESIAN_POINT('Ctrl Pts',(-2.3901660393656,74.3329448339845,14.0328757259305));
#45173=CARTESIAN_POINT('Ctrl Pts',(-2.41620504186434,74.3435653747897,13.9479406179044));
#45174=CARTESIAN_POINT('Ctrl Pts',(-2.43773388193084,74.3541711231403,13.8615570689893));
#45175=CARTESIAN_POINT('Ctrl Pts',(-2.45462226753716,74.3647649634114,13.774103436091));
#45176=CARTESIAN_POINT('Ctrl Pts',(-2.46450513939925,74.3709643461332,13.7229266647905));
#45177=CARTESIAN_POINT('Ctrl Pts',(-2.47279885746805,74.3771597574519,13.6713840314169));
#45178=CARTESIAN_POINT('Ctrl Pts',(-2.47947793825715,74.3833528359836,13.619556771821));
#45179=CARTESIAN_POINT('Ctrl Pts',(-2.49102244893907,74.3940573121714,13.529975529894));
#45180=CARTESIAN_POINT('Ctrl Pts',(-2.49768369321288,74.4046996691395,13.4400022552948));
#45181=CARTESIAN_POINT('Ctrl Pts',(-2.49948904565975,74.4152986643673,13.3500644366634));
#45182=CARTESIAN_POINT('Ctrl Pts',(-2.49982311671675,74.4172599531699,13.3334219122705));
#45183=CARTESIAN_POINT('Ctrl Pts',(-2.49999094463134,74.4192197919804,13.3167805118867));
#45184=CARTESIAN_POINT('Ctrl Pts',(-2.49999273450874,74.4211783466184,13.3001428234969));
#45185=CARTESIAN_POINT('',(2.15550409125805,72.6022418966679,12.0345911582846));
#45186=CARTESIAN_POINT('Ctrl Pts',(-2.5,73.4944230382101,13.2999999999288));
#45187=CARTESIAN_POINT('Ctrl Pts',(-2.50000000000897,73.4583731784959,13.6151761185301));
#45188=CARTESIAN_POINT('Ctrl Pts',(-2.44039283535546,73.4225014456294,13.9276778727858));
#45189=CARTESIAN_POINT('Ctrl Pts',(-2.23465482786394,73.3616757179031,14.446910667989));
#45190=CARTESIAN_POINT('Ctrl Pts',(-2.11265258757116,73.3362988716897,14.6585864733192));
#45191=CARTESIAN_POINT('Ctrl Pts',(-1.75550076090336,73.2733885901009,15.1108832337171));
#45192=CARTESIAN_POINT('Ctrl Pts',(-1.49860366585412,73.2355210576777,15.3286502061438));
#45193=CARTESIAN_POINT('Ctrl Pts',(-0.939078089956608,73.1675993626938,
15.636954284236));
#45194=CARTESIAN_POINT('Ctrl Pts',(-0.647003862542713,73.1376911885021,
15.7340470175276));
#45195=CARTESIAN_POINT('Ctrl Pts',(-0.0128277743704004,73.0709254514597,
15.8223130833006));
#45196=CARTESIAN_POINT('Ctrl Pts',(0.325221648481027,73.0349016869927,15.8013488882042));
#45197=CARTESIAN_POINT('Ctrl Pts',(0.939142011172969,72.9724547021774,15.63627649858));
#45198=CARTESIAN_POINT('Ctrl Pts',(1.21262516272004,72.9457745378757,15.5067371850223));
#45199=CARTESIAN_POINT('Ctrl Pts',(1.72046847219534,72.8845201048941,15.1426523782178));
#45200=CARTESIAN_POINT('Ctrl Pts',(1.945263761033,72.8512055310555,14.9036470538047));
#45201=CARTESIAN_POINT('Ctrl Pts',(2.27198004299956,72.7954271071532,14.3826338374693));
#45202=CARTESIAN_POINT('Ctrl Pts',(2.38199997869102,72.7725349973656,14.1123955096302));
#45203=CARTESIAN_POINT('Ctrl Pts',(2.5119201936499,72.7193307811069,13.5126520122323));
#45204=CARTESIAN_POINT('Ctrl Pts',(2.51837495144558,72.6893801651482,13.1851696111672));
#45205=CARTESIAN_POINT('Ctrl Pts',(2.41016238116982,72.6410772644571,12.5720763393092));
#45206=CARTESIAN_POINT('Ctrl Pts',(2.30646714388487,72.6223614865806,12.2906341890378));
#45207=CARTESIAN_POINT('Ctrl Pts',(2.15571927943544,72.6016597320381,12.0339532440426));
#45208=CARTESIAN_POINT('Ctrl Pts',(2.15445813049926,72.6018264157545,12.0336790882568));
#45209=CARTESIAN_POINT('Ctrl Pts',(2.12210370708062,72.591658948342,11.9780546956726));
#45210=CARTESIAN_POINT('Ctrl Pts',(2.08752077496568,72.5813095705524,11.9238853360025));
#45211=CARTESIAN_POINT('Ctrl Pts',(2.0509269321179,72.5709431692347,11.8712295010138));
#45212=CARTESIAN_POINT('Ctrl Pts',(2.03728749051808,72.5670793518718,11.8516033527242));
#45213=CARTESIAN_POINT('Ctrl Pts',(2.02336834487594,72.5632131129879,11.8321870798604));
#45214=CARTESIAN_POINT('Ctrl Pts',(2.00917947777018,72.5593527877987,11.8129823910257));
#45215=CARTESIAN_POINT('Ctrl Pts',(1.96030681681733,72.5460561403124,11.7468330473801));
#45216=CARTESIAN_POINT('Ctrl Pts',(1.90823764456952,72.5328301919631,11.6831924744939));
#45217=CARTESIAN_POINT('Ctrl Pts',(1.85312925906669,72.5197047773732,11.6223047551265));
#45218=CARTESIAN_POINT('Ctrl Pts',(1.85312527945052,72.51970382953,11.6223003581595));
#45219=CARTESIAN_POINT('Ctrl Pts',(1.85312129981847,72.5197028816872,11.6222959612069));
#45220=CARTESIAN_POINT('Ctrl Pts',(1.85311732017056,72.519701933845,11.6222915642686));
#45221=CARTESIAN_POINT('Ctrl Pts',(1.7942232423232,72.5056749910705,11.5572220828988));
#45222=CARTESIAN_POINT('Ctrl Pts',(1.73185568354955,72.4917632956444,11.4952916200479));
#45223=CARTESIAN_POINT('Ctrl Pts',(1.66629232202317,72.477862964003,11.436689910296));
#45224=CARTESIAN_POINT('Ctrl Pts',(1.61017157037369,72.4659645951316,11.3865281747984));
#45225=CARTESIAN_POINT('Ctrl Pts',(1.55170855157011,72.4540746396689,11.3388064413359));
#45226=CARTESIAN_POINT('Ctrl Pts',(1.49107618687501,72.4421388638591,11.2936704800694));
#45227=CARTESIAN_POINT('Ctrl Pts',(1.47473442913998,72.4389219093886,11.2815053443722));
#45228=CARTESIAN_POINT('Ctrl Pts',(1.45825494632662,72.4357055846102,11.2695429552899));
#45229=CARTESIAN_POINT('Ctrl Pts',(1.44164222522493,72.4324890061798,11.2577849739746));
#45230=CARTESIAN_POINT('Ctrl Pts',(1.44163802710613,72.4324881933341,11.2577820026732));
#45231=CARTESIAN_POINT('Ctrl Pts',(1.44163382897881,72.4324873804884,11.2577790313848));
#45232=CARTESIAN_POINT('Ctrl Pts',(1.44162963084299,72.4324865676427,11.2577760601094));
#45233=CARTESIAN_POINT('Ctrl Pts',(1.37521144133417,72.4196266359719,11.2107678789212));
#45234=CARTESIAN_POINT('Ctrl Pts',(1.30666667510322,72.4067598510506,11.1670299991077));
#45235=CARTESIAN_POINT('Ctrl Pts',(1.23625365020321,72.3939459221504,11.1267718668503));
#45236=CARTESIAN_POINT('Ctrl Pts',(1.22694982289881,72.3922527896405,11.1214524716013));
#45237=CARTESIAN_POINT('Ctrl Pts',(1.21761330386815,72.3905605750161,11.1161938360422));
#45238=CARTESIAN_POINT('Ctrl Pts',(1.2082446220452,72.3888694115082,11.1109964525919));
#45239=CARTESIAN_POINT('Ctrl Pts',(1.14036038558841,72.3766154631266,11.0733368955954));
#45240=CARTESIAN_POINT('Ctrl Pts',(1.07079149767844,72.3644175511415,11.038891524946));
#45241=CARTESIAN_POINT('Ctrl Pts',(0.999720811602757,72.3523496936735,11.0078290960524));
#45242=CARTESIAN_POINT('Ctrl Pts',(0.986751010578721,72.3501474114277,11.0021604646613));
#45243=CARTESIAN_POINT('Ctrl Pts',(0.973731061205759,72.3479494491451,10.9966045351065));
#45244=CARTESIAN_POINT('Ctrl Pts',(0.960661896435918,72.345756241502,10.9911623947048));
#45245=CARTESIAN_POINT('Ctrl Pts',(0.9606449335591,72.3457533948694,10.991155331181));
#45246=CARTESIAN_POINT('Ctrl Pts',(0.960627970599397,72.3457505482448,10.9911482678487));
#45247=CARTESIAN_POINT('Ctrl Pts',(0.960611007556961,72.3457477016284,10.9911412047082));
#45248=CARTESIAN_POINT('Ctrl Pts',(0.886022931418177,72.333230864126,10.9600839185077));
#45249=CARTESIAN_POINT('Ctrl Pts',(0.809832831377722,72.3208701164345,10.9327281948738));
#45250=CARTESIAN_POINT('Ctrl Pts',(0.7323055728732,72.3085740050782,10.9091238268088));
#45251=CARTESIAN_POINT('Ctrl Pts',(0.726075529266496,72.307585897006,10.9072269940665));
#45252=CARTESIAN_POINT('Ctrl Pts',(0.719836858514145,72.3065982083406,10.9053544128214));
#45253=CARTESIAN_POINT('Ctrl Pts',(0.713589702597001,72.3056108926817,10.9035061226376));
#45254=CARTESIAN_POINT('Ctrl Pts',(0.673379385175608,72.2992559566807,10.8916094554244));
#45255=CARTESIAN_POINT('Ctrl Pts',(0.632817383828258,72.2929166400686,10.8807186627525));
#45256=CARTESIAN_POINT('Ctrl Pts',(0.591942311665562,72.2865819985053,10.8708446832849));
#45257=CARTESIAN_POINT('Ctrl Pts',(0.507625532162543,72.2735149493805,10.8504767155837));
#45258=CARTESIAN_POINT('Ctrl Pts',(0.422412951260775,72.2605329770767,10.8345398594402));
#45259=CARTESIAN_POINT('Ctrl Pts',(0.33668559964136,72.2475589406759,10.8230152507945));
#45260=CARTESIAN_POINT('Ctrl Pts',(0.249438792457217,72.2343549488239,10.8112863767608));
#45261=CARTESIAN_POINT('Ctrl Pts',(0.161658859339895,72.2211590214262,10.8041282715558));
#45262=CARTESIAN_POINT('Ctrl Pts',(0.0737499573133302,72.2079216664521,
10.8015392279642));
#45263=CARTESIAN_POINT('Ctrl Pts',(-0.0146879078865501,72.1946046600078,
10.7989346056463));
#45264=CARTESIAN_POINT('Ctrl Pts',(-0.103255890545628,72.1812457512613,
10.8009545224982));
#45265=CARTESIAN_POINT('Ctrl Pts',(-0.191543702703014,72.1678273720905,
10.8076072262273));
#45266=CARTESIAN_POINT('Ctrl Pts',(-0.261945025597524,72.1571274620844,
10.8129121390109));
#45267=CARTESIAN_POINT('Ctrl Pts',(-0.332168127949612,72.1463904176932,
10.8211629270956));
#45268=CARTESIAN_POINT('Ctrl Pts',(-0.402008476277773,72.1356216272196,
10.8323678267623));
#45269=CARTESIAN_POINT('Ctrl Pts',(-0.484673496677335,72.1228753808808,
10.8456302643317));
#45270=CARTESIAN_POINT('Ctrl Pts',(-0.566386256195227,72.1101482039065,
10.8629640088588));
#45271=CARTESIAN_POINT('Ctrl Pts',(-0.646852322776328,72.0974697133191,
10.884271690602));
#45272=CARTESIAN_POINT('Ctrl Pts',(-0.651699454506012,72.0967059837543,
10.8855552271864));
#45273=CARTESIAN_POINT('Ctrl Pts',(-0.656542070174611,72.0959424300872,
10.8868531973606));
#45274=CARTESIAN_POINT('Ctrl Pts',(-0.661380108236213,72.0951790584958,
10.8881655851328));
#45275=CARTESIAN_POINT('Ctrl Pts',(-0.739392118190532,72.0828699051925,
10.9093274707255));
#45276=CARTESIAN_POINT('Ctrl Pts',(-0.816212330200092,72.0706085631986,
10.9342339141927));
#45277=CARTESIAN_POINT('Ctrl Pts',(-0.891603421851303,72.0584372139234,
10.9628214631198));
#45278=CARTESIAN_POINT('Ctrl Pts',(-0.901590736687165,72.0568248338062,
10.9666085531495));
#45279=CARTESIAN_POINT('Ctrl Pts',(-0.911552999715001,72.0552140281018,
10.9704603129576));
#45280=CARTESIAN_POINT('Ctrl Pts',(-0.921489682736567,72.0536048903777,
10.9743766598092));
#45281=CARTESIAN_POINT('Ctrl Pts',(-0.994021229411912,72.0418591953921,
11.0029635326968));
#45282=CARTESIAN_POINT('Ctrl Pts',(-1.06518927731977,72.0302031485049,11.0349870929658));
#45283=CARTESIAN_POINT('Ctrl Pts',(-1.13480147812153,72.0186828733091,11.0704289949137));
#45284=CARTESIAN_POINT('Ctrl Pts',(-1.14228992685233,72.0174435935682,11.0742416148654));
#45285=CARTESIAN_POINT('Ctrl Pts',(-1.14976038127993,72.0162058813937,11.0780938409884));
#45286=CARTESIAN_POINT('Ctrl Pts',(-1.15721260825799,72.0149697915856,11.0819856863963));
#45287=CARTESIAN_POINT('Ctrl Pts',(-1.16161711955472,72.0142392218459,11.0842858950607));
#45288=CARTESIAN_POINT('Ctrl Pts',(-1.16601526471472,72.0135092220089,11.0865999397769));
#45289=CARTESIAN_POINT('Ctrl Pts',(-1.17040699608717,72.0127798043756,11.0889278231301));
#45290=CARTESIAN_POINT('Ctrl Pts',(-1.17045349071948,72.0127720821354,11.0889524680984));
#45291=CARTESIAN_POINT('Ctrl Pts',(-1.17049998463185,72.0127643599604,11.0889771146175));
#45292=CARTESIAN_POINT('Ctrl Pts',(-1.17054647782407,72.0127566378507,11.0890017626873));
#45293=CARTESIAN_POINT('Ctrl Pts',(-1.22414151324484,72.0038549744893,11.1174148294504));
#45294=CARTESIAN_POINT('Ctrl Pts',(-1.27678131669416,71.9950398375616,11.1478881495438));
#45295=CARTESIAN_POINT('Ctrl Pts',(-1.32836841847262,71.9862671759764,11.1803669383502));
#45296=CARTESIAN_POINT('Ctrl Pts',(-1.40093940038355,71.9739260937435,11.2260569948508));
#45297=CARTESIAN_POINT('Ctrl Pts',(-1.47105635823873,71.9617309526274,11.2754813921305));
#45298=CARTESIAN_POINT('Ctrl Pts',(-1.5384767452491,71.9495765345888,11.3283759101635));
#45299=CARTESIAN_POINT('Ctrl Pts',(-1.60737156169563,71.9371563092397,11.3824271886046));
#45300=CARTESIAN_POINT('Ctrl Pts',(-1.67344975408167,71.9247783255427,11.4401030369362));
#45301=CARTESIAN_POINT('Ctrl Pts',(-1.73642125199137,71.9123625028405,11.501119461988));
#45302=CARTESIAN_POINT('Ctrl Pts',(-1.80028155331662,71.899771438545,11.5629970958213));
#45303=CARTESIAN_POINT('Ctrl Pts',(-1.86094577837497,71.8871413296168,11.628310602362));
#45304=CARTESIAN_POINT('Ctrl Pts',(-1.91809433407489,71.8744245247237,11.6967512407477));
#45305=CARTESIAN_POINT('Ctrl Pts',(-1.96392142140589,71.8642269944227,11.7516333821051));
#45306=CARTESIAN_POINT('Ctrl Pts',(-2.00748733228005,71.8539744388831,11.8085259627929));
#45307=CARTESIAN_POINT('Ctrl Pts',(-2.04862610987012,71.8436589813961,11.8672641727492));
#45308=CARTESIAN_POINT('Ctrl Pts',(-2.09986880400616,71.8308099891837,11.940428819421));
#45309=CARTESIAN_POINT('Ctrl Pts',(-2.14707274256881,71.8179306430369,12.0160672188127));
#45310=CARTESIAN_POINT('Ctrl Pts',(-2.19005724799498,71.8050374183289,12.0937883678593));
#45311=CARTESIAN_POINT('Ctrl Pts',(-2.23039136752221,71.7929391782466,12.1667173008402));
#45312=CARTESIAN_POINT('Ctrl Pts',(-2.26701071556132,71.7808290987621,12.2414796872062));
#45313=CARTESIAN_POINT('Ctrl Pts',(-2.29978576562082,71.7687423985122,12.317785146074));
#45314=CARTESIAN_POINT('Ctrl Pts',(-2.3019788303873,71.767933645622,12.3228909449371));
#45315=CARTESIAN_POINT('Ctrl Pts',(-2.30415467623841,71.7671249960947,12.3280036706565));
#45316=CARTESIAN_POINT('Ctrl Pts',(-2.30631326117513,71.7663164599153,12.3331232439072));
#45317=CARTESIAN_POINT('Ctrl Pts',(-2.33713893790816,71.7547701573039,12.4062333204906));
#45318=CARTESIAN_POINT('Ctrl Pts',(-2.36444692199442,71.7432476571416,12.4807358856692));
#45319=CARTESIAN_POINT('Ctrl Pts',(-2.38813010461055,71.7317930452142,12.5564168134418));
#45320=CARTESIAN_POINT('Ctrl Pts',(-2.3903252254031,71.7307313527373,12.5634314440701));
#45321=CARTESIAN_POINT('Ctrl Pts',(-2.3924891886415,71.7296702404246,12.5704562304934));
#45322=CARTESIAN_POINT('Ctrl Pts',(-2.39462189759618,71.728609741501,12.5774910220215));
#45323=CARTESIAN_POINT('Ctrl Pts',(-2.41449867855878,71.7187259245978,12.6430550597279));
#45324=CARTESIAN_POINT('Ctrl Pts',(-2.43166303877302,71.7088961288796,12.7094857594791));
#45325=CARTESIAN_POINT('Ctrl Pts',(-2.44603814558137,71.6991533694695,12.776672391503));
#45326=CARTESIAN_POINT('Ctrl Pts',(-2.44771547507019,71.698016555818,12.7845119241514));
#45327=CARTESIAN_POINT('Ctrl Pts',(-2.44935385450317,71.6968815805346,12.7923572810489));
#45328=CARTESIAN_POINT('Ctrl Pts',(-2.45095344119494,71.6957483748995,12.800209101295));
#45329=CARTESIAN_POINT('Ctrl Pts',(-2.45096445588852,71.6957405716882,12.8002631686329));
#45330=CARTESIAN_POINT('Ctrl Pts',(-2.45097546874151,71.6957327685606,12.8003172362761));
#45331=CARTESIAN_POINT('Ctrl Pts',(-2.4509864797539,71.6957249655165,12.8003713042251));
#45332=CARTESIAN_POINT('Ctrl Pts',(-2.4665313781018,71.6847089460218,12.8767022300982));
#45333=CARTESIAN_POINT('Ctrl Pts',(-2.47841178654089,71.6738590388587,12.9536438912108));
#45334=CARTESIAN_POINT('Ctrl Pts',(-2.48665911936036,71.6630936615033,13.0309612316457));
#45335=CARTESIAN_POINT('Ctrl Pts',(-2.48753921184129,71.661944862507,13.0392119487504));
#45336=CARTESIAN_POINT('Ctrl Pts',(-2.48837788944345,71.6607970308485,13.0474669218202));
#45337=CARTESIAN_POINT('Ctrl Pts',(-2.48917516051926,71.6596500707978,13.055725848435));
#45338=CARTESIAN_POINT('Ctrl Pts',(-2.49695389712681,71.6484595229351,13.1363057374423));
#45339=CARTESIAN_POINT('Ctrl Pts',(-2.50079429925675,71.6373514085253,13.2172645178092));
#45340=CARTESIAN_POINT('Ctrl Pts',(-2.50070443670409,71.6262534957662,13.2983067811559));
#45341=CARTESIAN_POINT('Origin',(0.,70.2,13.3));
#45342=CARTESIAN_POINT('',(-2.5,69.6117391960828,13.3));
#45343=CARTESIAN_POINT('',(-2.5,70.6202795746371,13.2999999999956));
#45344=CARTESIAN_POINT('',(-2.5,70.2,13.3));
#45345=CARTESIAN_POINT('Ctrl Pts',(-2.5,70.6202795746371,13.2999999999913));
#45346=CARTESIAN_POINT('Ctrl Pts',(-2.49999999999947,70.6394456460639,13.1486673749071));
#45347=CARTESIAN_POINT('Ctrl Pts',(-2.48625904090408,70.6585193331841,12.9976404384911));
#45348=CARTESIAN_POINT('Ctrl Pts',(-2.43277840039442,70.6958945847908,12.7061947707861));
#45349=CARTESIAN_POINT('Ctrl Pts',(-2.39426039670762,70.7141226191345,12.5661508897012));
#45350=CARTESIAN_POINT('Ctrl Pts',(-2.23708478719293,70.7709350702978,12.1425981655169));
#45351=CARTESIAN_POINT('Ctrl Pts',(-2.07829814092921,70.8090280780769,11.8770361458128));
#45352=CARTESIAN_POINT('Ctrl Pts',(-1.77069185889503,70.8670676595898,11.5280733342784));
#45353=CARTESIAN_POINT('Ctrl Pts',(-1.6549314539226,70.8867415846239,11.4195003937804));
#45354=CARTESIAN_POINT('Ctrl Pts',(-1.26525622213921,70.9479573936792,11.118054283164));
#45355=CARTESIAN_POINT('Ctrl Pts',(-0.962448457501469,70.9889095280149,
10.9685860005634));
#45356=CARTESIAN_POINT('Ctrl Pts',(-0.486186479102335,71.0494139724573,
10.8426287696168));
#45357=CARTESIAN_POINT('Ctrl Pts',(-0.329670559905892,71.0687462970969,
10.8167820739238));
#45358=CARTESIAN_POINT('Ctrl Pts',(0.161889237777242,71.128988982311,10.7829299228129));
#45359=CARTESIAN_POINT('Ctrl Pts',(0.496807426143598,71.1695298547018,10.8271342670815));
#45360=CARTESIAN_POINT('Ctrl Pts',(1.1014511275559,71.2469243672991,11.0350979139091));
#45361=CARTESIAN_POINT('Ctrl Pts',(1.36924285129701,71.2830941470646,11.1861958203389));
#45362=CARTESIAN_POINT('Ctrl Pts',(1.72990593570642,71.3395640352817,11.4876309496461));
#45363=CARTESIAN_POINT('Ctrl Pts',(1.84578861765027,71.3593803596938,11.6057968048365));
#45364=CARTESIAN_POINT('Ctrl Pts',(2.15902370342132,71.4191843054308,11.9958066083007));
#45365=CARTESIAN_POINT('Ctrl Pts',(2.31422879170653,71.4581444197495,12.2966570788982));
#45366=CARTESIAN_POINT('Ctrl Pts',(2.44806458548582,71.5158413414613,12.769531453346));
#45367=CARTESIAN_POINT('Ctrl Pts',(2.47642740497632,71.5342550132755,12.9235405313664));
#45368=CARTESIAN_POINT('Ctrl Pts',(2.51941730600979,71.5915723186385,13.4083478783766));
#45369=CARTESIAN_POINT('Ctrl Pts',(2.48305857205729,71.6295278341907,13.7401103735801));
#45370=CARTESIAN_POINT('Ctrl Pts',(2.28238998188811,71.7056552055624,14.3733326516439));
#45371=CARTESIAN_POINT('Ctrl Pts',(2.1189046935722,71.7440471228116,14.6680650732052));
#45372=CARTESIAN_POINT('Ctrl Pts',(1.71002515174723,71.8159518735498,15.1476277313869));
#45373=CARTESIAN_POINT('Ctrl Pts',(1.47903131089068,71.8486182465415,15.3372565262688));
#45374=CARTESIAN_POINT('Ctrl Pts',(0.928478468424501,71.9190597988017,15.6451304526573));
#45375=CARTESIAN_POINT('Ctrl Pts',(0.606958837930968,71.9567847148786,15.7481355386928));
#45376=CARTESIAN_POINT('Ctrl Pts',(-0.0378388720561457,72.0279255245038,
15.8194089948512));
#45377=CARTESIAN_POINT('Ctrl Pts',(-0.354076081769428,72.0610798581294,
15.7946931162187));
#45378=CARTESIAN_POINT('Ctrl Pts',(-0.813266661607912,72.1130629684333,
15.6695326377008));
#45379=CARTESIAN_POINT('Ctrl Pts',(-0.964634150853069,72.1306784652811,
15.6120511075016));
#45380=CARTESIAN_POINT('Ctrl Pts',(-1.37312510352448,72.1796227011478,15.4097695389725));
#45381=CARTESIAN_POINT('Ctrl Pts',(-1.61173468465016,72.2096798993154,15.2336373042292));
#45382=CARTESIAN_POINT('Ctrl Pts',(-2.04379044445544,72.2747064014632,14.7779134858905));
#45383=CARTESIAN_POINT('Ctrl Pts',(-2.22259154982646,72.310090929242,14.4922558729459));
#45384=CARTESIAN_POINT('Ctrl Pts',(-2.44582943646689,72.3739624854953,13.8985393364112));
#45385=CARTESIAN_POINT('Ctrl Pts',(-2.50000000539873,72.402390189325,13.6004818691382));
#45386=CARTESIAN_POINT('Ctrl Pts',(-2.5,72.4321658707887,13.2999999550827));
#45387=CARTESIAN_POINT('Ctrl Pts',(-2.49999938929793,71.6258524055026,13.2982525704591));
#45388=CARTESIAN_POINT('Ctrl Pts',(-2.50013773453631,71.5989545908592,13.4961792984747));
#45389=CARTESIAN_POINT('Ctrl Pts',(-2.47677199854322,71.5721754987909,13.6933916855558));
#45390=CARTESIAN_POINT('Ctrl Pts',(-2.39349175089188,71.5230701261886,14.0389321059686));
#45391=CARTESIAN_POINT('Ctrl Pts',(-2.34218548439843,71.5010839175006,14.1882422837462));
#45392=CARTESIAN_POINT('Ctrl Pts',(-2.17431598654963,71.4439554442844,14.5587640397383));
#45393=CARTESIAN_POINT('Ctrl Pts',(-2.03801120145824,71.4089634905474,14.7692753447635));
#45394=CARTESIAN_POINT('Ctrl Pts',(-1.65111115326409,71.3302018808504,15.2067576317367));
#45395=CARTESIAN_POINT('Ctrl Pts',(-1.38144107517593,71.2870343870214,15.4103504312543));
#45396=CARTESIAN_POINT('Ctrl Pts',(-0.801244258773137,71.2005757838904,
15.6881556512127));
#45397=CARTESIAN_POINT('Ctrl Pts',(-0.500572500224744,71.1584637136106,
15.7687414164191));
#45398=CARTESIAN_POINT('Ctrl Pts',(0.096429653907802,71.0778933685252,15.8149329684114));
#45399=CARTESIAN_POINT('Ctrl Pts',(0.387429532898798,71.0407407905083,15.7867968746636));
#45400=CARTESIAN_POINT('Ctrl Pts',(0.966568824290719,70.9627806760956,15.6264248990345));
#45401=CARTESIAN_POINT('Ctrl Pts',(1.24784204597565,70.9223411990915,15.4884539371541));
#45402=CARTESIAN_POINT('Ctrl Pts',(1.70024609970173,70.8475039101213,15.1503512405443));
#45403=CARTESIAN_POINT('Ctrl Pts',(1.879538234941,70.8139614360242,14.9679420148664));
#45404=CARTESIAN_POINT('Ctrl Pts',(2.22344387612902,70.737775010458,14.4907052154775));
#45405=CARTESIAN_POINT('Ctrl Pts',(2.3624270599191,70.6956188391405,14.183427827997));
#45406=CARTESIAN_POINT('Ctrl Pts',(2.50678602477161,70.6122113201419,13.5528840412773));
#45407=CARTESIAN_POINT('Ctrl Pts',(2.51873350559229,70.5718831580062,13.2374213908898));
#45408=CARTESIAN_POINT('Ctrl Pts',(2.42603921610482,70.4918509984893,12.6214768694168));
#45409=CARTESIAN_POINT('Ctrl Pts',(2.32331680181175,70.4530237610246,12.3261872834063));
#45410=CARTESIAN_POINT('Ctrl Pts',(2.08831773288123,70.3934112066731,11.9160204105586));
#45411=CARTESIAN_POINT('Ctrl Pts',(1.99384698139257,70.3729742695969,11.7830796893343));
#45412=CARTESIAN_POINT('Ctrl Pts',(1.66783097605583,70.3104879002622,11.4078770028622));
#45413=CARTESIAN_POINT('Ctrl Pts',(1.40010146279125,70.2690377384254,11.2020174536021));
#45414=CARTESIAN_POINT('Ctrl Pts',(0.957195817800658,70.2075114976101,10.9850495059801));
#45415=CARTESIAN_POINT('Ctrl Pts',(0.80824430601015,70.1877820793355,10.9289319082503));
#45416=CARTESIAN_POINT('Ctrl Pts',(0.332182962529846,70.1264957089557,10.7996944176321));
#45417=CARTESIAN_POINT('Ctrl Pts',(-0.00496502799410541,70.0855435982572,
10.7777216544529));
#45418=CARTESIAN_POINT('Ctrl Pts',(-0.631510731345653,70.007928039846,10.862817631781));
#45419=CARTESIAN_POINT('Ctrl Pts',(-0.917058190577315,69.9718426761726,
10.9552867834349));
#45420=CARTESIAN_POINT('Ctrl Pts',(-1.44432109297885,69.8988027482903,11.2374585300552));
#45421=CARTESIAN_POINT('Ctrl Pts',(-1.68138955700855,69.8626524387002,11.4256709683559));
#45422=CARTESIAN_POINT('Ctrl Pts',(-1.98219270859602,69.8077940472495,11.7685943223874));
#45423=CARTESIAN_POINT('Ctrl Pts',(-2.07378868692379,69.7891618773236,11.8951181545654));
#45424=CARTESIAN_POINT('Ctrl Pts',(-2.32283199014498,69.7303498246778,12.3170990858516));
#45425=CARTESIAN_POINT('Ctrl Pts',(-2.43327812336977,69.690515908006,12.6360336866484));
#45426=CARTESIAN_POINT('Ctrl Pts',(-2.49260078235443,69.6378455207597,13.0777903161134));
#45427=CARTESIAN_POINT('Ctrl Pts',(-2.5,69.6247727051849,13.1889492361916));
#45428=CARTESIAN_POINT('Ctrl Pts',(-2.5,69.6117391960828,13.3));
#45429=CARTESIAN_POINT('Origin',(0.,70.2,13.3));
#45430=CARTESIAN_POINT('',(-2.5,67.7617877809656,13.3000000230487));
#45431=CARTESIAN_POINT('',(-2.49999999984276,68.4536941147331,13.3000280391888));
#45432=CARTESIAN_POINT('',(-2.5,70.2,13.3));
#45433=CARTESIAN_POINT('',(-2.46701393303641,68.4808270900767,12.9018894245279));
#45434=CARTESIAN_POINT('Ctrl Pts',(-2.5,68.4536960240567,13.3));
#45435=CARTESIAN_POINT('Ctrl Pts',(-2.49999999999523,68.4582353924442,13.2333373963885));
#45436=CARTESIAN_POINT('Ctrl Pts',(-2.49733364133762,68.4627032333579,13.1666999747746));
#45437=CARTESIAN_POINT('Ctrl Pts',(-2.48667961645755,68.471683031839,13.0337855110735));
#45438=CARTESIAN_POINT('Ctrl Pts',(-2.47869585369853,68.4761914296149,12.967568059918));
#45439=CARTESIAN_POINT('Ctrl Pts',(-2.46807636330827,68.4808334773074,12.9017550190159));
#45440=CARTESIAN_POINT('',(-2.50001628522818,70.6201479917331,13.3010276898172));
#45441=CARTESIAN_POINT('Ctrl Pts',(-2.46710028502621,68.4807253128341,12.9017689911365));
#45442=CARTESIAN_POINT('Ctrl Pts',(-2.45701642861137,68.4909143573078,12.8376991620988));
#45443=CARTESIAN_POINT('Ctrl Pts',(-2.44427557470376,68.5012897672622,12.7741791907651));
#45444=CARTESIAN_POINT('Ctrl Pts',(-2.42907716009975,68.5116874000612,12.7113448092636));
#45445=CARTESIAN_POINT('Ctrl Pts',(-2.42367255572964,68.5153848312162,12.6890007041905));
#45446=CARTESIAN_POINT('Ctrl Pts',(-2.41795702470293,68.51908512482,12.6667428443687));
#45447=CARTESIAN_POINT('Ctrl Pts',(-2.41193893499027,68.5227810738497,12.644575871674));
#45448=CARTESIAN_POINT('Ctrl Pts',(-2.39162414618716,68.5352571962656,12.5697485775994));
#45449=CARTESIAN_POINT('Ctrl Pts',(-2.36786463113725,68.5476833482295,12.4959563733787));
#45450=CARTESIAN_POINT('Ctrl Pts',(-2.34072701070115,68.560051885539,12.4234391530385));
#45451=CARTESIAN_POINT('Ctrl Pts',(-2.34072148492479,68.560054404027,12.4234243870444));
#45452=CARTESIAN_POINT('Ctrl Pts',(-2.34071595900827,68.5600569225126,12.4234096211033));
#45453=CARTESIAN_POINT('Ctrl Pts',(-2.34071043295155,68.5600594409959,12.4233948552149));
#45454=CARTESIAN_POINT('Ctrl Pts',(-2.32462243553839,68.5673914959409,12.3804069552124));
#45455=CARTESIAN_POINT('Ctrl Pts',(-2.307346956239,68.5747029330603,12.3378665568768));
#45456=CARTESIAN_POINT('Ctrl Pts',(-2.28890451365498,68.5820029565785,12.295811501126));
#45457=CARTESIAN_POINT('Ctrl Pts',(-2.28889840876518,68.582005373061,12.2957975798962));
#45458=CARTESIAN_POINT('Ctrl Pts',(-2.28889230374749,68.5820077895422,12.2957836587196));
#45459=CARTESIAN_POINT('Ctrl Pts',(-2.28888619860188,68.5820102060222,12.2957697375963));
#45460=CARTESIAN_POINT('Ctrl Pts',(-2.27045717205942,68.5893046058984,12.2537473570202));
#45461=CARTESIAN_POINT('Ctrl Pts',(-2.25086289904019,68.5965877603358,12.2122098379469));
#45462=CARTESIAN_POINT('Ctrl Pts',(-2.23012083470916,68.6038595070499,12.1712137759273));
#45463=CARTESIAN_POINT('Ctrl Pts',(-2.23011422780498,68.6038618232964,12.1712007175813));
#45464=CARTESIAN_POINT('Ctrl Pts',(-2.23010762078434,68.6038641395417,12.1711876592902));
#45465=CARTESIAN_POINT('Ctrl Pts',(-2.23010101364719,68.6038664557859,12.1711746010541));
#45466=CARTESIAN_POINT('Ctrl Pts',(-2.19557652710775,68.6159696010891,12.102940979198));
#45467=CARTESIAN_POINT('Ctrl Pts',(-2.15787300844718,68.6280416842535,12.03620611478));
#45468=CARTESIAN_POINT('Ctrl Pts',(-2.11708179466995,68.6401060351926,11.9711914617286));
#45469=CARTESIAN_POINT('Ctrl Pts',(-2.10897264785992,68.642504384834,11.9582667821818));
#45470=CARTESIAN_POINT('Ctrl Pts',(-2.10074880264077,68.6449002213517,11.9454218985461));
#45471=CARTESIAN_POINT('Ctrl Pts',(-2.09241156316031,68.647293665484,11.9326581893751));
#45472=CARTESIAN_POINT('Ctrl Pts',(-2.09240410168288,68.6472958075155,11.9326467663941));
#45473=CARTESIAN_POINT('Ctrl Pts',(-2.09239664011459,68.647297949545,11.9326353434781));
#45474=CARTESIAN_POINT('Ctrl Pts',(-2.09238917845551,68.6473000915727,11.9326239206272));
#45475=CARTESIAN_POINT('Ctrl Pts',(-2.04472018782476,68.66098448729,11.859648759465));
#45476=CARTESIAN_POINT('Ctrl Pts',(-1.99334689902953,68.6745928541095,11.7893274485888));
#45477=CARTESIAN_POINT('Ctrl Pts',(-1.93851690543501,68.6881428727038,11.7219296825362));
#45478=CARTESIAN_POINT('Ctrl Pts',(-1.88304016296446,68.7018527209591,11.6537369240611));
#45479=CARTESIAN_POINT('Ctrl Pts',(-1.8240249662701,68.7155026501715,11.588536853598));
#45480=CARTESIAN_POINT('Ctrl Pts',(-1.7616944179658,68.7290851141273,11.5266064023743));
#45481=CARTESIAN_POINT('Ctrl Pts',(-1.75540230636181,68.7304562295978,11.5203546795612));
#45482=CARTESIAN_POINT('Ctrl Pts',(-1.74907637980759,68.7318266376466,11.5141362757948));
#45483=CARTESIAN_POINT('Ctrl Pts',(-1.74271684702026,68.733196317435,11.5079514767474));
#45484=CARTESIAN_POINT('Ctrl Pts',(-1.74270984886747,68.7331978246571,11.507944670875));
#45485=CARTESIAN_POINT('Ctrl Pts',(-1.74270285067398,68.7331993318784,11.5079378650433));
#45486=CARTESIAN_POINT('Ctrl Pts',(-1.7426958524398,68.7332008390987,11.5079310592522));
#45487=CARTESIAN_POINT('Ctrl Pts',(-1.67973330998321,68.7467611777024,11.4466999122221));
#45488=CARTESIAN_POINT('Ctrl Pts',(-1.61347719936441,68.7602523735259,11.3887599843362));
#45489=CARTESIAN_POINT('Ctrl Pts',(-1.54421130510449,68.773735668214,11.3343593984148));
#45490=CARTESIAN_POINT('Ctrl Pts',(-1.5076110920206,68.7808602634268,11.3056140388423));
#45491=CARTESIAN_POINT('Ctrl Pts',(-1.47017041061827,68.7879822034691,11.2778573990232));
#45492=CARTESIAN_POINT('Ctrl Pts',(-1.43193068565022,68.7951074030585,11.2511291391457));
#45493=CARTESIAN_POINT('Ctrl Pts',(-1.36025064822009,68.8084635287549,11.2010272445827));
#45494=CARTESIAN_POINT('Ctrl Pts',(-1.28613928825395,68.8217632664951,11.1548007140498));
#45495=CARTESIAN_POINT('Ctrl Pts',(-1.209937200357,68.8350248467504,11.1126014272649));
#45496=CARTESIAN_POINT('Ctrl Pts',(-1.13286004751762,68.8484387160607,11.0699175459304));
#45497=CARTESIAN_POINT('Ctrl Pts',(-1.05364415253597,68.8618133437034,11.0313536919916));
#45498=CARTESIAN_POINT('Ctrl Pts',(-0.97261117779691,68.875141448303,10.997073095939));
#45499=CARTESIAN_POINT('Ctrl Pts',(-0.919400315590347,68.8838934401879,
10.9745625059134));
#45500=CARTESIAN_POINT('Ctrl Pts',(-0.865405294095551,68.8926248332336,
10.9538989316396));
#45501=CARTESIAN_POINT('Ctrl Pts',(-0.810709125003197,68.9013283155877,
10.9351313915851));
#45502=CARTESIAN_POINT('Ctrl Pts',(-0.810708110977433,68.9013284769437,
10.935131043649));
#45503=CARTESIAN_POINT('Ctrl Pts',(-0.810707096951468,68.9013286382997,
10.9351306957136));
#45504=CARTESIAN_POINT('Ctrl Pts',(-0.810706082925222,68.9013287996557,
10.9351303477789));
#45505=CARTESIAN_POINT('Ctrl Pts',(-0.727629192316671,68.914548332826,10.9066248360828));
#45506=CARTESIAN_POINT('Ctrl Pts',(-0.642932326791323,68.9277049444459,
10.8824915327675));
#45507=CARTESIAN_POINT('Ctrl Pts',(-0.556971403557444,68.9408617620192,
10.8628491960142));
#45508=CARTESIAN_POINT('Ctrl Pts',(-0.544950324965995,68.9427016577777,
10.8601023423865));
#45509=CARTESIAN_POINT('Ctrl Pts',(-0.532904548884078,68.9445415150838,
10.8574433604609));
#45510=CARTESIAN_POINT('Ctrl Pts',(-0.520835071435796,68.9463814646041,
10.8548726168578));
#45511=CARTESIAN_POINT('Ctrl Pts',(-0.435403739039851,68.9594051716974,
10.8366761330245));
#45512=CARTESIAN_POINT('Ctrl Pts',(-0.349231485807851,68.9723675199397,
10.8229937466344));
#45513=CARTESIAN_POINT('Ctrl Pts',(-0.262694614641421,68.985299723341,10.8138246267049));
#45514=CARTESIAN_POINT('Ctrl Pts',(-0.173047108075527,68.9986967848907,
10.8043259156006));
#45515=CARTESIAN_POINT('Ctrl Pts',(-0.0830086539429363,69.0120614483157,
10.7996706163981));
#45516=CARTESIAN_POINT('Ctrl Pts',(0.00702312402538797,69.0253990666962,
10.7998740880398));
#45517=CARTESIAN_POINT('Ctrl Pts',(0.097054901993754,69.0387366850766,10.8000775596816));
#45518=CARTESIAN_POINT('Ctrl Pts',(0.187079837545918,69.0520469299655,10.8051391620622));
#45519=CARTESIAN_POINT('Ctrl Pts',(0.276724728185427,69.0653094366795,10.8150960485874));
#45520=CARTESIAN_POINT('Ctrl Pts',(0.276735596481498,69.0653110445888,10.8150972557325));
#45521=CARTESIAN_POINT('Ctrl Pts',(0.276746464771963,69.0653126524973,10.8150984629496));
#45522=CARTESIAN_POINT('Ctrl Pts',(0.276757333056906,69.0653142604051,10.8150996702387));
#45523=CARTESIAN_POINT('Ctrl Pts',(0.342204847938776,69.0749968894875,10.8223698212616));
#45524=CARTESIAN_POINT('Ctrl Pts',(0.407451436589961,69.0846537569479,10.8322500112889));
#45525=CARTESIAN_POINT('Ctrl Pts',(0.47233765325959,69.0943076633307,10.8447312387675));
#45526=CARTESIAN_POINT('Ctrl Pts',(0.557893594534456,69.1070368543661,10.8611884036326));
#45527=CARTESIAN_POINT('Ctrl Pts',(0.642377866330353,69.1196957004163,10.8820813114099));
#45528=CARTESIAN_POINT('Ctrl Pts',(0.725447266460774,69.1323140128587,10.9072645398335));
#45529=CARTESIAN_POINT('Ctrl Pts',(0.755066709573133,69.1368132314275,10.9162439377888));
#45530=CARTESIAN_POINT('Ctrl Pts',(0.784506363236137,69.1413070512098,10.925768961271));
#45531=CARTESIAN_POINT('Ctrl Pts',(0.813751012452173,69.145796031994,10.9358335828332));
#45532=CARTESIAN_POINT('Ctrl Pts',(0.813763275507918,69.1457979143425,10.9358378031955));
#45533=CARTESIAN_POINT('Ctrl Pts',(0.813775538529388,69.1457997966902,10.9358420236528));
#45534=CARTESIAN_POINT('Ctrl Pts',(0.813787801516542,69.1458016790371,10.935846244205));
#45535=CARTESIAN_POINT('Ctrl Pts',(0.900662829668634,69.1591368425563,10.9657460220978));
#45536=CARTESIAN_POINT('Ctrl Pts',(0.985816994502783,69.1724314404545,11.0004058925232));
#45537=CARTESIAN_POINT('Ctrl Pts',(1.06886499221508,69.1857090128889,11.0396648636248));
#45538=CARTESIAN_POINT('Ctrl Pts',(1.14754780382579,69.1982886868039,11.0768602965348));
#45539=CARTESIAN_POINT('Ctrl Pts',(1.22433976169283,69.2108528675956,11.1181841656645));
#45540=CARTESIAN_POINT('Ctrl Pts',(1.29891555615958,69.2233983758659,11.1635197194307));
#45541=CARTESIAN_POINT('Ctrl Pts',(1.30306400294486,69.224096248062,11.1660416118708));
#45542=CARTESIAN_POINT('Ctrl Pts',(1.3072055878291,69.2247940628451,11.1685759307943));
#45543=CARTESIAN_POINT('Ctrl Pts',(1.31134025317747,69.2254918197984,11.171122660597));
#45544=CARTESIAN_POINT('Ctrl Pts',(1.31135422434589,69.2254941775418,11.1711312660796));
#45545=CARTESIAN_POINT('Ctrl Pts',(1.31136819543531,69.2254965352845,11.1711398717039));
#45546=CARTESIAN_POINT('Ctrl Pts',(1.31138216644577,69.2254988930264,11.1711484774698));
#45547=CARTESIAN_POINT('Ctrl Pts',(1.33813162952027,69.23001312133,11.187625425764));
#45548=CARTESIAN_POINT('Ctrl Pts',(1.36459173541892,69.2345246994819,11.2046215361119));
#45549=CARTESIAN_POINT('Ctrl Pts',(1.39074802582465,69.239038624908,11.2221279654452));
#45550=CARTESIAN_POINT('Ctrl Pts',(1.40280709560774,69.2411197205398,11.2301991119919));
#45551=CARTESIAN_POINT('Ctrl Pts',(1.41479117008784,69.2431995200094,11.2383717723792));
#45552=CARTESIAN_POINT('Ctrl Pts',(1.42669913149396,69.245278482405,11.2466445228467));
#45553=CARTESIAN_POINT('Ctrl Pts',(1.42671293625134,69.2452808925213,11.2466541133475));
#45554=CARTESIAN_POINT('Ctrl Pts',(1.42672674090642,69.2452833026364,11.2466637039829));
#45555=CARTESIAN_POINT('Ctrl Pts',(1.42674054545918,69.2452857127505,11.2466732947528));
#45556=CARTESIAN_POINT('Ctrl Pts',(1.46452159863263,69.2518818444896,11.2729218371295));
#45557=CARTESIAN_POINT('Ctrl Pts',(1.50153584351307,69.2584697485006,11.3001776947919));
#45558=CARTESIAN_POINT('Ctrl Pts',(1.53772885816469,69.265029912732,11.3284086227869));
#45559=CARTESIAN_POINT('Ctrl Pts',(1.53774268781877,69.2650324194257,11.328419410061));
#45560=CARTESIAN_POINT('Ctrl Pts',(1.53775651735298,69.2650349261154,11.3284301974775));
#45561=CARTESIAN_POINT('Ctrl Pts',(1.53777034676736,69.265037432801,11.3284409850364));
#45562=CARTESIAN_POINT('Ctrl Pts',(1.59857550653995,69.2760588262814,11.3758717167935));
#45563=CARTESIAN_POINT('Ctrl Pts',(1.65706798729583,69.2870021977314,11.4260555927558));
#45564=CARTESIAN_POINT('Ctrl Pts',(1.71313960617886,69.2979608857032,11.4788041681358));
#45565=CARTESIAN_POINT('Ctrl Pts',(1.71915879412077,69.2991372812455,11.4844666333046));
#45566=CARTESIAN_POINT('Ctrl Pts',(1.72515003590684,69.3003138478121,11.4901586519967));
#45567=CARTESIAN_POINT('Ctrl Pts',(1.73111316273383,69.3014906969056,11.4958799888797));
#45568=CARTESIAN_POINT('Ctrl Pts',(1.73588764363626,69.3024329615405,11.5004608764705));
#45569=CARTESIAN_POINT('Ctrl Pts',(1.74064410521965,69.3033754035243,11.5050605551194));
#45570=CARTESIAN_POINT('Ctrl Pts',(1.745382460388,69.3043180775947,11.509678901346));
#45571=CARTESIAN_POINT('Ctrl Pts',(1.74539430201747,69.3043204334327,11.509690443061));
#45572=CARTESIAN_POINT('Ctrl Pts',(1.7454061435337,69.3043227892722,11.5097019848927));
#45573=CARTESIAN_POINT('Ctrl Pts',(1.74541798493674,69.3043251451133,11.5097135268411));
#45574=CARTESIAN_POINT('Ctrl Pts',(1.8030488418173,69.3157907747721,11.565886969636));
#45575=CARTESIAN_POINT('Ctrl Pts',(1.8579975848143,69.3272931358038,11.6248206449648));
#45576=CARTESIAN_POINT('Ctrl Pts',(1.91000833396433,69.3387810634638,11.6863106092312));
#45577=CARTESIAN_POINT('Ctrl Pts',(1.91629329806695,69.3401692613678,11.6937410389866));
#45578=CARTESIAN_POINT('Ctrl Pts',(1.92253536353318,69.3415572540476,11.7012088585325));
#45579=CARTESIAN_POINT('Ctrl Pts',(1.92873407884509,69.3429449558,11.7087137596157));
#45580=CARTESIAN_POINT('Ctrl Pts',(1.97669639644135,69.3536822439033,11.7667826385953));
#45581=CARTESIAN_POINT('Ctrl Pts',(2.02206426325868,69.3644013308688,11.827067119155));
#45582=CARTESIAN_POINT('Ctrl Pts',(2.06465495930781,69.3750445556727,11.8894330863254));
#45583=CARTESIAN_POINT('Ctrl Pts',(2.07313001076284,69.3771624331959,11.9018431859444));
#45584=CARTESIAN_POINT('Ctrl Pts',(2.08149507952893,69.3792773231086,11.9143358680576));
#45585=CARTESIAN_POINT('Ctrl Pts',(2.08974868801882,69.3813887954505,11.9269103220508));
#45586=CARTESIAN_POINT('Ctrl Pts',(2.09150796335126,69.3818388605597,11.9295905953829));
#45587=CARTESIAN_POINT('Ctrl Pts',(2.09326185186073,69.3822886730454,11.9322740599648));
#45588=CARTESIAN_POINT('Ctrl Pts',(2.09501033148427,69.3827382384023,11.9349607119884));
#45589=CARTESIAN_POINT('Ctrl Pts',(2.13784276421261,69.3937512222827,12.0007755150414));
#45590=CARTESIAN_POINT('Ctrl Pts',(2.17743371466383,69.4046163067197,12.0685030997901));
#45591=CARTESIAN_POINT('Ctrl Pts',(2.21373045870408,69.4154117303112,12.1379092891655));
#45592=CARTESIAN_POINT('Ctrl Pts',(2.21688249549914,69.4163492130876,12.1439365753175));
#45593=CARTESIAN_POINT('Ctrl Pts',(2.2200096575108,69.4172861675077,12.149976518639));
#45594=CARTESIAN_POINT('Ctrl Pts',(2.22311189218551,69.418222643084,12.1560289641454));
#45595=CARTESIAN_POINT('Ctrl Pts',(2.26053984883482,69.4295210685565,12.2290507345104));
#45596=CARTESIAN_POINT('Ctrl Pts',(2.2943429555824,69.4407507008421,12.3038935424851));
#45597=CARTESIAN_POINT('Ctrl Pts',(2.32442367345173,69.4519815543759,12.3802724719404));
#45598=CARTESIAN_POINT('Ctrl Pts',(2.32626576753546,69.4526693135224,12.3849497929632));
#45599=CARTESIAN_POINT('Ctrl Pts',(2.32809388645792,69.4533570757873,12.389632871055));
#45600=CARTESIAN_POINT('Ctrl Pts',(2.32990800177276,69.4540448566763,12.394321639167));
#45601=CARTESIAN_POINT('Ctrl Pts',(2.36193636236869,69.4661876869281,12.4771022400536));
#45602=CARTESIAN_POINT('Ctrl Pts',(2.38960387102893,69.4783370394601,12.5616579670394));
#45603=CARTESIAN_POINT('Ctrl Pts',(2.41276317008455,69.4905523650869,12.6475996965818));
#45604=CARTESIAN_POINT('Ctrl Pts',(2.43163782306541,69.500507762774,12.717641553971));
#45605=CARTESIAN_POINT('Ctrl Pts',(2.4475174504375,69.5105064253298,12.7886032742458));
#45606=CARTESIAN_POINT('Ctrl Pts',(2.46032036786947,69.5205657976629,12.8602613757723));
#45607=CARTESIAN_POINT('Ctrl Pts',(2.4759832095527,69.5328722393097,12.9479265119019));
#45608=CARTESIAN_POINT('Ctrl Pts',(2.48695700823147,69.5452044792185,13.0361632797939));
#45609=CARTESIAN_POINT('Ctrl Pts',(2.49324964569461,69.5575667617407,13.1245401413933));
#45610=CARTESIAN_POINT('Ctrl Pts',(2.49957447029312,69.569992277917,13.2133690547795));
#45611=CARTESIAN_POINT('Ctrl Pts',(2.50117071942633,69.5824477732759,13.3023385599671));
#45612=CARTESIAN_POINT('Ctrl Pts',(2.49805608672364,69.5949132923211,13.3910440920875));
#45613=CARTESIAN_POINT('Ctrl Pts',(2.49516671437906,69.6064772645221,13.4733341518749));
#45614=CARTESIAN_POINT('Ctrl Pts',(2.48822389015378,69.6180494984437,13.555396980219));
#45615=CARTESIAN_POINT('Ctrl Pts',(2.47723921943366,69.6295996054898,13.6369443361281));
#45616=CARTESIAN_POINT('Ctrl Pts',(2.47656532930736,69.6303081841349,13.6419471222264));
#45617=CARTESIAN_POINT('Ctrl Pts',(2.47587621401331,69.6310166808024,13.6469479777495));
#45618=CARTESIAN_POINT('Ctrl Pts',(2.47517187088532,69.6317250889864,13.6519468397047));
#45619=CARTESIAN_POINT('Ctrl Pts',(2.46537114414571,69.6415823797815,13.7215045284011));
#45620=CARTESIAN_POINT('Ctrl Pts',(2.45262528353376,69.6514218402911,13.7906750536128));
#45621=CARTESIAN_POINT('Ctrl Pts',(2.43692859562038,69.6612194466812,13.8593015173351));
#45622=CARTESIAN_POINT('Ctrl Pts',(2.42200437329576,69.6705348931514,13.924550734724));
#45623=CARTESIAN_POINT('Ctrl Pts',(2.40447319609836,69.6797747920806,13.9890458939864));
#45624=CARTESIAN_POINT('Ctrl Pts',(2.38437526957604,69.6889186140611,14.0526862067553));
#45625=CARTESIAN_POINT('Ctrl Pts',(2.38436632465434,69.6889226836736,14.0527145309515));
#45626=CARTESIAN_POINT('Ctrl Pts',(2.38435737922361,69.6889267532671,14.0527428549785));
#45627=CARTESIAN_POINT('Ctrl Pts',(2.38434843328378,69.6889308228417,14.0527711788364));
#45628=CARTESIAN_POINT('Ctrl Pts',(2.36151035591637,69.6993200342555,14.1250791162566));
#45629=CARTESIAN_POINT('Ctrl Pts',(2.33535676515888,69.7095864886297,14.1962881545291));
#45630=CARTESIAN_POINT('Ctrl Pts',(2.30598464802508,69.7197980582485,14.2662152096127));
#45631=CARTESIAN_POINT('Ctrl Pts',(2.30216951873161,69.721124433811,14.275297999084));
#45632=CARTESIAN_POINT('Ctrl Pts',(2.29830005562725,69.7224498762773,14.2843590964447));
#45633=CARTESIAN_POINT('Ctrl Pts',(2.29437644417292,69.7237745280003,14.2933980431371));
#45634=CARTESIAN_POINT('Ctrl Pts',(2.26276231626872,69.7344477838734,14.3662285005309));
#45635=CARTESIAN_POINT('Ctrl Pts',(2.22763349023853,69.7450704908474,14.4376246046964));
#45636=CARTESIAN_POINT('Ctrl Pts',(2.18910076349599,69.7557017740771,14.5073320387567));
#45637=CARTESIAN_POINT('Ctrl Pts',(2.1837793768327,69.757169959009,14.5169586663354));
#45638=CARTESIAN_POINT('Ctrl Pts',(2.17839304775096,69.7586382998401,14.5265530108488));
#45639=CARTESIAN_POINT('Ctrl Pts',(2.17294204808246,69.7601069449087,14.536114327533));
#45640=CARTESIAN_POINT('Ctrl Pts',(2.13137878965643,69.7713051981162,14.609018290183));
#45641=CARTESIAN_POINT('Ctrl Pts',(2.08605615374757,69.7825217257262,14.680005875772));
#45642=CARTESIAN_POINT('Ctrl Pts',(2.03712301582743,69.7938014659925,14.7487408392039));
#45643=CARTESIAN_POINT('Ctrl Pts',(2.03316839621133,69.7947130585046,14.7542957789901));
#45644=CARTESIAN_POINT('Ctrl Pts',(2.02919018990079,69.7956250616874,14.7598359784257));
#45645=CARTESIAN_POINT('Ctrl Pts',(2.02518847321715,69.7965374980996,14.765361245264));
#45646=CARTESIAN_POINT('Ctrl Pts',(1.97315048731705,69.80840274417,14.8372113487462));
#45647=CARTESIAN_POINT('Ctrl Pts',(1.9174131813531,69.8202791647436,14.9061601506594));
#45648=CARTESIAN_POINT('Ctrl Pts',(1.85829189772205,69.8321897426764,14.9718940227602));
#45649=CARTESIAN_POINT('Ctrl Pts',(1.79861679112262,69.8442118938232,15.0382436617376));
#45650=CARTESIAN_POINT('Ctrl Pts',(1.73549496583036,69.8562685440475,15.101316979798));
#45651=CARTESIAN_POINT('Ctrl Pts',(1.66925420501732,69.8683584881138,15.1608171881416));
#45652=CARTESIAN_POINT('Ctrl Pts',(1.60367188503604,69.8803282567364,15.2197259575254));
#45653=CARTESIAN_POINT('Ctrl Pts',(1.53503370614351,69.8923302386959,15.2751322740645));
#45654=CARTESIAN_POINT('Ctrl Pts',(1.46364342249625,69.9043445863292,15.3267799436083));
#45655=CARTESIAN_POINT('Ctrl Pts',(1.40873436921352,69.9135852899748,15.3665041818943));
#45656=CARTESIAN_POINT('Ctrl Pts',(1.35219717552376,69.9228328780306,15.4040057465273));
#45657=CARTESIAN_POINT('Ctrl Pts',(1.29415591594126,69.9320730965854,15.4391790836035));
#45658=CARTESIAN_POINT('Ctrl Pts',(1.23022248155498,69.9422513544479,15.4779231124942));
#45659=CARTESIAN_POINT('Ctrl Pts',(1.16474992615481,69.9523753930348,15.5136695269958));
#45660=CARTESIAN_POINT('Ctrl Pts',(1.09791606230348,69.9624237368063,15.5463656837148));
#45661=CARTESIAN_POINT('Ctrl Pts',(1.08528489012075,69.9643228094174,15.5525450479088));
#45662=CARTESIAN_POINT('Ctrl Pts',(1.07260494573646,69.9662191904854,15.5586154447488));
#45663=CARTESIAN_POINT('Ctrl Pts',(1.05987722280761,69.9681127520765,15.5645764873251));
#45664=CARTESIAN_POINT('Ctrl Pts',(1.01749693022492,69.9744178621662,15.5844253424497));
#45665=CARTESIAN_POINT('Ctrl Pts',(0.974587743570524,69.9806914853537,15.6030623844121));
#45666=CARTESIAN_POINT('Ctrl Pts',(0.931181893463117,69.9869285085228,15.6204741968846));
#45667=CARTESIAN_POINT('Ctrl Pts',(0.93113646091439,69.986935036764,15.6204924216865));
#45668=CARTESIAN_POINT('Ctrl Pts',(0.93109102782079,69.9869415649654,15.6205106451451));
#45669=CARTESIAN_POINT('Ctrl Pts',(0.931045594182292,69.9869480931269,15.6205288672604));
#45670=CARTESIAN_POINT('Ctrl Pts',(0.862582976136436,69.9967851883703,15.6479872386433));
#45671=CARTESIAN_POINT('Ctrl Pts',(0.792881203027636,70.006532272519,15.6723992841724));
#45672=CARTESIAN_POINT('Ctrl Pts',(0.722111028103673,70.0162431913653,15.6937042086057));
#45673=CARTESIAN_POINT('Ctrl Pts',(0.710197042261118,70.0178780007999,15.6972908405216));
#45674=CARTESIAN_POINT('Ctrl Pts',(0.698252834406958,70.0195117735174,15.7007893095625));
#45675=CARTESIAN_POINT('Ctrl Pts',(0.686279293816833,70.0211447521252,15.7041992031062));
#45676=CARTESIAN_POINT('Ctrl Pts',(0.612265188066109,70.0312389636461,15.7252773645273));
#45677=CARTESIAN_POINT('Ctrl Pts',(0.537127501164212,70.0413034609848,15.7429736632169));
#45678=CARTESIAN_POINT('Ctrl Pts',(0.461100222343306,70.0513841327094,15.7571915589655));
#45679=CARTESIAN_POINT('Ctrl Pts',(0.449893828301642,70.0528700201606,15.7592872717763));
#45680=CARTESIAN_POINT('Ctrl Pts',(0.438668165611532,70.0543562504055,15.7613073401694));
#45681=CARTESIAN_POINT('Ctrl Pts',(0.427424047954188,70.055842961437,15.7632513844396));
#45682=CARTESIAN_POINT('Ctrl Pts',(0.406594269687557,70.0585971002742,15.766852735148));
#45683=CARTESIAN_POINT('Ctrl Pts',(0.385701175003112,70.0613528250924,15.7701934092717));
#45684=CARTESIAN_POINT('Ctrl Pts',(0.364750122956928,70.0641108683095,15.7732712637113));
#45685=CARTESIAN_POINT('Ctrl Pts',(0.277743471818803,70.0755646179105,15.7860531424871));
#45686=CARTESIAN_POINT('Ctrl Pts',(0.19018823497606,70.087000641333,15.7942347475934));
#45687=CARTESIAN_POINT('Ctrl Pts',(0.102510667813711,70.0984565180099,15.7978109533579));
#45688=CARTESIAN_POINT('Ctrl Pts',(0.01358043595333,70.1100760667955,15.8014382529981));
#45689=CARTESIAN_POINT('Ctrl Pts',(-0.0754742851914581,70.1217158403208,
15.8003268962746));
#45690=CARTESIAN_POINT('Ctrl Pts',(-0.164199033821504,70.1333925230572,
15.7944943321978));
#45691=CARTESIAN_POINT('Ctrl Pts',(-0.252756319590444,70.1450471667263,
15.7886727767502));
#45692=CARTESIAN_POINT('Ctrl Pts',(-0.340983424829321,70.1567382485531,
15.7781481170492));
#45693=CARTESIAN_POINT('Ctrl Pts',(-0.428440479512438,70.1684641869835,
15.7629633930642));
#45694=CARTESIAN_POINT('Ctrl Pts',(-0.494062496909083,70.1772625593786,
15.751569775647));
#45695=CARTESIAN_POINT('Ctrl Pts',(-0.559251153861324,70.1860801433988,
15.7375532922927));
#45696=CARTESIAN_POINT('Ctrl Pts',(-0.623831971164928,70.1949113471847,
15.7209379703818));
#45697=CARTESIAN_POINT('Ctrl Pts',(-0.69839193812473,70.2051071652307,15.7017552176011));
#45698=CARTESIAN_POINT('Ctrl Pts',(-0.771800687543043,70.2152748164325,
15.6791962467254));
#45699=CARTESIAN_POINT('Ctrl Pts',(-0.843847806244314,70.2254015817701,
15.6533881351996));
#45700=CARTESIAN_POINT('Ctrl Pts',(-0.855334802569033,70.2270161656467,
15.6492733602081));
#45701=CARTESIAN_POINT('Ctrl Pts',(-0.866787255135574,70.2286297189187,
15.6450759093358));
#45702=CARTESIAN_POINT('Ctrl Pts',(-0.878204386210756,70.2302421999663,
15.6407962017555));
#45703=CARTESIAN_POINT('Ctrl Pts',(-0.947352556727918,70.2400082360834,
15.6148760342825));
#45704=CARTESIAN_POINT('Ctrl Pts',(-1.01520313841598,70.2497344017798,15.585942753797));
#45705=CARTESIAN_POINT('Ctrl Pts',(-1.08160798117368,70.2594089171849,15.5540849648858));
#45706=CARTESIAN_POINT('Ctrl Pts',(-1.0943450491834,70.2612645794462,15.5479743439258));
#45707=CARTESIAN_POINT('Ctrl Pts',(-1.10702900301784,70.2631183551719,15.541755994678));
#45708=CARTESIAN_POINT('Ctrl Pts',(-1.11965889759404,70.2649701808128,15.5354303468635));
#45709=CARTESIAN_POINT('Ctrl Pts',(-1.14794015873828,70.2691168476142,15.5212657553328));
#45710=CARTESIAN_POINT('Ctrl Pts',(-1.17595043962458,70.2732536617004,15.5065635206852));
#45711=CARTESIAN_POINT('Ctrl Pts',(-1.20368003277824,70.2773798529382,15.491327901301));
#45712=CARTESIAN_POINT('Ctrl Pts',(-1.2037229633007,70.277386241043,15.4913043137533));
#45713=CARTESIAN_POINT('Ctrl Pts',(-1.20376589315014,70.2773926291224,15.4912807249264));
#45714=CARTESIAN_POINT('Ctrl Pts',(-1.20380882232651,70.2773990171765,15.4912571348202));
#45715=CARTESIAN_POINT('Ctrl Pts',(-1.26742642944486,70.2868656026444,15.4562984834978));
#45716=CARTESIAN_POINT('Ctrl Pts',(-1.32957019752597,70.2962770242264,15.4185311107454));
#45717=CARTESIAN_POINT('Ctrl Pts',(-1.39009318732037,70.3056726599036,15.3780181758782));
#45718=CARTESIAN_POINT('Ctrl Pts',(-1.40251309408387,70.3076007358214,15.3697045272055));
#45719=CARTESIAN_POINT('Ctrl Pts',(-1.41486457486924,70.3095281303524,15.3612752388359));
#45720=CARTESIAN_POINT('Ctrl Pts',(-1.42714609176254,70.3114551579939,15.3527308358896));
#45721=CARTESIAN_POINT('Ctrl Pts',(-1.45440827917267,70.3157327231484,15.3337641954937));
#45722=CARTESIAN_POINT('Ctrl Pts',(-1.48132603291762,70.3200084353271,15.3142305611203));
#45723=CARTESIAN_POINT('Ctrl Pts',(-1.50788174594805,70.3242853535711,15.2941366208503));
#45724=CARTESIAN_POINT('Ctrl Pts',(-1.57266814708591,70.3347194978424,15.2451146242168));
#45725=CARTESIAN_POINT('Ctrl Pts',(-1.63499119347552,70.3451119765115,15.192990508662));
#45726=CARTESIAN_POINT('Ctrl Pts',(-1.69463638386186,70.3554981699385,15.1379691056813));
#45727=CARTESIAN_POINT('Ctrl Pts',(-1.69878705948321,70.3562209393618,15.1341401968535));
#45728=CARTESIAN_POINT('Ctrl Pts',(-1.70292474658918,70.3569436760685,15.130297254325));
#45729=CARTESIAN_POINT('Ctrl Pts',(-1.70704936373546,70.3576663909591,15.126440346116));
#45730=CARTESIAN_POINT('Ctrl Pts',(-1.77160880991124,70.3689784888895,15.0660711411471));
#45731=CARTESIAN_POINT('Ctrl Pts',(-1.83297023730468,70.3802857665096,15.0022808156671));
#45732=CARTESIAN_POINT('Ctrl Pts',(-1.89083291826391,70.3916163554277,14.9353661169356));
#45733=CARTESIAN_POINT('Ctrl Pts',(-1.94914069489051,70.4030341023543,14.8679366919247));
#45734=CARTESIAN_POINT('Ctrl Pts',(-2.00389420879611,70.4144753004314,14.7973351616577));
#45735=CARTESIAN_POINT('Ctrl Pts',(-2.0547890930373,70.4259538792498,14.7238968456928));
#45736=CARTESIAN_POINT('Ctrl Pts',(-2.09195668421999,70.4343364727312,14.6702662039176));
#45737=CARTESIAN_POINT('Ctrl Pts',(-2.12706653535575,70.4427386678698,14.6151234984332));
#45738=CARTESIAN_POINT('Ctrl Pts',(-2.16000686497024,70.4511621004216,14.5586058797152));
#45739=CARTESIAN_POINT('Ctrl Pts',(-2.20220603956577,70.4619531855476,14.4862023279622));
#45740=CARTESIAN_POINT('Ctrl Pts',(-2.24063570839904,70.4727262416205,14.4118998419532));
#45741=CARTESIAN_POINT('Ctrl Pts',(-2.27519405667041,70.4834798357975,14.3360364825278));
#45742=CARTESIAN_POINT('Ctrl Pts',(-2.27753892085078,70.484209492134,14.3308889774236));
#45743=CARTESIAN_POINT('Ctrl Pts',(-2.27986595804307,70.484939060164,14.3257342667091));
#45744=CARTESIAN_POINT('Ctrl Pts',(-2.2821751346037,70.4856685400044,14.3205724476062));
#45745=CARTESIAN_POINT('Ctrl Pts',(-2.31455928023641,70.4958988453829,14.2481825297417));
#45746=CARTESIAN_POINT('Ctrl Pts',(-2.3434322556813,70.5061113456515,14.174399032633));
#45747=CARTESIAN_POINT('Ctrl Pts',(-2.3687287929498,70.5163037689282,14.099477053488));
#45748=CARTESIAN_POINT('Ctrl Pts',(-2.37182718200157,70.5175521647998,14.0903004046267));
#45749=CARTESIAN_POINT('Ctrl Pts',(-2.37487189986608,70.5188002649376,14.081106614678));
#45750=CARTESIAN_POINT('Ctrl Pts',(-2.37786281017834,70.5200480697423,14.0718961013543));
#45751=CARTESIAN_POINT('Ctrl Pts',(-2.40125907834412,70.5298089695291,13.9998472542915));
#45752=CARTESIAN_POINT('Ctrl Pts',(-2.4213651855868,70.5395513109683,13.9267791929086));
#45753=CARTESIAN_POINT('Ctrl Pts',(-2.43812763170418,70.5492750724892,13.8528720253056));
#45754=CARTESIAN_POINT('Ctrl Pts',(-2.44065479389618,70.5507410591541,13.8417295346228));
#45755=CARTESIAN_POINT('Ctrl Pts',(-2.4431059143404,70.5522066324039,13.8305678847687));
#45756=CARTESIAN_POINT('Ctrl Pts',(-2.44548076118895,70.5536718016633,13.8193876015694));
#45757=CARTESIAN_POINT('Ctrl Pts',(-2.44973892873762,70.5562988915733,13.7993410376688));
#45758=CARTESIAN_POINT('Ctrl Pts',(-2.45375200762531,70.5589246676948,13.7792346069052));
#45759=CARTESIAN_POINT('Ctrl Pts',(-2.45751873206479,70.5615491847454,13.7590711743978));
#45760=CARTESIAN_POINT('Ctrl Pts',(-2.45752562215502,70.5615539855105,13.7590342914584));
#45761=CARTESIAN_POINT('Ctrl Pts',(-2.4575325114208,70.5615587862714,13.7589974083281));
#45762=CARTESIAN_POINT('Ctrl Pts',(-2.45753939986211,70.5615635870281,13.7589605250071));
#45763=CARTESIAN_POINT('Ctrl Pts',(-2.46528867627758,70.5669642849811,13.7174679671417));
#45764=CARTESIAN_POINT('Ctrl Pts',(-2.47199483430321,70.5723597156861,13.6757336645926));
#45765=CARTESIAN_POINT('Ctrl Pts',(-2.47764411293714,70.5777541555775,13.6337938114561));
#45766=CARTESIAN_POINT('Ctrl Pts',(-2.48852935099954,70.5881483609682,13.5529825583252));
#45767=CARTESIAN_POINT('Ctrl Pts',(-2.49544042130253,70.5984920278951,13.471776143099));
#45768=CARTESIAN_POINT('Ctrl Pts',(-2.49838216990339,70.6088101525565,13.3904693114515));
#45769=CARTESIAN_POINT('Ctrl Pts',(-2.49861827024406,70.6096382698018,13.3839437468113));
#45770=CARTESIAN_POINT('Ctrl Pts',(-2.49882877883583,70.6104662196973,13.3774175493841));
#45771=CARTESIAN_POINT('Ctrl Pts',(-2.49901368622386,70.6112940136901,13.3708908792594));
#45772=CARTESIAN_POINT('Ctrl Pts',(-2.49967335126509,70.6142472042803,13.3476067035272));
#45773=CARTESIAN_POINT('Ctrl Pts',(-2.50000751548752,70.6171983845687,13.3243165065547));
#45774=CARTESIAN_POINT('Ctrl Pts',(-2.50001628522819,70.6201479917331,13.3010276898172));
#45775=CARTESIAN_POINT('Ctrl Pts',(-2.49999978870036,70.6201493965427,13.3010278609544));
#45776=CARTESIAN_POINT('Ctrl Pts',(-2.49999992956743,70.6201927897384,13.3006852390838));
#45777=CARTESIAN_POINT('Ctrl Pts',(-2.5,70.620236182436,13.3003426187556));
#45778=CARTESIAN_POINT('Ctrl Pts',(-2.5,70.6202795746371,13.2999999999913));
#45779=CARTESIAN_POINT('',(1.35925139903161,68.5015684297319,11.2018017462371));
#45780=CARTESIAN_POINT('Ctrl Pts',(-2.5,69.6117391960828,13.3));
#45781=CARTESIAN_POINT('Ctrl Pts',(-2.5,69.5868984362623,13.5116533107127));
#45782=CARTESIAN_POINT('Ctrl Pts',(-2.47312159666966,69.5620969687835,13.7229015939511));
#45783=CARTESIAN_POINT('Ctrl Pts',(-2.37956580310906,69.5182587119009,14.083015772128));
#45784=CARTESIAN_POINT('Ctrl Pts',(-2.32476545853278,69.4995523412897,14.2332315126848));
#45785=CARTESIAN_POINT('Ctrl Pts',(-2.12606976051521,69.4458587704588,14.6493637701716));
#45786=CARTESIAN_POINT('Ctrl Pts',(-1.94793740573065,69.4117941420902,14.8957805457345));
#45787=CARTESIAN_POINT('Ctrl Pts',(-1.48832906641449,69.3386088439744,15.3364632396691));
#45788=CARTESIAN_POINT('Ctrl Pts',(-1.20220079857416,69.3001093631724,15.5174526183101));
#45789=CARTESIAN_POINT('Ctrl Pts',(-0.582791217961786,69.2255759157103,
15.7530787964279));
#45790=CARTESIAN_POINT('Ctrl Pts',(-0.256787408095275,69.1896508547796,
15.8082458630207));
#45791=CARTESIAN_POINT('Ctrl Pts',(0.368292389417417,69.119256871216,15.7905983579557));
#45792=CARTESIAN_POINT('Ctrl Pts',(0.662216165928006,69.0864985363696,15.7290484483144));
#45793=CARTESIAN_POINT('Ctrl Pts',(1.08466724944942,69.0372135465817,15.5579615117129));
#45794=CARTESIAN_POINT('Ctrl Pts',(1.22496652487473,69.0203448330629,15.4850279835998));
#45795=CARTESIAN_POINT('Ctrl Pts',(1.63261569660207,68.9676090591445,15.2214417251557));
#45796=CARTESIAN_POINT('Ctrl Pts',(1.87023210697087,68.9318521879707,14.9910721409861));
#45797=CARTESIAN_POINT('Ctrl Pts',(2.24050175203724,68.8634697219996,14.4553092538144));
#45798=CARTESIAN_POINT('Ctrl Pts',(2.37101546223115,68.8306680820086,14.1560772195167));
#45799=CARTESIAN_POINT('Ctrl Pts',(2.50473075109296,68.7656663114431,13.5520242921483));
#45800=CARTESIAN_POINT('Ctrl Pts',(2.516993553084,68.7355808882792,13.254584108532));
#45801=CARTESIAN_POINT('Ctrl Pts',(2.45537931489148,68.6908075740461,12.8033106644488));
#45802=CARTESIAN_POINT('Ctrl Pts',(2.41857985065703,68.6753936489625,12.6472704213994));
#45803=CARTESIAN_POINT('Ctrl Pts',(2.27002573796472,68.6299422017385,12.2099966991114));
#45804=CARTESIAN_POINT('Ctrl Pts',(2.12189734459302,68.5997252687359,11.9439725157658));
#45805=CARTESIAN_POINT('Ctrl Pts',(1.76687834959433,68.5473097365251,11.5128583182058));
#45806=CARTESIAN_POINT('Ctrl Pts',(1.57444119245041,68.5248031972306,11.3412057157747));
#45807=CARTESIAN_POINT('Ctrl Pts',(1.3592513647516,68.5015684831821,11.2018017902446));
#45808=CARTESIAN_POINT('Ctrl Pts',(1.35922685968084,68.5017698542948,11.2017859156125));
#45809=CARTESIAN_POINT('Ctrl Pts',(1.16329772448109,68.4679246869375,11.0748626692483));
#45810=CARTESIAN_POINT('Ctrl Pts',(0.950487220343815,68.4340759749094,10.9759635422888));
#45811=CARTESIAN_POINT('Ctrl Pts',(0.466658774060705,68.3626134545601,10.8289163155397));
#45812=CARTESIAN_POINT('Ctrl Pts',(0.19513354664671,68.3252407491545,10.7928130380239));
#45813=CARTESIAN_POINT('Ctrl Pts',(-0.383778198058173,68.2440015915658,
10.8106250704725));
#45814=CARTESIAN_POINT('Ctrl Pts',(-0.686331796473102,68.2006307553199,
10.8765229155169));
#45815=CARTESIAN_POINT('Ctrl Pts',(-1.2788474602455,68.1114145517084,11.1257719889208));
#45816=CARTESIAN_POINT('Ctrl Pts',(-1.55900536851427,68.0667979413492,11.3169972368763));
#45817=CARTESIAN_POINT('Ctrl Pts',(-2.00124833323174,67.9802453746223,11.7721669464916));
#45818=CARTESIAN_POINT('Ctrl Pts',(-2.16937622326692,67.9393861545933,12.0220700233241));
#45819=CARTESIAN_POINT('Ctrl Pts',(-2.42436824473168,67.8538965558814,12.6033695120974));
#45820=CARTESIAN_POINT('Ctrl Pts',(-2.49595863888419,67.8102147607181,12.9351487417965));
#45821=CARTESIAN_POINT('Ctrl Pts',(-2.49994461778903,67.7643387514265,13.2807826890184));
#45822=CARTESIAN_POINT('Ctrl Pts',(-2.50000000009011,67.7630631808826,13.2903925247493));
#45823=CARTESIAN_POINT('Ctrl Pts',(-2.5,67.7617877839724,13.3000000234479));
#45824=CARTESIAN_POINT('Origin',(0.,70.2,13.3));
#45825=CARTESIAN_POINT('',(-0.20632980674377,66.2927243572952,10.8082436938974));
#45826=CARTESIAN_POINT('Ctrl Pts',(-2.5,67.7617877839724,13.3000000234479));
#45827=CARTESIAN_POINT('Ctrl Pts',(-2.49999999722602,67.7225256620901,13.5957595488635));
#45828=CARTESIAN_POINT('Ctrl Pts',(-2.44751521952288,67.6833209369714,13.8892901188729));
#45829=CARTESIAN_POINT('Ctrl Pts',(-2.28875435858697,67.6232069710623,14.3187295896263));
#45830=CARTESIAN_POINT('Ctrl Pts',(-2.21799892564411,67.6021721375708,14.4647730683009));
#45831=CARTESIAN_POINT('Ctrl Pts',(-1.96868832241002,67.5399978003467,14.8730234644183));
#45832=CARTESIAN_POINT('Ctrl Pts',(-1.7539605333616,67.4993192332267,15.109363162545));
#45833=CARTESIAN_POINT('Ctrl Pts',(-1.36688160654624,67.4370998399759,15.3999264567616));
#45834=CARTESIAN_POINT('Ctrl Pts',(-1.22314933749683,67.4157082165148,15.4867709879815));
#45835=CARTESIAN_POINT('Ctrl Pts',(-0.9256486713516,67.3736180420083,15.6279493782103));
#45836=CARTESIAN_POINT('Ctrl Pts',(-0.773094630311917,67.3530216905194,
15.6829607786152));
#45837=CARTESIAN_POINT('Ctrl Pts',(-0.292696823526602,67.2899391679536,
15.8051584395702));
#45838=CARTESIAN_POINT('Ctrl Pts',(0.0441693313863235,67.2482188913854,
15.8218223071524));
#45839=CARTESIAN_POINT('Ctrl Pts',(0.693875930672618,67.1658110326071,15.7234184875379));
#45840=CARTESIAN_POINT('Ctrl Pts',(1.00101021270645,67.1258696982556,15.6135330787129));
#45841=CARTESIAN_POINT('Ctrl Pts',(1.41651319070852,67.0659308077562,15.366204515324));
#45842=CARTESIAN_POINT('Ctrl Pts',(1.5460938564108,67.0461661417386,15.271118924942));
#45843=CARTESIAN_POINT('Ctrl Pts',(1.90894206626637,66.986267381346,14.9469240839239));
#45844=CARTESIAN_POINT('Ctrl Pts',(2.10734890652499,66.9467409247531,14.6840280321213));
#45845=CARTESIAN_POINT('Ctrl Pts',(2.31887673554413,66.8877298751789,14.2476256427034));
#45846=CARTESIAN_POINT('Ctrl Pts',(2.3743444830329,66.8685386145047,14.0985475386327));
#45847=CARTESIAN_POINT('Ctrl Pts',(2.45661310108357,66.8300830155865,13.790580312074));
#45848=CARTESIAN_POINT('Ctrl Pts',(2.48297741687454,66.8109086574451,13.6323324635222));
#45849=CARTESIAN_POINT('Ctrl Pts',(2.51707300787301,66.7517406660427,13.139792194619));
#45850=CARTESIAN_POINT('Ctrl Pts',(2.47325120089564,66.7122277110131,12.8056304521614));
#45851=CARTESIAN_POINT('Ctrl Pts',(2.31268382373457,66.6537832086372,12.3368425662245));
#45852=CARTESIAN_POINT('Ctrl Pts',(2.2455174742449,66.6348512048037,12.1892192379082));
#45853=CARTESIAN_POINT('Ctrl Pts',(1.9995758508219,66.5772088143333,11.7636354028661));
#45854=CARTESIAN_POINT('Ctrl Pts',(1.77971327059208,66.5389983508999,11.5135514593427));
#45855=CARTESIAN_POINT('Ctrl Pts',(1.39541318339668,66.483385867781,11.2199826808397));
#45856=CARTESIAN_POINT('Ctrl Pts',(1.2648488428219,66.4658426669773,11.1381004340619));
#45857=CARTESIAN_POINT('Ctrl Pts',(0.914284569745283,66.4208540202292,10.9609400434414));
#45858=CARTESIAN_POINT('Ctrl Pts',(0.686598815799409,66.3936233209689,10.8842756362153));
#45859=CARTESIAN_POINT('Ctrl Pts',(0.234623662540332,66.34180468946,10.8012871093587));
#45860=CARTESIAN_POINT('Ctrl Pts',(0.0134371728524807,66.3173924881665,
10.7903300910262));
#45861=CARTESIAN_POINT('Ctrl Pts',(-0.206318250554135,66.2928316028488,
10.8085279894231));
#45862=CARTESIAN_POINT('',(-2.5,65.696789585947,13.2999999999999));
#45863=CARTESIAN_POINT('Ctrl Pts',(-0.206248650970427,66.2923157697828,
10.8085222268756));
#45864=CARTESIAN_POINT('Ctrl Pts',(-0.492720738343416,66.2438642690178,
10.832236860094));
#45865=CARTESIAN_POINT('Ctrl Pts',(-0.772845838683397,66.1937747245436,
10.9051866997659));
#45866=CARTESIAN_POINT('Ctrl Pts',(-1.25578965221234,66.1019374669533,11.1246328414266));
#45867=CARTESIAN_POINT('Ctrl Pts',(-1.46186855298299,66.0616368429323,11.2572875518897));
#45868=CARTESIAN_POINT('Ctrl Pts',(-1.89948718136495,65.9727967771414,11.6400300826565));
#45869=CARTESIAN_POINT('Ctrl Pts',(-2.10569846836433,65.9238380940771,11.9108527376458));
#45870=CARTESIAN_POINT('Ctrl Pts',(-2.37726386591633,65.8260764030656,12.4743249644652));
#45871=CARTESIAN_POINT('Ctrl Pts',(-2.45656126657527,65.7795732932735,12.7537071211792));
#45872=CARTESIAN_POINT('Ctrl Pts',(-2.49550840758641,65.7223041543191,13.1268508588702));
#45873=CARTESIAN_POINT('Ctrl Pts',(-2.49999999999999,65.709424128047,13.213474844254));
#45874=CARTESIAN_POINT('Ctrl Pts',(-2.5,65.696789585947,13.2999999999997));
#45875=CARTESIAN_POINT('',(-2.5,66.7778885669818,13.3));
#45876=CARTESIAN_POINT('',(-2.5,70.2,13.3));
#45877=CARTESIAN_POINT('Ctrl Pts',(-2.5,66.7778885669818,13.3));
#45878=CARTESIAN_POINT('Ctrl Pts',(-2.5,66.7918413044886,13.1852589379609));
#45879=CARTESIAN_POINT('Ctrl Pts',(-2.49210079537757,66.8057580925441,13.0703921209457));
#45880=CARTESIAN_POINT('Ctrl Pts',(-2.43495215129586,66.8558636094013,12.6587480632189));
#45881=CARTESIAN_POINT('Ctrl Pts',(-2.34038603459958,66.8912358567461,12.3711285140565));
#45882=CARTESIAN_POINT('Ctrl Pts',(-2.04271380146662,66.9660389016043,11.8228429549495));
#45883=CARTESIAN_POINT('Ctrl Pts',(-1.8345944822031,67.0044353555049,11.5711348115867));
#45884=CARTESIAN_POINT('Ctrl Pts',(-1.32734782214467,67.0820580522804,11.1555986421081));
#45885=CARTESIAN_POINT('Ctrl Pts',(-1.0310556023197,67.1205391368846,10.998432575161));
#45886=CARTESIAN_POINT('Ctrl Pts',(-0.560974796121357,67.1790585878968,
10.8586114429367));
#45887=CARTESIAN_POINT('Ctrl Pts',(-0.405248485500008,67.1979261353801,
10.827985950135));
#45888=CARTESIAN_POINT('Ctrl Pts',(0.0215944749802646,67.2485059398258,
10.78549190141));
#45889=CARTESIAN_POINT('Ctrl Pts',(0.293465307249012,67.2793701113925,10.8025706557839));
#45890=CARTESIAN_POINT('Ctrl Pts',(0.700935861631911,67.3269947439867,10.8957568463845));
#45891=CARTESIAN_POINT('Ctrl Pts',(0.841319429460069,67.3437349888158,10.9412140832751));
#45892=CARTESIAN_POINT('Ctrl Pts',(1.28520168748909,67.3997086012979,11.1296436413456));
#45893=CARTESIAN_POINT('Ctrl Pts',(1.56421133847712,67.4389649266098,11.3212222920514));
#45894=CARTESIAN_POINT('Ctrl Pts',(2.01027649080665,67.5113508665155,11.7825148298095));
#45895=CARTESIAN_POINT('Ctrl Pts',(2.18101087549921,67.5442913843132,12.0401744489584));
#45896=CARTESIAN_POINT('Ctrl Pts',(2.4240201399684,67.6148620195753,12.6120683372072));
#45897=CARTESIAN_POINT('Ctrl Pts',(2.49135655174185,67.6509290513449,12.9226361181987));
#45898=CARTESIAN_POINT('Ctrl Pts',(2.50682470755549,67.7187639505598,13.5421114795545));
#45899=CARTESIAN_POINT('Ctrl Pts',(2.45871982272519,67.750186200484,13.8454189862729));
#45900=CARTESIAN_POINT('Ctrl Pts',(2.251745196374,67.8185899091536,14.4313842011514));
#45901=CARTESIAN_POINT('Ctrl Pts',(2.0903038501426,67.8540092266959,14.7075513449628));
#45902=CARTESIAN_POINT('Ctrl Pts',(1.68396679177138,67.9188317723156,15.1719572106393));
#45903=CARTESIAN_POINT('Ctrl Pts',(1.44748494170992,67.9480240235824,15.3602784316105));
#45904=CARTESIAN_POINT('Ctrl Pts',(0.899674880587149,68.0132688187001,15.654619675979));
#45905=CARTESIAN_POINT('Ctrl Pts',(0.589032099880397,68.0479853858131,15.7509057350415));
#45906=CARTESIAN_POINT('Ctrl Pts',(-0.0270692607296119,68.109375633073,
15.8174764530437));
#45907=CARTESIAN_POINT('Ctrl Pts',(-0.325929982479385,68.1360588846597,
15.7964296452563));
#45908=CARTESIAN_POINT('Ctrl Pts',(-0.927580749741263,68.1969626388315,
15.6439618401786));
#45909=CARTESIAN_POINT('Ctrl Pts',(-1.22304781389004,68.230108754567,15.504328224522));
#45910=CARTESIAN_POINT('Ctrl Pts',(-1.71691579141469,68.2857881259515,15.1401472128048));
#45911=CARTESIAN_POINT('Ctrl Pts',(-1.91827023404044,68.3087014678107,14.9291326085142));
#45912=CARTESIAN_POINT('Ctrl Pts',(-2.2326618221574,68.3577384042391,14.4583269641961));
#45913=CARTESIAN_POINT('Ctrl Pts',(-2.34717466342319,68.3834492539409,14.2041450269218));
#45914=CARTESIAN_POINT('Ctrl Pts',(-2.47231368909138,68.4235361610872,13.7286746008922));
#45915=CARTESIAN_POINT('Ctrl Pts',(-2.49999759002584,68.4390631270895,13.5148895441053));
#45916=CARTESIAN_POINT('Ctrl Pts',(-2.49999999984276,68.453694114733,13.3000280391888));
#45917=CARTESIAN_POINT('Origin',(0.,70.2,13.3));
#45918=CARTESIAN_POINT('',(-2.5,63.5861738118246,13.3));
#45919=CARTESIAN_POINT('',(-2.5,64.7766865736815,13.2999999985417));
#45920=CARTESIAN_POINT('',(-2.5,70.2,13.3));
#45921=CARTESIAN_POINT('Ctrl Pts',(-2.5,64.7766865736815,13.2999999970835));
#45922=CARTESIAN_POINT('Ctrl Pts',(-2.49999999965576,64.8164008365653,13.0049246949997));
#45923=CARTESIAN_POINT('Ctrl Pts',(-2.44775725432166,64.855896686039,12.7120539935902));
#45924=CARTESIAN_POINT('Ctrl Pts',(-2.23481454245837,64.9376441713423,12.1346235687608));
#45925=CARTESIAN_POINT('Ctrl Pts',(-2.06735487938246,64.9800658702118,11.8582854382355));
#45926=CARTESIAN_POINT('Ctrl Pts',(-1.62784326520881,65.0667847652865,11.373375077376));
#45927=CARTESIAN_POINT('Ctrl Pts',(-1.35589850308388,65.1101015735457,11.1731892740713));
#45928=CARTESIAN_POINT('Ctrl Pts',(-0.749236115015228,65.1982470950867,
10.8915700195959));
#45929=CARTESIAN_POINT('Ctrl Pts',(-0.420611491999876,65.241294996556,10.8130324822582));
#45930=CARTESIAN_POINT('Ctrl Pts',(0.0722700300150027,65.3056861833212,
10.7960151635174));
#45931=CARTESIAN_POINT('Ctrl Pts',(0.230969399305698,65.3263938329972,10.8056426584217));
#45932=CARTESIAN_POINT('Ctrl Pts',(0.717892393503333,65.390532821863,10.8820766748746));
#45933=CARTESIAN_POINT('Ctrl Pts',(1.03439191845666,65.433173265611,10.9996139717914));
#45934=CARTESIAN_POINT('Ctrl Pts',(1.60248948455939,65.519743013992,11.3522268419152));
#45935=CARTESIAN_POINT('Ctrl Pts',(1.84834766112784,65.5621883103019,11.5837742387333));
#45936=CARTESIAN_POINT('Ctrl Pts',(2.13372005689657,65.625678982509,11.9874361549427));
#45937=CARTESIAN_POINT('Ctrl Pts',(2.21331029422729,65.6461981821876,12.1266098265435));
#45938=CARTESIAN_POINT('Ctrl Pts',(2.4164263685598,65.7095121501173,12.5771040557331));
#45939=CARTESIAN_POINT('Ctrl Pts',(2.4913221117068,65.7515893489608,12.906264654977));
#45940=CARTESIAN_POINT('Ctrl Pts',(2.50725549696481,65.8367710959168,13.5744797604832));
#45941=CARTESIAN_POINT('Ctrl Pts',(2.44815922708852,65.8786796610131,13.906802360106));
#45942=CARTESIAN_POINT('Ctrl Pts',(2.26683798631002,65.941188151735,14.3662878980475));
#45943=CARTESIAN_POINT('Ctrl Pts',(2.19408169130771,65.9613563491209,14.5089382612658));
#45944=CARTESIAN_POINT('Ctrl Pts',(1.92866174281978,66.0237002790106,14.9253809960834));
#45945=CARTESIAN_POINT('Ctrl Pts',(1.69444577020903,66.0652338265536,15.1682811507576));
#45946=CARTESIAN_POINT('Ctrl Pts',(1.28307061606148,66.1279136968628,15.4520142477283));
#45947=CARTESIAN_POINT('Ctrl Pts',(1.13770749664708,66.1486105514198,15.5322768763966));
#45948=CARTESIAN_POINT('Ctrl Pts',(0.837972295611676,66.1893788022971,15.660839261364));
#45949=CARTESIAN_POINT('Ctrl Pts',(0.68471636599104,66.2093617375317,15.7097562943906));
#45950=CARTESIAN_POINT('Ctrl Pts',(0.375294234782263,66.2488151249023,15.7765917640375));
#45951=CARTESIAN_POINT('Ctrl Pts',(0.220006241415938,66.2681970853179,15.7951856248744));
#45952=CARTESIAN_POINT('Ctrl Pts',(-0.271061763174914,66.3292938258388,
15.8077609983177));
#45953=CARTESIAN_POINT('Ctrl Pts',(-0.604471184224974,66.3705211903455,
15.7488730727342));
#45954=CARTESIAN_POINT('Ctrl Pts',(-1.21037029596744,66.4509066517408,15.510173913772));
#45955=CARTESIAN_POINT('Ctrl Pts',(-1.47978289942527,66.4893481870635,15.3396352947398));
#45956=CARTESIAN_POINT('Ctrl Pts',(-1.93196083231809,66.5657496062255,14.9155187257816));
#45957=CARTESIAN_POINT('Ctrl Pts',(-2.11389669558551,66.6028166560054,14.6688851926677));
#45958=CARTESIAN_POINT('Ctrl Pts',(-2.31646774840565,66.6591071355653,14.2534227207639));
#45959=CARTESIAN_POINT('Ctrl Pts',(-2.37215638311095,66.678258350027,14.1049304926687));
#45960=CARTESIAN_POINT('Ctrl Pts',(-2.47102083162873,66.7243196319004,13.7390717503395));
#45961=CARTESIAN_POINT('Ctrl Pts',(-2.5,66.7511646065957,13.5197658771335));
#45962=CARTESIAN_POINT('Ctrl Pts',(-2.5,66.7778885669818,13.3));
#45963=CARTESIAN_POINT('Ctrl Pts',(-2.5,65.696789585947,13.2999999999997));
#45964=CARTESIAN_POINT('Ctrl Pts',(-2.50000000000002,65.6606212395657,13.5476917468759));
#45965=CARTESIAN_POINT('Ctrl Pts',(-2.46320526908407,65.6259776293922,13.7945024697698));
#45966=CARTESIAN_POINT('Ctrl Pts',(-2.34675403472998,65.5682504655492,14.174556274757));
#45967=CARTESIAN_POINT('Ctrl Pts',(-2.29062164953506,65.5463543672022,14.312485993215));
#45968=CARTESIAN_POINT('Ctrl Pts',(-2.09627605640216,65.4828785527232,14.6898759582726));
#45969=CARTESIAN_POINT('Ctrl Pts',(-1.93020081276959,65.4407810355203,14.9126111261388));
#45970=CARTESIAN_POINT('Ctrl Pts',(-1.48931269496749,65.3522800206411,15.33573253192));
#45971=CARTESIAN_POINT('Ctrl Pts',(-1.20330963137783,65.3075904348623,15.5168712083578));
#45972=CARTESIAN_POINT('Ctrl Pts',(-0.583806940896402,65.2139673687482,
15.7528477763624));
#45973=CARTESIAN_POINT('Ctrl Pts',(-0.257803732388431,65.1662698905148,
15.8081282301965));
#45974=CARTESIAN_POINT('Ctrl Pts',(0.347315996248517,65.0794127826204,15.7913143648248));
#45975=CARTESIAN_POINT('Ctrl Pts',(0.621957310552961,65.0419753787324,15.737324534739));
#45976=CARTESIAN_POINT('Ctrl Pts',(1.18165338917458,64.9610831563909,15.5262297058993));
#45977=CARTESIAN_POINT('Ctrl Pts',(1.45651850407446,64.9175262604713,15.3568994673308));
#45978=CARTESIAN_POINT('Ctrl Pts',(1.86865997329142,64.8391995882492,14.9780108429671));
#45979=CARTESIAN_POINT('Ctrl Pts',(2.02111302776291,64.8055394947104,14.7909051061706));
#45980=CARTESIAN_POINT('Ctrl Pts',(2.31657298205842,64.7277876819778,14.2977508391837));
#45981=CARTESIAN_POINT('Ctrl Pts',(2.42923108392718,64.6848035235328,13.978942722645));
#45982=CARTESIAN_POINT('Ctrl Pts',(2.52015281979624,64.5977656973278,13.3308689765477));
#45983=CARTESIAN_POINT('Ctrl Pts',(2.50345875413146,64.5547767687459,13.0088120080675));
#45984=CARTESIAN_POINT('Ctrl Pts',(2.35075483869388,64.4700617407981,12.392593825506));
#45985=CARTESIAN_POINT('Ctrl Pts',(2.21768277196079,64.4299216122369,12.1035926913253));
#45986=CARTESIAN_POINT('Ctrl Pts',(1.85229888222638,64.3484960718886,11.5920563535047));
#45987=CARTESIAN_POINT('Ctrl Pts',(1.62401830993652,64.3077502366141,11.3737113160013));
#45988=CARTESIAN_POINT('Ctrl Pts',(1.18147612245848,64.2381881831123,11.0863720959783));
#45989=CARTESIAN_POINT('Ctrl Pts',(0.98719503872063,64.2100366034237,10.99315893442));
#45990=CARTESIAN_POINT('Ctrl Pts',(0.638182294179026,64.1625544867496,10.8779974120894));
#45991=CARTESIAN_POINT('Ctrl Pts',(0.488894506674402,64.1430428931642,10.8435055930678));
#45992=CARTESIAN_POINT('Ctrl Pts',(0.0191928557524364,64.0825479846592,
10.7795332818075));
#45993=CARTESIAN_POINT('Ctrl Pts',(-0.304380293821025,64.0420105464618,
10.7979070045178));
#45994=CARTESIAN_POINT('Ctrl Pts',(-0.937368490865787,63.9585250257917,
10.9587286875582));
#45995=CARTESIAN_POINT('Ctrl Pts',(-1.23968286156801,63.9165679531756,11.1037644527327));
#45996=CARTESIAN_POINT('Ctrl Pts',(-1.76645161829872,63.833499977726,11.5008412785666));
#45997=CARTESIAN_POINT('Ctrl Pts',(-1.98677737394653,63.7928727123624,11.7475622274495));
#45998=CARTESIAN_POINT('Ctrl Pts',(-2.30902557930508,63.7135869421685,12.2938209223983));
#45999=CARTESIAN_POINT('Ctrl Pts',(-2.41491369294374,63.6756793594576,12.5843141463113));
#46000=CARTESIAN_POINT('Ctrl Pts',(-2.48854959505432,63.6203739294691,13.0236138047583));
#46001=CARTESIAN_POINT('Ctrl Pts',(-2.5,63.6032428589473,13.1618533917633));
#46002=CARTESIAN_POINT('Ctrl Pts',(-2.5,63.5861738118246,13.3));
#46003=CARTESIAN_POINT('Origin',(0.,70.2,13.3));
#46004=CARTESIAN_POINT('',(-2.5,61.6106677866271,13.299999999999));
#46005=CARTESIAN_POINT('',(-2.5,62.5034831341457,13.3));
#46006=CARTESIAN_POINT('',(-2.5,70.2,13.3));
#46007=CARTESIAN_POINT('',(-0.95113387948199,62.8051682013071,10.9879645736141));
#46008=CARTESIAN_POINT('Ctrl Pts',(-2.5,62.5034831341457,13.3));
#46009=CARTESIAN_POINT('Ctrl Pts',(-2.5,62.5134432259226,13.2082675133545));
#46010=CARTESIAN_POINT('Ctrl Pts',(-2.49495101965816,62.5233554399033,13.1165445974971));
#46011=CARTESIAN_POINT('Ctrl Pts',(-2.45278266979642,62.5644149407621,12.7351703849783));
#46012=CARTESIAN_POINT('Ctrl Pts',(-2.3701642172966,62.5940975669794,12.4529177587687));
#46013=CARTESIAN_POINT('Ctrl Pts',(-2.0966825207848,62.6573818047408,11.9002278508217));
#46014=CARTESIAN_POINT('Ctrl Pts',(-1.89733435958966,62.691549647966,11.6399939848498));
#46015=CARTESIAN_POINT('Ctrl Pts',(-1.4454503030277,62.7519607742206,11.2414035082826));
#46016=CARTESIAN_POINT('Ctrl Pts',(-1.20800434745213,62.7781618468012,11.0936720557263));
#46017=CARTESIAN_POINT('Ctrl Pts',(-0.951119787994485,62.8051408818796,
10.9879941287087));
#46018=CARTESIAN_POINT('Ctrl Pts',(-0.951158341752456,62.8053674325562,
10.9880099894431));
#46019=CARTESIAN_POINT('Ctrl Pts',(-0.748346167324441,62.8492893880777,
10.904572565131));
#46020=CARTESIAN_POINT('Ctrl Pts',(-0.535268424204013,62.8917771650403,
10.8481154674408));
#46021=CARTESIAN_POINT('Ctrl Pts',(-0.0889495945967942,62.9804306988286,
10.7909909524606));
#46022=CARTESIAN_POINT('Ctrl Pts',(0.142613438430281,63.0260526474146,10.7934352654522));
#46023=CARTESIAN_POINT('Ctrl Pts',(0.699104733539934,63.1294345358272,10.8768801767992));
#46024=CARTESIAN_POINT('Ctrl Pts',(1.01495953001673,63.1833347447265,10.991118965619));
#46025=CARTESIAN_POINT('Ctrl Pts',(1.54273258886205,63.290342160986,11.3123026100822));
#46026=CARTESIAN_POINT('Ctrl Pts',(1.75905112041114,63.3401990429101,11.5008112959782));
#46027=CARTESIAN_POINT('Ctrl Pts',(2.14172120523175,63.4396702711262,11.9710484837984));
#46028=CARTESIAN_POINT('Ctrl Pts',(2.29464284649186,63.4904376972501,12.2569608158226));
#46029=CARTESIAN_POINT('Ctrl Pts',(2.47662564756037,63.5890843688263,12.8478464586179));
#46030=CARTESIAN_POINT('Ctrl Pts',(2.51282222328703,63.6351455260115,13.14498589657));
#46031=CARTESIAN_POINT('Ctrl Pts',(2.47864321403863,63.7269539372175,13.7471624079164));
#46032=CARTESIAN_POINT('Ctrl Pts',(2.40535918588835,63.7738565060348,14.0469516213565));
#46033=CARTESIAN_POINT('Ctrl Pts',(2.21256971785119,63.844126463776,14.4752928707189));
#46034=CARTESIAN_POINT('Ctrl Pts',(2.13090646374222,63.8681490390869,14.6175867503245));
#46035=CARTESIAN_POINT('Ctrl Pts',(1.94168182561234,63.9163656631226,14.8831073813957));
#46036=CARTESIAN_POINT('Ctrl Pts',(1.83480669666587,63.9404276085913,15.0058259153776));
#46037=CARTESIAN_POINT('Ctrl Pts',(1.47875293674026,64.0126768939748,15.3421845921755));
#46038=CARTESIAN_POINT('Ctrl Pts',(1.19884115664813,64.0585668993632,15.5181273955644));
#46039=CARTESIAN_POINT('Ctrl Pts',(0.745927806343105,64.1282335562372,15.691304811016));
#46040=CARTESIAN_POINT('Ctrl Pts',(0.594008037624197,64.1508934864502,15.733496942561));
#46041=CARTESIAN_POINT('Ctrl Pts',(0.277723065736383,64.1966550626599,15.7899295768095));
#46042=CARTESIAN_POINT('Ctrl Pts',(0.113863356180166,64.2196131224913,15.8027837998128));
#46043=CARTESIAN_POINT('Ctrl Pts',(-0.215059461004993,64.2660254171419,
15.7961921332998));
#46044=CARTESIAN_POINT('Ctrl Pts',(-0.379294277305768,64.2893611369709,
15.7765617810483));
#46045=CARTESIAN_POINT('Ctrl Pts',(-0.857227760767255,64.3585474097511,
15.6707529771788));
#46046=CARTESIAN_POINT('Ctrl Pts',(-1.15743174475583,64.4025777893146,15.5395829385504));
#46047=CARTESIAN_POINT('Ctrl Pts',(-1.55565506513275,64.4695488243418,15.263545430248));
#46048=CARTESIAN_POINT('Ctrl Pts',(-1.67804127748925,64.4917087080322,15.1600409967452));
#46049=CARTESIAN_POINT('Ctrl Pts',(-1.90299735637489,64.5360832026101,14.9293956022825));
#46050=CARTESIAN_POINT('Ctrl Pts',(-2.00471820278112,64.5580814761814,14.8024784541755));
#46051=CARTESIAN_POINT('Ctrl Pts',(-2.26248951748846,64.6223594959449,14.4076066676219));
#46052=CARTESIAN_POINT('Ctrl Pts',(-2.38204455263811,64.6646992209118,14.11947654915));
#46053=CARTESIAN_POINT('Ctrl Pts',(-2.47995802895167,64.728787571935,13.6560923109532));
#46054=CARTESIAN_POINT('Ctrl Pts',(-2.49799735875449,64.750796444763,13.4923763989412));
#46055=CARTESIAN_POINT('Ctrl Pts',(-2.49994748911428,64.7741681509402,13.3187124487616));
#46056=CARTESIAN_POINT('Ctrl Pts',(-2.50000000001091,64.7754274660069,13.3093551141232));
#46057=CARTESIAN_POINT('Ctrl Pts',(-2.5,64.7766865736815,13.2999999970835));
#46058=CARTESIAN_POINT('',(-1.05593533999082,62.1312800345432,11.0339552088038));
#46059=CARTESIAN_POINT('Ctrl Pts',(-2.5,63.5861738118246,13.3));
#46060=CARTESIAN_POINT('Ctrl Pts',(-2.5,63.5618355279943,13.4969794410489));
#46061=CARTESIAN_POINT('Ctrl Pts',(-2.47671861934085,63.5376308222105,13.6937707697339));
#46062=CARTESIAN_POINT('Ctrl Pts',(-2.35237461690196,63.4726961590915,14.209267299241));
#46063=CARTESIAN_POINT('Ctrl Pts',(-2.21081146089628,63.4326027026238,14.5135737800926));
#46064=CARTESIAN_POINT('Ctrl Pts',(-1.83677979572786,63.3557031742944,15.0220899791508));
#46065=CARTESIAN_POINT('Ctrl Pts',(-1.61788509968431,63.3198464727878,15.2292071572241));
#46066=CARTESIAN_POINT('Ctrl Pts',(-1.23633831161108,63.2651741875956,15.4785444763662));
#46067=CARTESIAN_POINT('Ctrl Pts',(-1.09729487286071,63.2464608355503,15.5517842501154));
#46068=CARTESIAN_POINT('Ctrl Pts',(-0.65304333740367,63.1888084607364,15.7348093327135));
#46069=CARTESIAN_POINT('Ctrl Pts',(-0.332619401530084,63.1503506761926,
15.7988360913035));
#46070=CARTESIAN_POINT('Ctrl Pts',(0.149764845495188,63.0935063297738,15.8005468611102));
#46071=CARTESIAN_POINT('Ctrl Pts',(0.308094869727977,63.0749797054085,15.7860098994124));
#46072=CARTESIAN_POINT('Ctrl Pts',(0.793028183159608,63.0171521241753,15.6944185410486));
#46073=CARTESIAN_POINT('Ctrl Pts',(1.10628083734864,62.9778276726596,15.5667840736932));
#46074=CARTESIAN_POINT('Ctrl Pts',(1.6421354944158,62.9032050294953,15.2101635679604));
#46075=CARTESIAN_POINT('Ctrl Pts',(1.86528134142054,62.868495484353,14.992948509786));
#46076=CARTESIAN_POINT('Ctrl Pts',(2.22589220972072,62.796441996323,14.4814847880212));
#46077=CARTESIAN_POINT('Ctrl Pts',(2.35766988115371,62.7602485560122,14.18993062246));
#46078=CARTESIAN_POINT('Ctrl Pts',(2.46841211352946,62.7069325753515,13.7268655699382));
#46079=CARTESIAN_POINT('Ctrl Pts',(2.49055727223028,62.6893607887676,13.5690734070085));
#46080=CARTESIAN_POINT('Ctrl Pts',(2.51231105272378,62.6345021586197,13.0762421278448));
#46081=CARTESIAN_POINT('Ctrl Pts',(2.4599096092195,62.596869803934,12.7426248548224));
#46082=CARTESIAN_POINT('Ctrl Pts',(2.23536643917119,62.5263208200567,12.1383733469182));
#46083=CARTESIAN_POINT('Ctrl Pts',(2.07411883505748,62.4938036036167,11.8702147044956));
#46084=CARTESIAN_POINT('Ctrl Pts',(1.66115536010345,62.4262744560102,11.4059731185847));
#46085=CARTESIAN_POINT('Ctrl Pts',(1.4127414065054,62.3927876344703,11.2140810921841));
#46086=CARTESIAN_POINT('Ctrl Pts',(0.994382633338479,62.3440182625655,11.0008126638597));
#46087=CARTESIAN_POINT('Ctrl Pts',(0.846837094673137,62.3278983183272,10.9424737002965));
#46088=CARTESIAN_POINT('Ctrl Pts',(0.384509880431944,62.278476354872,10.8087226587651));
#46089=CARTESIAN_POINT('Ctrl Pts',(0.059763906012211,62.2444794544955,10.7799212919263));
#46090=CARTESIAN_POINT('Ctrl Pts',(-0.536687791893848,62.1843125767197,
10.8426602317689));
#46091=CARTESIAN_POINT('Ctrl Pts',(-0.80512551759084,62.1581728462725,10.9170737303865));
#46092=CARTESIAN_POINT('Ctrl Pts',(-1.0559353435001,62.1312734393566,11.0339460398421));
#46093=CARTESIAN_POINT('Ctrl Pts',(-1.05588007528467,62.1309604529623,11.0339202867911));
#46094=CARTESIAN_POINT('Ctrl Pts',(-1.28187597354016,62.0803724841633,11.1392230988119));
#46095=CARTESIAN_POINT('Ctrl Pts',(-1.49124228115003,62.031193003458,11.2779710600194));
#46096=CARTESIAN_POINT('Ctrl Pts',(-1.90685064701863,61.9225543060576,11.6536992054081));
#46097=CARTESIAN_POINT('Ctrl Pts',(-2.09635136197059,61.8672490886137,11.902875871808));
#46098=CARTESIAN_POINT('Ctrl Pts',(-2.36481197668388,61.7591668280173,12.4391365608076));
#46099=CARTESIAN_POINT('Ctrl Pts',(-2.44852088510863,61.7086069741114,12.7181463211823));
#46100=CARTESIAN_POINT('Ctrl Pts',(-2.4942115345676,61.6434985370641,13.1034831108955));
#46101=CARTESIAN_POINT('Ctrl Pts',(-2.49999999999992,61.6270837917359,13.2017877758211));
#46102=CARTESIAN_POINT('Ctrl Pts',(-2.5,61.6106677866271,13.299999999998));
#46103=CARTESIAN_POINT('Origin',(0.,70.2,13.3));
#46104=CARTESIAN_POINT('',(-2.5,59.3994433450696,13.3));
#46105=CARTESIAN_POINT('',(-2.50005097985869,60.6167707974153,13.3003061727703));
#46106=CARTESIAN_POINT('',(-2.5,70.2,13.3));
#46107=CARTESIAN_POINT('Ctrl Pts',(-2.49999998106492,60.6167825252036,13.3003076936568));
#46108=CARTESIAN_POINT('Ctrl Pts',(-2.50003167432271,60.6503069125688,13.0428011051694));
#46109=CARTESIAN_POINT('Ctrl Pts',(-2.46027730575809,60.6836579553173,12.786819843935));
#46110=CARTESIAN_POINT('Ctrl Pts',(-2.29644321278257,60.7536512825819,12.2723264854255));
#46111=CARTESIAN_POINT('Ctrl Pts',(-2.16575661142914,60.7895694189813,12.0196521562626));
#46112=CARTESIAN_POINT('Ctrl Pts',(-1.89997952644266,60.8460870435028,11.6674296411658));
#46113=CARTESIAN_POINT('Ctrl Pts',(-1.79248929773588,60.8663775023704,11.5500881844077));
#46114=CARTESIAN_POINT('Ctrl Pts',(-1.43354632066325,60.9282128096194,11.2262737701675));
#46115=CARTESIAN_POINT('Ctrl Pts',(-1.15240914753211,60.9691002371946,11.0578176679183));
#46116=CARTESIAN_POINT('Ctrl Pts',(-0.555685804014866,61.0493877044964,
10.8429651857453));
#46117=CARTESIAN_POINT('Ctrl Pts',(-0.247484298851549,61.0881331015775,
10.7930928430669));
#46118=CARTESIAN_POINT('Ctrl Pts',(0.231228210956693,61.1482337357571,10.8049662505859));
#46119=CARTESIAN_POINT('Ctrl Pts',(0.399612079283944,61.1693637168444,10.826343877124));
#46120=CARTESIAN_POINT('Ctrl Pts',(0.862306460298472,61.2286679117027,10.9335989626459));
#46121=CARTESIAN_POINT('Ctrl Pts',(1.14491670061985,61.2663615499773,11.0566516905333));
#46122=CARTESIAN_POINT('Ctrl Pts',(1.53566880802269,61.3248000057025,11.3203091326199));
#46123=CARTESIAN_POINT('Ctrl Pts',(1.66347295866566,61.3452538209656,11.4264160646674));
#46124=CARTESIAN_POINT('Ctrl Pts',(2.0142493549841,61.4068455850894,11.7820336132132));
#46125=CARTESIAN_POINT('Ctrl Pts',(2.19872426078175,61.4472436498982,12.0642538241026));
#46126=CARTESIAN_POINT('Ctrl Pts',(2.37977989143596,61.5068727069176,12.5185127945139));
#46127=CARTESIAN_POINT('Ctrl Pts',(2.42368541458096,61.5257723766018,12.6676831439235));
#46128=CARTESIAN_POINT('Ctrl Pts',(2.51698705120129,61.5849334691689,13.1445457620724));
#46129=CARTESIAN_POINT('Ctrl Pts',(2.51546320204714,61.6244248978137,13.4785687636092));
#46130=CARTESIAN_POINT('Ctrl Pts',(2.38421848069762,61.7025293376362,14.1180243412869));
#46131=CARTESIAN_POINT('Ctrl Pts',(2.25916099771928,61.7408909013013,14.4179751268707));
#46132=CARTESIAN_POINT('Ctrl Pts',(1.91668378618502,61.8144096986113,14.9321171412022));
#46133=CARTESIAN_POINT('Ctrl Pts',(1.71030723496061,61.8487793672088,15.1472590005306));
#46134=CARTESIAN_POINT('Ctrl Pts',(1.20040881389063,61.9226347869468,15.5183592177604));
#46135=CARTESIAN_POINT('Ctrl Pts',(0.892840490250037,61.96191338326,15.6590194630925));
#46136=CARTESIAN_POINT('Ctrl Pts',(0.262417594039295,62.0368102437113,15.8057398815962));
#46137=CARTESIAN_POINT('Ctrl Pts',(-0.0524529815479305,62.0718865390332,
15.8188997708182));
#46138=CARTESIAN_POINT('Ctrl Pts',(-0.671634931442725,62.1439398580234,
15.7283921689737));
#46139=CARTESIAN_POINT('Ctrl Pts',(-0.970482295014021,62.1796355811393,
15.6251724561424));
#46140=CARTESIAN_POINT('Ctrl Pts',(-1.38124944674192,62.232582959014,15.3899086427978));
#46141=CARTESIAN_POINT('Ctrl Pts',(-1.51206128228296,62.250243219615,15.2973084796327));
#46142=CARTESIAN_POINT('Ctrl Pts',(-1.88618394378343,62.3052287457407,14.9745185526001));
#46143=CARTESIAN_POINT('Ctrl Pts',(-2.09292902595285,62.3428443665707,14.7076243431039));
#46144=CARTESIAN_POINT('Ctrl Pts',(-2.37990882752752,62.4136135517456,14.1271384734215));
#46145=CARTESIAN_POINT('Ctrl Pts',(-2.46472935062807,62.446468573607,13.8227282112553));
#46146=CARTESIAN_POINT('Ctrl Pts',(-2.49703912277934,62.4882012010445,13.4405024502384));
#46147=CARTESIAN_POINT('Ctrl Pts',(-2.5,62.4958557361002,13.3702483676872));
#46148=CARTESIAN_POINT('Ctrl Pts',(-2.5,62.5034831341457,13.3));
#46149=CARTESIAN_POINT('Ctrl Pts',(-2.5,61.6106677866271,13.2999999999979));
#46150=CARTESIAN_POINT('Ctrl Pts',(-2.50000000000017,61.5753977216309,13.5110106269549));
#46151=CARTESIAN_POINT('Ctrl Pts',(-2.47328881942191,61.5399743614456,13.7215699957689));
#46152=CARTESIAN_POINT('Ctrl Pts',(-2.34086749087818,61.4536198113013,14.2329923829222));
#46153=CARTESIAN_POINT('Ctrl Pts',(-2.20399523672876,61.4032180149517,14.5217670579512));
#46154=CARTESIAN_POINT('Ctrl Pts',(-1.83146316933345,61.3029540924801,15.0303651257921));
#46155=CARTESIAN_POINT('Ctrl Pts',(-1.60020023359404,61.2571020417161,15.2462503961835));
#46156=CARTESIAN_POINT('Ctrl Pts',(-1.07677625810136,61.1639043490878,15.5767667070598));
#46157=CARTESIAN_POINT('Ctrl Pts',(-0.791217250734542,61.1166318477133,
15.6910244293695));
#46158=CARTESIAN_POINT('Ctrl Pts',(-0.162002177805606,61.0205089410304,
15.8173747927169));
#46159=CARTESIAN_POINT('Ctrl Pts',(0.178249166057133,60.9738822900553,15.8163040584398));
#46160=CARTESIAN_POINT('Ctrl Pts',(0.661210841276149,60.9016095528027,15.716034411891));
#46161=CARTESIAN_POINT('Ctrl Pts',(0.810899553950083,60.8784850141691,15.66999065206));
#46162=CARTESIAN_POINT('Ctrl Pts',(1.2338256231954,60.8110986230562,15.4951128133702));
#46163=CARTESIAN_POINT('Ctrl Pts',(1.48928700482673,60.7690305034994,15.330514957981));
#46164=CARTESIAN_POINT('Ctrl Pts',(1.94055110680696,60.6820145210843,14.9076771002005));
#46165=CARTESIAN_POINT('Ctrl Pts',(2.12846386403743,60.6375835412521,14.6490782544425));
#46166=CARTESIAN_POINT('Ctrl Pts',(2.40528866024503,60.5466316330392,14.0593351017857));
#46167=CARTESIAN_POINT('Ctrl Pts',(2.48523782949149,60.5013429511135,13.730853322367));
#46168=CARTESIAN_POINT('Ctrl Pts',(2.5107276025244,60.4097155920456,13.0701376918266));
#46169=CARTESIAN_POINT('Ctrl Pts',(2.45928938940062,60.3658637000904,12.7445343508971));
#46170=CARTESIAN_POINT('Ctrl Pts',(2.29143638730971,60.299482163651,12.2875788530185));
#46171=CARTESIAN_POINT('Ctrl Pts',(2.22185050580503,60.277588760923,12.1428227299824));
#46172=CARTESIAN_POINT('Ctrl Pts',(1.96568075416499,60.2103221284824,11.7194831123215));
#46173=CARTESIAN_POINT('Ctrl Pts',(1.73674823198205,60.1661649256645,11.4708829128064));
#46174=CARTESIAN_POINT('Ctrl Pts',(1.20107551719154,60.0770022268735,11.0832234339517));
#46175=CARTESIAN_POINT('Ctrl Pts',(0.901469739307313,60.0340434543022,10.9454136203066));
#46176=CARTESIAN_POINT('Ctrl Pts',(0.286501669427965,59.9498332087379,10.7977189146826));
#46177=CARTESIAN_POINT('Ctrl Pts',(-0.0214358916469852,59.9093592186135,
10.7814543511458));
#46178=CARTESIAN_POINT('Ctrl Pts',(-0.639429444520793,59.8273145602628,
10.8623987714831));
#46179=CARTESIAN_POINT('Ctrl Pts',(-0.943485454479146,59.7856405535461,
10.9632049556967));
#46180=CARTESIAN_POINT('Ctrl Pts',(-1.36462591161955,59.722341325843,11.1987964870087));
#46181=CARTESIAN_POINT('Ctrl Pts',(-1.50038760761804,59.7008903977335,11.2934850410936));
#46182=CARTESIAN_POINT('Ctrl Pts',(-1.7495610949226,59.6580734504445,11.5067993877266));
#46183=CARTESIAN_POINT('Ctrl Pts',(-1.86264971926353,59.6368153223749,11.6245694910179));
#46184=CARTESIAN_POINT('Ctrl Pts',(-2.17060216608482,59.5718096871366,12.0153003709833));
#46185=CARTESIAN_POINT('Ctrl Pts',(-2.32288678666953,59.5290983426027,12.3170477084673));
#46186=CARTESIAN_POINT('Ctrl Pts',(-2.45341481384624,59.4651200924951,12.7937991660323));
#46187=CARTESIAN_POINT('Ctrl Pts',(-2.48072617625929,59.4444711572715,12.9514556000494));
#46188=CARTESIAN_POINT('Ctrl Pts',(-2.49761161611624,59.4156963943897,13.1737417293526));
#46189=CARTESIAN_POINT('Ctrl Pts',(-2.5,59.4075609409309,13.2369073430154));
#46190=CARTESIAN_POINT('Ctrl Pts',(-2.5,59.3994433450696,13.3));
#46191=CARTESIAN_POINT('Origin',(0.,70.2,13.3));
#46192=CARTESIAN_POINT('',(-2.5,57.4769927816046,13.3));
#46193=CARTESIAN_POINT('',(-2.49999999761251,58.4092448555943,13.3001092586366));
#46194=CARTESIAN_POINT('',(-2.5,70.2,13.3));
#46195=CARTESIAN_POINT('',(-1.71831766398917,58.6398093087261,11.4856494580447));
#46196=CARTESIAN_POINT('Ctrl Pts',(-2.5,58.4092574955175,13.3000000000002));
#46197=CARTESIAN_POINT('Ctrl Pts',(-2.5,58.4285081348677,13.1335985253904));
#46198=CARTESIAN_POINT('Ctrl Pts',(-2.48338644354128,58.4475613350895,12.9676028553435));
#46199=CARTESIAN_POINT('Ctrl Pts',(-2.41623371863719,58.4863852419782,12.6355231449167));
#46200=CARTESIAN_POINT('Ctrl Pts',(-2.36468214575892,58.5061348190271,12.4705448459811));
#46201=CARTESIAN_POINT('Ctrl Pts',(-2.22765497520508,58.5457343700435,12.1519709352431));
#46202=CARTESIAN_POINT('Ctrl Pts',(-2.14215917281841,58.5654413971552,11.9993906346628));
#46203=CARTESIAN_POINT('Ctrl Pts',(-1.94650672128539,58.6034839248316,11.722604870779));
#46204=CARTESIAN_POINT('Ctrl Pts',(-1.83851610981518,58.6217439894937,11.5979641222271));
#46205=CARTESIAN_POINT('Ctrl Pts',(-1.71906196354253,58.64008093262,11.4848344523154));
#46206=CARTESIAN_POINT('Ctrl Pts',(-1.71827827352178,58.6398165637634,11.4856099157301));
#46207=CARTESIAN_POINT('Ctrl Pts',(-1.67168277133379,58.6506632299144,11.4415863705764));
#46208=CARTESIAN_POINT('Ctrl Pts',(-1.62358535300898,58.6613329356252,11.3993011150436));
#46209=CARTESIAN_POINT('Ctrl Pts',(-1.5740109869715,58.6720612790877,11.3589698018563));
#46210=CARTESIAN_POINT('Ctrl Pts',(-1.55542295036543,58.6760838991824,11.343847471793));
#46211=CARTESIAN_POINT('Ctrl Pts',(-1.53662750959264,58.6801146947408,11.3290003063795));
#46212=CARTESIAN_POINT('Ctrl Pts',(-1.51762695332325,58.6841658372305,11.3144412813472));
#46213=CARTESIAN_POINT('Ctrl Pts',(-1.44725522850215,58.6991699181874,11.2605195072315));
#46214=CARTESIAN_POINT('Ctrl Pts',(-1.37420002501608,58.7141619361767,11.2103505537322));
#46215=CARTESIAN_POINT('Ctrl Pts',(-1.2987892723116,58.7291444985975,11.1641594431883));
#46216=CARTESIAN_POINT('Ctrl Pts',(-1.22407694124179,58.7439882990333,11.1183961346458));
#46217=CARTESIAN_POINT('Ctrl Pts',(-1.14705267636555,58.7588225370595,11.076536897693));
#46218=CARTESIAN_POINT('Ctrl Pts',(-1.06800390276438,58.7736204504448,11.0388066892096));
#46219=CARTESIAN_POINT('Ctrl Pts',(-1.0053145409205,58.7853558854742,11.008884875318));
#46220=CARTESIAN_POINT('Ctrl Pts',(-0.941351322191961,58.7970678425373,
10.9815597990238));
#46221=CARTESIAN_POINT('Ctrl Pts',(-0.876242310501115,58.8087316248811,
10.9569505145643));
#46222=CARTESIAN_POINT('Ctrl Pts',(-0.800964081422921,58.8222171448789,
10.9284975661185));
#46223=CARTESIAN_POINT('Ctrl Pts',(-0.724519456047828,58.8355729945648,
10.9038121138826));
#46224=CARTESIAN_POINT('Ctrl Pts',(-0.647114574550911,58.8487502606411,
10.8829842087397));
#46225=CARTESIAN_POINT('Ctrl Pts',(-0.639468270488092,58.8500519535213,
10.8809267610357));
#46226=CARTESIAN_POINT('Ctrl Pts',(-0.631812560411286,58.8513519060032,
10.8789069777978));
#46227=CARTESIAN_POINT('Ctrl Pts',(-0.624147619917967,58.8526500724191,
10.8769249611432));
#46228=CARTESIAN_POINT('Ctrl Pts',(-0.587811188157204,58.8588041626469,
10.8675290091486));
#46229=CARTESIAN_POINT('Ctrl Pts',(-0.551267549895413,58.8649179004233,
10.8589815057862));
#46230=CARTESIAN_POINT('Ctrl Pts',(-0.514534554199861,58.8709857720265,
10.8512937498166));
#46231=CARTESIAN_POINT('Ctrl Pts',(-0.514459951384814,58.87099809556,10.8512781363817));
#46232=CARTESIAN_POINT('Ctrl Pts',(-0.514385347791356,58.8710104189047,
10.8512625264951));
#46233=CARTESIAN_POINT('Ctrl Pts',(-0.514310743419481,58.8710227420607,
10.8512469201572));
#46234=CARTESIAN_POINT('Ctrl Pts',(-0.430731462675848,58.8848283742604,
10.8337631391232));
#46235=CARTESIAN_POINT('Ctrl Pts',(-0.346173773906837,58.8983975898941,
10.8207279432178));
#46236=CARTESIAN_POINT('Ctrl Pts',(-0.260978977584018,58.911854953297,10.8121073648089));
#46237=CARTESIAN_POINT('Ctrl Pts',(-0.178135598296444,58.9249408870479,
10.8037247184781));
#46238=CARTESIAN_POINT('Ctrl Pts',(-0.094689111867007,58.9379215364864,
10.7995176207406));
#46239=CARTESIAN_POINT('Ctrl Pts',(-0.0109716505076562,58.950890909248,
10.799488647867));
#46240=CARTESIAN_POINT('Ctrl Pts',(-0.00631521864721163,58.9516122760878,
10.7994870363727));
#46241=CARTESIAN_POINT('Ctrl Pts',(-0.00165795546027684,58.9523336071144,
10.7994983620118));
#46242=CARTESIAN_POINT('Ctrl Pts',(0.00300007929513795,58.9530549181748,
10.7995226291543));
#46243=CARTESIAN_POINT('Ctrl Pts',(0.0364730885342065,58.9582383169807,
10.7996970147757));
#46244=CARTESIAN_POINT('Ctrl Pts',(0.0699860464254556,58.9634204505794,
10.8005393829189));
#46245=CARTESIAN_POINT('Ctrl Pts',(0.103516510062052,58.9686061984143,10.8020510141029));
#46246=CARTESIAN_POINT('Ctrl Pts',(0.191067906454456,58.9821467050178,10.8059980344132));
#46247=CARTESIAN_POINT('Ctrl Pts',(0.278280705036573,58.9956442394026,10.814486745742));
#46248=CARTESIAN_POINT('Ctrl Pts',(0.36475353336839,59.0091613741268,10.8274087422704));
#46249=CARTESIAN_POINT('Ctrl Pts',(0.452514906646568,59.0228799297594,10.8405232914613));
#46250=CARTESIAN_POINT('Ctrl Pts',(0.53951370060598,59.036618702049,10.8582045625988));
#46251=CARTESIAN_POINT('Ctrl Pts',(0.625334894065203,59.0504062987958,10.8803525144015));
#46252=CARTESIAN_POINT('Ctrl Pts',(0.711016321799679,59.0641714414916,10.9024643967393));
#46253=CARTESIAN_POINT('Ctrl Pts',(0.795523583189255,59.077985064378,10.9290282286279));
#46254=CARTESIAN_POINT('Ctrl Pts',(0.878454469038144,59.0918405742896,10.959956495412));
#46255=CARTESIAN_POINT('Ctrl Pts',(0.943779983616589,59.1027547024272,10.9843190103184));
#46256=CARTESIAN_POINT('Ctrl Pts',(1.00812761085416,59.113694076328,11.011389659825));
#46257=CARTESIAN_POINT('Ctrl Pts',(1.07130720503626,59.124641521194,11.0411336050755));
#46258=CARTESIAN_POINT('Ctrl Pts',(1.14502710516054,59.1374153376861,11.0758397582497));
#46259=CARTESIAN_POINT('Ctrl Pts',(1.21679595895508,59.1501382469946,11.1140152441909));
#46260=CARTESIAN_POINT('Ctrl Pts',(1.28638304892513,59.1627657238264,11.1555235388176));
#46261=CARTESIAN_POINT('Ctrl Pts',(1.2927845440097,59.1639273578436,11.1593419934208));
#46262=CARTESIAN_POINT('Ctrl Pts',(1.29916758597747,59.1650881863615,11.1631886872241));
#46263=CARTESIAN_POINT('Ctrl Pts',(1.30553200080499,59.166248176004,11.1670635353192));
#46264=CARTESIAN_POINT('Ctrl Pts',(1.37291006161506,59.1785286220133,11.2080853350687));
#46265=CARTESIAN_POINT('Ctrl Pts',(1.43820025096216,59.1907143811178,11.25225816944));
#46266=CARTESIAN_POINT('Ctrl Pts',(1.50121024247637,59.2027530099914,11.2994955979673));
#46267=CARTESIAN_POINT('Ctrl Pts',(1.50839977487922,59.2041266351943,11.3048854578112));
#46268=CARTESIAN_POINT('Ctrl Pts',(1.5155596272048,59.2054983486907,11.3103152715227));
#46269=CARTESIAN_POINT('Ctrl Pts',(1.52268951705691,59.206868075529,11.3157849541186));
#46270=CARTESIAN_POINT('Ctrl Pts',(1.53622473082987,59.2094683324685,11.3261684698169));
#46271=CARTESIAN_POINT('Ctrl Pts',(1.54965199117437,59.2120613804525,11.3366956126132));
#46272=CARTESIAN_POINT('Ctrl Pts',(1.56296939946788,59.2146466487011,11.3473658306531));
#46273=CARTESIAN_POINT('Ctrl Pts',(1.56300888168497,59.2146543132646,11.347397464726));
#46274=CARTESIAN_POINT('Ctrl Pts',(1.56304836293562,59.21466197776,11.3474291000564));
#46275=CARTESIAN_POINT('Ctrl Pts',(1.5630878432197,59.2146696421874,11.3474607366442));
#46276=CARTESIAN_POINT('Ctrl Pts',(1.62498333468977,59.2266856017106,11.3970592184399));
#46277=CARTESIAN_POINT('Ctrl Pts',(1.68450744753681,59.2385345056002,11.4497473619077));
#46278=CARTESIAN_POINT('Ctrl Pts',(1.74149536111069,59.2503104816428,11.5053325961441));
#46279=CARTESIAN_POINT('Ctrl Pts',(1.74713357180979,59.2514755608666,11.5108320300193));
#46280=CARTESIAN_POINT('Ctrl Pts',(1.75274691561814,59.2526399229283,11.5163598294427));
#46281=CARTESIAN_POINT('Ctrl Pts',(1.75833520571778,59.2538036567991,11.5219158116712));
#46282=CARTESIAN_POINT('Ctrl Pts',(1.79515167104113,59.2614705042492,11.5585194280552));
#46283=CARTESIAN_POINT('Ctrl Pts',(1.83088173082515,59.2691099214016,11.5963461675733));
#46284=CARTESIAN_POINT('Ctrl Pts',(1.86546985158908,59.2767442297419,11.6353424213068));
#46285=CARTESIAN_POINT('Ctrl Pts',(1.92317617836415,59.2894812007614,11.7004032141815));
#46286=CARTESIAN_POINT('Ctrl Pts',(1.97740579089471,59.3021394830516,11.7683814677034));
#46287=CARTESIAN_POINT('Ctrl Pts',(2.02797839793939,59.3148007611641,11.8389300574549));
#46288=CARTESIAN_POINT('Ctrl Pts',(2.07947086483033,59.3276923339364,11.9107618481074));
#46289=CARTESIAN_POINT('Ctrl Pts',(2.12717125216542,59.3405871608286,11.9852585855909));
#46290=CARTESIAN_POINT('Ctrl Pts',(2.17087373687153,59.3535372860957,12.0620537631012));
#46291=CARTESIAN_POINT('Ctrl Pts',(2.21483013926339,59.3665626534425,12.1392951315749));
#46292=CARTESIAN_POINT('Ctrl Pts',(2.25474142351539,59.3796439165231,12.2188614005462));
#46293=CARTESIAN_POINT('Ctrl Pts',(2.29039399640346,59.3927990942328,12.300380149045));
#46294=CARTESIAN_POINT('Ctrl Pts',(2.31841991380376,59.4031401690561,12.3644607336126));
#46295=CARTESIAN_POINT('Ctrl Pts',(2.34381422166481,59.4135261815954,12.429747660825));
#46296=CARTESIAN_POINT('Ctrl Pts',(2.36647381168078,59.4239515112605,12.4960633986888));
#46297=CARTESIAN_POINT('Ctrl Pts',(2.39355470089487,59.4364110128439,12.5753185462432));
#46298=CARTESIAN_POINT('Ctrl Pts',(2.41659439458519,59.448864999823,12.6556462291611));
#46299=CARTESIAN_POINT('Ctrl Pts',(2.43554026660505,59.4612821491933,12.7367302669068));
#46300=CARTESIAN_POINT('Ctrl Pts',(2.43677049553403,59.4620884428468,12.7419953678643));
#46301=CARTESIAN_POINT('Ctrl Pts',(2.43798345428773,59.462894582159,12.7472636737242));
#46302=CARTESIAN_POINT('Ctrl Pts',(2.4391791245498,59.4637005589631,12.7525351043601));
#46303=CARTESIAN_POINT('Ctrl Pts',(2.45699519767812,59.4757100085065,12.8310820053568));
#46304=CARTESIAN_POINT('Ctrl Pts',(2.47097570716193,59.4876827505012,12.9103191771994));
#46305=CARTESIAN_POINT('Ctrl Pts',(2.48106971641073,59.4995755236576,12.9900022613495));
#46306=CARTESIAN_POINT('Ctrl Pts',(2.48200456958852,59.500676968733,12.9973820826473));
#46307=CARTESIAN_POINT('Ctrl Pts',(2.48290606404071,59.5017777304834,13.0047657580969));
#46308=CARTESIAN_POINT('Ctrl Pts',(2.48377414493789,59.5028777761427,13.012153111169));
#46309=CARTESIAN_POINT('Ctrl Pts',(2.49281344617476,59.5143325197286,13.0890774047206));
#46310=CARTESIAN_POINT('Ctrl Pts',(2.49823326059392,59.5257089156831,13.1663976070584));
#46311=CARTESIAN_POINT('Ctrl Pts',(2.49996888262786,59.5369602010634,13.2439331579682));
#46312=CARTESIAN_POINT('Ctrl Pts',(2.50014131000419,59.5380779730095,13.2516360168595));
#46313=CARTESIAN_POINT('Ctrl Pts',(2.50027734442346,59.539194513445,13.2593410299962));
#46314=CARTESIAN_POINT('Ctrl Pts',(2.50037690087323,59.5403097787046,13.2670480389967));
#46315=CARTESIAN_POINT('Ctrl Pts',(2.50037737123612,59.5403150478698,13.2670844514136));
#46316=CARTESIAN_POINT('Ctrl Pts',(2.50037784078482,59.5403203170064,13.2671208638747));
#46317=CARTESIAN_POINT('Ctrl Pts',(2.50037830951934,59.5403255861145,13.2671572763801));
#46318=CARTESIAN_POINT('Ctrl Pts',(2.50128601740068,59.550529253138,13.3376703644645));
#46319=CARTESIAN_POINT('Ctrl Pts',(2.49914256466633,59.5606260739844,13.408351690911));
#46320=CARTESIAN_POINT('Ctrl Pts',(2.49395012281287,59.5706793582291,13.4790286814146));
#46321=CARTESIAN_POINT('Ctrl Pts',(2.48764039382557,59.5828958646063,13.5649136404185));
#46322=CARTESIAN_POINT('Ctrl Pts',(2.47686026899674,59.5949868619463,13.6503509074918));
#46323=CARTESIAN_POINT('Ctrl Pts',(2.46172657029248,59.6070473770885,13.7350019088095));
#46324=CARTESIAN_POINT('Ctrl Pts',(2.44627835339879,59.6193585415571,13.8214121812868));
#46325=CARTESIAN_POINT('Ctrl Pts',(2.42629251947667,59.6316381721857,13.907002805738));
#46326=CARTESIAN_POINT('Ctrl Pts',(2.40188227406564,59.6439566260316,13.9913867545134));
#46327=CARTESIAN_POINT('Ctrl Pts',(2.37717338292673,59.6564257892846,14.0768030938027));
#46328=CARTESIAN_POINT('Ctrl Pts',(2.34793048083732,59.6689348013427,14.160982229526));
#46329=CARTESIAN_POINT('Ctrl Pts',(2.31427441934883,59.68152324342,14.2435047244255));
#46330=CARTESIAN_POINT('Ctrl Pts',(2.28751075741139,59.6915337079002,14.3091274995824));
#46331=CARTESIAN_POINT('Ctrl Pts',(2.25795655633981,59.7015937118674,14.3737021478923));
#46332=CARTESIAN_POINT('Ctrl Pts',(2.22567631510524,59.7117083510003,14.4370154482916));
#46333=CARTESIAN_POINT('Ctrl Pts',(2.18511903193608,59.7244165052079,14.5165630400834));
#46334=CARTESIAN_POINT('Ctrl Pts',(2.14047539887216,59.7371441213632,14.5936941839776));
#46335=CARTESIAN_POINT('Ctrl Pts',(2.0920013610226,59.749873529981,14.6680773519142));
#46336=CARTESIAN_POINT('Ctrl Pts',(2.04685992951998,59.7617277874903,14.7373466521275));
#46337=CARTESIAN_POINT('Ctrl Pts',(1.99839712194163,59.7735832333912,14.8042330946931));
#46338=CARTESIAN_POINT('Ctrl Pts',(1.94679834215026,59.7854074525574,14.8685006188011));
#46339=CARTESIAN_POINT('Ctrl Pts',(1.94297012406212,59.7862847153506,14.8732687567157));
#46340=CARTESIAN_POINT('Ctrl Pts',(1.93912462063216,59.7871618079109,14.8780224820268));
#46341=CARTESIAN_POINT('Ctrl Pts',(1.93526189621512,59.7880387177967,14.8827616994595));
#46342=CARTESIAN_POINT('Ctrl Pts',(1.88543794211375,59.7993496768976,14.9438912355979));
#46343=CARTESIAN_POINT('Ctrl Pts',(1.83275345257738,59.8106295757333,15.0026072895304));
#46344=CARTESIAN_POINT('Ctrl Pts',(1.77733724064179,59.8218393754625,15.0587248540365));
#46345=CARTESIAN_POINT('Ctrl Pts',(1.77189331698259,59.8229405928108,15.064237676484));
#46346=CARTESIAN_POINT('Ctrl Pts',(1.76642298929319,59.8240411370812,15.0697254218942));
#46347=CARTESIAN_POINT('Ctrl Pts',(1.76092635230643,59.8251409735031,15.0751879137462));
#46348=CARTESIAN_POINT('Ctrl Pts',(1.71347422013327,59.834635794316,15.1223452730516));
#46349=CARTESIAN_POINT('Ctrl Pts',(1.66406433723682,59.8440772105526,15.1676214971317));
#46350=CARTESIAN_POINT('Ctrl Pts',(1.61274763941038,59.8534385124002,15.2109084390397));
#46351=CARTESIAN_POINT('Ctrl Pts',(1.61271278144252,59.8534448712653,15.2109378426236));
#46352=CARTESIAN_POINT('Ctrl Pts',(1.612677922594,59.8534512300934,15.2109672452895));
#46353=CARTESIAN_POINT('Ctrl Pts',(1.6126430628648,59.8534575888844,15.2109966470373));
#46354=CARTESIAN_POINT('Ctrl Pts',(1.61148134785781,59.853669498245,15.2119764725392));
#46355=CARTESIAN_POINT('Ctrl Pts',(1.61031865478613,59.8538813664654,15.2129552784351));
#46356=CARTESIAN_POINT('Ctrl Pts',(1.60915498477109,59.8540931941773,15.2139330635866));
#46357=CARTESIAN_POINT('Ctrl Pts',(1.55020696078019,59.864823749129,15.2634647193182));
#46358=CARTESIAN_POINT('Ctrl Pts',(1.48902325362349,59.8754021982025,15.3101515096413));
#46359=CARTESIAN_POINT('Ctrl Pts',(1.42581404612227,59.8859070487761,15.353905724036));
#46360=CARTESIAN_POINT('Ctrl Pts',(1.41912316332405,59.887019018484,15.3585372378932));
#46361=CARTESIAN_POINT('Ctrl Pts',(1.41240958468812,59.8881301587286,15.3631358449879));
#46362=CARTESIAN_POINT('Ctrl Pts',(1.40567356052368,59.8892405592113,15.3677014078902));
#46363=CARTESIAN_POINT('Ctrl Pts',(1.33883089404637,59.9002592443159,15.4130062332463));
#46364=CARTESIAN_POINT('Ctrl Pts',(1.26977717227794,59.9112058480364,15.4550610497965));
#46365=CARTESIAN_POINT('Ctrl Pts',(1.19877265293406,59.922150181128,15.4937272790274));
#46366=CARTESIAN_POINT('Ctrl Pts',(1.19324757079086,59.9230017936717,15.4967360183956));
#46367=CARTESIAN_POINT('Ctrl Pts',(1.18771068101699,59.9238533899401,15.4997242146752));
#46368=CARTESIAN_POINT('Ctrl Pts',(1.1821621088393,59.9247050015428,15.5026917897785));
#46369=CARTESIAN_POINT('Ctrl Pts',(1.10377082825718,59.9367367318624,15.5446182539426));
#46370=CARTESIAN_POINT('Ctrl Pts',(1.02304627281204,59.9487723007819,15.5824329766345));
#46371=CARTESIAN_POINT('Ctrl Pts',(0.940367691462049,59.9608733853385,15.6159261158047));
#46372=CARTESIAN_POINT('Ctrl Pts',(0.870834804575598,59.971050426719,15.6440939268552));
#46373=CARTESIAN_POINT('Ctrl Pts',(0.79992069165266,59.9812732470463,15.6692043885178));
#46374=CARTESIAN_POINT('Ctrl Pts',(0.727868067876903,59.9915612181891,15.6911316846438));
#46375=CARTESIAN_POINT('Ctrl Pts',(0.642453056742453,60.0037571261751,15.7171254673072));
#46376=CARTESIAN_POINT('Ctrl Pts',(0.555895002218752,60.0159802616778,15.7385065701487));
#46377=CARTESIAN_POINT('Ctrl Pts',(0.468642151115674,60.0282337224108,15.7552261443502));
#46378=CARTESIAN_POINT('Ctrl Pts',(0.38094541171423,60.0405495211393,15.7720307773577));
#46379=CARTESIAN_POINT('Ctrl Pts',(0.292548020977324,60.052895543025,15.7841268590937));
#46380=CARTESIAN_POINT('Ctrl Pts',(0.203871504215768,60.0652501800661,15.7914861794489));
#46381=CARTESIAN_POINT('Ctrl Pts',(0.122822309657222,60.0765421592486,15.798212503498));
#46382=CARTESIAN_POINT('Ctrl Pts',(0.0415400858558959,60.0878409708304,
15.8009825371921));
#46383=CARTESIAN_POINT('Ctrl Pts',(-0.039689640861549,60.0991162829269,
15.7997813431565));
#46384=CARTESIAN_POINT('Ctrl Pts',(-0.0458630406410711,60.099973198394,
15.7996900532889));
#46385=CARTESIAN_POINT('Ctrl Pts',(-0.0520361549971498,60.1008299802659,
15.7995758086185));
#46386=CARTESIAN_POINT('Ctrl Pts',(-0.0582088671208629,60.1016866162842,
15.7994385936371));
#46387=CARTESIAN_POINT('Ctrl Pts',(-0.12734800021417,60.1112815998986,15.7979016800937));
#46388=CARTESIAN_POINT('Ctrl Pts',(-0.196435023005444,60.1208575677164,
15.7934860962484));
#46389=CARTESIAN_POINT('Ctrl Pts',(-0.265319269215243,60.1303911617268,
15.7861745697976));
#46390=CARTESIAN_POINT('Ctrl Pts',(-0.328785114153774,60.1391748478738,
15.7794381644578));
#46391=CARTESIAN_POINT('Ctrl Pts',(-0.391836588715798,60.1478888811247,
15.7702695356354));
#46392=CARTESIAN_POINT('Ctrl Pts',(-0.454382638560456,60.1565152457386,
15.75869807515));
#46393=CARTESIAN_POINT('Ctrl Pts',(-0.454430746547466,60.1565218808025,
15.758689174833));
#46394=CARTESIAN_POINT('Ctrl Pts',(-0.454478854236144,60.1565285158147,
15.7586802730931));
#46395=CARTESIAN_POINT('Ctrl Pts',(-0.454526961626474,60.1565351507754,
15.7586713699301));
#46396=CARTESIAN_POINT('Ctrl Pts',(-0.52837655333923,60.1667204701915,15.7450041361788));
#46397=CARTESIAN_POINT('Ctrl Pts',(-0.601526523728802,60.1767846212224,
15.7279862217928));
#46398=CARTESIAN_POINT('Ctrl Pts',(-0.673804609387891,60.1867910088178,
15.7076882553179));
#46399=CARTESIAN_POINT('Ctrl Pts',(-0.683827269572054,60.1881785749331,
15.704873576172));
#46400=CARTESIAN_POINT('Ctrl Pts',(-0.693833097284363,60.1895650222819,
15.7019957794827));
#46401=CARTESIAN_POINT('Ctrl Pts',(-0.703821567336172,60.1909505121541,
15.6990550122623));
#46402=CARTESIAN_POINT('Ctrl Pts',(-0.77894100990679,60.2013702487447,15.6769386327583));
#46403=CARTESIAN_POINT('Ctrl Pts',(-0.853082298181796,60.2117366076373,
15.6512616831298));
#46404=CARTESIAN_POINT('Ctrl Pts',(-0.92600381073812,60.2221056842168,15.6220951695599));
#46405=CARTESIAN_POINT('Ctrl Pts',(-0.938161850952179,60.2238344970955,
15.6172323021775));
#46406=CARTESIAN_POINT('Ctrl Pts',(-0.950285876321194,60.2255633742816,
15.6122723851462));
#46407=CARTESIAN_POINT('Ctrl Pts',(-0.962374636235121,60.2272925622388,
15.6072156980307));
#46408=CARTESIAN_POINT('Ctrl Pts',(-1.03842434324269,60.2381707861794,15.575404364503));
#46409=CARTESIAN_POINT('Ctrl Pts',(-1.11308213560497,60.2490619084814,15.5397639548018));
#46410=CARTESIAN_POINT('Ctrl Pts',(-1.18602358418327,60.2600099587645,15.5003883468616));
#46411=CARTESIAN_POINT('Ctrl Pts',(-1.19421937252181,60.2612400947789,15.4959640564935));
#46412=CARTESIAN_POINT('Ctrl Pts',(-1.20239343972178,60.2624709450305,15.4914925952459));
#46413=CARTESIAN_POINT('Ctrl Pts',(-1.21054528533793,60.2637025685625,15.4869740871883));
#46414=CARTESIAN_POINT('Ctrl Pts',(-1.28805374649585,60.2754129528346,15.4440117173443));
#46415=CARTESIAN_POINT('Ctrl Pts',(-1.36314756475987,60.2871320961967,15.397024406493));
#46416=CARTESIAN_POINT('Ctrl Pts',(-1.43548080528418,60.2988870358612,15.3462784106231));
#46417=CARTESIAN_POINT('Ctrl Pts',(-1.50857195784496,60.3107651444892,15.2950006951621));
#46418=CARTESIAN_POINT('Ctrl Pts',(-1.57884328318765,60.3226795409351,15.2398857656068));
#46419=CARTESIAN_POINT('Ctrl Pts',(-1.64595639049583,60.33463524494,15.1812194589559));
#46420=CARTESIAN_POINT('Ctrl Pts',(-1.71256112033185,60.346500385256,15.1229975458054));
#46421=CARTESIAN_POINT('Ctrl Pts',(-1.77605491076421,60.3584058279396,15.0612791137166));
#46422=CARTESIAN_POINT('Ctrl Pts',(-1.83613637053914,60.370339024527,14.9963398423922));
#46423=CARTESIAN_POINT('Ctrl Pts',(-1.88144242810172,60.3793375757193,14.9473706200111));
#46424=CARTESIAN_POINT('Ctrl Pts',(-1.92480886439003,60.3883515105436,14.8965700506351));
#46425=CARTESIAN_POINT('Ctrl Pts',(-1.96611780436083,60.3973708602517,14.8440474848212));
#46426=CARTESIAN_POINT('Ctrl Pts',(-2.01328239313746,60.4076687260482,14.7840797098103));
#46427=CARTESIAN_POINT('Ctrl Pts',(-2.0575505040754,60.4179269682567,14.7221404931659));
#46428=CARTESIAN_POINT('Ctrl Pts',(-2.09883875439965,60.428127898034,14.6584211624251));
#46429=CARTESIAN_POINT('Ctrl Pts',(-2.10585568884355,60.4298615451358,14.6475920678738));
#46430=CARTESIAN_POINT('Ctrl Pts',(-2.11278655893247,60.431593546692,14.6367114369141));
#46431=CARTESIAN_POINT('Ctrl Pts',(-2.11963095313664,60.4333238279332,14.6257800593745));
#46432=CARTESIAN_POINT('Ctrl Pts',(-2.14375367382694,60.4394221165259,14.5872529729325));
#46433=CARTESIAN_POINT('Ctrl Pts',(-2.16680272970016,60.4454988338563,14.5480963312027));
#46434=CARTESIAN_POINT('Ctrl Pts',(-2.18876181863496,60.4515503313939,14.5083413758981));
#46435=CARTESIAN_POINT('Ctrl Pts',(-2.1887828027413,60.4515561142052,14.508303386061));
#46436=CARTESIAN_POINT('Ctrl Pts',(-2.18880378585152,60.4515618969937,14.5082653956769));
#46437=CARTESIAN_POINT('Ctrl Pts',(-2.18882476796558,60.4515676797595,14.5082274047455));
#46438=CARTESIAN_POINT('Ctrl Pts',(-2.22650688805877,60.4619530429175,14.439998872852));
#46439=CARTESIAN_POINT('Ctrl Pts',(-2.26098034919205,60.4722653626783,14.3700047366866));
#46440=CARTESIAN_POINT('Ctrl Pts',(-2.29214000432683,60.4825490008941,14.298457429472));
#46441=CARTESIAN_POINT('Ctrl Pts',(-2.29567845576629,60.4837167979794,14.2903326068092));
#46442=CARTESIAN_POINT('Ctrl Pts',(-2.29917412029052,60.484884220357,14.2821877680779));
#46443=CARTESIAN_POINT('Ctrl Pts',(-2.30262680350284,60.4860513292658,14.2740232358047));
#46444=CARTESIAN_POINT('Ctrl Pts',(-2.33454719484305,60.4968413643812,14.1985413426673));
#46445=CARTESIAN_POINT('Ctrl Pts',(-2.36279750989817,60.5076050639362,14.1213748437473));
#46446=CARTESIAN_POINT('Ctrl Pts',(-2.38723291317746,60.5183775034172,14.0428001666309));
#46447=CARTESIAN_POINT('Ctrl Pts',(-2.38905840304868,60.5191822774959,14.0369301068831));
#46448=CARTESIAN_POINT('Ctrl Pts',(-2.3908625787226,60.5199870986543,14.031052195651));
#46449=CARTESIAN_POINT('Ctrl Pts',(-2.39264536888567,60.5207919806927,14.0251665522838));
#46450=CARTESIAN_POINT('Ctrl Pts',(-2.39886622731632,60.5236005317593,14.0046292198936));
#46451=CARTESIAN_POINT('Ctrl Pts',(-2.40482696298709,60.5264097579991,13.9839978030011));
#46452=CARTESIAN_POINT('Ctrl Pts',(-2.41052510737083,60.5292202247935,13.9632766606078));
#46453=CARTESIAN_POINT('Ctrl Pts',(-2.43381076806375,60.5407052928709,13.8785990079467));
#46454=CARTESIAN_POINT('Ctrl Pts',(-2.45258513433876,60.5521506386081,13.792878745595));
#46455=CARTESIAN_POINT('Ctrl Pts',(-2.4668090159224,60.5635766116674,13.70651223253));
#46456=CARTESIAN_POINT('Ctrl Pts',(-2.48044230741506,60.5745281666553,13.6237317452983));
#46457=CARTESIAN_POINT('Ctrl Pts',(-2.48989536647366,60.5854615711786,13.5403583727911));
#46458=CARTESIAN_POINT('Ctrl Pts',(-2.49514302977644,60.5963827299336,13.4567264576687));
#46459=CARTESIAN_POINT('Ctrl Pts',(-2.49514465071334,60.5963861033416,13.4567006248267));
#46460=CARTESIAN_POINT('Ctrl Pts',(-2.49514627124893,60.5963894767483,13.4566747919598));
#46461=CARTESIAN_POINT('Ctrl Pts',(-2.4951478913832,60.5963928501539,13.4566489590681));
#46462=CARTESIAN_POINT('Ctrl Pts',(-2.49841156595885,60.6031883967148,13.4046099686768));
#46463=CARTESIAN_POINT('Ctrl Pts',(-2.5000472486871,60.6099790432102,13.3524700211784));
#46464=CARTESIAN_POINT('Ctrl Pts',(-2.50005097985869,60.6167707974152,13.3003061727703));
#46465=CARTESIAN_POINT('Ctrl Pts',(-2.5,59.3994433450696,13.3));
#46466=CARTESIAN_POINT('Ctrl Pts',(-2.5,59.3645326518074,13.5713375280958));
#46467=CARTESIAN_POINT('Ctrl Pts',(-2.45582275699131,59.3298728723396,13.8413154973223));
#46468=CARTESIAN_POINT('Ctrl Pts',(-2.26198134694515,59.2520835125909,14.4158398109649));
#46469=CARTESIAN_POINT('Ctrl Pts',(-2.09274908494108,59.2099873435,14.7078640735593));
#46470=CARTESIAN_POINT('Ctrl Pts',(-1.76542759316789,59.147088947621,15.0772629224902));
#46471=CARTESIAN_POINT('Ctrl Pts',(-1.64857013328762,59.1268133617154,15.1861645024256));
#46472=CARTESIAN_POINT('Ctrl Pts',(-1.39232480313582,59.0857511129315,15.3828374172618));
#46473=CARTESIAN_POINT('Ctrl Pts',(-1.25303350586245,59.0650777127863,15.4694908484802));
#46474=CARTESIAN_POINT('Ctrl Pts',(-0.830465451583301,59.0054283505205,
15.6780073168761));
#46475=CARTESIAN_POINT('Ctrl Pts',(-0.53188567776378,58.966814499779,15.762052975899));
#46476=CARTESIAN_POINT('Ctrl Pts',(-0.0632947915091542,58.9075684335156,
15.8045037340727));
#46477=CARTESIAN_POINT('Ctrl Pts',(0.100020462504728,58.8871449597277,15.8033065024178));
#46478=CARTESIAN_POINT('Ctrl Pts',(0.419134632114546,58.8468549178829,15.7696707599079));
#46479=CARTESIAN_POINT('Ctrl Pts',(0.574292788339893,58.8270821187475,15.7382651271886));
#46480=CARTESIAN_POINT('Ctrl Pts',(1.04510008816248,58.7654333506753,15.5955037295384));
#46481=CARTESIAN_POINT('Ctrl Pts',(1.34212244248392,58.7241320994188,15.4354857585171));
#46482=CARTESIAN_POINT('Ctrl Pts',(1.72305534902668,58.6624257125961,15.1185586697063));
#46483=CARTESIAN_POINT('Ctrl Pts',(1.83689407189847,58.6423915696704,15.0034956389685));
#46484=CARTESIAN_POINT('Ctrl Pts',(2.04238469877396,58.6019544913329,14.7510570451429));
#46485=CARTESIAN_POINT('Ctrl Pts',(2.13316363596419,58.5816551435649,14.613970192102));
#46486=CARTESIAN_POINT('Ctrl Pts',(2.35859713029488,58.5219805079189,14.1878064710611));
#46487=CARTESIAN_POINT('Ctrl Pts',(2.45231769902695,58.483116114058,13.8808031272104));
#46488=CARTESIAN_POINT('Ctrl Pts',(2.50271885245684,58.4244300543436,13.4070548963955));
#46489=CARTESIAN_POINT('Ctrl Pts',(2.50447649653974,58.4050121415564,13.2483910766068));
#46490=CARTESIAN_POINT('Ctrl Pts',(2.47775045955394,58.3658932325713,12.9303955960265));
#46491=CARTESIAN_POINT('Ctrl Pts',(2.44885674681256,58.3462843322562,12.7718360701045));
#46492=CARTESIAN_POINT('Ctrl Pts',(2.31576608143569,58.2866967409114,12.3031020865792));
#46493=CARTESIAN_POINT('Ctrl Pts',(2.16593231736754,58.2472017253765,12.0095183875325));
#46494=CARTESIAN_POINT('Ctrl Pts',(1.75727584906853,58.1671523836789,11.4907247669193));
#46495=CARTESIAN_POINT('Ctrl Pts',(1.50017129145475,58.1269675630468,11.2724387051608));
#46496=CARTESIAN_POINT('Ctrl Pts',(1.0689625956934,58.0676891342559,11.0345071919954));
#46497=CARTESIAN_POINT('Ctrl Pts',(0.923165792334853,58.0487401405484,10.9712866142904));
#46498=CARTESIAN_POINT('Ctrl Pts',(0.454178518263113,57.989610193629,10.8189425390981));
#46499=CARTESIAN_POINT('Ctrl Pts',(0.118436411469683,57.9497763461178,10.7804901403219));
#46500=CARTESIAN_POINT('Ctrl Pts',(-0.536725224395779,57.8717130480077,
10.8370236215221));
#46501=CARTESIAN_POINT('Ctrl Pts',(-0.85009979282434,57.8343099805388,10.9268917939241));
#46502=CARTESIAN_POINT('Ctrl Pts',(-1.3840831280269,57.7629396421448,11.1997909007637));
#46503=CARTESIAN_POINT('Ctrl Pts',(-1.60791004167294,57.7297936317739,11.365772965549));
#46504=CARTESIAN_POINT('Ctrl Pts',(-1.99099596710922,57.6651288580241,11.7632217121788));
#46505=CARTESIAN_POINT('Ctrl Pts',(-2.14799101676222,57.6340707102155,11.9915921922629));
#46506=CARTESIAN_POINT('Ctrl Pts',(-2.40621270997693,57.5646689399261,12.5437760893431));
#46507=CARTESIAN_POINT('Ctrl Pts',(-2.4856484868962,57.5259257271973,12.8718967308891));
#46508=CARTESIAN_POINT('Ctrl Pts',(-2.49941036415996,57.4841426208034,13.2372814670857));
#46509=CARTESIAN_POINT('Ctrl Pts',(-2.5,57.4805638506737,13.26865141346));
#46510=CARTESIAN_POINT('Ctrl Pts',(-2.5,57.4769927816046,13.3));
#46511=CARTESIAN_POINT('Origin',(0.,70.2,13.3));
#46512=CARTESIAN_POINT('',(1.36952200671963,56.456522023403,11.210153809184));
#46513=CARTESIAN_POINT('Ctrl Pts',(-2.5,57.4769927816046,13.3));
#46514=CARTESIAN_POINT('Ctrl Pts',(-2.5,57.4459316982446,13.5726693438026));
#46515=CARTESIAN_POINT('Ctrl Pts',(-2.45538841038206,57.4156542366357,13.8437456246808));
#46516=CARTESIAN_POINT('Ctrl Pts',(-2.25976716009472,57.3469461366581,14.4209791769068));
#46517=CARTESIAN_POINT('Ctrl Pts',(-2.08862106037187,57.3078837011561,14.7145146492395));
#46518=CARTESIAN_POINT('Ctrl Pts',(-1.67879428804009,57.2396608994169,15.173327824965));
#46519=CARTESIAN_POINT('Ctrl Pts',(-1.45963520298074,57.2105138890148,15.3487075687647));
#46520=CARTESIAN_POINT('Ctrl Pts',(-0.924771568170676,57.1451182786575,
15.6464691107768));
#46521=CARTESIAN_POINT('Ctrl Pts',(-0.604120811806337,57.1074465471387,
15.7486948490657));
#46522=CARTESIAN_POINT('Ctrl Pts',(0.00103428072363587,57.0419646916788,
15.8151364688876));
#46523=CARTESIAN_POINT('Ctrl Pts',(0.277999449479295,57.0142712095688,15.7997361875592));
#46524=CARTESIAN_POINT('Ctrl Pts',(0.874633747031843,56.9522497055724,15.6659664618541));
#46525=CARTESIAN_POINT('Ctrl Pts',(1.18406779077029,56.9158900746659,15.5272610971029));
#46526=CARTESIAN_POINT('Ctrl Pts',(1.57583850097768,56.8664620514363,15.2463189710605));
#46527=CARTESIAN_POINT('Ctrl Pts',(1.68709219417902,56.8519536134822,15.1507213273601));
#46528=CARTESIAN_POINT('Ctrl Pts',(2.02101231098688,56.8058296438384,14.808485994022));
#46529=CARTESIAN_POINT('Ctrl Pts',(2.20310153977486,56.7752544493422,14.5273228999349));
#46530=CARTESIAN_POINT('Ctrl Pts',(2.42812484038507,56.7140033923145,13.9579751872364));
#46531=CARTESIAN_POINT('Ctrl Pts',(2.48667123778913,56.6869043094238,13.6813465795139));
#46532=CARTESIAN_POINT('Ctrl Pts',(2.51062235352946,56.6347298760345,13.0864889195961));
#46533=CARTESIAN_POINT('Ctrl Pts',(2.46393343806034,56.6097884288235,12.7728566775426));
#46534=CARTESIAN_POINT('Ctrl Pts',(2.30818385936516,56.5675513054282,12.3267067575381));
#46535=CARTESIAN_POINT('Ctrl Pts',(2.24198890991713,56.5533848606566,12.1826241047964));
#46536=CARTESIAN_POINT('Ctrl Pts',(2.05772104536115,56.5224072325291,11.8649117906946));
#46537=CARTESIAN_POINT('Ctrl Pts',(1.93057620891326,56.5064572664569,11.697920368476));
#46538=CARTESIAN_POINT('Ctrl Pts',(1.65862592877859,56.479276351471,11.4209094098465));
#46539=CARTESIAN_POINT('Ctrl Pts',(1.51996586495887,56.4677225622875,11.3070874124032));
#46540=CARTESIAN_POINT('Ctrl Pts',(1.37035622588183,56.455286737476,11.2090375866155));
#46541=CARTESIAN_POINT('',(-2.50125173685429,55.6414517644448,13.3001584307864));
#46542=CARTESIAN_POINT('Ctrl Pts',(1.36944901719983,56.4564965633172,11.2101199336514));
#46543=CARTESIAN_POINT('Ctrl Pts',(1.29603082900563,56.4426908388302,11.1624967982744));
#46544=CARTESIAN_POINT('Ctrl Pts',(1.22027156825106,56.428933734737,11.1187547073001));
#46545=CARTESIAN_POINT('Ctrl Pts',(1.14255504747613,56.4151597343664,11.0790266810285));
#46546=CARTESIAN_POINT('Ctrl Pts',(1.06363597865445,56.4011726017417,11.0386839223947));
#46547=CARTESIAN_POINT('Ctrl Pts',(0.98269862043085,56.3871679761864,11.0024808901664));
#46548=CARTESIAN_POINT('Ctrl Pts',(0.90013272529909,56.373112312793,10.970569505787));
#46549=CARTESIAN_POINT('Ctrl Pts',(0.817545950255569,56.3590530948931,10.9386500514061));
#46550=CARTESIAN_POINT('Ctrl Pts',(0.733330146478969,56.344942943031,10.911024534462));
#46551=CARTESIAN_POINT('Ctrl Pts',(0.647860516769757,56.330782502838,10.8878527637467));
#46552=CARTESIAN_POINT('Ctrl Pts',(0.580271343564073,56.3195844615205,10.8695285843898));
#46553=CARTESIAN_POINT('Ctrl Pts',(0.511897862989226,56.3083556916996,10.8539896154898));
#46554=CARTESIAN_POINT('Ctrl Pts',(0.442916666885505,56.2971105655553,10.8413190935192));
#46555=CARTESIAN_POINT('Ctrl Pts',(0.361629173409385,56.2838593004318,10.8263881408799));
#46556=CARTESIAN_POINT('Ctrl Pts',(0.279900731404808,56.2706501227155,10.8155140490353));
#46557=CARTESIAN_POINT('Ctrl Pts',(0.198010739746884,56.2575256924461,10.8087225081528));
#46558=CARTESIAN_POINT('Ctrl Pts',(0.191809252601509,56.2565317860607,10.8082081882386));
#46559=CARTESIAN_POINT('Ctrl Pts',(0.185606819982153,56.2555383643905,10.8077172973724));
#46560=CARTESIAN_POINT('Ctrl Pts',(0.179403554156247,56.2545454453184,10.8072498547535));
#46561=CARTESIAN_POINT('Ctrl Pts',(0.0994616940672659,56.2417496374696,
10.8012258935873));
#46562=CARTESIAN_POINT('Ctrl Pts',(0.0193841213790183,56.2290379427932,
10.7990925696856));
#46563=CARTESIAN_POINT('Ctrl Pts',(-0.0606086754043837,56.2164626019884,
10.8008947606548));
#46564=CARTESIAN_POINT('Ctrl Pts',(-0.0682721219220201,56.2152578628672,
10.8010674136268));
#46565=CARTESIAN_POINT('Ctrl Pts',(-0.0759348159106824,56.2140543726688,
10.8012762167855));
#46566=CARTESIAN_POINT('Ctrl Pts',(-0.0835965792288266,56.2128521757121,
10.8015212294454));
#46567=CARTESIAN_POINT('Ctrl Pts',(-0.110826037820625,56.2085796380608,
10.8023919901046));
#46568=CARTESIAN_POINT('Ctrl Pts',(-0.138043705741017,56.2043235614105,
10.8037199228905));
#46569=CARTESIAN_POINT('Ctrl Pts',(-0.165241826304231,56.2000861980125,
10.8055077843409));
#46570=CARTESIAN_POINT('Ctrl Pts',(-0.165242864855589,56.2000860362101,
10.8055078526098));
#46571=CARTESIAN_POINT('Ctrl Pts',(-0.165243903406876,56.2000858744078,
10.8055079208794));
#46572=CARTESIAN_POINT('Ctrl Pts',(-0.165244941958176,56.2000857126056,
10.8055079891497));
#46573=CARTESIAN_POINT('Ctrl Pts',(-0.245392444874828,56.1875990410136,
10.8107765684174));
#46574=CARTESIAN_POINT('Ctrl Pts',(-0.325372755007318,56.1752736773837,
10.8200370396293));
#46575=CARTESIAN_POINT('Ctrl Pts',(-0.404926294732208,56.1630147684855,
10.8332229156012));
#46576=CARTESIAN_POINT('Ctrl Pts',(-0.411686604966254,56.1619730294558,
10.83434342655));
#46577=CARTESIAN_POINT('Ctrl Pts',(-0.418443811964095,56.1609317726542,
10.8354923063435));
#46578=CARTESIAN_POINT('Ctrl Pts',(-0.425197744114492,56.1598909411829,
10.836669526147));
#46579=CARTESIAN_POINT('Ctrl Pts',(-0.466390339984701,56.1535428539932,
10.8438494531194));
#46580=CARTESIAN_POINT('Ctrl Pts',(-0.507461483222913,56.1472107569749,
10.8520832082565));
#46581=CARTESIAN_POINT('Ctrl Pts',(-0.548371370921128,56.1408831966229,
10.8613642367384));
#46582=CARTESIAN_POINT('Ctrl Pts',(-0.632916656422052,56.127806519404,10.8805446170056));
#46583=CARTESIAN_POINT('Ctrl Pts',(-0.716335870297029,56.1148144342113,
10.904097743567));
#46584=CARTESIAN_POINT('Ctrl Pts',(-0.798288826299474,56.101825375084,10.9318430111096));
#46585=CARTESIAN_POINT('Ctrl Pts',(-0.881714476844274,56.0886029025764,
10.960086861084));
#46586=CARTESIAN_POINT('Ctrl Pts',(-0.963620305287153,56.0753834070735,
10.9926755305163));
#46587=CARTESIAN_POINT('Ctrl Pts',(-1.04363603309156,56.0621136895825,11.0294319090248));
#46588=CARTESIAN_POINT('Ctrl Pts',(-1.12414277452161,56.0487625429491,11.0664138417234));
#46589=CARTESIAN_POINT('Ctrl Pts',(-1.20273558800698,56.035360582838,11.1076149159066));
#46590=CARTESIAN_POINT('Ctrl Pts',(-1.27903342209982,56.0218874888268,11.1528620961267));
#46591=CARTESIAN_POINT('Ctrl Pts',(-1.33966487582784,56.0111808510065,11.1888185861956));
#46592=CARTESIAN_POINT('Ctrl Pts',(-1.39884693568266,56.0004299968532,11.2273301795414));
#46593=CARTESIAN_POINT('Ctrl Pts',(-1.4563897806272,55.9896392984033,11.2683141868384));
#46594=CARTESIAN_POINT('Ctrl Pts',(-1.5250305535497,55.9767674655509,11.3172025228433));
#46595=CARTESIAN_POINT('Ctrl Pts',(-1.59099181520561,55.9639034410327,11.3693610284727));
#46596=CARTESIAN_POINT('Ctrl Pts',(-1.6540427539691,55.9510765991678,11.4245667677993));
#46597=CARTESIAN_POINT('Ctrl Pts',(-1.65755599969368,55.9503618778928,11.4276428731114));
#46598=CARTESIAN_POINT('Ctrl Pts',(-1.66106021037135,55.9496472714153,11.4307284528359));
#46599=CARTESIAN_POINT('Ctrl Pts',(-1.66455534626192,55.9489327845877,11.4338234731183));
#46600=CARTESIAN_POINT('Ctrl Pts',(-1.72541332248449,55.9364920029623,11.4877145596608));
#46601=CARTESIAN_POINT('Ctrl Pts',(-1.78352031244173,55.9240879815468,11.5444634611635));
#46602=CARTESIAN_POINT('Ctrl Pts',(-1.83868488776429,55.9117632804885,11.6039034913596));
#46603=CARTESIAN_POINT('Ctrl Pts',(-1.84571234650124,55.910193227105,11.6114756036632));
#46604=CARTESIAN_POINT('Ctrl Pts',(-1.85269205021684,55.9086244564431,11.6190914578392));
#46605=CARTESIAN_POINT('Ctrl Pts',(-1.8596235971321,55.9070570525137,11.6267507699646));
#46606=CARTESIAN_POINT('Ctrl Pts',(-1.91219654572504,55.8951689347226,11.6848435200463));
#46607=CARTESIAN_POINT('Ctrl Pts',(-1.96200070672626,55.8833602282237,11.7454318674796));
#46608=CARTESIAN_POINT('Ctrl Pts',(-2.00886749518019,55.871677708519,11.8084100756291));
#46609=CARTESIAN_POINT('Ctrl Pts',(-2.01377586110376,55.8704541964434,11.8150057930018));
#46610=CARTESIAN_POINT('Ctrl Pts',(-2.01865199736498,55.8692320650099,11.8216277691318));
#46611=CARTESIAN_POINT('Ctrl Pts',(-2.02349570117022,55.8680113655344,11.828275914873));
#46612=CARTESIAN_POINT('Ctrl Pts',(-2.02636737027956,55.8672876538632,11.8322173769291));
#46613=CARTESIAN_POINT('Ctrl Pts',(-2.02922764241447,55.8665644486409,11.8361680346309));
#46614=CARTESIAN_POINT('Ctrl Pts',(-2.03207647586611,55.865841761517,11.8401278694902));
#46615=CARTESIAN_POINT('Ctrl Pts',(-2.03211492050008,55.865832008949,11.8401813069425));
#46616=CARTESIAN_POINT('Ctrl Pts',(-2.03215336304922,55.8658222564752,11.8402347460648));
#46617=CARTESIAN_POINT('Ctrl Pts',(-2.03219180351324,55.8658125040956,11.8402881868568));
#46618=CARTESIAN_POINT('Ctrl Pts',(-2.06766621902012,55.8568126136023,11.8896055119599));
#46619=CARTESIAN_POINT('Ctrl Pts',(-2.10136653431973,55.8478927840317,11.9403452179639));
#46620=CARTESIAN_POINT('Ctrl Pts',(-2.13322179210664,55.8390117877274,11.992403401392));
#46621=CARTESIAN_POINT('Ctrl Pts',(-2.1779864217838,55.8265317596772,12.0655582105106));
#46622=CARTESIAN_POINT('Ctrl Pts',(-2.21887907971105,55.8141907353134,12.1409422096651));
#46623=CARTESIAN_POINT('Ctrl Pts',(-2.25578928865405,55.8018972314393,12.218181355777));
#46624=CARTESIAN_POINT('Ctrl Pts',(-2.29350245773508,55.7893362895351,12.2971007946101));
#46625=CARTESIAN_POINT('Ctrl Pts',(-2.32705691767267,55.7768247567593,12.3779571064769));
#46626=CARTESIAN_POINT('Ctrl Pts',(-2.35632092094978,55.7643023245731,12.4603424912428));
#46627=CARTESIAN_POINT('Ctrl Pts',(-2.38592694917522,55.7516335356434,12.5436907605704));
#46628=CARTESIAN_POINT('Ctrl Pts',(-2.41114083119113,55.7389535795631,12.6286035012372));
#46629=CARTESIAN_POINT('Ctrl Pts',(-2.43182710159743,55.7262393017939,12.7146528205441));
#46630=CARTESIAN_POINT('Ctrl Pts',(-2.44241010168477,55.7197347362005,12.7586752535808));
#46631=CARTESIAN_POINT('Ctrl Pts',(-2.45180819335629,55.7132218194797,12.8029951221362));
#46632=CARTESIAN_POINT('Ctrl Pts',(-2.46000407553754,55.7067013018513,12.8475555370706));
#46633=CARTESIAN_POINT('Ctrl Pts',(-2.46001189210237,55.7066950831127,12.8475980351647));
#46634=CARTESIAN_POINT('Ctrl Pts',(-2.46001970757379,55.7066888643674,12.8476405334778));
#46635=CARTESIAN_POINT('Ctrl Pts',(-2.46002752195179,55.7066826456154,12.8476830320098));
#46636=CARTESIAN_POINT('Ctrl Pts',(-2.46481980748636,55.7028689018423,12.8737458997491));
#46637=CARTESIAN_POINT('Ctrl Pts',(-2.46920089563749,55.6990526313445,12.899891090277));
#46638=CARTESIAN_POINT('Ctrl Pts',(-2.47316768476101,55.6952351470767,12.9261138759658));
#46639=CARTESIAN_POINT('Ctrl Pts',(-2.48294489086037,55.6858259424769,12.990746900862));
#46640=CARTESIAN_POINT('Ctrl Pts',(-2.49016872377525,55.6764461520061,13.0556000782221));
#46641=CARTESIAN_POINT('Ctrl Pts',(-2.49483923918304,55.6671113889433,13.1206080688506));
#46642=CARTESIAN_POINT('Ctrl Pts',(-2.49484248107682,55.6671049095063,13.1206531921361));
#46643=CARTESIAN_POINT('Ctrl Pts',(-2.49484572173883,55.6670984300904,13.1206983154964));
#46644=CARTESIAN_POINT('Ctrl Pts',(-2.49484896116907,55.6670919506956,13.1207434389313));
#46645=CARTESIAN_POINT('Ctrl Pts',(-2.49913669539619,55.6585157748956,13.1804691569517));
#46646=CARTESIAN_POINT('Ctrl Pts',(-2.50126743306733,55.6499764118575,13.2403259773289));
#46647=CARTESIAN_POINT('Ctrl Pts',(-2.50125173685429,55.6414517644448,13.3001584307864));
#46648=CARTESIAN_POINT('',(-2.5,56.395745969557,13.3));
#46649=CARTESIAN_POINT('',(-2.5,70.2,13.3));
#46650=CARTESIAN_POINT('',(-2.46826046448302,56.4316304354619,12.9028993853228));
#46651=CARTESIAN_POINT('Ctrl Pts',(-2.5,56.395745969557,13.3));
#46652=CARTESIAN_POINT('Ctrl Pts',(-2.5,56.4077454755149,13.1671729739548));
#46653=CARTESIAN_POINT('Ctrl Pts',(-2.48941435575088,56.4195677315213,13.0343816947313));
#46654=CARTESIAN_POINT('Ctrl Pts',(-2.46825964356923,56.4316313272142,12.9028925436012));
#46655=CARTESIAN_POINT('Ctrl Pts',(-2.46825694932604,56.4314940421042,12.9028757976354));
#46656=CARTESIAN_POINT('Ctrl Pts',(-2.43520383378043,56.461992268376,12.6974398618336));
#46657=CARTESIAN_POINT('Ctrl Pts',(-2.3766228776081,56.4924752322176,12.4968768864496));
#46658=CARTESIAN_POINT('Ctrl Pts',(-2.19111489475908,56.5590511745454,12.0688458864486));
#46659=CARTESIAN_POINT('Ctrl Pts',(-2.0522520440533,56.5945121834133,11.8491177263255));
#46660=CARTESIAN_POINT('Ctrl Pts',(-1.66671822294653,56.6763109067864,11.4081288818872));
#46661=CARTESIAN_POINT('Ctrl Pts',(-1.40497744941339,56.7223224480549,11.2064031416049));
#46662=CARTESIAN_POINT('Ctrl Pts',(-0.972108750619124,56.7897769391544,
10.9914621828345));
#46663=CARTESIAN_POINT('Ctrl Pts',(-0.826166856433883,56.8111836067347,
10.93530015989));
#46664=CARTESIAN_POINT('Ctrl Pts',(-0.369399857416966,56.8761099376736,
10.807029416002));
#46665=CARTESIAN_POINT('Ctrl Pts',(-0.0492021703253953,56.9191676728897,
10.7802800871358));
#46666=CARTESIAN_POINT('Ctrl Pts',(0.433302312139852,56.9847184945054,10.8321902665078));
#46667=CARTESIAN_POINT('Ctrl Pts',(0.596991241850096,57.0070965552408,10.8665986960538));
#46668=CARTESIAN_POINT('Ctrl Pts',(0.91232652892166,57.0515843353888,10.9666447355976));
#46669=CARTESIAN_POINT('Ctrl Pts',(1.06336864643656,57.0735814735889,11.0314900382241));
#46670=CARTESIAN_POINT('Ctrl Pts',(1.34799849265034,57.117101753697,11.188405258786));
#46671=CARTESIAN_POINT('Ctrl Pts',(1.48119110792558,57.138464255273,11.2796006096996));
#46672=CARTESIAN_POINT('Ctrl Pts',(1.84765740379511,57.2018052376995,11.586361653006));
#46673=CARTESIAN_POINT('Ctrl Pts',(2.04977963288396,57.2434055391266,11.8341096808076));
#46674=CARTESIAN_POINT('Ctrl Pts',(2.27874118847686,57.3066143958866,12.2585242906968));
#46675=CARTESIAN_POINT('Ctrl Pts',(2.34261540956501,57.3281056529485,12.4114660491561));
#46676=CARTESIAN_POINT('Ctrl Pts',(2.48230431115144,57.3903420304424,12.8687288980539));
#46677=CARTESIAN_POINT('Ctrl Pts',(2.51675090670696,57.4306842182026,13.1823973446887));
#46678=CARTESIAN_POINT('Ctrl Pts',(2.4795336408618,57.492319675819,13.6598471795062));
#46679=CARTESIAN_POINT('Ctrl Pts',(2.4501631459233,57.5135330746118,13.8237211100322));
#46680=CARTESIAN_POINT('Ctrl Pts',(2.318547542361,57.5750706742593,14.2868005586607));
#46681=CARTESIAN_POINT('Ctrl Pts',(2.17571283375371,57.6149163814681,14.5711198884439));
#46682=CARTESIAN_POINT('Ctrl Pts',(1.88386088806936,57.6755517746152,14.951673850455));
#46683=CARTESIAN_POINT('Ctrl Pts',(1.77134472640245,57.6961843048605,15.0718074279181));
#46684=CARTESIAN_POINT('Ctrl Pts',(1.40788708041656,57.7569018446779,15.3903782784728));
#46685=CARTESIAN_POINT('Ctrl Pts',(1.12982731653552,57.7964293220125,15.552854342033));
#46686=CARTESIAN_POINT('Ctrl Pts',(0.675575006530766,57.8562171006933,15.7124561782358));
#46687=CARTESIAN_POINT('Ctrl Pts',(0.517551642506458,57.8762570492878,15.7512226167826));
#46688=CARTESIAN_POINT('Ctrl Pts',(0.0391949544407114,57.9358455834721,
15.8202158073517));
#46689=CARTESIAN_POINT('Ctrl Pts',(-0.284388345736859,57.9747798850292,
15.8044320481447));
#46690=CARTESIAN_POINT('Ctrl Pts',(-0.899717038167667,58.0520139946708,
15.653341691228));
#46691=CARTESIAN_POINT('Ctrl Pts',(-1.18665887089664,58.0894794143834,15.5225189252697));
#46692=CARTESIAN_POINT('Ctrl Pts',(-1.7146742041079,58.1670655530837,15.1496685883279));
#46693=CARTESIAN_POINT('Ctrl Pts',(-1.94603656445841,58.2066718111652,14.9044838725725));
#46694=CARTESIAN_POINT('Ctrl Pts',(-2.24294382232247,58.2731478789509,14.427480083543));
#46695=CARTESIAN_POINT('Ctrl Pts',(-2.33640446706872,58.2997659432329,14.2182773391564));
#46696=CARTESIAN_POINT('Ctrl Pts',(-2.46638263202234,58.3543009467222,13.7721573370521));
#46697=CARTESIAN_POINT('Ctrl Pts',(-2.49998965566844,58.38186849262,13.5367483102214));
#46698=CARTESIAN_POINT('Ctrl Pts',(-2.49999999761251,58.4092448555942,13.3001092586366));
#46699=CARTESIAN_POINT('Origin',(0.,70.2,13.3));
#46700=CARTESIAN_POINT('',(-2.5,53.601880595513,13.2999999999966));
#46701=CARTESIAN_POINT('',(-2.5,54.6185115759899,13.3));
#46702=CARTESIAN_POINT('',(-2.5,70.2,13.3));
#46703=CARTESIAN_POINT('Ctrl Pts',(-2.5,54.6185115759899,13.3));
#46704=CARTESIAN_POINT('Ctrl Pts',(-2.5,54.6256816081909,13.2428501459448));
#46705=CARTESIAN_POINT('Ctrl Pts',(-2.4980403631648,54.6328527105969,13.1856442401504));
#46706=CARTESIAN_POINT('Ctrl Pts',(-2.48320476460674,54.6599395432761,12.9699132169714));
#46707=CARTESIAN_POINT('Ctrl Pts',(-2.45720238398481,54.6797643890759,12.8127396260848));
#46708=CARTESIAN_POINT('Ctrl Pts',(-2.33302560160475,54.7402005328981,12.3445441614442));
#46709=CARTESIAN_POINT('Ctrl Pts',(-2.18897094356574,54.7802755360276,12.0492654123138));
#46710=CARTESIAN_POINT('Ctrl Pts',(-1.81028555321965,54.8578225681675,11.5496473271837));
#46711=CARTESIAN_POINT('Ctrl Pts',(-1.58622614775164,54.8945743522683,11.3442941017801));
#46712=CARTESIAN_POINT('Ctrl Pts',(-1.04874269305375,54.972199004244,11.0062399209845));
#46713=CARTESIAN_POINT('Ctrl Pts',(-0.733763163302521,55.0124741275843,
10.886948758197));
#46714=CARTESIAN_POINT('Ctrl Pts',(-0.24315258734495,55.0727292892315,10.806475911269));
#46715=CARTESIAN_POINT('Ctrl Pts',(-0.0794297301991653,55.0924802060136,
10.7959072366966));
#46716=CARTESIAN_POINT('Ctrl Pts',(0.247103105746923,55.1318695094133,10.8069049501745));
#46717=CARTESIAN_POINT('Ctrl Pts',(0.409130891528226,55.1514061426414,10.8283208184865));
#46718=CARTESIAN_POINT('Ctrl Pts',(0.727223091315103,55.1906127019791,10.9025211533163));
#46719=CARTESIAN_POINT('Ctrl Pts',(0.882501490435353,55.2101772749367,10.9552283963109));
#46720=CARTESIAN_POINT('Ctrl Pts',(1.32114398037918,55.2676383950357,11.1539172495321));
#46721=CARTESIAN_POINT('Ctrl Pts',(1.58312223767498,55.3048904217772,11.3391714937393));
#46722=CARTESIAN_POINT('Ctrl Pts',(2.03490250559403,55.381797392642,11.809718075388));
#46723=CARTESIAN_POINT('Ctrl Pts',(2.21575623272531,55.421156485849,12.0949124350888));
#46724=CARTESIAN_POINT('Ctrl Pts',(2.44469767641483,55.4957097072909,12.6937526721326));
#46725=CARTESIAN_POINT('Ctrl Pts',(2.50057746437837,55.5302945892199,12.9979890867919));
#46726=CARTESIAN_POINT('Ctrl Pts',(2.49938474111581,55.6028559205025,13.6266753707104));
#46727=CARTESIAN_POINT('Ctrl Pts',(2.43659302018294,55.6397778948392,13.9455522396094));
#46728=CARTESIAN_POINT('Ctrl Pts',(2.25525689348932,55.6937730616882,14.3903531379472));
#46729=CARTESIAN_POINT('Ctrl Pts',(2.1817163323055,55.7113335238116,14.5309230217389));
#46730=CARTESIAN_POINT('Ctrl Pts',(1.9129600563537,55.7662886867816,14.9439075857987));
#46731=CARTESIAN_POINT('Ctrl Pts',(1.67612906556862,55.8040630675707,15.1848021877775));
#46732=CARTESIAN_POINT('Ctrl Pts',(1.14388756487371,55.8747303709051,15.5441473790804));
#46733=CARTESIAN_POINT('Ctrl Pts',(0.859266810832548,55.9071604172506,15.6677742999895));
#46734=CARTESIAN_POINT('Ctrl Pts',(0.253630371974718,55.974891106573,15.8068021057106));
#46735=CARTESIAN_POINT('Ctrl Pts',(-0.0626823167098201,56.008815340953,
15.8188438213752));
#46736=CARTESIAN_POINT('Ctrl Pts',(-0.529596877881329,56.0581367373013,
15.7483874886325));
#46737=CARTESIAN_POINT('Ctrl Pts',(-0.683577128958439,56.074362666002,15.7099378941588));
#46738=CARTESIAN_POINT('Ctrl Pts',(-1.14763743670498,56.1251986327514,15.5459656276796));
#46739=CARTESIAN_POINT('Ctrl Pts',(-1.43697091166929,56.1605841531913,15.372826789526));
#46740=CARTESIAN_POINT('Ctrl Pts',(-1.90876623848562,56.2249845726101,14.9429390715));
#46741=CARTESIAN_POINT('Ctrl Pts',(-2.09442498998999,56.2537431699344,14.6985877607604));
#46742=CARTESIAN_POINT('Ctrl Pts',(-2.35889595293474,56.311807009802,14.1748280973507));
#46743=CARTESIAN_POINT('Ctrl Pts',(-2.44260186386045,56.3397192377136,13.9029365998579));
#46744=CARTESIAN_POINT('Ctrl Pts',(-2.49303031383222,56.3761580991573,13.5155872348193));
#46745=CARTESIAN_POINT('Ctrl Pts',(-2.5,56.3860090119722,13.4077820306317));
#46746=CARTESIAN_POINT('Ctrl Pts',(-2.5,56.395745969557,13.3));
#46747=CARTESIAN_POINT('',(-2.49999996150753,53.6019333424293,13.2995612946774));
#46748=CARTESIAN_POINT('Ctrl Pts',(-2.49999999962317,55.6406441094823,13.3000434069646));
#46749=CARTESIAN_POINT('Ctrl Pts',(-2.49999514856348,55.6008789438551,13.5794374930429));
#46750=CARTESIAN_POINT('Ctrl Pts',(-2.45315110307401,55.561142419573,13.8569861486731));
#46751=CARTESIAN_POINT('Ctrl Pts',(-2.32260733326474,55.506429780821,14.2324084986736));
#46752=CARTESIAN_POINT('Ctrl Pts',(-2.27606908246108,55.4904458047403,14.3408684472124));
#46753=CARTESIAN_POINT('Ctrl Pts',(-2.071826177445,55.4298800450285,14.7370079936151));
#46754=CARTESIAN_POINT('Ctrl Pts',(-1.86581453799125,55.3851594898524,14.9958973400834));
#46755=CARTESIAN_POINT('Ctrl Pts',(-1.4313046639714,55.3051154312028,15.3639385942157));
#46756=CARTESIAN_POINT('Ctrl Pts',(-1.2250133956775,55.2710204191418,15.4926933185702));
#46757=CARTESIAN_POINT('Ctrl Pts',(-0.696699257190743,55.1926776146113,
15.724192593985));
#46758=CARTESIAN_POINT('Ctrl Pts',(-0.366087260910269,55.1495429980827,
15.7956331535918));
#46759=CARTESIAN_POINT('Ctrl Pts',(0.286967813768001,55.0618561944297,15.8037691593593));
#46760=CARTESIAN_POINT('Ctrl Pts',(0.602914036599877,55.0184354138797,15.7469702169358));
#46761=CARTESIAN_POINT('Ctrl Pts',(1.15381366359778,54.938697353611,15.5344819690884));
#46762=CARTESIAN_POINT('Ctrl Pts',(1.39025769175468,54.9035361389359,15.3955795865521));
#46763=CARTESIAN_POINT('Ctrl Pts',(1.84106150969616,54.8274471042439,15.0202170579832));
#46764=CARTESIAN_POINT('Ctrl Pts',(2.04236777153051,54.7867425911399,14.7755761270405));
#46765=CARTESIAN_POINT('Ctrl Pts',(2.31693127172701,54.7110312123163,14.2738426169271));
#46766=CARTESIAN_POINT('Ctrl Pts',(2.40501956916731,54.6768940542676,14.0297055291302));
#46767=CARTESIAN_POINT('Ctrl Pts',(2.48430527144445,54.6228541884747,13.621249360735));
#46768=CARTESIAN_POINT('Ctrl Pts',(2.49964426585912,54.6025971645548,13.4635911560632));
#46769=CARTESIAN_POINT('Ctrl Pts',(2.50059200737536,54.5475880435969,13.035112195922));
#46770=CARTESIAN_POINT('Ctrl Pts',(2.45731107975392,54.5130740518882,12.7663952638752));
#46771=CARTESIAN_POINT('Ctrl Pts',(2.26943700520349,54.4362594902424,12.2024299909904));
#46772=CARTESIAN_POINT('Ctrl Pts',(2.10820642991216,54.394567649508,11.91778419352));
#46773=CARTESIAN_POINT('Ctrl Pts',(1.6792492715809,54.3106503627889,11.4179720115442));
#46774=CARTESIAN_POINT('Ctrl Pts',(1.41260525198989,54.2689477200906,11.2103832946605));
#46775=CARTESIAN_POINT('Ctrl Pts',(0.96464551892134,54.2059927401207,10.9876615128587));
#46776=CARTESIAN_POINT('Ctrl Pts',(0.809319659711741,54.1852240841484,10.9288283632719));
#46777=CARTESIAN_POINT('Ctrl Pts',(0.352595701903903,54.1259154090887,10.8059896289497));
#46778=CARTESIAN_POINT('Ctrl Pts',(0.0436742169096238,54.0878238786443,
10.7815632772995));
#46779=CARTESIAN_POINT('Ctrl Pts',(-0.420033436857514,54.0297578632496,
10.830415860734));
#46780=CARTESIAN_POINT('Ctrl Pts',(-0.576192859075911,54.0100451599276,
10.8621158564814));
#46781=CARTESIAN_POINT('Ctrl Pts',(-0.887017238542555,53.9697638273405,
10.9567687532628));
#46782=CARTESIAN_POINT('Ctrl Pts',(-1.04055054904443,53.9492993877314,11.0207913615787));
#46783=CARTESIAN_POINT('Ctrl Pts',(-1.45642500566705,53.8910929605599,11.2450557000329));
#46784=CARTESIAN_POINT('Ctrl Pts',(-1.69720452912144,53.8539341723211,11.4389556136179));
#46785=CARTESIAN_POINT('Ctrl Pts',(-2.09992975582247,53.7783345828611,11.9080769050163));
#46786=CARTESIAN_POINT('Ctrl Pts',(-2.25696948369581,53.7406047263216,12.1805000813266));
#46787=CARTESIAN_POINT('Ctrl Pts',(-2.45257708898085,53.6690720952781,12.7398788473275));
#46788=CARTESIAN_POINT('Ctrl Pts',(-2.49995067680506,53.6357011960875,13.0187081845893));
#46789=CARTESIAN_POINT('Ctrl Pts',(-2.49999996150753,53.6019333424293,13.2995612946774));
#46790=CARTESIAN_POINT('Ctrl Pts',(-2.49999996150753,53.6019333424293,13.2995612946774));
#46791=CARTESIAN_POINT('Ctrl Pts',(-2.49999998775002,53.6019153621539,13.2997108397542));
#46792=CARTESIAN_POINT('Ctrl Pts',(-2.5,53.6018985756711,13.2998504558639));
#46793=CARTESIAN_POINT('Ctrl Pts',(-2.5,53.601880595513,13.2999999999933));
#46794=CARTESIAN_POINT('Origin',(0.,70.2,13.3));
#46795=CARTESIAN_POINT('',(-2.5,51.768689088129,13.3));
#46796=CARTESIAN_POINT('',(-2.5,52.4544328862007,13.2999999995898));
#46797=CARTESIAN_POINT('',(-2.5,70.2,13.3));
#46798=CARTESIAN_POINT('Ctrl Pts',(-2.5,52.4544328862007,13.2999999991796));
#46799=CARTESIAN_POINT('Ctrl Pts',(-2.49999999992006,52.4942096580698,13.0563895109075));
#46800=CARTESIAN_POINT('Ctrl Pts',(-2.46439545171715,52.5345368483334,12.8140008047215));
#46801=CARTESIAN_POINT('Ctrl Pts',(-2.30070537491682,52.6234500099736,12.2692915759769));
#46802=CARTESIAN_POINT('Ctrl Pts',(-2.147508716278,52.6680607852065,11.9794028432668));
#46803=CARTESIAN_POINT('Ctrl Pts',(-1.84810007490051,52.7375150314633,11.6096789462031));
#46804=CARTESIAN_POINT('Ctrl Pts',(-1.74303612520946,52.7598253545768,11.5015421202317));
#46805=CARTESIAN_POINT('Ctrl Pts',(-1.51675776766793,52.8048938653409,11.3071849715741));
#46806=CARTESIAN_POINT('Ctrl Pts',(-1.39627322822478,52.8275433882984,11.2209922473548));
#46807=CARTESIAN_POINT('Ctrl Pts',(-1.05758175359877,52.8876127463687,11.0214751733709));
#46808=CARTESIAN_POINT('Ctrl Pts',(-0.828886735133715,52.9239955574636,
10.9286382373325));
#46809=CARTESIAN_POINT('Ctrl Pts',(-0.264221855574125,53.0058422648009,
10.7914922772734));
#46810=CARTESIAN_POINT('Ctrl Pts',(0.074144148524351,53.0515521422413,10.778707717533));
#46811=CARTESIAN_POINT('Ctrl Pts',(0.700533014429393,53.1433159233277,10.8815396724768));
#46812=CARTESIAN_POINT('Ctrl Pts',(0.984924941083911,53.1877492055136,10.9827586030877));
#46813=CARTESIAN_POINT('Ctrl Pts',(1.53106617933084,53.2780073671093,11.2962766464776));
#46814=CARTESIAN_POINT('Ctrl Pts',(1.7821939982874,53.322619800311,11.5158993287024));
#46815=CARTESIAN_POINT('Ctrl Pts',(2.08290058941423,53.3912612919028,11.90779082202));
#46816=CARTESIAN_POINT('Ctrl Pts',(2.16945461946802,53.4139721382326,12.0469279035097));
#46817=CARTESIAN_POINT('Ctrl Pts',(2.36753984400065,53.4760439036145,12.4482612832306));
#46818=CARTESIAN_POINT('Ctrl Pts',(2.44895659786436,53.5152035156178,12.7226276688593));
#46819=CARTESIAN_POINT('Ctrl Pts',(2.5220255039177,53.5989556973617,13.3371076043503));
#46820=CARTESIAN_POINT('Ctrl Pts',(2.49442606497016,53.6422366924613,13.6740224821022));
#46821=CARTESIAN_POINT('Ctrl Pts',(2.30976107345451,53.7316145808187,14.3115528646591));
#46822=CARTESIAN_POINT('Ctrl Pts',(2.15675044867975,53.7766768871334,14.6063719814992));
#46823=CARTESIAN_POINT('Ctrl Pts',(1.75355144184725,53.8643022791095,15.1096681853563));
#46824=CARTESIAN_POINT('Ctrl Pts',(1.51099909853781,53.9054716088556,15.3166330063897));
#46825=CARTESIAN_POINT('Ctrl Pts',(1.09610865819898,53.9684124584055,15.552673695711));
#46826=CARTESIAN_POINT('Ctrl Pts',(0.948591906231343,53.9896138414012,15.6186562571482));
#46827=CARTESIAN_POINT('Ctrl Pts',(0.480197868595057,54.0547280313389,15.7759261900835));
#46828=CARTESIAN_POINT('Ctrl Pts',(0.146584506599161,54.0984333203008,15.817814060565));
#46829=CARTESIAN_POINT('Ctrl Pts',(-0.51913771734361,54.1846857779829,15.7682872903183));
#46830=CARTESIAN_POINT('Ctrl Pts',(-0.844472258303415,54.2266669885973,
15.6767307406235));
#46831=CARTESIAN_POINT('Ctrl Pts',(-1.44195705231916,54.3127851301454,15.369868722278));
#46832=CARTESIAN_POINT('Ctrl Pts',(-1.70755417061573,54.3560029992327,15.1568383263904));
#46833=CARTESIAN_POINT('Ctrl Pts',(-2.13458258207599,54.441757663764,14.6428521509289));
#46834=CARTESIAN_POINT('Ctrl Pts',(-2.29353918990075,54.4832145497734,14.3485349460562));
#46835=CARTESIAN_POINT('Ctrl Pts',(-2.46318625238237,54.5563678179391,13.7943353265305));
#46836=CARTESIAN_POINT('Ctrl Pts',(-2.5,54.5874357260752,13.54769488302));
#46837=CARTESIAN_POINT('Ctrl Pts',(-2.5,54.6185115759899,13.3));
#46838=CARTESIAN_POINT('',(0.286897399705336,52.3546462541016,10.8159730008272));
#46839=CARTESIAN_POINT('Ctrl Pts',(-2.5,53.601880595513,13.2999999999933));
#46840=CARTESIAN_POINT('Ctrl Pts',(-2.50000000000064,53.5731131225576,13.5392641191748));
#46841=CARTESIAN_POINT('Ctrl Pts',(-2.46565160583379,53.5445458247303,13.7773194039659));
#46842=CARTESIAN_POINT('Ctrl Pts',(-2.339909469218,53.4918334916248,14.2038876647921));
#46843=CARTESIAN_POINT('Ctrl Pts',(-2.25777010751144,53.467827568561,14.3930116395779));
#46844=CARTESIAN_POINT('Ctrl Pts',(-1.9836209286351,53.4045220441114,14.8578746983225));
#46845=CARTESIAN_POINT('Ctrl Pts',(-1.75778464162242,53.3652473856669,15.1088530205023));
#46846=CARTESIAN_POINT('Ctrl Pts',(-1.24350967275062,53.2908752019447,15.4902761625381));
#46847=CARTESIAN_POINT('Ctrl Pts',(-0.966350613583913,53.2564059017049,
15.6258997525158));
#46848=CARTESIAN_POINT('Ctrl Pts',(-0.511099720078386,53.201969793668,15.7528629360861));
#46849=CARTESIAN_POINT('Ctrl Pts',(-0.346530686780513,53.1827388820718,
15.7814675360167));
#46850=CARTESIAN_POINT('Ctrl Pts',(0.151806240932969,53.125532032502,15.8175089616181));
#46851=CARTESIAN_POINT('Ctrl Pts',(0.4854494957925,53.0888957746755,15.7749317149148));
#46852=CARTESIAN_POINT('Ctrl Pts',(1.11783352102538,53.0144318994423,15.5610460638276));
#46853=CARTESIAN_POINT('Ctrl Pts',(1.41001520366356,52.9767114590674,15.3913618338837));
#46854=CARTESIAN_POINT('Ctrl Pts',(1.89550517844697,52.9055575406695,14.9601614973445));
#46855=CARTESIAN_POINT('Ctrl Pts',(2.08926806752941,52.8723934770927,14.7085612058889));
#46856=CARTESIAN_POINT('Ctrl Pts',(2.30418077339101,52.8203737657069,14.2833087793285));
#46857=CARTESIAN_POINT('Ctrl Pts',(2.36294884427428,52.8027429700754,14.1322437127345));
#46858=CARTESIAN_POINT('Ctrl Pts',(2.48645812186145,52.7537446260197,13.6928781057888));
#46859=CARTESIAN_POINT('Ctrl Pts',(2.51543151191713,52.7236489171256,13.3973254962775));
#46860=CARTESIAN_POINT('Ctrl Pts',(2.46604118017213,52.6585527230857,12.7708822172963));
#46861=CARTESIAN_POINT('Ctrl Pts',(2.37349349969795,52.623144414568,12.4468103461552));
#46862=CARTESIAN_POINT('Ctrl Pts',(2.07867279225929,52.5585387625586,11.8774673299877));
#46863=CARTESIAN_POINT('Ctrl Pts',(1.88820132051613,52.5294443406335,11.6329067702848));
#46864=CARTESIAN_POINT('Ctrl Pts',(1.4522969279502,52.4716038860416,11.2465932927216));
#46865=CARTESIAN_POINT('Ctrl Pts',(1.21767054179381,52.4444919352275,11.0993087674344));
#46866=CARTESIAN_POINT('Ctrl Pts',(0.747444085012265,52.3970136639375,10.9028660147942));
#46867=CARTESIAN_POINT('Ctrl Pts',(0.519589731567782,52.3764011794508,10.8433860242739));
#46868=CARTESIAN_POINT('Ctrl Pts',(0.286774387752517,52.3551642862145,10.8165023755741));
#46869=CARTESIAN_POINT('Ctrl Pts',(0.286877445958826,52.3542721930149,10.816514278076));
#46870=CARTESIAN_POINT('Ctrl Pts',(0.0534685891634007,52.3201799922785,
10.7895522802234));
#46871=CARTESIAN_POINT('Ctrl Pts',(-0.18266081179476,52.2862606553252,10.7956204292661));
#46872=CARTESIAN_POINT('Ctrl Pts',(-0.683558456558155,52.2146770321189,
10.8798405647647));
#46873=CARTESIAN_POINT('Ctrl Pts',(-0.943406753658285,52.1772598924145,
10.9688110113775));
#46874=CARTESIAN_POINT('Ctrl Pts',(-1.4516945793859,52.0964405945036,11.2420579055508));
#46875=CARTESIAN_POINT('Ctrl Pts',(-1.6911231432963,52.0535484484607,11.4338091393431));
#46876=CARTESIAN_POINT('Ctrl Pts',(-2.1101240378482,51.9649275935853,11.9178794987417));
#46877=CARTESIAN_POINT('Ctrl Pts',(-2.276600969804,51.9204574267858,12.2136993571353));
#46878=CARTESIAN_POINT('Ctrl Pts',(-2.45946237885603,51.839359618117,12.781485196561));
#46879=CARTESIAN_POINT('Ctrl Pts',(-2.5,51.8038794390372,13.0400814168076));
#46880=CARTESIAN_POINT('Ctrl Pts',(-2.5,51.768689088129,13.3));
#46881=CARTESIAN_POINT('Origin',(0.,70.2,13.3));
#46882=CARTESIAN_POINT('',(-2.5,49.7250834523465,13.3));
#46883=CARTESIAN_POINT('',(-2.5,50.7693915870611,13.3));
#46884=CARTESIAN_POINT('',(-2.5,70.2,13.3));
#46885=CARTESIAN_POINT('',(-2.38836719431143,52.3345987243418,14.039166525391));
#46886=CARTESIAN_POINT('Ctrl Pts',(-2.5,50.7693915870611,13.3));
#46887=CARTESIAN_POINT('Ctrl Pts',(-2.5,50.7725682780938,13.2734783251166));
#46888=CARTESIAN_POINT('Ctrl Pts',(-2.49957796284895,50.7757476555801,13.2469500982438));
#46889=CARTESIAN_POINT('Ctrl Pts',(-2.48841632301576,50.8177866315958,12.8964628064063));
#46890=CARTESIAN_POINT('Ctrl Pts',(-2.41519323296121,50.8563021021842,12.5775523474777));
#46891=CARTESIAN_POINT('Ctrl Pts',(-2.14875170210609,50.9338853896533,11.9802824721953));
#46892=CARTESIAN_POINT('Ctrl Pts',(-1.95610079506944,50.9720594824519,11.7086364044699));
#46893=CARTESIAN_POINT('Ctrl Pts',(-1.5070040047066,51.045941333298,11.2846108392235));
#46894=CARTESIAN_POINT('Ctrl Pts',(-1.26509151548325,51.0801655353141,11.124574871138));
#46895=CARTESIAN_POINT('Ctrl Pts',(-0.730537283946954,51.147916669297,10.8909381507117));
#46896=CARTESIAN_POINT('Ctrl Pts',(-0.441024149265621,51.1808843734047,
10.8215380968865));
#46897=CARTESIAN_POINT('Ctrl Pts',(0.187481298086497,51.2534729750946,10.7847442286701));
#46898=CARTESIAN_POINT('Ctrl Pts',(0.521694952288247,51.291995383055,10.832296344163));
#46899=CARTESIAN_POINT('Ctrl Pts',(1.14160679155934,51.3666808956943,11.052458057065));
#46900=CARTESIAN_POINT('Ctrl Pts',(1.42259703054374,51.4022470936342,11.2189164682836));
#46901=CARTESIAN_POINT('Ctrl Pts',(1.88099796831056,51.4727552274126,11.6277728686283));
#46902=CARTESIAN_POINT('Ctrl Pts',(2.06262362807787,51.5059263156767,11.8577059227597));
#46903=CARTESIAN_POINT('Ctrl Pts',(2.34314018473742,51.5704941531685,12.378117007052));
#46904=CARTESIAN_POINT('Ctrl Pts',(2.43682352816317,51.6012773454488,12.665924165674));
#46905=CARTESIAN_POINT('Ctrl Pts',(2.52134667315964,51.66994238345,13.2880912876859));
#46906=CARTESIAN_POINT('Ctrl Pts',(2.50122058728866,51.706676664711,13.61847547561));
#46907=CARTESIAN_POINT('Ctrl Pts',(2.34212047022356,51.7723260907281,14.2236805603188));
#46908=CARTESIAN_POINT('Ctrl Pts',(2.21555212298877,51.8012326111194,14.4958383739554));
#46909=CARTESIAN_POINT('Ctrl Pts',(1.85692002585776,51.8662425903497,15.0051465134759));
#46910=CARTESIAN_POINT('Ctrl Pts',(1.61951574509793,51.9012134617866,15.2321217609254));
#46911=CARTESIAN_POINT('Ctrl Pts',(1.0937158446704,51.962859639302,15.5677722942097));
#46912=CARTESIAN_POINT('Ctrl Pts',(0.815636928066772,51.9895830661086,15.6819558533277));
#46913=CARTESIAN_POINT('Ctrl Pts',(0.208048024794138,52.050481122095,15.8121921422632));
#46914=CARTESIAN_POINT('Ctrl Pts',(-0.118429000940584,52.083533541405,15.818077387983));
#46915=CARTESIAN_POINT('Ctrl Pts',(-0.723190307698781,52.1391610915244,
15.7106921402116));
#46916=CARTESIAN_POINT('Ctrl Pts',(-0.998037080650211,52.1620883105981,
15.6104670007487));
#46917=CARTESIAN_POINT('Ctrl Pts',(-1.53285632026417,52.2156576959321,15.3018320883281));
#46918=CARTESIAN_POINT('Ctrl Pts',(-1.78177453963372,52.246149476322,15.0840161997767));
#46919=CARTESIAN_POINT('Ctrl Pts',(-2.16284095185504,52.2949202092249,14.5885950881461));
#46920=CARTESIAN_POINT('Ctrl Pts',(-2.30043496719591,52.3136961116099,14.322847980847));
#46921=CARTESIAN_POINT('Ctrl Pts',(-2.38824601620833,52.3343772023775,14.0391082235133));
#46922=CARTESIAN_POINT('',(-2.49999907835137,52.4541831787799,13.3021466817004));
#46923=CARTESIAN_POINT('Ctrl Pts',(-2.38823974721953,52.3348094618126,14.039128479901));
#46924=CARTESIAN_POINT('Ctrl Pts',(-2.39249209790126,52.3367544905651,14.0253884696141));
#46925=CARTESIAN_POINT('Ctrl Pts',(-2.39661953396157,52.3390485561389,14.0116326761911));
#46926=CARTESIAN_POINT('Ctrl Pts',(-2.40062839257814,52.3413419978795,13.9978419024017));
#46927=CARTESIAN_POINT('Ctrl Pts',(-2.42328041852285,52.3543010734616,13.9199172371658));
#46928=CARTESIAN_POINT('Ctrl Pts',(-2.44212535260044,52.367239303345,13.8409335891714));
#46929=CARTESIAN_POINT('Ctrl Pts',(-2.45709519403956,52.3802030616442,13.761175896408));
#46930=CARTESIAN_POINT('Ctrl Pts',(-2.4721416566318,52.3932331732254,13.6810099744449));
#46931=CARTESIAN_POINT('Ctrl Pts',(-2.48322978256872,52.406256383375,13.6002940375464));
#46932=CARTESIAN_POINT('Ctrl Pts',(-2.49036063219162,52.4192841759952,13.5193260623595));
#46933=CARTESIAN_POINT('Ctrl Pts',(-2.49672451963419,52.4309107577132,13.4470666391785));
#46934=CARTESIAN_POINT('Ctrl Pts',(-2.49993685890941,52.4425409927571,13.374606677753));
#46935=CARTESIAN_POINT('Ctrl Pts',(-2.49999907835137,52.4541831787799,13.3021466817004));
#46936=CARTESIAN_POINT('Ctrl Pts',(-2.49999909203731,52.4540850015726,13.3021306836036));
#46937=CARTESIAN_POINT('Ctrl Pts',(-2.49999969735462,52.4542009600857,13.3014204454813));
#46938=CARTESIAN_POINT('Ctrl Pts',(-2.50000000000023,52.4543169216404,13.3007102172747));
#46939=CARTESIAN_POINT('Ctrl Pts',(-2.5,52.4544328862007,13.2999999991796));
#46940=CARTESIAN_POINT('',(-1.29179640210147,50.1461249705794,11.1593417706458));
#46941=CARTESIAN_POINT('Ctrl Pts',(-2.5,51.768689088129,13.3));
#46942=CARTESIAN_POINT('Ctrl Pts',(-2.5,51.7629474434776,13.3424082199945));
#46943=CARTESIAN_POINT('Ctrl Pts',(-2.49892094169084,51.7572160263818,13.3848519830099));
#46944=CARTESIAN_POINT('Ctrl Pts',(-2.47966187969698,51.7063255121688,13.762610749563));
#46945=CARTESIAN_POINT('Ctrl Pts',(-2.3951862990094,51.6625830605823,14.0911222396105));
#46946=CARTESIAN_POINT('Ctrl Pts',(-2.1164369446295,51.5778134849495,14.6644346748973));
#46947=CARTESIAN_POINT('Ctrl Pts',(-1.93651301242115,51.5377720997179,14.909640372495));
#46948=CARTESIAN_POINT('Ctrl Pts',(-1.60034318458678,51.4770039596661,15.2273759684802));
#46949=CARTESIAN_POINT('Ctrl Pts',(-1.47303267800506,51.4561009033281,15.3263417277534));
#46950=CARTESIAN_POINT('Ctrl Pts',(-1.06878369447911,51.3939318251766,15.5822202654902));
#46951=CARTESIAN_POINT('Ctrl Pts',(-0.770539737270521,51.353141705809,15.6994025429945));
#46952=CARTESIAN_POINT('Ctrl Pts',(-0.293525913282724,51.2907737945221,
15.7883625346195));
#46953=CARTESIAN_POINT('Ctrl Pts',(-0.126038071449243,51.2693639414798,
15.8024438062637));
#46954=CARTESIAN_POINT('Ctrl Pts',(0.203287682843875,51.2272633415639,15.7969629520643));
#46955=CARTESIAN_POINT('Ctrl Pts',(0.364338283359357,51.2066748147378,15.7785905382435));
#46956=CARTESIAN_POINT('Ctrl Pts',(0.849018184601001,51.1435978432017,15.6750074593532));
#46957=CARTESIAN_POINT('Ctrl Pts',(1.15831829398671,51.1018788792346,15.5404999244014));
#46958=CARTESIAN_POINT('Ctrl Pts',(1.69668112210125,51.0195170473709,15.1642659370116));
#46959=CARTESIAN_POINT('Ctrl Pts',(1.92300757144743,50.9796175269159,14.9298133782415));
#46960=CARTESIAN_POINT('Ctrl Pts',(2.18566631018747,50.9197137082865,14.5241669991209));
#46961=CARTESIAN_POINT('Ctrl Pts',(2.25968390187904,50.8999441277541,14.3814601295327));
#46962=CARTESIAN_POINT('Ctrl Pts',(2.44111483740834,50.8400732404914,13.9302334886086));
#46963=CARTESIAN_POINT('Ctrl Pts',(2.50241299235157,50.8005785073798,13.6069190536023));
#46964=CARTESIAN_POINT('Ctrl Pts',(2.49871746097642,50.7416018946686,13.1222708694074));
#46965=CARTESIAN_POINT('Ctrl Pts',(2.48240477128401,50.722412470282,12.96406939397));
#46966=CARTESIAN_POINT('Ctrl Pts',(2.41975546825254,50.6839698686371,12.6516407152287));
#46967=CARTESIAN_POINT('Ctrl Pts',(2.37332527689488,50.6648064992292,12.4981782058203));
#46968=CARTESIAN_POINT('Ctrl Pts',(2.18578563885437,50.6056495927986,12.0415610428059));
#46969=CARTESIAN_POINT('Ctrl Pts',(1.9984932814877,50.5661344829914,11.7613637016388));
#46970=CARTESIAN_POINT('Ctrl Pts',(1.64697059303443,50.5076987274167,11.4122406162932));
#46971=CARTESIAN_POINT('Ctrl Pts',(1.52144957518724,50.4887776532648,11.3096877666298));
#46972=CARTESIAN_POINT('Ctrl Pts',(1.11231307495995,50.4311138012836,11.0368872096299));
#46973=CARTESIAN_POINT('Ctrl Pts',(0.804131611952014,50.3928664901067,10.9099476749318));
#46974=CARTESIAN_POINT('Ctrl Pts',(0.329225561166609,50.3372175099223,10.8170049888917));
#46975=CARTESIAN_POINT('Ctrl Pts',(0.175883705644164,50.319673507889,10.8014562283027));
#46976=CARTESIAN_POINT('Ctrl Pts',(-0.217021322703808,50.2746726455672,
10.7979852562611));
#46977=CARTESIAN_POINT('Ctrl Pts',(-0.455224259394456,50.2474269416367,
10.8301880342919));
#46978=CARTESIAN_POINT('Ctrl Pts',(-0.898164367839591,50.1954873287541,
10.9564291233102));
#46979=CARTESIAN_POINT('Ctrl Pts',(-1.10210590474819,50.1709733136877,11.0451389016571));
#46980=CARTESIAN_POINT('Ctrl Pts',(-1.29169878399524,50.1463083191803,11.159552791722));
#46981=CARTESIAN_POINT('Ctrl Pts',(-1.29163435892636,50.1458351890062,11.1595139143548));
#46982=CARTESIAN_POINT('Ctrl Pts',(-1.46762460773575,50.1105095323541,11.2657117792802));
#46983=CARTESIAN_POINT('Ctrl Pts',(-1.62986516721391,50.0749704644603,11.393219411866));
#46984=CARTESIAN_POINT('Ctrl Pts',(-1.94536507579223,49.9990922641977,11.7112007736914));
#46985=CARTESIAN_POINT('Ctrl Pts',(-2.09010636036623,49.9604708810454,11.9070648993695));
#46986=CARTESIAN_POINT('Ctrl Pts',(-2.35338776298511,49.8708349028971,12.3993094134785));
#46987=CARTESIAN_POINT('Ctrl Pts',(-2.44820394406151,49.8195830419382,12.7033849088837));
#46988=CARTESIAN_POINT('Ctrl Pts',(-2.49465709755074,49.7543437774861,13.1111596643773));
#46989=CARTESIAN_POINT('Ctrl Pts',(-2.5,49.7395751853974,13.2056242711644));
#46990=CARTESIAN_POINT('Ctrl Pts',(-2.5,49.7250834523465,13.2999999999999));
#46991=CARTESIAN_POINT('Origin',(0.,70.2,13.3));
#46992=CARTESIAN_POINT('',(-2.5,47.5828357057113,13.3000000065378));
#46993=CARTESIAN_POINT('',(-2.5,48.7838403868077,13.299999999879));
#46994=CARTESIAN_POINT('',(-2.5,70.2,13.3));
#46995=CARTESIAN_POINT('',(-2.4999999894034,48.7838710165738,13.2997698196152));
#46996=CARTESIAN_POINT('Ctrl Pts',(-2.5,48.7838403868077,13.2999999997579));
#46997=CARTESIAN_POINT('Ctrl Pts',(-2.49999999999999,48.7838510363932,13.2999199689242));
#46998=CARTESIAN_POINT('Ctrl Pts',(-2.49999999615702,48.7838616860023,13.2998399380025));
#46999=CARTESIAN_POINT('Ctrl Pts',(-2.49999998847107,48.7838723356347,13.2997599069931));
#47000=CARTESIAN_POINT('Ctrl Pts',(-2.4999999894034,48.7838710165738,13.2997698196152));
#47001=CARTESIAN_POINT('Ctrl Pts',(-2.49997574528622,48.8189102305316,13.0364533222377));
#47002=CARTESIAN_POINT('Ctrl Pts',(-2.45835285905331,48.8540155824351,12.774780871668));
#47003=CARTESIAN_POINT('Ctrl Pts',(-2.28928258735442,48.9260073663749,12.2566873908404));
#47004=CARTESIAN_POINT('Ctrl Pts',(-2.15729167260878,48.962680734914,12.0056201297113));
#47005=CARTESIAN_POINT('Ctrl Pts',(-1.78503266972356,49.0435148904801,11.5185791184643));
#47006=CARTESIAN_POINT('Ctrl Pts',(-1.53344516837968,49.0862670222244,11.2979060528129));
#47007=CARTESIAN_POINT('Ctrl Pts',(-0.976340908060309,49.1702162853774,
10.9775845227962));
#47008=CARTESIAN_POINT('Ctrl Pts',(-0.679913943215935,49.2106048164309,
10.8741807152196));
#47009=CARTESIAN_POINT('Ctrl Pts',(-0.0538643248561953,49.2926435889597,
10.7799440859284));
#47010=CARTESIAN_POINT('Ctrl Pts',(0.270685388248418,49.3339325108916,10.7939412577153));
#47011=CARTESIAN_POINT('Ctrl Pts',(0.746092934661981,49.3969442602778,10.9080864923979));
#47012=CARTESIAN_POINT('Ctrl Pts',(0.904210893931087,49.4183681529807,10.9632694047121));
#47013=CARTESIAN_POINT('Ctrl Pts',(1.20169591364608,49.4605596397534,11.1018445214737));
#47014=CARTESIAN_POINT('Ctrl Pts',(1.3408343894498,49.4812203909971,11.1838417173814));
#47015=CARTESIAN_POINT('Ctrl Pts',(1.74148294898111,49.5447523390527,11.475429903687));
#47016=CARTESIAN_POINT('Ctrl Pts',(1.96965794407698,49.5866819322116,11.7244709889722));
#47017=CARTESIAN_POINT('Ctrl Pts',(2.3035072345252,49.6690421294183,12.279278766032));
#47018=CARTESIAN_POINT('Ctrl Pts',(2.41311500808524,49.7086718580359,12.5754945777285));
#47019=CARTESIAN_POINT('Ctrl Pts',(2.49255119753986,49.7691462220849,13.0464939837112));
#47020=CARTESIAN_POINT('Ctrl Pts',(2.50383101667476,49.7898790402248,13.2110631978932));
#47021=CARTESIAN_POINT('Ctrl Pts',(2.48876699441618,49.8527914321867,13.7093365956019));
#47022=CARTESIAN_POINT('Ctrl Pts',(2.41189695913903,49.8943888319195,14.0377567516765));
#47023=CARTESIAN_POINT('Ctrl Pts',(2.20582409122037,49.9565519988986,14.4875106276615));
#47024=CARTESIAN_POINT('Ctrl Pts',(2.12492163897261,49.9766894446145,14.6268578607494));
#47025=CARTESIAN_POINT('Ctrl Pts',(1.93541762073261,50.0174132607323,14.8909594056961));
#47026=CARTESIAN_POINT('Ctrl Pts',(1.82670587767699,50.0378968015838,15.0146842823719));
#47027=CARTESIAN_POINT('Ctrl Pts',(1.51696441892292,50.0907830912343,15.3040444892191));
#47028=CARTESIAN_POINT('Ctrl Pts',(1.30083833751125,50.1228859371001,15.4506283318528));
#47029=CARTESIAN_POINT('Ctrl Pts',(0.762507559903441,50.1968745761546,15.7044104100344));
#47030=CARTESIAN_POINT('Ctrl Pts',(0.433230957433051,50.2381038171472,15.7849436110871));
#47031=CARTESIAN_POINT('Ctrl Pts',(-0.1515114467204,50.3102707019366,15.8078546984625));
#47032=CARTESIAN_POINT('Ctrl Pts',(-0.400965222433192,50.3407507399289,
15.7802255237307));
#47033=CARTESIAN_POINT('Ctrl Pts',(-0.966146157028917,50.4128391759118,
15.6300073374752));
#47034=CARTESIAN_POINT('Ctrl Pts',(-1.26954502935261,50.4537469703206,15.4796029785403));
#47035=CARTESIAN_POINT('Ctrl Pts',(-1.76994747238211,50.5309283253864,15.0906410124269));
#47036=CARTESIAN_POINT('Ctrl Pts',(-1.97093128696611,50.5667926990972,14.8666983644878));
#47037=CARTESIAN_POINT('Ctrl Pts',(-2.30115625921089,50.6432443336031,14.3314327480784));
#47038=CARTESIAN_POINT('Ctrl Pts',(-2.41720417231426,50.6827743714643,14.0185729409194));
#47039=CARTESIAN_POINT('Ctrl Pts',(-2.48965734046885,50.7380156454991,13.5624242089609));
#47040=CARTESIAN_POINT('Ctrl Pts',(-2.5,50.7536658271994,13.4312918020845));
#47041=CARTESIAN_POINT('Ctrl Pts',(-2.5,50.7693915870611,13.3));
#47042=CARTESIAN_POINT('Ctrl Pts',(-2.5,49.7250834523465,13.2999999999999));
#47043=CARTESIAN_POINT('Ctrl Pts',(-2.50000000000001,49.6903982705044,13.5258832193953));
#47044=CARTESIAN_POINT('Ctrl Pts',(-2.46939640538158,49.6567888895813,13.7511788687082));
#47045=CARTESIAN_POINT('Ctrl Pts',(-2.32753734732961,49.5766501239402,14.2613220295873));
#47046=CARTESIAN_POINT('Ctrl Pts',(-2.19419348848113,49.5302683919951,14.5357830192452));
#47047=CARTESIAN_POINT('Ctrl Pts',(-1.91789616941836,49.4609289592335,14.9120140623529));
#47048=CARTESIAN_POINT('Ctrl Pts',(-1.80799082825554,49.4370358396022,15.0343884028129));
#47049=CARTESIAN_POINT('Ctrl Pts',(-1.46177996646387,49.3682292374493,15.3509041504178));
#47050=CARTESIAN_POINT('Ctrl Pts',(-1.20093128353508,49.3231151588567,15.5137705746146));
#47051=CARTESIAN_POINT('Ctrl Pts',(-0.604625773530855,49.2303253984791,
15.7489461068489));
#47052=CARTESIAN_POINT('Ctrl Pts',(-0.270477891234554,49.1857501758419,
15.8079524723122));
#47053=CARTESIAN_POINT('Ctrl Pts',(0.211777654371516,49.1186201656644,15.7953058242519));
#47054=CARTESIAN_POINT('Ctrl Pts',(0.357352633227321,49.0980103424572,15.7786439468728));
#47055=CARTESIAN_POINT('Ctrl Pts',(0.78740304282428,49.0351235627537,15.6907506695462));
#47056=CARTESIAN_POINT('Ctrl Pts',(1.06166772416961,48.9921157803747,15.5822247676385));
#47057=CARTESIAN_POINT('Ctrl Pts',(1.59682086504989,48.9029774494922,15.2526649230808));
#47058=CARTESIAN_POINT('Ctrl Pts',(1.8443772937165,48.8589548350079,15.0207937331081));
#47059=CARTESIAN_POINT('Ctrl Pts',(2.22984221920842,48.7677785303737,14.4776143496617));
#47060=CARTESIAN_POINT('Ctrl Pts',(2.36564142860816,48.7216196921004,14.1732696455439));
#47061=CARTESIAN_POINT('Ctrl Pts',(2.49828338508911,48.6375467068815,13.5867578797384));
#47062=CARTESIAN_POINT('Ctrl Pts',(2.5146696928622,48.6010656145741,13.3140065050327));
#47063=CARTESIAN_POINT('Ctrl Pts',(2.45262497002278,48.5203840757889,12.7116469996151));
#47064=CARTESIAN_POINT('Ctrl Pts',(2.3521838591124,48.4765720900617,12.3896289644743));
#47065=CARTESIAN_POINT('Ctrl Pts',(2.11339554843581,48.4106913930493,11.9546869439607));
#47066=CARTESIAN_POINT('Ctrl Pts',(2.02168512650663,48.3891711071079,11.8204398478526));
#47067=CARTESIAN_POINT('Ctrl Pts',(1.7026193999923,48.3232321701159,11.4389836398935));
#47068=CARTESIAN_POINT('Ctrl Pts',(1.4381010366275,48.279843063557,11.2277544124366));
#47069=CARTESIAN_POINT('Ctrl Pts',(0.844613033353298,48.192514944874,10.9237369856404));
#47070=CARTESIAN_POINT('Ctrl Pts',(0.522249665684434,48.1498093742071,10.8327578245077));
#47071=CARTESIAN_POINT('Ctrl Pts',(0.0309148217236938,48.0858638403156,
10.7950069533122));
#47072=CARTESIAN_POINT('Ctrl Pts',(-0.130513606119788,48.0650250082897,
10.7982173017314));
#47073=CARTESIAN_POINT('Ctrl Pts',(-0.451827532153677,48.0232626490109,
10.8358104321365));
#47074=CARTESIAN_POINT('Ctrl Pts',(-0.610925446739087,48.0024123387974,
10.8703596175259));
#47075=CARTESIAN_POINT('Ctrl Pts',(-1.08299660625344,47.9386852182676,11.0222118837479));
#47076=CARTESIAN_POINT('Ctrl Pts',(-1.37684940664384,47.8964615822085,11.1868232541413));
#47077=CARTESIAN_POINT('Ctrl Pts',(-1.73989261239969,47.8354714326538,11.4989253870466));
#47078=CARTESIAN_POINT('Ctrl Pts',(-1.84157450578367,47.8170194101915,11.6030316477075));
#47079=CARTESIAN_POINT('Ctrl Pts',(-2.14516061070636,47.7562049055104,11.9734840618113));
#47080=CARTESIAN_POINT('Ctrl Pts',(-2.30289297602479,47.7146384666952,12.2713687991248));
#47081=CARTESIAN_POINT('Ctrl Pts',(-2.46550448428009,47.6426728931688,12.8215874592548));
#47082=CARTESIAN_POINT('Ctrl Pts',(-2.50000000125408,47.612791848772,13.0602271230663));
#47083=CARTESIAN_POINT('Ctrl Pts',(-2.5,47.5828357057113,13.3000000130757));
#47084=CARTESIAN_POINT('Origin',(0.,70.2,13.3));
#47085=CARTESIAN_POINT('',(-2.4999999974205,45.6622550402693,13.3001106063177));
#47086=CARTESIAN_POINT('',(-2.5,46.4777801864859,13.3));
#47087=CARTESIAN_POINT('',(-2.5,70.2,13.3));
#47088=CARTESIAN_POINT('',(-1.87910183479348,46.6587897073237,11.6508024920329));
#47089=CARTESIAN_POINT('Ctrl Pts',(-2.5,46.4777801864859,13.3));
#47090=CARTESIAN_POINT('Ctrl Pts',(-2.5,46.4830105492051,13.2490202868915));
#47091=CARTESIAN_POINT('Ctrl Pts',(-2.49844064223901,46.4882548457263,13.1980275614499));
#47092=CARTESIAN_POINT('Ctrl Pts',(-2.47718908444389,46.5241995259477,12.8512180824113));
#47093=CARTESIAN_POINT('Ctrl Pts',(-2.40656458679348,46.5551780664903,12.5607941863735));
#47094=CARTESIAN_POINT('Ctrl Pts',(-2.18400029226825,46.6100024289926,12.0571541864303));
#47095=CARTESIAN_POINT('Ctrl Pts',(-2.0465266140265,46.6339946691803,11.8418305389474));
#47096=CARTESIAN_POINT('Ctrl Pts',(-1.87896154964605,46.6586668546072,11.6509082818255));
#47097=CARTESIAN_POINT('Ctrl Pts',(-1.87901788858152,46.6592025379051,11.6509724761573));
#47098=CARTESIAN_POINT('Ctrl Pts',(-1.74699164114983,46.6998851401868,11.500532488286));
#47099=CARTESIAN_POINT('Ctrl Pts',(-1.59720813559193,46.7391955629047,11.3663107355683));
#47100=CARTESIAN_POINT('Ctrl Pts',(-1.25403850047345,46.8210059840895,11.1262930418455));
#47101=CARTESIAN_POINT('Ctrl Pts',(-1.05944758583789,46.8632172518255,11.0250662714878));
#47102=CARTESIAN_POINT('Ctrl Pts',(-0.544166560882871,46.9645676849873,
10.8377624703872));
#47103=CARTESIAN_POINT('Ctrl Pts',(-0.214915533581655,47.0186313783139,
10.7874704793054));
#47104=CARTESIAN_POINT('Ctrl Pts',(0.276761682213298,47.1043207465961,10.8100873388383));
#47105=CARTESIAN_POINT('Ctrl Pts',(0.437519261792401,47.1328212176497,10.8332545201594));
#47106=CARTESIAN_POINT('Ctrl Pts',(0.885760131996727,47.21292858199,10.9430729957404));
#47107=CARTESIAN_POINT('Ctrl Pts',(1.16130971101538,47.2602483499833,11.0658987731741));
#47108=CARTESIAN_POINT('Ctrl Pts',(1.66921185219965,47.3586066748806,11.4124045837215));
#47109=CARTESIAN_POINT('Ctrl Pts',(1.89345795437946,47.410470043977,11.6374877762812));
#47110=CARTESIAN_POINT('Ctrl Pts',(2.24644783535437,47.5111516605348,12.1587326169901));
#47111=CARTESIAN_POINT('Ctrl Pts',(2.37215372753031,47.5573696330684,12.4502498929423));
#47112=CARTESIAN_POINT('Ctrl Pts',(2.4747600485298,47.6288937975688,12.9119953233282));
#47113=CARTESIAN_POINT('Ctrl Pts',(2.4943430314003,47.6527929533407,13.0692291393975));
#47114=CARTESIAN_POINT('Ctrl Pts',(2.50378384770508,47.7012700702939,13.3936681567683));
#47115=CARTESIAN_POINT('Ctrl Pts',(2.49199646048104,47.7258929996258,13.5601290139263));
#47116=CARTESIAN_POINT('Ctrl Pts',(2.43725263891949,47.7739830422757,13.8780890896514));
#47117=CARTESIAN_POINT('Ctrl Pts',(2.39639110721557,47.7973022583608,14.0291817578749));
#47118=CARTESIAN_POINT('Ctrl Pts',(2.2244785699268,47.8695901545692,14.4890030179992));
#47119=CARTESIAN_POINT('Ctrl Pts',(2.04556865224883,47.9148274738864,14.7757189017264));
#47120=CARTESIAN_POINT('Ctrl Pts',(1.61883799436477,48.0030114602919,15.2264157643961));
#47121=CARTESIAN_POINT('Ctrl Pts',(1.38818249737406,48.0448566395512,15.3987030382261));
#47122=CARTESIAN_POINT('Ctrl Pts',(0.839139340630911,48.1340437022763,15.6780182320207));
#47123=CARTESIAN_POINT('Ctrl Pts',(0.517942830195246,48.1784860240865,15.7679950903323));
#47124=CARTESIAN_POINT('Ctrl Pts',(0.0340986027569455,48.2451128817299,
15.8045479509993));
#47125=CARTESIAN_POINT('Ctrl Pts',(-0.120860399820526,48.266421357235,15.8018601577716));
#47126=CARTESIAN_POINT('Ctrl Pts',(-0.43290277621311,48.3101123509077,15.7673820577644));
#47127=CARTESIAN_POINT('Ctrl Pts',(-0.589208928960504,48.3324054043071,
15.7347917179916));
#47128=CARTESIAN_POINT('Ctrl Pts',(-1.06106293249441,48.4011291534717,15.588278470483));
#47129=CARTESIAN_POINT('Ctrl Pts',(-1.35762355331889,48.4457745713593,15.4257913365375));
#47130=CARTESIAN_POINT('Ctrl Pts',(-1.73500600029322,48.5132396489618,15.1069565607301));
#47131=CARTESIAN_POINT('Ctrl Pts',(-1.84652571753528,48.5349543464534,14.9928360831729));
#47132=CARTESIAN_POINT('Ctrl Pts',(-2.12160124238921,48.5941076542015,14.651559193866));
#47133=CARTESIAN_POINT('Ctrl Pts',(-2.25914295898414,48.6312127057787,14.4064310035721));
#47134=CARTESIAN_POINT('Ctrl Pts',(-2.40004964397745,48.6874862202398,14.0133847018049));
#47135=CARTESIAN_POINT('Ctrl Pts',(-2.43586215021993,48.7060956575831,13.8794306460086));
#47136=CARTESIAN_POINT('Ctrl Pts',(-2.48674785730144,48.7443900574573,13.5969335522108));
#47137=CARTESIAN_POINT('Ctrl Pts',(-2.50000000001439,48.7640641411391,13.4486169967807));
#47138=CARTESIAN_POINT('Ctrl Pts',(-2.5,48.7838403868077,13.2999999997579));
#47139=CARTESIAN_POINT('',(-1.95241364042681,45.9847503099714,11.7382273262856));
#47140=CARTESIAN_POINT('Ctrl Pts',(-2.5,47.5828357057113,13.3000000130757));
#47141=CARTESIAN_POINT('Ctrl Pts',(-2.49999999988754,47.580149426164,13.3215013461792));
#47142=CARTESIAN_POINT('Ctrl Pts',(-2.49972261604871,47.5774625853922,13.3430117973173));
#47143=CARTESIAN_POINT('Ctrl Pts',(-2.49064932102071,47.5335626046913,13.694430775638));
#47144=CARTESIAN_POINT('Ctrl Pts',(-2.41689054183271,47.4928768995489,14.0194297820736));
#47145=CARTESIAN_POINT('Ctrl Pts',(-2.21590428308462,47.4319732142735,14.4687935698638));
#47146=CARTESIAN_POINT('Ctrl Pts',(-2.13542073530784,47.4120208351259,14.6100742067107));
#47147=CARTESIAN_POINT('Ctrl Pts',(-1.86622631964636,47.3547396476907,14.9910932697066));
#47148=CARTESIAN_POINT('Ctrl Pts',(-1.64672079606039,47.3180163680394,15.2054990699382));
#47149=CARTESIAN_POINT('Ctrl Pts',(-1.1240201231474,47.2412721013692,15.5566442994732));
#47150=CARTESIAN_POINT('Ctrl Pts',(-0.82107028701758,47.202049173162,15.6836418282125));
#47151=CARTESIAN_POINT('Ctrl Pts',(-0.348087286477959,47.1439686671439,
15.7806469592988));
#47152=CARTESIAN_POINT('Ctrl Pts',(-0.19125206581969,47.1251608335839,15.7976388201433));
#47153=CARTESIAN_POINT('Ctrl Pts',(0.30112414241352,47.0661834403037,15.8043080367654));
#47154=CARTESIAN_POINT('Ctrl Pts',(0.633656549999821,47.0262185349478,15.7414654240893));
#47155=CARTESIAN_POINT('Ctrl Pts',(1.23211609927269,46.9497561628566,15.4974418996739));
#47156=CARTESIAN_POINT('Ctrl Pts',(1.49585027002142,46.9138741700829,15.3271423933475));
#47157=CARTESIAN_POINT('Ctrl Pts',(1.95245580769975,46.8397792533204,14.8935256422817));
#47158=CARTESIAN_POINT('Ctrl Pts',(2.13939672991357,46.8026790523447,14.6320864962856));
#47159=CARTESIAN_POINT('Ctrl Pts',(2.33801366848224,46.7478665454617,14.1992046869808));
#47160=CARTESIAN_POINT('Ctrl Pts',(2.39007607071443,46.7298967541087,14.0499438109266));
#47161=CARTESIAN_POINT('Ctrl Pts',(2.50758575779311,46.6734948504716,13.5719024989991));
#47162=CARTESIAN_POINT('Ctrl Pts',(2.5214364021705,46.6349281579702,13.2342557529887));
#47163=CARTESIAN_POINT('Ctrl Pts',(2.41883814181262,46.5618299390585,12.5949272678783));
#47164=CARTESIAN_POINT('Ctrl Pts',(2.31169697158706,46.5277144725562,12.2980148716835));
#47165=CARTESIAN_POINT('Ctrl Pts',(2.06963958082871,46.4742334299024,11.8882013837772));
#47166=CARTESIAN_POINT('Ctrl Pts',(1.973178442969,46.4559226114626,11.7562514514113));
#47167=CARTESIAN_POINT('Ctrl Pts',(1.66895942718863,46.4052547431179,11.4156482224247));
#47168=CARTESIAN_POINT('Ctrl Pts',(1.43630474427017,46.374001177999,11.2328084599424));
#47169=CARTESIAN_POINT('Ctrl Pts',(0.882482661220567,46.3064936411012,10.9371963448682));
#47170=CARTESIAN_POINT('Ctrl Pts',(0.559159106126154,46.2698835019907,10.8405253564252));
#47171=CARTESIAN_POINT('Ctrl Pts',(-0.07844214110819,46.2024042558339,10.7825577128121));
#47172=CARTESIAN_POINT('Ctrl Pts',(-0.385755012755789,46.1718357764588,
10.8110474174565));
#47173=CARTESIAN_POINT('Ctrl Pts',(-0.949126279226214,46.1109526265218,
10.9703629760132));
#47174=CARTESIAN_POINT('Ctrl Pts',(-1.20341881472457,46.0820057444069,11.090943154281));
#47175=CARTESIAN_POINT('Ctrl Pts',(-1.62814787306659,46.0306164683876,11.3879041868699));
#47176=CARTESIAN_POINT('Ctrl Pts',(-1.80315871885665,46.0080357480293,11.5519756553128));
#47177=CARTESIAN_POINT('Ctrl Pts',(-1.95225418005292,45.9848322558052,11.7383650822084));
#47178=CARTESIAN_POINT('Ctrl Pts',(-1.95219597877177,45.9842543345744,11.73829232554));
#47179=CARTESIAN_POINT('Ctrl Pts',(-2.12796165206232,45.9271257317385,11.9580063259355));
#47180=CARTESIAN_POINT('Ctrl Pts',(-2.26566846203269,45.8714534636839,12.2062796187581));
#47181=CARTESIAN_POINT('Ctrl Pts',(-2.45229591942592,45.7631222498252,12.7381805495956));
#47182=CARTESIAN_POINT('Ctrl Pts',(-2.50000000001646,45.7131063519431,13.0178816481088));
#47183=CARTESIAN_POINT('Ctrl Pts',(-2.5,45.6622749689603,13.3000000001458));
#47184=CARTESIAN_POINT('Origin',(0.,70.2,13.3));
#47185=CARTESIAN_POINT('',(-2.5,43.4016964318852,13.3));
#47186=CARTESIAN_POINT('Ctrl Pts',(-2.49999999728054,45.6622539589675,13.3001166074741));
#47187=CARTESIAN_POINT('Ctrl Pts',(-2.49998664111617,45.6106604689999,13.5864654126283));
#47188=CARTESIAN_POINT('Ctrl Pts',(-2.45078497592242,45.5605981192958,13.8709891497258));
#47189=CARTESIAN_POINT('Ctrl Pts',(-2.24983810586681,45.4604737620495,14.4333224109686));
#47190=CARTESIAN_POINT('Ctrl Pts',(-2.09195269470515,45.4086587772158,14.7035850380949));
#47191=CARTESIAN_POINT('Ctrl Pts',(-1.68198748850155,45.3064765619204,15.1762625889758));
#47192=CARTESIAN_POINT('Ctrl Pts',(-1.43193516873979,45.2562510834677,15.3734451691347));
#47193=CARTESIAN_POINT('Ctrl Pts',(-0.875083021048201,45.1566278827318,
15.662508131224));
#47194=CARTESIAN_POINT('Ctrl Pts',(-0.574044701395826,45.1112015984706,
15.7531198772918));
#47195=CARTESIAN_POINT('Ctrl Pts',(0.0422675366606626,45.0182474319853,
15.8185227476926));
#47196=CARTESIAN_POINT('Ctrl Pts',(0.351594189057949,44.9707018991942,15.7941971063011));
#47197=CARTESIAN_POINT('Ctrl Pts',(0.974006309437163,44.8742410321479,15.6269684377271));
#47198=CARTESIAN_POINT('Ctrl Pts',(1.27837052541315,44.8274949233512,15.4747111513947));
#47199=CARTESIAN_POINT('Ctrl Pts',(1.76609381912382,44.7364782702921,15.0919199708914));
#47200=CARTESIAN_POINT('Ctrl Pts',(1.9574996528276,44.6942642651608,14.8806308671294));
#47201=CARTESIAN_POINT('Ctrl Pts',(2.19626282599974,44.6307703526445,14.5052293408213));
#47202=CARTESIAN_POINT('Ctrl Pts',(2.26961685394048,44.6081147478852,14.3606626821417));
#47203=CARTESIAN_POINT('Ctrl Pts',(2.44389497539902,44.5406851690895,13.9147221371947));
#47204=CARTESIAN_POINT('Ctrl Pts',(2.50207812577016,44.4961668043628,13.6001750912055));
#47205=CARTESIAN_POINT('Ctrl Pts',(2.49767576479121,44.4048307230385,12.9464434015316));
#47206=CARTESIAN_POINT('Ctrl Pts',(2.42740886800472,44.360108503826,12.6136318761029));
#47207=CARTESIAN_POINT('Ctrl Pts',(2.17739961569252,44.272955151226,12.0375697022272));
#47208=CARTESIAN_POINT('Ctrl Pts',(2.01566261751725,44.2319988345987,11.7926948973962));
#47209=CARTESIAN_POINT('Ctrl Pts',(1.59635476843331,44.1486730222525,11.3498389243424));
#47210=CARTESIAN_POINT('Ctrl Pts',(1.33506313530245,44.1062760606926,11.1624410516961));
#47211=CARTESIAN_POINT('Ctrl Pts',(0.75828226891258,44.0209097855453,10.8968640038899));
#47212=CARTESIAN_POINT('Ctrl Pts',(0.448433039469844,43.9781994253374,10.8202922877834));
#47213=CARTESIAN_POINT('Ctrl Pts',(-0.201557863363527,43.8908353903719,
10.7857725748925));
#47214=CARTESIAN_POINT('Ctrl Pts',(-0.535922828130152,43.8472982241007,
10.8352900581576));
#47215=CARTESIAN_POINT('Ctrl Pts',(-1.1613401152287,43.7588818971409,11.0615921907786));
#47216=CARTESIAN_POINT('Ctrl Pts',(-1.44672243022223,43.715966191786,11.2345198571569));
#47217=CARTESIAN_POINT('Ctrl Pts',(-1.80873444394829,43.6512782533907,11.5666939944687));
#47218=CARTESIAN_POINT('Ctrl Pts',(-1.91647670182185,43.6300914126777,11.6866220255007));
#47219=CARTESIAN_POINT('Ctrl Pts',(-2.21038599525522,43.5650433675776,12.0851112037626));
#47220=CARTESIAN_POINT('Ctrl Pts',(-2.3528632622903,43.5220521048097,12.3912576082094));
#47221=CARTESIAN_POINT('Ctrl Pts',(-2.47691254645397,43.4525796362456,12.9079271234051));
#47222=CARTESIAN_POINT('Ctrl Pts',(-2.5,43.4270730771034,13.1038350369808));
#47223=CARTESIAN_POINT('Ctrl Pts',(-2.5,43.4016964318852,13.3));
#47224=CARTESIAN_POINT('',(-2.50002611214299,44.6193946092241,13.2998651846547));
#47225=CARTESIAN_POINT('',(-2.5,70.2,13.3));
#47226=CARTESIAN_POINT('Ctrl Pts',(-2.49999999639604,44.6193990784213,13.2998657621837));
#47227=CARTESIAN_POINT('Ctrl Pts',(-2.49999100145858,44.6409901617092,13.1323470686192));
#47228=CARTESIAN_POINT('Ctrl Pts',(-2.48314441819972,44.6624023350778,12.965242875278));
#47229=CARTESIAN_POINT('Ctrl Pts',(-2.41797240101115,44.7042228684327,12.645248990369));
#47230=CARTESIAN_POINT('Ctrl Pts',(-2.37143889695187,44.7245287023665,12.4928019948569));
#47231=CARTESIAN_POINT('Ctrl Pts',(-2.18409069381321,44.7872598979828,12.0391052509022));
#47232=CARTESIAN_POINT('Ctrl Pts',(-1.99762736346973,44.8289540052538,11.7606413626008));
#47233=CARTESIAN_POINT('Ctrl Pts',(-1.6499239108512,44.8909851826536,11.4151083239769));
#47234=CARTESIAN_POINT('Ctrl Pts',(-1.52727392969976,44.910955647363,11.3144264890428));
#47235=CARTESIAN_POINT('Ctrl Pts',(-1.12680585458803,44.9718631052918,11.0448848129115));
#47236=CARTESIAN_POINT('Ctrl Pts',(-0.824963188572854,45.0121601453836,
10.9178359801667));
#47237=CARTESIAN_POINT('Ctrl Pts',(-0.193166708270342,45.092687514167,10.7869188662199));
#47238=CARTESIAN_POINT('Ctrl Pts',(0.130555871776583,45.1322023431919,10.7828845587215));
#47239=CARTESIAN_POINT('Ctrl Pts',(0.6110651145995,45.1926497638151,10.8700470275991));
#47240=CARTESIAN_POINT('Ctrl Pts',(0.772505911741462,45.2132826631378,10.9164498203768));
#47241=CARTESIAN_POINT('Ctrl Pts',(1.22047443871637,45.2726551871119,11.0955513659098));
#47242=CARTESIAN_POINT('Ctrl Pts',(1.4881722943468,45.3108153377255,11.2666486023629));
#47243=CARTESIAN_POINT('Ctrl Pts',(1.96020347156416,45.3900826946697,11.7127038147139));
#47244=CARTESIAN_POINT('Ctrl Pts',(2.15479685788948,45.4304878677962,11.9889690111091));
#47245=CARTESIAN_POINT('Ctrl Pts',(2.35152892376341,45.4894170845314,12.4372568622078));
#47246=CARTESIAN_POINT('Ctrl Pts',(2.4004766743675,45.5079360915437,12.5846471038827));
#47247=CARTESIAN_POINT('Ctrl Pts',(2.51074327011427,45.5663738945558,13.0604826415139));
#47248=CARTESIAN_POINT('Ctrl Pts',(2.52027469121408,45.606157467725,13.3971634017789));
#47249=CARTESIAN_POINT('Ctrl Pts',(2.43701399373081,45.6641806090174,13.8788750633255));
#47250=CARTESIAN_POINT('Ctrl Pts',(2.39634217504537,45.6824450932429,14.0291676522049));
#47251=CARTESIAN_POINT('Ctrl Pts',(2.2873235497184,45.7189880718122,14.3210540672638));
#47252=CARTESIAN_POINT('Ctrl Pts',(2.21907468010472,45.7371867695919,14.4619410912828));
#47253=CARTESIAN_POINT('Ctrl Pts',(1.96668954146464,45.7943870256208,14.8784732453492));
#47254=CARTESIAN_POINT('Ctrl Pts',(1.74075136704802,45.8330427646287,15.1246358015802));
#47255=CARTESIAN_POINT('Ctrl Pts',(1.20657239910928,45.9092064476877,15.5143347371929));
#47256=CARTESIAN_POINT('Ctrl Pts',(0.903774907157531,45.94648570611,15.6542057950761));
#47257=CARTESIAN_POINT('Ctrl Pts',(0.29484300743038,46.0185762956438,15.8001221323276));
#47258=CARTESIAN_POINT('Ctrl Pts',(-0.00291286656667483,46.0518804236423,
15.817460744914));
#47259=CARTESIAN_POINT('Ctrl Pts',(-0.453161161170635,46.1023490630304,
15.7636226737825));
#47260=CARTESIAN_POINT('Ctrl Pts',(-0.607379572154865,46.1197172591066,
15.7302015365156));
#47261=CARTESIAN_POINT('Ctrl Pts',(-1.06786022589398,46.1737629291231,15.5838090281928));
#47262=CARTESIAN_POINT('Ctrl Pts',(-1.35612248569427,46.2101726162091,15.4253567197509));
#47263=CARTESIAN_POINT('Ctrl Pts',(-1.85627153822428,46.2810207370737,15.0061606385636));
#47264=CARTESIAN_POINT('Ctrl Pts',(-2.06311401634006,46.3155215088971,14.7492349693685));
#47265=CARTESIAN_POINT('Ctrl Pts',(-2.35137090934781,46.3830590275481,14.1988172104408));
#47266=CARTESIAN_POINT('Ctrl Pts',(-2.44089286653981,46.4141758958576,13.9156024449375));
#47267=CARTESIAN_POINT('Ctrl Pts',(-2.49299721967078,46.45566800665,13.5160100875658));
#47268=CARTESIAN_POINT('Ctrl Pts',(-2.5,46.4666961661161,13.4080346065628));
#47269=CARTESIAN_POINT('Ctrl Pts',(-2.5,46.4777801864859,13.3));
#47270=CARTESIAN_POINT('Origin',(0.,70.2,13.3));
#47271=CARTESIAN_POINT('',(-2.5,41.4625301506567,13.3));
#47272=CARTESIAN_POINT('',(-2.5,42.3946776132135,13.2999999999965));
#47273=CARTESIAN_POINT('',(-2.5,70.2,13.3));
#47274=CARTESIAN_POINT('',(-2.49999999975899,42.3946815632985,13.2999652863836));
#47275=CARTESIAN_POINT('Ctrl Pts',(-2.5,42.3946776132135,13.2999999999929));
#47276=CARTESIAN_POINT('Ctrl Pts',(-2.5,42.3946793067792,13.2999851168335));
#47277=CARTESIAN_POINT('Ctrl Pts',(-2.49999999996565,42.3946798697338,13.2999801695507));
#47278=CARTESIAN_POINT('Ctrl Pts',(-2.49999999975899,42.3946815632985,13.2999652863836));
#47279=CARTESIAN_POINT('',(-2.34562647967194,42.4937495273014,12.438593281029));
#47280=CARTESIAN_POINT('Ctrl Pts',(-2.49999999975899,42.3946815632985,13.2999652863836));
#47281=CARTESIAN_POINT('Ctrl Pts',(-2.49999796332142,42.4113700776466,13.1533054315592));
#47282=CARTESIAN_POINT('Ctrl Pts',(-2.48709055897572,42.4279012816079,13.0069169709822));
#47283=CARTESIAN_POINT('Ctrl Pts',(-2.46141993395718,42.4443477685325,12.8624935329413));
#47284=CARTESIAN_POINT('Ctrl Pts',(-2.43572996625103,42.4608066478028,12.7179612725618));
#47285=CARTESIAN_POINT('Ctrl Pts',(-2.39735907207736,42.4771173025678,12.5759685022323));
#47286=CARTESIAN_POINT('Ctrl Pts',(-2.3467496852355,42.4934796045645,12.4381613173876));
#47287=CARTESIAN_POINT('Ctrl Pts',(-2.34568410818789,42.4936477083913,12.4384943467529));
#47288=CARTESIAN_POINT('Ctrl Pts',(-2.32319243510089,42.5044066341044,12.3767211629903));
#47289=CARTESIAN_POINT('Ctrl Pts',(-2.29816641170027,42.5154051459049,12.3160036445523));
#47290=CARTESIAN_POINT('Ctrl Pts',(-2.27084402275472,42.5264576965297,12.2564468004019));
#47291=CARTESIAN_POINT('Ctrl Pts',(-2.26153191904919,42.5302246620698,12.2361484469084));
#47292=CARTESIAN_POINT('Ctrl Pts',(-2.25195285533498,42.5339979531538,12.2159845285737));
#47293=CARTESIAN_POINT('Ctrl Pts',(-2.24211553933993,42.5377703748663,12.1959580269618));
#47294=CARTESIAN_POINT('Ctrl Pts',(-2.20303425107432,42.5527572981777,12.1163975571304));
#47295=CARTESIAN_POINT('Ctrl Pts',(-2.15988069017721,42.5677305682467,12.039004668424));
#47296=CARTESIAN_POINT('Ctrl Pts',(-2.11284707137413,42.5826925682951,11.9641262426941));
#47297=CARTESIAN_POINT('Ctrl Pts',(-2.06625695767561,42.5975134836564,11.8899538856205));
#47298=CARTESIAN_POINT('Ctrl Pts',(-2.01585996950672,42.6123230568688,11.8182484823373));
#47299=CARTESIAN_POINT('Ctrl Pts',(-1.96181183979858,42.6270945088235,11.7493389656302));
#47300=CARTESIAN_POINT('Ctrl Pts',(-1.91893037685003,42.6388140904837,11.6946665670952));
#47301=CARTESIAN_POINT('Ctrl Pts',(-1.87375012255244,42.650509046783,11.641753753135));
#47302=CARTESIAN_POINT('Ctrl Pts',(-1.826332024504,42.6621547426356,11.5907643122431));
#47303=CARTESIAN_POINT('Ctrl Pts',(-1.77150630319007,42.6756197212323,11.5318093353177));
#47304=CARTESIAN_POINT('Ctrl Pts',(-1.71395546762424,42.6889535887934,11.4757108190844));
#47305=CARTESIAN_POINT('Ctrl Pts',(-1.65382295290227,42.7021077324741,11.4226417084105));
#47306=CARTESIAN_POINT('Ctrl Pts',(-1.64790473396646,42.7034023582281,11.4174186669803));
#47307=CARTESIAN_POINT('Ctrl Pts',(-1.64196146632311,42.7046952453212,11.4122249735563));
#47308=CARTESIAN_POINT('Ctrl Pts',(-1.63599325951888,42.7059863488698,11.4070607964659));
#47309=CARTESIAN_POINT('Ctrl Pts',(-1.60759618180394,42.7121294952131,11.3824893392459));
#47310=CARTESIAN_POINT('Ctrl Pts',(-1.578634839558,42.7182320534431,11.3585859512818));
#47311=CARTESIAN_POINT('Ctrl Pts',(-1.54912007543092,42.7242885560419,11.3353687778235));
#47312=CARTESIAN_POINT('Ctrl Pts',(-1.54906789469659,42.7242992636576,11.3353277309375));
#47313=CARTESIAN_POINT('Ctrl Pts',(-1.54901571223328,42.7243099711298,11.3352866861985));
#47314=CARTESIAN_POINT('Ctrl Pts',(-1.54896352804101,42.7243206784584,11.3352456436066));
#47315=CARTESIAN_POINT('Ctrl Pts',(-1.4852389421749,42.7373959040039,11.2851265931339));
#47316=CARTESIAN_POINT('Ctrl Pts',(-1.41893687593455,42.7502574375949,11.2382051472508));
#47317=CARTESIAN_POINT('Ctrl Pts',(-1.35033349917278,42.7630133468244,11.1945851413839));
#47318=CARTESIAN_POINT('Ctrl Pts',(-1.34666103087231,42.7636961947322,11.1922500801031));
#47319=CARTESIAN_POINT('Ctrl Pts',(-1.34298196643404,42.764378739025,11.1899244918653));
#47320=CARTESIAN_POINT('Ctrl Pts',(-1.33929634791449,42.7650609959637,11.1876083967253));
#47321=CARTESIAN_POINT('Ctrl Pts',(-1.26884491142833,42.7781024925612,11.1433357112092));
#47322=CARTESIAN_POINT('Ctrl Pts',(-1.19599798804975,42.7910398549919,11.10252762203));
#47323=CARTESIAN_POINT('Ctrl Pts',(-1.12105332117687,42.8039678222148,11.06533510557));
#47324=CARTESIAN_POINT('Ctrl Pts',(-1.11678133648451,42.8047047402689,11.0632150633092));
#47325=CARTESIAN_POINT('Ctrl Pts',(-1.11250253714567,42.805441626814,11.0611067827626));
#47326=CARTESIAN_POINT('Ctrl Pts',(-1.10821697898267,42.8061784990389,11.0590102969284));
#47327=CARTESIAN_POINT('Ctrl Pts',(-1.07812049158259,42.8113533828664,11.0442871600362));
#47328=CARTESIAN_POINT('Ctrl Pts',(-1.04769071115196,42.8165273203326,11.0301453979786));
#47329=CARTESIAN_POINT('Ctrl Pts',(-1.01694738227775,42.8217052392388,11.0165962399779));
#47330=CARTESIAN_POINT('Ctrl Pts',(-0.93670336909343,42.8352202686189,10.9812312078537));
#47331=CARTESIAN_POINT('Ctrl Pts',(-0.854743063674407,42.8486949837781,
10.9500878614058));
#47332=CARTESIAN_POINT('Ctrl Pts',(-0.771477953212197,42.8621921408794,
10.9232487200998));
#47333=CARTESIAN_POINT('Ctrl Pts',(-0.686960198914593,42.8758923497817,
10.8960058096193));
#47334=CARTESIAN_POINT('Ctrl Pts',(-0.601098315861208,42.889615710475,10.8731980714603));
#47335=CARTESIAN_POINT('Ctrl Pts',(-0.51431293246352,42.9033902912299,10.8549208363218));
#47336=CARTESIAN_POINT('Ctrl Pts',(-0.427674693022967,42.917141517288,10.8366745900964));
#47337=CARTESIAN_POINT('Ctrl Pts',(-0.340116556399769,42.9309436015435,
10.8229435031144));
#47338=CARTESIAN_POINT('Ctrl Pts',(-0.25204183770853,42.9447886797666,10.8138274198997));
#47339=CARTESIAN_POINT('Ctrl Pts',(-0.182662170169835,42.9556949527408,
10.8066463487354));
#47340=CARTESIAN_POINT('Ctrl Pts',(-0.112961714143479,42.9666271453375,
10.8023289442864));
#47341=CARTESIAN_POINT('Ctrl Pts',(-0.0431280667894809,42.9775671581277,
10.8009278439028));
#47342=CARTESIAN_POINT('Ctrl Pts',(0.0381176356362617,42.9902949628087,
10.7992977788962));
#47343=CARTESIAN_POINT('Ctrl Pts',(0.119146921010516,43.0029718850833,10.8016226020268));
#47344=CARTESIAN_POINT('Ctrl Pts',(0.199692924382387,43.0155519372969,10.8078810650787));
#47345=CARTESIAN_POINT('Ctrl Pts',(0.207357072027646,43.0167489597873,10.8084765730227));
#47346=CARTESIAN_POINT('Ctrl Pts',(0.215016870767598,43.017945107523,10.8091077243278));
#47347=CARTESIAN_POINT('Ctrl Pts',(0.222672106946552,43.0191403423437,10.8097745190492));
#47348=CARTESIAN_POINT('Ctrl Pts',(0.300986738960001,43.0313678390491,10.8165959654443));
#47349=CARTESIAN_POINT('Ctrl Pts',(0.378821715553078,43.0434991211718,10.827143874682));
#47350=CARTESIAN_POINT('Ctrl Pts',(0.455967538276286,43.0554802484494,10.8414244650109));
#47351=CARTESIAN_POINT('Ctrl Pts',(0.46504699424431,43.056890332803,10.843105178062));
#47352=CARTESIAN_POINT('Ctrl Pts',(0.474116936893891,43.0582983414146,10.8448376437622));
#47353=CARTESIAN_POINT('Ctrl Pts',(0.483177049511238,43.0597041896624,10.8466219132699));
#47354=CARTESIAN_POINT('Ctrl Pts',(0.499926919556773,43.0623032495691,10.8499205789316));
#47355=CARTESIAN_POINT('Ctrl Pts',(0.516643191327323,43.0648948743572,10.8533962415694));
#47356=CARTESIAN_POINT('Ctrl Pts',(0.533323908054583,43.0674784687919,10.8570492350127));
#47357=CARTESIAN_POINT('Ctrl Pts',(0.533345151962504,43.0674817591566,10.8570538873222));
#47358=CARTESIAN_POINT('Ctrl Pts',(0.53336639581264,43.0674850495084,10.8570585399193));
#47359=CARTESIAN_POINT('Ctrl Pts',(0.53338763960503,43.0674883398472,10.8570631928042));
#47360=CARTESIAN_POINT('Ctrl Pts',(0.610680985342629,43.0794598978972,10.8739922339886));
#47361=CARTESIAN_POINT('Ctrl Pts',(0.687212959521698,43.0912600067255,10.8947268596381));
#47362=CARTESIAN_POINT('Ctrl Pts',(0.762760064942518,43.1029827530012,10.9191678164538));
#47363=CARTESIAN_POINT('Ctrl Pts',(0.770392154344625,43.1041670346109,10.9216369457004));
#47364=CARTESIAN_POINT('Ctrl Pts',(0.778014157187172,43.1053505232405,10.9241439273632));
#47365=CARTESIAN_POINT('Ctrl Pts',(0.785625818862137,43.1065333135789,10.9266886756104));
#47366=CARTESIAN_POINT('Ctrl Pts',(0.834861599878281,43.1141841536418,10.9431492952216));
#47367=CARTESIAN_POINT('Ctrl Pts',(0.88366555061725,43.121805651543,10.9611895958705));
#47368=CARTESIAN_POINT('Ctrl Pts',(0.931966035147949,43.1294206320113,10.9807864459211));
#47369=CARTESIAN_POINT('Ctrl Pts',(1.01245564838017,43.1421105012459,11.0134433208255));
#47370=CARTESIAN_POINT('Ctrl Pts',(1.09113085014283,43.1547180044794,11.0502524528365));
#47371=CARTESIAN_POINT('Ctrl Pts',(1.16768393250191,43.1673282101208,11.0909858831448));
#47372=CARTESIAN_POINT('Ctrl Pts',(1.24565870789114,43.1801726041309,11.1324757876822));
#47373=CARTESIAN_POINT('Ctrl Pts',(1.32143121951073,43.1930199757638,11.1780377923875));
#47374=CARTESIAN_POINT('Ctrl Pts',(1.39465893046395,43.2059273251432,11.2274383518593));
#47375=CARTESIAN_POINT('Ctrl Pts',(1.46841068418584,43.2189270439687,11.2771924387816));
#47376=CARTESIAN_POINT('Ctrl Pts',(1.53958036669501,43.2319875908329,11.3308403079002));
#47377=CARTESIAN_POINT('Ctrl Pts',(1.60781086821449,43.245132980258,11.3881447146781));
#47378=CARTESIAN_POINT('Ctrl Pts',(1.66135999036038,43.2554498334,11.4331187454959));
#47379=CARTESIAN_POINT('Ctrl Pts',(1.7130985314609,43.2658182261341,11.4803449079438));
#47380=CARTESIAN_POINT('Ctrl Pts',(1.76285458740213,43.2762356050361,11.5297102091189));
#47381=CARTESIAN_POINT('Ctrl Pts',(1.82624126810301,43.2895068150972,11.5925990881528));
#47382=CARTESIAN_POINT('Ctrl Pts',(1.88607272173309,43.302787518306,11.6586233216415));
#47383=CARTESIAN_POINT('Ctrl Pts',(1.94211797655693,43.3160456689778,11.7274674702159));
#47384=CARTESIAN_POINT('Ctrl Pts',(1.99379031998758,43.3282693570835,11.7909400781915));
#47385=CARTESIAN_POINT('Ctrl Pts',(2.04224493801208,43.3404734842481,11.8568096895573));
#47386=CARTESIAN_POINT('Ctrl Pts',(2.08731732559338,43.3526168843612,11.9248659069953));
#47387=CARTESIAN_POINT('Ctrl Pts',(2.09085119221849,43.3535689785074,11.9302018035019));
#47388=CARTESIAN_POINT('Ctrl Pts',(2.0943642622003,43.3545207011585,11.9355511675448));
#47389=CARTESIAN_POINT('Ctrl Pts',(2.09785645310077,43.355472033399,11.9409139109309));
#47390=CARTESIAN_POINT('Ctrl Pts',(2.14079863407173,43.367170214397,12.0068575845583));
#47391=CARTESIAN_POINT('Ctrl Pts',(2.18058568411325,43.3788086512971,12.0748201437439));
#47392=CARTESIAN_POINT('Ctrl Pts',(2.21707146100581,43.3903416718601,12.1446554705317));
#47393=CARTESIAN_POINT('Ctrl Pts',(2.22000048808778,43.3912675266025,12.1502617527836));
#47394=CARTESIAN_POINT('Ctrl Pts',(2.22290822948716,43.3921927040942,12.1558801303465));
#47395=CARTESIAN_POINT('Ctrl Pts',(2.22579460380645,43.3931171818214,12.1615105412205));
#47396=CARTESIAN_POINT('Ctrl Pts',(2.2257964153244,43.393117762033,12.1615140749237));
#47397=CARTESIAN_POINT('Ctrl Pts',(2.22579822683392,43.3931183422444,12.1615176086317));
#47398=CARTESIAN_POINT('Ctrl Pts',(2.22580003833503,43.3931189224555,12.1615211423445));
#47399=CARTESIAN_POINT('Ctrl Pts',(2.25801117034599,43.4034359219842,12.2243557090336));
#47400=CARTESIAN_POINT('Ctrl Pts',(2.28756377580288,43.4136658527735,12.2886892862194));
#47401=CARTESIAN_POINT('Ctrl Pts',(2.31437366623366,43.4238602643772,12.3543583619918));
#47402=CARTESIAN_POINT('Ctrl Pts',(2.346991566351,43.4362631609986,12.4342537781954));
#47403=CARTESIAN_POINT('Ctrl Pts',(2.37538129216963,43.4485510705151,12.5157145710211));
#47404=CARTESIAN_POINT('Ctrl Pts',(2.39948963992353,43.4607964735314,12.5983792902655));
#47405=CARTESIAN_POINT('Ctrl Pts',(2.42403098143446,43.4732618079637,12.6825286947204));
#47406=CARTESIAN_POINT('Ctrl Pts',(2.44413497407805,43.4856831727977,12.7679255998961));
#47407=CARTESIAN_POINT('Ctrl Pts',(2.459729330354,43.4981074995305,12.8541844160181));
#47408=CARTESIAN_POINT('Ctrl Pts',(2.47544197671866,43.5106260702761,12.9410975434068));
#47409=CARTESIAN_POINT('Ctrl Pts',(2.48657593222927,43.523147559786,13.028885236833));
#47410=CARTESIAN_POINT('Ctrl Pts',(2.49305021988218,43.5356904189153,13.117152922644));
#47411=CARTESIAN_POINT('Ctrl Pts',(2.49560756544813,43.5406448520357,13.1520186850302));
#47412=CARTESIAN_POINT('Ctrl Pts',(2.49743783559164,43.5456023050079,13.1869593782955));
#47413=CARTESIAN_POINT('Ctrl Pts',(2.49853582421476,43.5505627268715,13.2219509696579));
#47414=CARTESIAN_POINT('Ctrl Pts',(2.49853638756189,43.5505652719246,13.2219689228608));
#47415=CARTESIAN_POINT('Ctrl Pts',(2.49853695071622,43.5505678169786,13.221986876077));
#47416=CARTESIAN_POINT('Ctrl Pts',(2.49853751367776,43.5505703620333,13.2220048293067));
#47417=CARTESIAN_POINT('Ctrl Pts',(2.49967622144808,43.555718268927,13.2583190012753));
#47418=CARTESIAN_POINT('Ctrl Pts',(2.50002624606076,43.5608693880851,13.2946880561884));
#47419=CARTESIAN_POINT('Ctrl Pts',(2.49958353970284,43.5660259951698,13.3310838093336));
#47420=CARTESIAN_POINT('Ctrl Pts',(2.49850970026858,43.5785339881895,13.4193662436561));
#47421=CARTESIAN_POINT('Ctrl Pts',(2.49277750870894,43.5910106166133,13.5073402163106));
#47422=CARTESIAN_POINT('Ctrl Pts',(2.4824727741004,43.603468467095,13.5946136719723));
#47423=CARTESIAN_POINT('Ctrl Pts',(2.47210445202433,43.6160031912849,13.6824256662998));
#47424=CARTESIAN_POINT('Ctrl Pts',(2.45710753280093,43.6285186011674,13.7695279489814));
#47425=CARTESIAN_POINT('Ctrl Pts',(2.43756057094178,43.6410022854227,13.8555491732612));
#47426=CARTESIAN_POINT('Ctrl Pts',(2.41934319006255,43.6526368316245,13.9357192486773));
#47427=CARTESIAN_POINT('Ctrl Pts',(2.39717411513907,43.6642434867231,14.0149504283669));
#47428=CARTESIAN_POINT('Ctrl Pts',(2.37110114656571,43.6757960912124,14.0929682274303));
#47429=CARTESIAN_POINT('Ctrl Pts',(2.36957346353064,43.6764729883535,14.0975394931735));
#47430=CARTESIAN_POINT('Ctrl Pts',(2.36803236379235,43.6771497009232,14.1021065974979));
#47431=CARTESIAN_POINT('Ctrl Pts',(2.3664778515487,43.67782622403,14.1066694866157));
#47432=CARTESIAN_POINT('Ctrl Pts',(2.3445325218236,43.6873768227509,14.1710846152822));
#47433=CARTESIAN_POINT('Ctrl Pts',(2.31991723310749,43.696888999328,14.2346595029851));
#47434=CARTESIAN_POINT('Ctrl Pts',(2.2926420156784,43.7063422882946,14.2972517365443));
#47435=CARTESIAN_POINT('Ctrl Pts',(2.2926368945365,43.7063440632258,14.2972634887406));
#47436=CARTESIAN_POINT('Ctrl Pts',(2.29263177330077,43.7063458381549,14.2972752409023));
#47437=CARTESIAN_POINT('Ctrl Pts',(2.29262665197122,43.706347613082,14.2972869930294));
#47438=CARTESIAN_POINT('Ctrl Pts',(2.29200670382658,43.7065624718801,14.2987096137206));
#47439=CARTESIAN_POINT('Ctrl Pts',(2.29138538081122,43.7067773000871,14.3001317271333));
#47440=CARTESIAN_POINT('Ctrl Pts',(2.2907626834559,43.70699209831,14.3015533316609));
#47441=CARTESIAN_POINT('Ctrl Pts',(2.25906768334438,43.7179252260014,14.3739123280138));
#47442=CARTESIAN_POINT('Ctrl Pts',(2.2239627150649,43.7287303647691,14.4446137883274));
#47443=CARTESIAN_POINT('Ctrl Pts',(2.18561078838783,43.739482210611,14.5134705831952));
#47444=CARTESIAN_POINT('Ctrl Pts',(2.18234908166992,43.7403966201557,14.5193266298102));
#47445=CARTESIAN_POINT('Ctrl Pts',(2.17906387504082,43.7413106412124,14.5251693069775));
#47446=CARTESIAN_POINT('Ctrl Pts',(2.17575526116822,43.7422243180421,14.5309984843913));
#47447=CARTESIAN_POINT('Ctrl Pts',(2.13482840560831,43.7535263076608,14.6031041791731));
#47448=CARTESIAN_POINT('Ctrl Pts',(2.09032113816982,43.7647763544049,14.6731479851909));
#47449=CARTESIAN_POINT('Ctrl Pts',(2.04242125552808,43.7760397844312,14.7408738036126));
#47450=CARTESIAN_POINT('Ctrl Pts',(2.03981864874256,43.7766517750624,14.7445536388201));
#47451=CARTESIAN_POINT('Ctrl Pts',(2.03720602191432,43.7772638040268,14.7482266188967));
#47452=CARTESIAN_POINT('Ctrl Pts',(2.03458340383749,43.7778758813964,14.7518926986234));
#47453=CARTESIAN_POINT('Ctrl Pts',(1.98281974934335,43.7899566955126,14.8242515700877));
#47454=CARTESIAN_POINT('Ctrl Pts',(1.92716488177324,43.8020570141243,14.8939263283273));
#47455=CARTESIAN_POINT('Ctrl Pts',(1.86786532911653,43.8142284487568,14.9605698698303));
#47456=CARTESIAN_POINT('Ctrl Pts',(1.81861304804456,43.8243376467644,15.0159218293423));
#47457=CARTESIAN_POINT('Ctrl Pts',(1.7668468882253,43.8344953552915,15.0691818697345));
#47458=CARTESIAN_POINT('Ctrl Pts',(1.71271910845011,43.8447159041991,15.1201448262752));
#47459=CARTESIAN_POINT('Ctrl Pts',(1.64769299153216,43.8569943056224,15.1813688998334));
#47460=CARTESIAN_POINT('Ctrl Pts',(1.5796070055678,43.8692984228793,15.2389495971852));
#47461=CARTESIAN_POINT('Ctrl Pts',(1.50882929121771,43.8816268677423,15.2926564756774));
#47462=CARTESIAN_POINT('Ctrl Pts',(1.4377895602789,43.8940009520711,15.3465621751292));
#47463=CARTESIAN_POINT('Ctrl Pts',(1.36403937126748,43.906399135297,15.3965654700129));
#47464=CARTESIAN_POINT('Ctrl Pts',(1.28792448754835,43.9187985854612,15.4424636499677));
#47465=CARTESIAN_POINT('Ctrl Pts',(1.21837472863129,43.9301285478482,15.4844029816018));
#47466=CARTESIAN_POINT('Ctrl Pts',(1.14685089075896,43.9414592226689,15.522915452623));
#47467=CARTESIAN_POINT('Ctrl Pts',(1.07358427247098,43.9527617434253,15.5578634725687));
#47468=CARTESIAN_POINT('Ctrl Pts',(1.06805073755035,43.9536153776554,15.56050295687));
#47469=CARTESIAN_POINT('Ctrl Pts',(1.06250723822261,43.9544688533448,15.5631221008957));
#47470=CARTESIAN_POINT('Ctrl Pts',(1.05695386278732,43.955322159067,15.5657208410323));
#47471=CARTESIAN_POINT('Ctrl Pts',(0.994491935694773,43.9649197669421,15.5949503283653));
#47472=CARTESIAN_POINT('Ctrl Pts',(0.930783327332353,43.9744952258414,15.6216005644104));
#47473=CARTESIAN_POINT('Ctrl Pts',(0.865943140492572,43.9840274102256,15.6455878229252));
#47474=CARTESIAN_POINT('Ctrl Pts',(0.806103392321384,43.9928244779219,15.6677251975812));
#47475=CARTESIAN_POINT('Ctrl Pts',(0.745528272931709,44.001550983782,15.6875102987326));
#47476=CARTESIAN_POINT('Ctrl Pts',(0.684304520976044,44.0101912848952,15.7049249939626));
#47477=CARTESIAN_POINT('Ctrl Pts',(0.684249582127082,44.0101990382292,15.7049406209583));
#47478=CARTESIAN_POINT('Ctrl Pts',(0.684194642754202,44.0102067914943,15.7049562460436));
#47479=CARTESIAN_POINT('Ctrl Pts',(0.684139702857418,44.0102145446905,15.7049718692182));
#47480=CARTESIAN_POINT('Ctrl Pts',(0.612191421570442,44.0203679882298,15.7254316922686));
#47481=CARTESIAN_POINT('Ctrl Pts',(0.539342580598442,44.03040372576,15.7426187073691));
#47482=CARTESIAN_POINT('Ctrl Pts',(0.465792504227374,44.0403870832344,15.7565067758889));
#47483=CARTESIAN_POINT('Ctrl Pts',(0.455193062131454,44.0418258039631,15.7585082119902));
#47484=CARTESIAN_POINT('Ctrl Pts',(0.444579102294771,44.0432634277579,15.7604410598144));
#47485=CARTESIAN_POINT('Ctrl Pts',(0.433951270121274,44.044700140944,15.7623051681519));
#47486=CARTESIAN_POINT('Ctrl Pts',(0.356602895948348,44.0551564058984,15.7758719752706));
#47487=CARTESIAN_POINT('Ctrl Pts',(0.278516886314291,44.0655652642482,15.7858001471926));
#47488=CARTESIAN_POINT('Ctrl Pts',(0.19996358876216,44.0759832197129,15.7920378279043));
#47489=CARTESIAN_POINT('Ctrl Pts',(0.186903219592773,44.0777153219747,15.7930749124748));
#47490=CARTESIAN_POINT('Ctrl Pts',(0.173830010431977,44.0794476642253,15.7940098946058));
#47491=CARTESIAN_POINT('Ctrl Pts',(0.160745300561244,44.0811804923826,15.7948424364924));
#47492=CARTESIAN_POINT('Ctrl Pts',(0.0773994813251622,44.0922181068039,
15.8001454876317));
#47493=CARTESIAN_POINT('Ctrl Pts',(-0.00641597124643042,44.1032760357438,
15.8012945090207));
#47494=CARTESIAN_POINT('Ctrl Pts',(-0.0903323110069834,44.1143968109666,
15.7982274792389));
#47495=CARTESIAN_POINT('Ctrl Pts',(-0.0988286635242062,44.1155227660169,
15.7979169489384));
#47496=CARTESIAN_POINT('Ctrl Pts',(-0.107326017400065,44.1166493617228,
15.7975631700255));
#47497=CARTESIAN_POINT('Ctrl Pts',(-0.115823966859831,44.1177766397923,
15.797166059037));
#47498=CARTESIAN_POINT('Ctrl Pts',(-0.204584845519198,44.1295510322401,
15.7930182442686));
#47499=CARTESIAN_POINT('Ctrl Pts',(-0.292943942210145,44.1413382533506,
15.7841678945119));
#47500=CARTESIAN_POINT('Ctrl Pts',(-0.380449539413418,44.1531590749493,
15.770710573128));
#47501=CARTESIAN_POINT('Ctrl Pts',(-0.468800318782251,44.165094069217,15.7571232727669));
#47502=CARTESIAN_POINT('Ctrl Pts',(-0.556279560261329,44.1770629824426,
15.7388399646226));
#47503=CARTESIAN_POINT('Ctrl Pts',(-0.642444892911005,44.189062777786,15.7159833031921));
#47504=CARTESIAN_POINT('Ctrl Pts',(-0.727700913903991,44.2009359380496,
15.6933678504709));
#47505=CARTESIAN_POINT('Ctrl Pts',(-0.811669692603273,44.2128388856667,
15.6662763592815));
#47506=CARTESIAN_POINT('Ctrl Pts',(-0.893962707722052,44.2247508796413,
15.6348383833099));
#47507=CARTESIAN_POINT('Ctrl Pts',(-0.956576084841162,44.2338142268754,
15.6109185179054));
#47508=CARTESIAN_POINT('Ctrl Pts',(-1.01822021388613,44.242882402068,15.5844829630128));
#47509=CARTESIAN_POINT('Ctrl Pts',(-1.07874311180981,44.2519416693289,15.5555843741965));
#47510=CARTESIAN_POINT('Ctrl Pts',(-1.14496652126029,44.2618542079831,15.5239638942563));
#47511=CARTESIAN_POINT('Ctrl Pts',(-1.20955741377997,44.2717127862346,15.4895336024582));
#47512=CARTESIAN_POINT('Ctrl Pts',(-1.27238454152044,44.2814976143977,15.4524181007049));
#47513=CARTESIAN_POINT('Ctrl Pts',(-1.28569633879536,44.2835708215227,15.4445540767894));
#47514=CARTESIAN_POINT('Ctrl Pts',(-1.29892904457969,44.2856407336629,15.4365693429927));
#47515=CARTESIAN_POINT('Ctrl Pts',(-1.3120815432013,44.2877071882353,15.4284648153511));
#47516=CARTESIAN_POINT('Ctrl Pts',(-1.35081614496656,44.2937929744598,15.4045966774614));
#47517=CARTESIAN_POINT('Ctrl Pts',(-1.38885518000683,44.299848553427,15.3796905867644));
#47518=CARTESIAN_POINT('Ctrl Pts',(-1.42617359642233,44.3058694449266,15.3537669118777));
#47519=CARTESIAN_POINT('Ctrl Pts',(-1.42626314939669,44.3058838932552,15.3537047028556));
#47520=CARTESIAN_POINT('Ctrl Pts',(-1.42635269822065,44.3058983413847,15.3536424879691));
#47521=CARTESIAN_POINT('Ctrl Pts',(-1.42644224289338,44.3059127893153,15.3535802672179));
#47522=CARTESIAN_POINT('Ctrl Pts',(-1.48664804685902,44.3156269269582,15.3117458371601));
#47523=CARTESIAN_POINT('Ctrl Pts',(-1.5449815724511,44.3252515595638,15.2672608493679));
#47524=CARTESIAN_POINT('Ctrl Pts',(-1.60132034593166,44.3348359188048,15.2202238907525));
#47525=CARTESIAN_POINT('Ctrl Pts',(-1.61100448833462,44.3364833863302,15.2121386489679));
#47526=CARTESIAN_POINT('Ctrl Pts',(-1.62062956923397,44.3381296519929,15.2039779924162));
#47527=CARTESIAN_POINT('Ctrl Pts',(-1.63019481385692,44.3397749509719,15.1957424125318));
#47528=CARTESIAN_POINT('Ctrl Pts',(-1.68776433825106,44.3496773720222,15.1461756282264));
#47529=CARTESIAN_POINT('Ctrl Pts',(-1.74317011067206,44.3595453660952,15.0938940531257));
#47530=CARTESIAN_POINT('Ctrl Pts',(-1.79622626396811,44.3694216474947,15.039020570549));
#47531=CARTESIAN_POINT('Ctrl Pts',(-1.80469338301604,44.3709977823097,15.0302634277731));
#47532=CARTESIAN_POINT('Ctrl Pts',(-1.8131005545515,44.3725741181431,15.0214402852565));
#47533=CARTESIAN_POINT('Ctrl Pts',(-1.8214469022326,44.3741508171333,15.0125516606569));
#47534=CARTESIAN_POINT('Ctrl Pts',(-1.836280361967,44.3769529890388,14.996754444901));
#47535=CARTESIAN_POINT('Ctrl Pts',(-1.85092185963658,44.3797562606112,14.9807505146924));
#47536=CARTESIAN_POINT('Ctrl Pts',(-1.86536652856784,44.3825614203959,14.9645430656605));
#47537=CARTESIAN_POINT('Ctrl Pts',(-1.92371379910021,44.393892480846,14.899075285277));
#47538=CARTESIAN_POINT('Ctrl Pts',(-1.97854811218913,44.405197219464,14.8306240014923));
#47539=CARTESIAN_POINT('Ctrl Pts',(-2.0296405263341,44.4165150690176,14.7595164795904));
#47540=CARTESIAN_POINT('Ctrl Pts',(-2.081506579579,44.4280042929539,14.6873322507025));
#47541=CARTESIAN_POINT('Ctrl Pts',(-2.12951514617069,44.4395068705651,14.612411143145));
#47542=CARTESIAN_POINT('Ctrl Pts',(-2.17342850391493,44.4510446190335,14.5351199866075));
#47543=CARTESIAN_POINT('Ctrl Pts',(-2.21738895172838,44.4625947398961,14.4577459476376));
#47544=CARTESIAN_POINT('Ctrl Pts',(-2.2572446314795,44.4741798323454,14.377997877658));
#47545=CARTESIAN_POINT('Ctrl Pts',(-2.29277556231768,44.4858057950063,14.2962564099619));
#47546=CARTESIAN_POINT('Ctrl Pts',(-2.31886668641432,44.494342988583,14.236231898158));
#47547=CARTESIAN_POINT('Ctrl Pts',(-2.34262629986971,44.5029018614689,14.1751328954114));
#47548=CARTESIAN_POINT('Ctrl Pts',(-2.36397569414679,44.5114807594104,14.1131078193728));
#47549=CARTESIAN_POINT('Ctrl Pts',(-2.39010827060216,44.5219816993176,14.037186459699));
#47550=CARTESIAN_POINT('Ctrl Pts',(-2.41250514705558,44.5324630052681,13.960239143359));
#47551=CARTESIAN_POINT('Ctrl Pts',(-2.43114099486024,44.5429171624905,13.8825489827748));
#47552=CARTESIAN_POINT('Ctrl Pts',(-2.43324911742662,44.544099756649,13.8737605239706));
#47553=CARTESIAN_POINT('Ctrl Pts',(-2.43530909415252,44.5452820075015,13.8649625075572));
#47554=CARTESIAN_POINT('Ctrl Pts',(-2.43732087366301,44.5464639073091,13.8561553043701));
#47555=CARTESIAN_POINT('Ctrl Pts',(-2.45444088241008,44.5565217366781,13.7812070335404));
#47556=CARTESIAN_POINT('Ctrl Pts',(-2.46807305677235,44.5665536359262,13.705597453051));
#47557=CARTESIAN_POINT('Ctrl Pts',(-2.47819858923538,44.5765524043719,13.6295333731716));
#47558=CARTESIAN_POINT('Ctrl Pts',(-2.47972970810502,44.5780643547899,13.6180314449095));
#47559=CARTESIAN_POINT('Ctrl Pts',(-2.48118060018608,44.5795755559865,13.6065190388408));
#47560=CARTESIAN_POINT('Ctrl Pts',(-2.48255114815379,44.5810859919839,13.5949967802098));
#47561=CARTESIAN_POINT('Ctrl Pts',(-2.48626354567838,44.5851773036271,13.5637864866433));
#47562=CARTESIAN_POINT('Ctrl Pts',(-2.48938680535883,44.589262937982,13.5325040260609));
#47563=CARTESIAN_POINT('Ctrl Pts',(-2.49191879076888,44.5933425241649,13.5011609896512));
#47564=CARTESIAN_POINT('Ctrl Pts',(-2.4919202673538,44.5933449032685,13.5011427112462));
#47565=CARTESIAN_POINT('Ctrl Pts',(-2.49192174373751,44.5933472823699,13.5011244328207));
#47566=CARTESIAN_POINT('Ctrl Pts',(-2.49192321992002,44.5933496614694,13.5011061543745));
#47567=CARTESIAN_POINT('Ctrl Pts',(-2.49732230562144,44.6020511341444,13.434253379173));
#47568=CARTESIAN_POINT('Ctrl Pts',(-2.50003180211327,44.6107255757689,13.36712281549));
#47569=CARTESIAN_POINT('Ctrl Pts',(-2.50002611214299,44.6193946092241,13.2998651846547));
#47570=CARTESIAN_POINT('Ctrl Pts',(-2.5,43.4016964318853,13.3));
#47571=CARTESIAN_POINT('Ctrl Pts',(-2.5,43.3852617716781,13.4270421871792));
#47572=CARTESIAN_POINT('Ctrl Pts',(-2.49031634926891,43.368834406787,13.5541860796652));
#47573=CARTESIAN_POINT('Ctrl Pts',(-2.4462108798017,43.3313307762581,13.8407368121712));
#47574=CARTESIAN_POINT('Ctrl Pts',(-2.40595538844556,43.3103489662895,13.9983720971123));
#47575=CARTESIAN_POINT('Ctrl Pts',(-2.29609289339089,43.2686567057597,14.3018471431555));
#47576=CARTESIAN_POINT('Ctrl Pts',(-2.22708344547497,43.2481001380742,14.4471026079539));
#47577=CARTESIAN_POINT('Ctrl Pts',(-1.98107654260903,43.1866566466313,14.8577616816271));
#47578=CARTESIAN_POINT('Ctrl Pts',(-1.76688211021228,43.146034744725,15.0970604390272));
#47579=CARTESIAN_POINT('Ctrl Pts',(-1.38192588260007,43.0841941276021,15.389889404462));
#47580=CARTESIAN_POINT('Ctrl Pts',(-1.24066763196097,43.063137545343,15.4767184333445));
#47581=CARTESIAN_POINT('Ctrl Pts',(-0.809252614246744,43.0019770630349,
15.6861705819616));
#47582=CARTESIAN_POINT('Ctrl Pts',(-0.503271371124684,42.9623486760914,
15.7688942205564));
#47583=CARTESIAN_POINT('Ctrl Pts',(0.130316300639296,42.881860589194,15.8171817823848));
#47584=CARTESIAN_POINT('Ctrl Pts',(0.452347003458223,42.8415374579058,15.7796331097567));
#47585=CARTESIAN_POINT('Ctrl Pts',(1.07677407195124,42.7588523199414,15.5808241331816));
#47586=CARTESIAN_POINT('Ctrl Pts',(1.3715928254352,42.7173390934895,15.4166850306452));
#47587=CARTESIAN_POINT('Ctrl Pts',(1.87923963864281,42.6335652038256,14.9822738126762));
#47588=CARTESIAN_POINT('Ctrl Pts',(2.08696858621688,42.5922263089786,14.716393108069));
#47589=CARTESIAN_POINT('Ctrl Pts',(2.30808784746728,42.5305927477067,14.2739169922799));
#47590=CARTESIAN_POINT('Ctrl Pts',(2.3658637645178,42.5106600890778,14.1236955877563));
#47591=CARTESIAN_POINT('Ctrl Pts',(2.4972689708802,42.4496258159417,13.6505319233069));
#47592=CARTESIAN_POINT('Ctrl Pts',(2.52169285474868,42.4090602178902,13.3176772921114));
#47593=CARTESIAN_POINT('Ctrl Pts',(2.43922334176455,42.3270557602614,12.6583659515808));
#47594=CARTESIAN_POINT('Ctrl Pts',(2.33180699975093,42.2862597604716,12.3386462133287));
#47595=CARTESIAN_POINT('Ctrl Pts',(2.08504868622191,42.2257498641914,11.9114877736278));
#47596=CARTESIAN_POINT('Ctrl Pts',(1.9923246159707,42.2063050422175,11.7814351912134));
#47597=CARTESIAN_POINT('Ctrl Pts',(1.66953336889731,42.1460936517606,11.4096126348075));
#47598=CARTESIAN_POINT('Ctrl Pts',(1.40313558136579,42.1057789244256,11.2042557730935));
#47599=CARTESIAN_POINT('Ctrl Pts',(0.957230451939393,42.0455123513771,10.9847047047587));
#47600=CARTESIAN_POINT('Ctrl Pts',(0.803366474576863,42.0257016335364,10.9269250852756));
#47601=CARTESIAN_POINT('Ctrl Pts',(0.490212340613467,41.9863894499915,10.8433059540261));
#47602=CARTESIAN_POINT('Ctrl Pts',(0.331845479247272,41.9670348596456,10.8169500191847));
#47603=CARTESIAN_POINT('Ctrl Pts',(0.0153217978071606,41.928800515166,10.7951160967115));
#47604=CARTESIAN_POINT('Ctrl Pts',(-0.142074101189276,41.9100042517287,
10.7991008620169));
#47605=CARTESIAN_POINT('Ctrl Pts',(-0.629403268990953,41.8511612068468,
10.8576190259936));
#47606=CARTESIAN_POINT('Ctrl Pts',(-0.949473633184957,41.8113724229515,
10.9633568070406));
#47607=CARTESIAN_POINT('Ctrl Pts',(-1.5162652735471,41.7338116666724,11.2868898818915));
#47608=CARTESIAN_POINT('Ctrl Pts',(-1.76039885847095,41.6967872741871,11.4964861436722));
#47609=CARTESIAN_POINT('Ctrl Pts',(-2.16616343486832,41.6193772711827,12.0079784770186));
#47610=CARTESIAN_POINT('Ctrl Pts',(-2.31925376322761,41.5793150797788,12.3086842005688));
#47611=CARTESIAN_POINT('Ctrl Pts',(-2.46935912315545,41.5139154476201,12.8488261886895));
#47612=CARTESIAN_POINT('Ctrl Pts',(-2.5,41.4882539293719,13.0740124126314));
#47613=CARTESIAN_POINT('Ctrl Pts',(-2.5,41.4625301506567,13.3));
#47614=CARTESIAN_POINT('Origin',(0.,70.2,13.3));
#47615=CARTESIAN_POINT('',(-2.5,39.6612570972331,13.3));
#47616=CARTESIAN_POINT('',(-2.5,40.3937280662289,13.2999999991311));
#47617=CARTESIAN_POINT('',(-2.5,70.2,13.3));
#47618=CARTESIAN_POINT('Ctrl Pts',(-2.5,40.3937280662289,13.2999999982622));
#47619=CARTESIAN_POINT('Ctrl Pts',(-2.49999999978245,40.4379661198564,12.9870368453108));
#47620=CARTESIAN_POINT('Ctrl Pts',(-2.4412336387843,40.4807379631984,12.6767857341882));
#47621=CARTESIAN_POINT('Ctrl Pts',(-2.22632554663737,40.5630948484494,12.1300634584708));
#47622=CARTESIAN_POINT('Ctrl Pts',(-2.08459119418497,40.6017157099769,11.8929518149928));
#47623=CARTESIAN_POINT('Ctrl Pts',(-1.70481717270669,40.6832438792545,11.4448602899963));
#47624=CARTESIAN_POINT('Ctrl Pts',(-1.4593661341119,40.7257339676381,11.2461567437301));
#47625=CARTESIAN_POINT('Ctrl Pts',(-0.897988983361204,40.8124308533914,
10.9444213644873));
#47626=CARTESIAN_POINT('Ctrl Pts',(-0.585206760151349,40.8548620227273,
10.8479121602653));
#47627=CARTESIAN_POINT('Ctrl Pts',(0.0523483348050161,40.9400703617392,
10.7805569331726));
#47628=CARTESIAN_POINT('Ctrl Pts',(0.37077061627588,40.9823279848828,10.8074510801111));
#47629=CARTESIAN_POINT('Ctrl Pts',(0.932837788469853,41.0612960462026,10.9652248757414));
#47630=CARTESIAN_POINT('Ctrl Pts',(1.17687075883366,41.0972486812662,11.0781972004358));
#47631=CARTESIAN_POINT('Ctrl Pts',(1.53549458939259,41.1540447941993,11.3202010414756));
#47632=CARTESIAN_POINT('Ctrl Pts',(1.66307411447041,41.1753016305061,11.426088176817));
#47633=CARTESIAN_POINT('Ctrl Pts',(1.99958072047131,41.2374130441304,11.7670181048818));
#47634=CARTESIAN_POINT('Ctrl Pts',(2.17594664465665,41.277926458624,12.0297106921224));
#47635=CARTESIAN_POINT('Ctrl Pts',(2.43031359161238,41.3612878253565,12.6253518496065));
#47636=CARTESIAN_POINT('Ctrl Pts',(2.49862527908222,41.4034052564218,12.9557752115897));
#47637=CARTESIAN_POINT('Ctrl Pts',(2.50063792532608,41.4665288918307,13.4523173142111));
#47638=CARTESIAN_POINT('Ctrl Pts',(2.4854606234463,41.487086984546,13.6144541337529));
#47639=CARTESIAN_POINT('Ctrl Pts',(2.42353912827401,41.5283481061993,13.9351374775737));
#47640=CARTESIAN_POINT('Ctrl Pts',(2.37662234536734,41.5489654588928,14.0928509423556));
#47641=CARTESIAN_POINT('Ctrl Pts',(2.19491288165371,41.6093531387659,14.537991146173));
#47642=CARTESIAN_POINT('Ctrl Pts',(2.02061728609311,41.6485874461389,14.805790271673));
#47643=CARTESIAN_POINT('Ctrl Pts',(1.68897440073113,41.7079628689352,15.1502531036789));
#47644=CARTESIAN_POINT('Ctrl Pts',(1.56597429620276,41.7278968398917,15.2554542210286));
#47645=CARTESIAN_POINT('Ctrl Pts',(1.17463083430046,41.7867872521025,15.5294025584051));
#47646=CARTESIAN_POINT('Ctrl Pts',(0.883488052794584,41.825142327897,15.6599732144183));
#47647=CARTESIAN_POINT('Ctrl Pts',(0.418544378133756,41.8833837069086,15.7700017928239));
#47648=CARTESIAN_POINT('Ctrl Pts',(0.25812254959729,41.902963575707,15.7918802302917));
#47649=CARTESIAN_POINT('Ctrl Pts',(-0.22337415050963,41.9612293877349,15.8105196380457));
#47650=CARTESIAN_POINT('Ctrl Pts',(-0.54289773123516,41.9992630877993,15.7612797742278));
#47651=CARTESIAN_POINT('Ctrl Pts',(-1.13728900707918,42.0747361686259,15.5479725788548));
#47652=CARTESIAN_POINT('Ctrl Pts',(-1.40799801326119,42.1112338469496,15.3891135199219));
#47653=CARTESIAN_POINT('Ctrl Pts',(-1.89412243233685,42.1869085569829,14.9654175430183));
#47654=CARTESIAN_POINT('Ctrl Pts',(-2.0992561914926,42.2257196768098,14.6980291423986));
#47655=CARTESIAN_POINT('Ctrl Pts',(-2.32729552311567,42.2857231314088,14.231700131323));
#47656=CARTESIAN_POINT('Ctrl Pts',(-2.38996358047702,42.3069006498049,14.0566049252537));
#47657=CARTESIAN_POINT('Ctrl Pts',(-2.47741115240338,42.3503735727866,13.6873956138112));
#47658=CARTESIAN_POINT('Ctrl Pts',(-2.50000000000055,42.3725986254843,13.4940315075717));
#47659=CARTESIAN_POINT('Ctrl Pts',(-2.5,42.3946776132135,13.2999999999929));
#47660=CARTESIAN_POINT('',(0.29921364472731,40.3086929042607,10.8178945405685));
#47661=CARTESIAN_POINT('Ctrl Pts',(-2.5,41.4625301506567,13.3));
#47662=CARTESIAN_POINT('Ctrl Pts',(-2.5,41.4560785509388,13.3566783547267));
#47663=CARTESIAN_POINT('Ctrl Pts',(-2.49807254879367,41.4496179201224,13.4134065353913));
#47664=CARTESIAN_POINT('Ctrl Pts',(-2.47148213767631,41.4049536465583,13.8033386835103));
#47665=CARTESIAN_POINT('Ctrl Pts',(-2.38219647438595,41.3663719935291,14.1286848321518));
#47666=CARTESIAN_POINT('Ctrl Pts',(-2.09236349753892,41.2928990371905,14.7026692336443));
#47667=CARTESIAN_POINT('Ctrl Pts',(-1.90315733928508,41.2584345053206,14.9502974710062));
#47668=CARTESIAN_POINT('Ctrl Pts',(-1.43371380883422,41.1872437576834,15.3733411230399));
#47669=CARTESIAN_POINT('Ctrl Pts',(-1.15414839789977,41.1510689780122,15.5410470043474));
#47670=CARTESIAN_POINT('Ctrl Pts',(-0.552493634150507,41.080644518305,15.7586776853435));
#47671=CARTESIAN_POINT('Ctrl Pts',(-0.236875365769137,41.0471638778177,
15.8088231800092));
#47672=CARTESIAN_POINT('Ctrl Pts',(0.398445077487314,40.9770276470599,15.7885661577294));
#47673=CARTESIAN_POINT('Ctrl Pts',(0.712541558724279,40.9411190516746,15.7174744657946));
#47674=CARTESIAN_POINT('Ctrl Pts',(1.27025636778447,40.8767556601898,15.4726642950741));
#47675=CARTESIAN_POINT('Ctrl Pts',(1.51333231666157,40.8483665405938,15.310924910557));
#47676=CARTESIAN_POINT('Ctrl Pts',(1.96510748387776,40.7840312890235,14.8810647713995));
#47677=CARTESIAN_POINT('Ctrl Pts',(2.15854110160934,40.7479263175339,14.6047292565089));
#47678=CARTESIAN_POINT('Ctrl Pts',(2.40840350182393,40.68618936217,14.0311557266678));
#47679=CARTESIAN_POINT('Ctrl Pts',(2.47714514170984,40.660214611156,13.7457199251508));
#47680=CARTESIAN_POINT('Ctrl Pts',(2.51593287324437,40.6001147718643,13.1208255095539));
#47681=CARTESIAN_POINT('Ctrl Pts',(2.46937870516111,40.5653455467743,12.7857883898233));
#47682=CARTESIAN_POINT('Ctrl Pts',(2.26356318381571,40.5083103638821,12.2012046620872));
#47683=CARTESIAN_POINT('Ctrl Pts',(2.12391289303238,40.4853118764239,11.9509252325965));
#47684=CARTESIAN_POINT('Ctrl Pts',(1.73613868327223,40.4322867871816,11.4706618591433));
#47685=CARTESIAN_POINT('Ctrl Pts',(1.47750592152716,40.4010497148421,11.2560098035361));
#47686=CARTESIAN_POINT('Ctrl Pts',(0.909078151443106,40.3501549758377,10.9502852158795));
#47687=CARTESIAN_POINT('Ctrl Pts',(0.609047735460097,40.3305173363008,10.8553192285048));
#47688=CARTESIAN_POINT('Ctrl Pts',(0.299195963681299,40.3088185629972,10.817968216296));
#47689=CARTESIAN_POINT('Ctrl Pts',(0.29922011908992,40.3085872692275,10.8179711282236));
#47690=CARTESIAN_POINT('Ctrl Pts',(0.116198641054608,40.2789287682072,10.7959070382057));
#47691=CARTESIAN_POINT('Ctrl Pts',(-0.0686762603413709,40.2491054246701,
10.7941574537077));
#47692=CARTESIAN_POINT('Ctrl Pts',(-0.438507985113607,40.1886677747163,
10.8316316522575));
#47693=CARTESIAN_POINT('Ctrl Pts',(-0.622391748993356,40.1582791495571,
10.8714511195648));
#47694=CARTESIAN_POINT('Ctrl Pts',(-0.939390485172885,40.1059611621546,
10.9785492634775));
#47695=CARTESIAN_POINT('Ctrl Pts',(-1.07421589908956,40.0835661295813,11.0377722117975));
#47696=CARTESIAN_POINT('Ctrl Pts',(-1.48656905412663,40.0115779517093,11.2641483984129));
#47697=CARTESIAN_POINT('Ctrl Pts',(-1.73714292844758,39.9616407800466,11.4732906075798));
#47698=CARTESIAN_POINT('Ctrl Pts',(-2.14142033006415,39.8636098967804,11.9712737432747));
#47699=CARTESIAN_POINT('Ctrl Pts',(-2.29295694249452,39.8182922052658,12.2542172428525));
#47700=CARTESIAN_POINT('Ctrl Pts',(-2.46213065903313,39.7350203443603,12.7986694947532));
#47701=CARTESIAN_POINT('Ctrl Pts',(-2.5,39.6979590514318,13.048786034241));
#47702=CARTESIAN_POINT('Ctrl Pts',(-2.5,39.6612570972331,13.3000000000001));
#47703=CARTESIAN_POINT('Origin',(0.,70.2,13.3));
#47704=CARTESIAN_POINT('',(-2.5,37.5946437602656,13.3));
#47705=CARTESIAN_POINT('',(-2.5,38.6159089611155,13.3000000021922));
#47706=CARTESIAN_POINT('',(-2.5,70.2,13.3));
#47707=CARTESIAN_POINT('',(-2.38728043808747,40.2846522490296,14.040572526374));
#47708=CARTESIAN_POINT('Ctrl Pts',(-2.5,38.6159089611155,13.3000000043844));
#47709=CARTESIAN_POINT('Ctrl Pts',(-2.50000000005366,38.6197079913925,13.2694025310785));
#47710=CARTESIAN_POINT('Ctrl Pts',(-2.49943827756166,38.6235065893519,13.2387964405414));
#47711=CARTESIAN_POINT('Ctrl Pts',(-2.48616875692374,38.6683390855345,12.8776808724054));
#47712=CARTESIAN_POINT('Ctrl Pts',(-2.40855367298769,38.7088102422073,12.5528105212031));
#47713=CARTESIAN_POINT('Ctrl Pts',(-2.20426898953433,38.7686465464089,12.110140157825));
#47714=CARTESIAN_POINT('Ctrl Pts',(-2.12535056754911,38.7877875407426,11.9743093800384));
#47715=CARTESIAN_POINT('Ctrl Pts',(-1.83956379670401,38.8479220297597,11.5742668391486));
#47716=CARTESIAN_POINT('Ctrl Pts',(-1.59209400869922,38.8884943271984,11.3436189247701));
#47717=CARTESIAN_POINT('Ctrl Pts',(-1.03650133667816,38.9672215982648,11.003050754753));
#47718=CARTESIAN_POINT('Ctrl Pts',(-0.737456794249405,39.004744620235,10.8903358409477));
#47719=CARTESIAN_POINT('Ctrl Pts',(-0.264597610750918,39.0624274558073,
10.8086961660701));
#47720=CARTESIAN_POINT('Ctrl Pts',(-0.101519839748652,39.0819694629327,
10.7967407944093));
#47721=CARTESIAN_POINT('Ctrl Pts',(0.357618543640866,39.136733000928,10.808051036079));
#47722=CARTESIAN_POINT('Ctrl Pts',(0.650055821113488,39.1712127316438,10.8678901023741));
#47723=CARTESIAN_POINT('Ctrl Pts',(1.23610977859552,39.2453369040003,11.1013585233494));
#47724=CARTESIAN_POINT('Ctrl Pts',(1.51901982093872,39.2846640132817,11.2863925577538));
#47725=CARTESIAN_POINT('Ctrl Pts',(1.9819103061487,39.360075244422,11.7437561604655));
#47726=CARTESIAN_POINT('Ctrl Pts',(2.16256841943955,39.3956859872853,12.0064890572955));
#47727=CARTESIAN_POINT('Ctrl Pts',(2.35474165464431,39.450929005508,12.4446749399196));
#47728=CARTESIAN_POINT('Ctrl Pts',(2.40533665564667,39.4696436602941,12.5994621647907));
#47729=CARTESIAN_POINT('Ctrl Pts',(2.50465014408154,39.5219387860576,13.0467179202076));
#47730=CARTESIAN_POINT('Ctrl Pts',(2.51703839078177,39.5545358882292,13.3444754963876));
#47731=CARTESIAN_POINT('Ctrl Pts',(2.43198342987368,39.6248445748884,13.9687351236858));
#47732=CARTESIAN_POINT('Ctrl Pts',(2.32087015026554,39.6625696127848,14.2876059817832));
#47733=CARTESIAN_POINT('Ctrl Pts',(1.99069784765935,39.7335660593531,14.8443579787623));
#47734=CARTESIAN_POINT('Ctrl Pts',(1.78195990589462,39.7665295035597,15.0811655365627));
#47735=CARTESIAN_POINT('Ctrl Pts',(1.40684512634722,39.8183912037277,15.372951244866));
#47736=CARTESIAN_POINT('Ctrl Pts',(1.2693272398596,39.8360946785057,15.4598980632706));
#47737=CARTESIAN_POINT('Ctrl Pts',(0.861901378213536,39.8850927100737,15.6650501996874));
#47738=CARTESIAN_POINT('Ctrl Pts',(0.578200738693645,39.9151341009516,15.7499114424441));
#47739=CARTESIAN_POINT('Ctrl Pts',(-0.0453251220284939,39.980052375392,
15.8217714213526));
#47740=CARTESIAN_POINT('Ctrl Pts',(-0.381226569776738,40.0154482219679,
15.7932152220384));
#47741=CARTESIAN_POINT('Ctrl Pts',(-0.995051864017533,40.0799329075217,
15.6137225977727));
#47742=CARTESIAN_POINT('Ctrl Pts',(-1.2702394715904,40.1088324258242,15.4748466918823));
#47743=CARTESIAN_POINT('Ctrl Pts',(-1.73611838947518,40.1668483767574,15.1204622490944));
#47744=CARTESIAN_POINT('Ctrl Pts',(-1.9287966619377,40.1944548137299,14.9149472035747));
#47745=CARTESIAN_POINT('Ctrl Pts',(-2.21484989923174,40.242696624887,14.4836180021855));
#47746=CARTESIAN_POINT('Ctrl Pts',(-2.31729815284615,40.2635916253591,14.2678011957536));
#47747=CARTESIAN_POINT('Ctrl Pts',(-2.38773478971345,40.2851228191638,14.0407581076114));
#47748=CARTESIAN_POINT('',(-2.50017028063955,40.3932053939429,13.3030872967355));
#47749=CARTESIAN_POINT('Ctrl Pts',(-2.38677922580708,40.2852562553959,14.0403593245475));
#47750=CARTESIAN_POINT('Ctrl Pts',(-2.39184533847209,40.2871499823883,14.0260557859757));
#47751=CARTESIAN_POINT('Ctrl Pts',(-2.39633423477753,40.289226676514,14.0118231755317));
#47752=CARTESIAN_POINT('Ctrl Pts',(-2.40062259401216,40.2914645379331,13.997116667899));
#47753=CARTESIAN_POINT('Ctrl Pts',(-2.40187210465684,40.2921165895714,13.9928315936252));
#47754=CARTESIAN_POINT('Ctrl Pts',(-2.4031190599626,40.2927734317743,13.9885118894307));
#47755=CARTESIAN_POINT('Ctrl Pts',(-2.40434046058925,40.2934230064818,13.9842373073297));
#47756=CARTESIAN_POINT('Ctrl Pts',(-2.41558848106818,40.2994050155402,13.9448721834205));
#47757=CARTESIAN_POINT('Ctrl Pts',(-2.42583769655266,40.305368540572,13.9053526778095));
#47758=CARTESIAN_POINT('Ctrl Pts',(-2.43511138146535,40.3113250164977,13.8656194028656));
#47759=CARTESIAN_POINT('Ctrl Pts',(-2.45309587693699,40.3228764348737,13.7885644985822));
#47760=CARTESIAN_POINT('Ctrl Pts',(-2.46737957066467,40.3343853235716,13.7108178911225));
#47761=CARTESIAN_POINT('Ctrl Pts',(-2.47793032286022,40.3458219873893,13.632612756334));
#47762=CARTESIAN_POINT('Ctrl Pts',(-2.4791981035249,40.3471962193861,13.6232156104314));
#47763=CARTESIAN_POINT('Ctrl Pts',(-2.48041195249927,40.348569413132,13.6138117924165));
#47764=CARTESIAN_POINT('Ctrl Pts',(-2.48157178479104,40.3499415208601,13.6044016653308));
#47765=CARTESIAN_POINT('Ctrl Pts',(-2.48817989424502,40.3577590632017,13.5507877504573));
#47766=CARTESIAN_POINT('Ctrl Pts',(-2.49303592985813,40.3655409146392,13.4969698553965));
#47767=CARTESIAN_POINT('Ctrl Pts',(-2.49612472346855,40.3732761501296,13.4430096946578));
#47768=CARTESIAN_POINT('Ctrl Pts',(-2.4961274246664,40.3732829147128,13.4429625056616));
#47769=CARTESIAN_POINT('Ctrl Pts',(-2.49613012451236,40.3732896792603,13.442915316556));
#47770=CARTESIAN_POINT('Ctrl Pts',(-2.49613282300637,40.3732964437722,13.4428681273412));
#47771=CARTESIAN_POINT('Ctrl Pts',(-2.4972156371881,40.3760108130897,13.4239326948875));
#47772=CARTESIAN_POINT('Ctrl Pts',(-2.49808077532599,40.3787194363049,13.4049796606347));
#47773=CARTESIAN_POINT('Ctrl Pts',(-2.49872813109644,40.3814232168861,13.3860127359362));
#47774=CARTESIAN_POINT('Ctrl Pts',(-2.49967173148025,40.3853643084938,13.3583661183537));
#47775=CARTESIAN_POINT('Ctrl Pts',(-2.50015159683804,40.3892908682538,13.3307197832459));
#47776=CARTESIAN_POINT('Ctrl Pts',(-2.50017028063955,40.3932053939429,13.3030872967355));
#47777=CARTESIAN_POINT('Ctrl Pts',(-2.49999807917248,40.3932899595023,13.3030990537122));
#47778=CARTESIAN_POINT('Ctrl Pts',(-2.49999935976079,40.3934360152657,13.3020660066571));
#47779=CARTESIAN_POINT('Ctrl Pts',(-2.50000000000072,40.3935820507829,13.3010329879761));
#47780=CARTESIAN_POINT('Ctrl Pts',(-2.5,40.3937280662289,13.2999999982622));
#47781=CARTESIAN_POINT('Ctrl Pts',(-2.5,39.6612570972331,13.3000000000001));
#47782=CARTESIAN_POINT('Ctrl Pts',(-2.5,39.653123693213,13.3556707326246));
#47783=CARTESIAN_POINT('Ctrl Pts',(-2.49814051750878,39.6450187406706,13.4113969395304));
#47784=CARTESIAN_POINT('Ctrl Pts',(-2.47203053406049,39.5886061827757,13.8011874110541));
#47785=CARTESIAN_POINT('Ctrl Pts',(-2.38274677131432,39.5417764947153,14.1274812070693));
#47786=CARTESIAN_POINT('Ctrl Pts',(-2.11676137747124,39.4571269586374,14.6544383766883));
#47787=CARTESIAN_POINT('Ctrl Pts',(-1.96740882675978,39.4207476870172,14.8635361530646));
#47788=CARTESIAN_POINT('Ctrl Pts',(-1.55539887166156,39.3402050054438,15.285547448765));
#47789=CARTESIAN_POINT('Ctrl Pts',(-1.27641278910592,39.2962232120126,15.4754170763141));
#47790=CARTESIAN_POINT('Ctrl Pts',(-0.683041882390598,39.20670885425,15.7247077964409));
#47791=CARTESIAN_POINT('Ctrl Pts',(-0.37803167167398,39.1625312623935,15.7905412413853));
#47792=CARTESIAN_POINT('Ctrl Pts',(0.24676645044173,39.075250993696,15.8077393947595));
#47793=CARTESIAN_POINT('Ctrl Pts',(0.561122788821101,39.0340312077439,15.7566007588563));
#47794=CARTESIAN_POINT('Ctrl Pts',(1.15912961578192,38.9487172099549,15.538157668776));
#47795=CARTESIAN_POINT('Ctrl Pts',(1.43642055723788,38.9051946996757,15.3711177459246));
#47796=CARTESIAN_POINT('Ctrl Pts',(1.86818525975432,38.8253475582604,14.9816366012639));
#47797=CARTESIAN_POINT('Ctrl Pts',(2.03338676521065,38.7901985060572,14.7776534031731));
#47798=CARTESIAN_POINT('Ctrl Pts',(2.33203173855803,38.7114740038227,14.2613354170784));
#47799=CARTESIAN_POINT('Ctrl Pts',(2.43986117781533,38.6681480807116,13.9400460554133));
#47800=CARTESIAN_POINT('Ctrl Pts',(2.5191469391265,38.5837584416547,13.2993991938612));
#47801=CARTESIAN_POINT('Ctrl Pts',(2.49966976205757,38.5434006298179,12.987311343042));
#47802=CARTESIAN_POINT('Ctrl Pts',(2.3829592714491,38.4816382884601,12.5260638648528));
#47803=CARTESIAN_POINT('Ctrl Pts',(2.3264199951752,38.4602954115601,12.3698131664047));
#47804=CARTESIAN_POINT('Ctrl Pts',(2.11089682384098,38.3958959010657,11.919715190783));
#47805=CARTESIAN_POINT('Ctrl Pts',(1.90829196915177,38.3533731762915,11.650905560836));
#47806=CARTESIAN_POINT('Ctrl Pts',(1.49340588822079,38.2821957701758,11.2828973519894));
#47807=CARTESIAN_POINT('Ctrl Pts',(1.3090878023652,38.2539541001287,11.1586759057338));
#47808=CARTESIAN_POINT('Ctrl Pts',(0.971035791073398,38.2060186696871,10.9910097382391));
#47809=CARTESIAN_POINT('Ctrl Pts',(0.825057175685232,38.1863712699139,10.9349136382988));
#47810=CARTESIAN_POINT('Ctrl Pts',(0.372703141526457,38.1271811573218,10.8081084724525));
#47811=CARTESIAN_POINT('Ctrl Pts',(0.0573506802001572,38.0880693821565,
10.7810431777528));
#47812=CARTESIAN_POINT('Ctrl Pts',(-0.582631752832415,38.0070454280135,
10.8466001293174));
#47813=CARTESIAN_POINT('Ctrl Pts',(-0.9006695475721,37.9659291787871,10.9446979810559));
#47814=CARTESIAN_POINT('Ctrl Pts',(-1.45574598758833,37.8869746020048,11.245303144746));
#47815=CARTESIAN_POINT('Ctrl Pts',(-1.69282980968617,37.8497733454819,11.4357732717793));
#47816=CARTESIAN_POINT('Ctrl Pts',(-2.06678961815314,37.7793227065523,11.8678221581079));
#47817=CARTESIAN_POINT('Ctrl Pts',(-2.20916254837202,37.7465508507352,12.0990102715484));
#47818=CARTESIAN_POINT('Ctrl Pts',(-2.36787119150113,37.6957025312189,12.4846114182324));
#47819=CARTESIAN_POINT('Ctrl Pts',(-2.41176838513802,37.6777969568209,12.6254296680502));
#47820=CARTESIAN_POINT('Ctrl Pts',(-2.48098939879585,37.6379899850485,12.944073891754));
#47821=CARTESIAN_POINT('Ctrl Pts',(-2.5,37.6162662367362,13.1219981617627));
#47822=CARTESIAN_POINT('Ctrl Pts',(-2.5,37.5946437602656,13.3));
#47823=CARTESIAN_POINT('Origin',(0.,70.2,13.3));
#47824=CARTESIAN_POINT('',(-2.5,35.7784429531659,13.3000000000001));
#47825=CARTESIAN_POINT('',(-2.5,36.4895163993155,13.2999999996801));
#47826=CARTESIAN_POINT('',(-2.5,70.2,13.3));
#47827=CARTESIAN_POINT('Ctrl Pts',(-2.5,36.4895163993155,13.2999999993602));
#47828=CARTESIAN_POINT('Ctrl Pts',(-2.49999999995295,36.5164180716991,13.1161283443394));
#47829=CARTESIAN_POINT('Ctrl Pts',(-2.47971719676694,36.5426838350161,12.9328114292078));
#47830=CARTESIAN_POINT('Ctrl Pts',(-2.40581734184516,36.5922050891777,12.6030249444719));
#47831=CARTESIAN_POINT('Ctrl Pts',(-2.35832606702688,36.6151111253982,12.456202198798));
#47832=CARTESIAN_POINT('Ctrl Pts',(-2.19166732682489,36.679208359259,12.0675547917492));
#47833=CARTESIAN_POINT('Ctrl Pts',(-2.04649721218126,36.7210257240423,11.8391132907617));
#47834=CARTESIAN_POINT('Ctrl Pts',(-1.64339674723545,36.8111514981178,11.3860721774674));
#47835=CARTESIAN_POINT('Ctrl Pts',(-1.3703643495528,36.8565045600032,11.1819499306933));
#47836=CARTESIAN_POINT('Ctrl Pts',(-0.930516986354473,36.9255076032598,
10.9748808728237));
#47837=CARTESIAN_POINT('Ctrl Pts',(-0.790869092248727,36.9468256709158,
10.9237542248518));
#47838=CARTESIAN_POINT('Ctrl Pts',(-0.373829622410181,37.0096987915266,
10.8119160537901));
#47839=CARTESIAN_POINT('Ctrl Pts',(-0.089576260525372,37.0517207460895,
10.785572083852));
#47840=CARTESIAN_POINT('Ctrl Pts',(0.352206631553183,37.1146775549043,10.8197933542263));
#47841=CARTESIAN_POINT('Ctrl Pts',(0.509832674521626,37.1366856662043,10.8473337001418));
#47842=CARTESIAN_POINT('Ctrl Pts',(0.821882994016063,37.1816746792334,10.9332730038645));
#47843=CARTESIAN_POINT('Ctrl Pts',(0.975304176411618,37.2045973705891,10.9922595136116));
#47844=CARTESIAN_POINT('Ctrl Pts',(1.26582779450248,37.2498606385876,11.1381392135487));
#47845=CARTESIAN_POINT('Ctrl Pts',(1.40249855676195,37.2719384241438,11.2241943982254));
#47846=CARTESIAN_POINT('Ctrl Pts',(1.73582296806904,37.3298506647626,11.4821223403624));
#47847=CARTESIAN_POINT('Ctrl Pts',(1.9155823494612,37.3660185428071,11.672626415537));
#47848=CARTESIAN_POINT('Ctrl Pts',(2.25181029285251,37.446292962554,12.1636152157564));
#47849=CARTESIAN_POINT('Ctrl Pts',(2.38357327113818,37.4893590535764,12.4749734475991));
#47850=CARTESIAN_POINT('Ctrl Pts',(2.51390957361782,37.5774358033074,13.1176269747578));
#47851=CARTESIAN_POINT('Ctrl Pts',(2.51653062361988,37.6213426693713,13.4414966009373));
#47852=CARTESIAN_POINT('Ctrl Pts',(2.40771056069729,37.7020097291258,14.0268330908957));
#47853=CARTESIAN_POINT('Ctrl Pts',(2.31342928036838,37.7375889165503,14.286650095782));
#47854=CARTESIAN_POINT('Ctrl Pts',(2.02413879705667,37.8143820612513,14.8007484593905));
#47855=CARTESIAN_POINT('Ctrl Pts',(1.81898422348574,37.8553460540575,15.0437380248159));
#47856=CARTESIAN_POINT('Ctrl Pts',(1.36398729756465,37.9330087116023,15.4125147219413));
#47857=CARTESIAN_POINT('Ctrl Pts',(1.12752760846014,37.968797771397,15.5476473510898));
#47858=CARTESIAN_POINT('Ctrl Pts',(0.560752962874162,38.0474284766851,15.7591313971231));
#47859=CARTESIAN_POINT('Ctrl Pts',(0.227197742383383,38.0898486321667,15.8120102985733));
#47860=CARTESIAN_POINT('Ctrl Pts',(-0.428500615184119,38.1742873286512,
15.7839513490688));
#47861=CARTESIAN_POINT('Ctrl Pts',(-0.744476071039354,38.2152359311912,
15.7081968566207));
#47862=CARTESIAN_POINT('Ctrl Pts',(-1.1861135341602,38.2771193234957,15.5067733757899));
#47863=CARTESIAN_POINT('Ctrl Pts',(-1.32781794756963,38.2978322412313,15.4245276218427));
#47864=CARTESIAN_POINT('Ctrl Pts',(-1.72782306550425,38.3603536520828,15.1366077188321));
#47865=CARTESIAN_POINT('Ctrl Pts',(-1.95453124588622,38.4016882989555,14.8932143590788));
#47866=CARTESIAN_POINT('Ctrl Pts',(-2.30134502414229,38.4848482211263,14.3311940669407));
#47867=CARTESIAN_POINT('Ctrl Pts',(-2.41751828882584,38.5258444555845,14.0177667258479));
#47868=CARTESIAN_POINT('Ctrl Pts',(-2.48973048211815,38.5834135228102,13.5614970169554));
#47869=CARTESIAN_POINT('Ctrl Pts',(-2.49999999977056,38.5996652405177,13.4308272869097));
#47870=CARTESIAN_POINT('Ctrl Pts',(-2.5,38.6159089611155,13.3000000043844));
#47871=CARTESIAN_POINT('',(-0.846350554922702,36.2086580169322,10.9476201968673));
#47872=CARTESIAN_POINT('Ctrl Pts',(-2.5,37.5946437602656,13.3));
#47873=CARTESIAN_POINT('Ctrl Pts',(-2.5,37.5758608613471,13.4546256988409));
#47874=CARTESIAN_POINT('Ctrl Pts',(-2.48565439642402,37.5571557154162,13.6093100923753));
#47875=CARTESIAN_POINT('Ctrl Pts',(-2.42722680302701,37.5190899388255,13.9200051148318));
#47876=CARTESIAN_POINT('Ctrl Pts',(-2.38235405824464,37.4998674146584,14.074743695524));
#47877=CARTESIAN_POINT('Ctrl Pts',(-2.19953877727962,37.4405207481708,14.5342901767562));
#47878=CARTESIAN_POINT('Ctrl Pts',(-2.01523932029944,37.4007250256698,14.8166736003359));
#47879=CARTESIAN_POINT('Ctrl Pts',(-1.55195139548261,37.3226156505755,15.2869258589061));
#47880=CARTESIAN_POINT('Ctrl Pts',(-1.27970061915826,37.2848103581954,15.4722797841508));
#47881=CARTESIAN_POINT('Ctrl Pts',(-0.832456925475637,37.227433105574,15.662747169702));
#47882=CARTESIAN_POINT('Ctrl Pts',(-0.679686613721388,37.2086502929714,
15.7111394399072));
#47883=CARTESIAN_POINT('Ctrl Pts',(-0.230815413171425,37.1551129962611,
15.8072317848003));
#47884=CARTESIAN_POINT('Ctrl Pts',(0.0705894370523697,37.1212759056622,
15.8168486334183));
#47885=CARTESIAN_POINT('Ctrl Pts',(0.696802929063635,37.0484863977452,15.7240331077785));
#47886=CARTESIAN_POINT('Ctrl Pts',(1.01399181665485,37.0100092636035,15.6094059933073));
#47887=CARTESIAN_POINT('Ctrl Pts',(1.57564176945598,36.9358143495937,15.267731913643));
#47888=CARTESIAN_POINT('Ctrl Pts',(1.81674497014354,36.9002892620361,15.0475850688783));
#47889=CARTESIAN_POINT('Ctrl Pts',(2.18687825476669,36.8301304928963,14.5476811492629));
#47890=CARTESIAN_POINT('Ctrl Pts',(2.32017373464543,36.7971620961948,14.2777673705857));
#47891=CARTESIAN_POINT('Ctrl Pts',(2.44629623413705,36.747711257298,13.8390132560229));
#47892=CARTESIAN_POINT('Ctrl Pts',(2.47543338932105,36.7308325383625,13.6835728546094));
#47893=CARTESIAN_POINT('Ctrl Pts',(2.51988750766847,36.6776037066035,13.1947716125488));
#47894=CARTESIAN_POINT('Ctrl Pts',(2.48348290504879,36.6411712216394,12.8603075551738));
#47895=CARTESIAN_POINT('Ctrl Pts',(2.28547246478389,36.572464920124,12.2372861160282));
#47896=CARTESIAN_POINT('Ctrl Pts',(2.13052447711007,36.5400411722486,11.9532964471577));
#47897=CARTESIAN_POINT('Ctrl Pts',(1.73688060457641,36.4751983782657,11.4775185956148));
#47898=CARTESIAN_POINT('Ctrl Pts',(1.50824003305037,36.4448691380507,11.2841788113515));
#47899=CARTESIAN_POINT('Ctrl Pts',(1.11149638239736,36.3998183440908,11.0548919430727));
#47900=CARTESIAN_POINT('Ctrl Pts',(0.964611197203937,36.3843195301676,10.9879754236812));
#47901=CARTESIAN_POINT('Ctrl Pts',(0.523767514788698,36.3385852022954,10.8365158384325));
#47902=CARTESIAN_POINT('Ctrl Pts',(0.219386868080082,36.3080353712077,10.7910011058256));
#47903=CARTESIAN_POINT('Ctrl Pts',(-0.34532869839718,36.2549870908647,10.8103777802712));
#47904=CARTESIAN_POINT('Ctrl Pts',(-0.601927411664119,36.2321980347213,
10.8596804591393));
#47905=CARTESIAN_POINT('Ctrl Pts',(-0.846350554899145,36.2086580169353,
10.9476201968598));
#47906=CARTESIAN_POINT('Ctrl Pts',(-0.846422303514195,36.2091836693201,
10.9476460121585));
#47907=CARTESIAN_POINT('Ctrl Pts',(-1.0597631465936,36.1762938847118,11.0244101593771));
#47908=CARTESIAN_POINT('Ctrl Pts',(-1.26174119076661,36.1433776234327,11.1298657021809));
#47909=CARTESIAN_POINT('Ctrl Pts',(-1.66633664079304,36.0731727395765,11.416968366155));
#47910=CARTESIAN_POINT('Ctrl Pts',(-1.85933278671221,36.0362450266669,11.607246829317));
#47911=CARTESIAN_POINT('Ctrl Pts',(-2.20651957219189,35.953839120045,12.082201117234));
#47912=CARTESIAN_POINT('Ctrl Pts',(-2.3437487822392,35.9087830563224,12.3733919715845));
#47913=CARTESIAN_POINT('Ctrl Pts',(-2.4740799188374,35.8352051968173,12.8847061362566));
#47914=CARTESIAN_POINT('Ctrl Pts',(-2.5,35.8068403729879,13.0921698303673));
#47915=CARTESIAN_POINT('Ctrl Pts',(-2.5,35.7784429531659,13.3000000000002));
#47916=CARTESIAN_POINT('Origin',(0.,70.2,13.3));
#47917=CARTESIAN_POINT('',(-2.5,33.7644650054088,13.3000000002187));
#47918=CARTESIAN_POINT('',(-2.5,34.7604761263293,13.3000000000185));
#47919=CARTESIAN_POINT('',(-2.5,70.2,13.3));
#47920=CARTESIAN_POINT('',(-2.49999982102973,34.7605873473017,13.2990540341987));
#47921=CARTESIAN_POINT('Ctrl Pts',(-2.5,34.7604761263292,13.3000000000369));
#47922=CARTESIAN_POINT('Ctrl Pts',(-2.5,34.76051358954,13.2996813693674));
#47923=CARTESIAN_POINT('Ctrl Pts',(-2.49999994159659,34.7605498847325,13.2993726684756));
#47924=CARTESIAN_POINT('Ctrl Pts',(-2.49999982102973,34.7605873473017,13.2990540341987));
#47925=CARTESIAN_POINT('',(-1.81156843952179,36.1875454226321,15.0225226611708));
#47926=CARTESIAN_POINT('Ctrl Pts',(-2.49999982102973,34.7605873473017,13.2990540341987));
#47927=CARTESIAN_POINT('Ctrl Pts',(-2.49988526272856,34.7961829353405,12.9962991861577));
#47928=CARTESIAN_POINT('Ctrl Pts',(-2.44478214320481,34.8310453620436,12.6961179853287));
#47929=CARTESIAN_POINT('Ctrl Pts',(-2.21937139071209,34.9069292536943,12.1020579693682));
#47930=CARTESIAN_POINT('Ctrl Pts',(-2.04040483388747,34.9462712647688,11.8175882391226));
#47931=CARTESIAN_POINT('Ctrl Pts',(-1.61883026837122,35.0167936072861,11.3746355767685));
#47932=CARTESIAN_POINT('Ctrl Pts',(-1.39436054437815,35.0480617144675,11.206345733161));
#47933=CARTESIAN_POINT('Ctrl Pts',(-0.851399687633854,35.1193207762706,
10.9260536485853));
#47934=CARTESIAN_POINT('Ctrl Pts',(-0.528436593682016,35.1578251634748,
10.8339507381643));
#47935=CARTESIAN_POINT('Ctrl Pts',(0.0788819293477749,35.2260961580154,
10.7859847309334));
#47936=CARTESIAN_POINT('Ctrl Pts',(0.356262375455895,35.2560238915552,10.8101080910456));
#47937=CARTESIAN_POINT('Ctrl Pts',(0.948103528783883,35.3255621256351,10.9626771769118));
#47938=CARTESIAN_POINT('Ctrl Pts',(1.25226516906477,35.3637818791458,11.1104808091419));
#47939=CARTESIAN_POINT('Ctrl Pts',(1.74208957173634,35.4308120215263,11.48493736365));
#47940=CARTESIAN_POINT('Ctrl Pts',(1.93530129987065,35.4599097139804,11.6925391593047));
#47941=CARTESIAN_POINT('Ctrl Pts',(2.1802985620806,35.5090599584891,12.0657192359799));
#47942=CARTESIAN_POINT('Ctrl Pts',(2.25688961478123,35.5275353176654,12.2120648221172));
#47943=CARTESIAN_POINT('Ctrl Pts',(2.4195931220143,35.5755168003784,12.6154731181076));
#47944=CARTESIAN_POINT('Ctrl Pts',(2.47940567072807,35.6039391298189,12.8808651027996));
#47945=CARTESIAN_POINT('Ctrl Pts',(2.504627900418,35.6470887925279,13.3027428438554));
#47946=CARTESIAN_POINT('Ctrl Pts',(2.49981578545345,35.6623656760365,13.4551760500165));
#47947=CARTESIAN_POINT('Ctrl Pts',(2.44034072548846,35.7125940126195,13.9370946533036));
#47948=CARTESIAN_POINT('Ctrl Pts',(2.33368952095993,35.7486272092269,14.2566886833866));
#47949=CARTESIAN_POINT('Ctrl Pts',(2.0210274980302,35.8106804137796,14.8005548952924));
#47950=CARTESIAN_POINT('Ctrl Pts',(1.83107790409723,35.8369690342989,15.0272182923819));
#47951=CARTESIAN_POINT('Ctrl Pts',(1.35024119677199,35.8976767669939,15.4303522275185));
#47952=CARTESIAN_POINT('Ctrl Pts',(1.05363837512255,35.9324273498156,15.5916543627122));
#47953=CARTESIAN_POINT('Ctrl Pts',(0.461734683688209,35.9892932414591,15.7734383683323));
#47954=CARTESIAN_POINT('Ctrl Pts',(0.177422069362182,36.0121792761678,15.8098899341102));
#47955=CARTESIAN_POINT('Ctrl Pts',(-0.43915284457503,36.0652002822201,15.7834842281171));
#47956=CARTESIAN_POINT('Ctrl Pts',(-0.765391457556897,36.0963838848401,
15.7031261159702));
#47957=CARTESIAN_POINT('Ctrl Pts',(-1.34626741194371,36.1469262513021,15.4291419512213));
#47958=CARTESIAN_POINT('Ctrl Pts',(-1.59879965261283,36.166409407584,15.2466270173068));
#47959=CARTESIAN_POINT('Ctrl Pts',(-1.81175956334301,36.1879287370222,15.0226512370864));
#47960=CARTESIAN_POINT('',(-2.49999928840966,36.4881581266667,13.3018862532181));
#47961=CARTESIAN_POINT('Ctrl Pts',(-1.81183660638924,36.1881958906855,15.0225702051725));
#47962=CARTESIAN_POINT('Ctrl Pts',(-1.81892097439324,36.189477370912,15.0151187136488));
#47963=CARTESIAN_POINT('Ctrl Pts',(-1.82595923910941,36.1907591156391,15.0076235328133));
#47964=CARTESIAN_POINT('Ctrl Pts',(-1.83293662276303,36.1923838835242,15.0001009784522));
#47965=CARTESIAN_POINT('Ctrl Pts',(-1.84686725918764,36.1956278001275,14.9850818860543));
#47966=CARTESIAN_POINT('Ctrl Pts',(-1.86061157959221,36.1989020602568,14.9698934450896));
#47967=CARTESIAN_POINT('Ctrl Pts',(-1.87416777695279,36.2021760116161,14.9545377432479));
#47968=CARTESIAN_POINT('Ctrl Pts',(-1.90119016409984,36.2087021766444,14.9239282951081));
#47969=CARTESIAN_POINT('Ctrl Pts',(-1.92745885272653,36.215225832546,14.8926611467449));
#47970=CARTESIAN_POINT('Ctrl Pts',(-1.95294978830251,36.2217532634333,14.8607649164333));
#47971=CARTESIAN_POINT('Ctrl Pts',(-2.00440094616609,36.2349282948489,14.7963852479774));
#47972=CARTESIAN_POINT('Ctrl Pts',(-2.05255602129216,36.248114920072,14.7296015234022));
#47973=CARTESIAN_POINT('Ctrl Pts',(-2.09726221388262,36.2613077135368,14.6606951187611));
#47974=CARTESIAN_POINT('Ctrl Pts',(-2.14223936592775,36.2745804671126,14.5913710797668));
#47975=CARTESIAN_POINT('Ctrl Pts',(-2.18372552160831,36.2878594629992,14.5198993718759));
#47976=CARTESIAN_POINT('Ctrl Pts',(-2.22157690179356,36.3011401026881,14.4465583584874));
#47977=CARTESIAN_POINT('Ctrl Pts',(-2.25890395136072,36.3142367742897,14.374233290586));
#47978=CARTESIAN_POINT('Ctrl Pts',(-2.29269662736909,36.3273350454751,14.3000911924193));
#47979=CARTESIAN_POINT('Ctrl Pts',(-2.32282676136498,36.3404313990264,14.224378621933));
#47980=CARTESIAN_POINT('Ctrl Pts',(-2.34756675175684,36.3511848746356,14.1622106851216));
#47981=CARTESIAN_POINT('Ctrl Pts',(-2.36983787706874,36.3619370729079,14.0989837571188));
#47982=CARTESIAN_POINT('Ctrl Pts',(-2.38956957911678,36.3726865049897,14.0348178186188));
#47983=CARTESIAN_POINT('Ctrl Pts',(-2.42230018775947,36.3905174784022,13.9283804613081));
#47984=CARTESIAN_POINT('Ctrl Pts',(-2.44782899532107,36.4080893877882,13.8200452990317));
#47985=CARTESIAN_POINT('Ctrl Pts',(-2.46605367650299,36.4253945284877,13.7105840530343));
#47986=CARTESIAN_POINT('Ctrl Pts',(-2.47192729325118,36.4309717873285,13.6753058826592));
#47987=CARTESIAN_POINT('Ctrl Pts',(-2.4770427155916,36.4365213511696,13.63990910798));
#47988=CARTESIAN_POINT('Ctrl Pts',(-2.4813971292479,36.4420430033563,13.6044146628536));
#47989=CARTESIAN_POINT('Ctrl Pts',(-2.49369610207015,36.4576388230323,13.5041611613707));
#47990=CARTESIAN_POINT('Ctrl Pts',(-2.49992291223824,36.4730118750243,13.4031135817416));
#47991=CARTESIAN_POINT('Ctrl Pts',(-2.49999928840966,36.4881581266667,13.3018862532181));
#47992=CARTESIAN_POINT('Ctrl Pts',(-2.49999916661337,36.489217714823,13.3020413065548));
#47993=CARTESIAN_POINT('Ctrl Pts',(-2.49999972221066,36.4893172865525,13.3013608635544));
#47994=CARTESIAN_POINT('Ctrl Pts',(-2.50000000000017,36.4894168480168,13.3006804277656));
#47995=CARTESIAN_POINT('Ctrl Pts',(-2.5,36.4895163993155,13.2999999993602));
#47996=CARTESIAN_POINT('',(-2.10782919047724,33.9999546381749,11.9560483405783));
#47997=CARTESIAN_POINT('Ctrl Pts',(-2.5,35.7784429531659,13.3000000000002));
#47998=CARTESIAN_POINT('Ctrl Pts',(-2.5,35.7627803554752,13.4146287358281));
#47999=CARTESIAN_POINT('Ctrl Pts',(-2.49211673543698,35.7471213482476,13.5293708036824));
#48000=CARTESIAN_POINT('Ctrl Pts',(-2.43395053540011,35.6894310917777,13.948793271294));
#48001=CARTESIAN_POINT('Ctrl Pts',(-2.33546939726797,35.6477491297446,14.2437533052336));
#48002=CARTESIAN_POINT('Ctrl Pts',(-2.02286969681855,35.5613152085308,14.8068850758757));
#48003=CARTESIAN_POINT('Ctrl Pts',(-1.80244624105573,35.5176163173916,15.0646366521508));
#48004=CARTESIAN_POINT('Ctrl Pts',(-1.29670845882954,35.4324203175144,15.4591561473659));
#48005=CARTESIAN_POINT('Ctrl Pts',(-1.0232670581393,35.3918957264238,15.6013840293111));
#48006=CARTESIAN_POINT('Ctrl Pts',(-0.57538516105805,35.3303880647178,15.7383171466564));
#48007=CARTESIAN_POINT('Ctrl Pts',(-0.415546395330684,35.3092506195382,
15.770584746121));
#48008=CARTESIAN_POINT('Ctrl Pts',(0.0604876803035786,35.247045108235,15.8191427816985));
#48009=CARTESIAN_POINT('Ctrl Pts',(0.377948259338413,35.2064302707169,15.7913710836388));
#48010=CARTESIAN_POINT('Ctrl Pts',(0.842453040063227,35.1443465641293,15.6596908634744));
#48011=CARTESIAN_POINT('Ctrl Pts',(0.998106002767982,35.1230218397156,15.5981857595108));
#48012=CARTESIAN_POINT('Ctrl Pts',(1.2906191205536,35.0809419559713,15.4472343310581));
#48013=CARTESIAN_POINT('Ctrl Pts',(1.42719287203555,35.0602890630069,15.3589893598535));
#48014=CARTESIAN_POINT('Ctrl Pts',(1.81579281967665,34.9971449917828,15.0505408321967));
#48015=CARTESIAN_POINT('Ctrl Pts',(2.03313609359154,34.9554187807748,14.7926160878873));
#48016=CARTESIAN_POINT('Ctrl Pts',(2.34860970661178,34.8729588784015,14.2157888108851));
#48017=CARTESIAN_POINT('Ctrl Pts',(2.44729156605952,34.8329736674971,13.9045136917868));
#48018=CARTESIAN_POINT('Ctrl Pts',(2.50209267416223,34.7729763375332,13.423624155607));
#48019=CARTESIAN_POINT('Ctrl Pts',(2.50486966442622,34.7531962872763,13.2627979850154));
#48020=CARTESIAN_POINT('Ctrl Pts',(2.46646526313834,34.6932587855849,12.7774161968489));
#48021=CARTESIAN_POINT('Ctrl Pts',(2.37723685619148,34.6537100764755,12.4601643297973));
#48022=CARTESIAN_POINT('Ctrl Pts',(2.15774410174524,34.5946730153388,12.0274704339981));
#48023=CARTESIAN_POINT('Ctrl Pts',(2.07262060717391,34.5754789665299,11.8930738701525));
#48024=CARTESIAN_POINT('Ctrl Pts',(1.87717294151182,34.5370104578763,11.6411256027248));
#48025=CARTESIAN_POINT('Ctrl Pts',(1.7670869458932,34.5178261190561,11.5243167589954));
#48026=CARTESIAN_POINT('Ctrl Pts',(1.39551967463749,34.4586456697698,11.1990837780451));
#48027=CARTESIAN_POINT('Ctrl Pts',(1.10295796694357,34.4191313361643,11.031772149259));
#48028=CARTESIAN_POINT('Ctrl Pts',(0.632527884577907,34.3606794892829,10.8759327976478));
#48029=CARTESIAN_POINT('Ctrl Pts',(0.474309764613275,34.3417414496223,10.8400757207167));
#48030=CARTESIAN_POINT('Ctrl Pts',(-0.0132039176921074,34.2841108186178,
10.7784083992674));
#48031=CARTESIAN_POINT('Ctrl Pts',(-0.345159421783913,34.2459202829331,
10.8020965808484));
#48032=CARTESIAN_POINT('Ctrl Pts',(-0.811350338434691,34.1903158765828,
10.9303191753661));
#48033=CARTESIAN_POINT('Ctrl Pts',(-0.955632434546944,34.172761615236,10.9847363963674));
#48034=CARTESIAN_POINT('Ctrl Pts',(-1.30888815416826,34.1277598923389,11.1566550628106));
#48035=CARTESIAN_POINT('Ctrl Pts',(-1.50770133280881,34.1005301349767,11.2915237191095));
#48036=CARTESIAN_POINT('Ctrl Pts',(-1.84710194884547,34.0487412720109,11.6009638960582));
#48037=CARTESIAN_POINT('Ctrl Pts',(-1.98954353185177,34.0243565893973,11.7702174610211));
#48038=CARTESIAN_POINT('Ctrl Pts',(-2.10796460894866,33.9998221304067,11.9559444924335));
#48039=CARTESIAN_POINT('',(-2.49999978507887,33.7646310379939,13.2989633681452));
#48040=CARTESIAN_POINT('Ctrl Pts',(-2.1079929847411,34.0001676959785,11.9559889969638));
#48041=CARTESIAN_POINT('Ctrl Pts',(-2.2350777214743,33.9597552880639,12.1553130597104));
#48042=CARTESIAN_POINT('Ctrl Pts',(-2.33326888345894,33.9189932195931,12.3716816396712));
#48043=CARTESIAN_POINT('Ctrl Pts',(-2.46608509532503,33.8399117586071,12.8261052420337));
#48044=CARTESIAN_POINT('Ctrl Pts',(-2.49990145924373,33.8026104324006,13.0618352444272));
#48045=CARTESIAN_POINT('Ctrl Pts',(-2.49999978507887,33.7646310379939,13.2989633681452));
#48046=CARTESIAN_POINT('Ctrl Pts',(-2.49999978507887,33.7646310379939,13.2989633681452));
#48047=CARTESIAN_POINT('Ctrl Pts',(-2.49999992836101,33.7645756937527,13.2993089154159));
#48048=CARTESIAN_POINT('Ctrl Pts',(-2.50000000000006,33.7645203495589,13.2996544595209));
#48049=CARTESIAN_POINT('Ctrl Pts',(-2.5,33.7644650054088,13.3000000004374));
#48050=CARTESIAN_POINT('Origin',(0.,70.2,13.3));
#48051=CARTESIAN_POINT('',(-2.5,31.5805533683886,13.3));
#48052=CARTESIAN_POINT('',(-2.5,32.7902304403868,13.2999999999969));
#48053=CARTESIAN_POINT('',(-2.5,70.2,13.3));
#48054=CARTESIAN_POINT('',(-2.49999995188264,32.7902949052944,13.2995095035349));
#48055=CARTESIAN_POINT('Ctrl Pts',(-2.5,32.7902304403868,13.2999999999938));
#48056=CARTESIAN_POINT('Ctrl Pts',(-2.5,32.7902519286456,13.2998365014727));
#48057=CARTESIAN_POINT('Ctrl Pts',(-2.49999998396094,32.790273416948,13.2996730026523));
#48058=CARTESIAN_POINT('Ctrl Pts',(-2.49999995188264,32.7902949052944,13.2995095035349));
#48059=CARTESIAN_POINT('Ctrl Pts',(-2.49999995188264,32.7902949052944,13.2995095035349));
#48060=CARTESIAN_POINT('Ctrl Pts',(-2.49995240028355,32.8221483810988,13.0571448711518));
#48061=CARTESIAN_POINT('Ctrl Pts',(-2.46465984246264,32.8540041982013,12.816068610491));
#48062=CARTESIAN_POINT('Ctrl Pts',(-2.32238072864385,32.9193046319804,12.3401911228632));
#48063=CARTESIAN_POINT('Ctrl Pts',(-2.21276418048508,32.9521513730157,12.1090455123802));
#48064=CARTESIAN_POINT('Ctrl Pts',(-1.98020768498113,33.006334104292,11.7655545297637));
#48065=CARTESIAN_POINT('Ctrl Pts',(-1.87766845540534,33.0272937485804,11.6416550501174));
#48066=CARTESIAN_POINT('Ctrl Pts',(-1.52704079262838,33.0917878030711,11.2925311818988));
#48067=CARTESIAN_POINT('Ctrl Pts',(-1.24517172042504,33.1344194555062,11.1065199284851));
#48068=CARTESIAN_POINT('Ctrl Pts',(-0.630070992392071,33.2202889134947,
10.8584509285913));
#48069=CARTESIAN_POINT('Ctrl Pts',(-0.303762911995021,33.2620942606438,
10.7968205077297));
#48070=CARTESIAN_POINT('Ctrl Pts',(0.187332606069724,33.3251398722849,10.8017566523966));
#48071=CARTESIAN_POINT('Ctrl Pts',(0.348996910087456,33.3459397449376,10.8191703724959));
#48072=CARTESIAN_POINT('Ctrl Pts',(0.664335829411573,33.387218306528,10.8845900060884));
#48073=CARTESIAN_POINT('Ctrl Pts',(0.81737129877269,33.4075566807512,10.9319932162142));
#48074=CARTESIAN_POINT('Ctrl Pts',(1.25742166181102,33.4683358412982,11.1160863738191));
#48075=CARTESIAN_POINT('Ctrl Pts',(1.52406886358301,33.5084599627421,11.2930584250303));
#48076=CARTESIAN_POINT('Ctrl Pts',(1.87026155311123,33.5700005219807,11.6325905227454));
#48077=CARTESIAN_POINT('Ctrl Pts',(1.97788978347042,33.5911737889312,11.7617909008723));
#48078=CARTESIAN_POINT('Ctrl Pts',(2.16206369501838,33.6328179738398,12.0344926036629));
#48079=CARTESIAN_POINT('Ctrl Pts',(2.23920647585614,33.6531855465169,12.1766193944784));
#48080=CARTESIAN_POINT('Ctrl Pts',(2.43239537442833,33.7157885259535,12.6328533288876));
#48081=CARTESIAN_POINT('Ctrl Pts',(2.49969166971146,33.7573544465519,12.9635536918305));
#48082=CARTESIAN_POINT('Ctrl Pts',(2.50014741199627,33.8195433266639,13.4591576360897));
#48083=CARTESIAN_POINT('Ctrl Pts',(2.48465459633391,33.8397376209209,13.6202531452103));
#48084=CARTESIAN_POINT('Ctrl Pts',(2.42211976875742,33.8805988150891,13.9407768108108));
#48085=CARTESIAN_POINT('Ctrl Pts',(2.37452790699005,33.9011689958892,14.0992990967107));
#48086=CARTESIAN_POINT('Ctrl Pts',(2.19228714425991,33.9608547969121,14.5418310691081));
#48087=CARTESIAN_POINT('Ctrl Pts',(2.01945451037192,33.9995052285358,14.8066797884993));
#48088=CARTESIAN_POINT('Ctrl Pts',(1.58391383992079,34.0775164844838,15.2596927499158));
#48089=CARTESIAN_POINT('Ctrl Pts',(1.32469161326571,34.1161183192664,15.4434535509518));
#48090=CARTESIAN_POINT('Ctrl Pts',(0.899137327357358,34.1737421130743,15.6377148221355));
#48091=CARTESIAN_POINT('Ctrl Pts',(0.754576004154566,34.1924985381063,15.6882993059959));
#48092=CARTESIAN_POINT('Ctrl Pts',(0.282164411263705,34.2524777834034,15.8063949038974));
#48093=CARTESIAN_POINT('Ctrl Pts',(-0.0549778219401599,34.2933479375769,
15.8216347394788));
#48094=CARTESIAN_POINT('Ctrl Pts',(-0.691583271603203,34.3719565762885,
15.722374142115));
#48095=CARTESIAN_POINT('Ctrl Pts',(-0.986475161246398,34.4091519823723,
15.617986030409));
#48096=CARTESIAN_POINT('Ctrl Pts',(-1.39323446843087,34.4663353644852,15.3819557310794));
#48097=CARTESIAN_POINT('Ctrl Pts',(-1.52370245446907,34.4857341309826,15.2884612938777));
#48098=CARTESIAN_POINT('Ctrl Pts',(-1.87205302472696,34.5415566079259,14.9842837313462));
#48099=CARTESIAN_POINT('Ctrl Pts',(-2.06183036897234,34.5772281284375,14.7457728306188));
#48100=CARTESIAN_POINT('Ctrl Pts',(-2.30778850546009,34.6397836339721,14.2859659798799));
#48101=CARTESIAN_POINT('Ctrl Pts',(-2.38529276680687,34.6662730588992,14.0799959682308));
#48102=CARTESIAN_POINT('Ctrl Pts',(-2.47816977164688,34.7154661110473,13.6808400840174));
#48103=CARTESIAN_POINT('Ctrl Pts',(-2.49999999999718,34.7380489073261,13.490747126747));
#48104=CARTESIAN_POINT('Ctrl Pts',(-2.5,34.7604761263292,13.3000000000369));
#48105=CARTESIAN_POINT('Ctrl Pts',(-2.5,33.7644650054088,13.3000000004374));
#48106=CARTESIAN_POINT('Ctrl Pts',(-2.4999999999464,33.7153957113629,13.6063638855109));
#48107=CARTESIAN_POINT('Ctrl Pts',(-2.44368938266213,33.6656454075914,13.910106766958));
#48108=CARTESIAN_POINT('Ctrl Pts',(-2.21520576547411,33.564932618596,14.5051916857309));
#48109=CARTESIAN_POINT('Ctrl Pts',(-2.03631438537295,33.5165219282223,14.7876816829902));
#48110=CARTESIAN_POINT('Ctrl Pts',(-1.69586182941511,33.4416766566087,15.1439416871495));
#48111=CARTESIAN_POINT('Ctrl Pts',(-1.57326960941569,33.4170237337179,15.2495862741076));
#48112=CARTESIAN_POINT('Ctrl Pts',(-1.17765250647787,33.3433430490473,15.5287443851009));
#48113=CARTESIAN_POINT('Ctrl Pts',(-0.880372849210694,33.296682342617,15.6620372307967));
#48114=CARTESIAN_POINT('Ctrl Pts',(-0.279274251402382,33.2058518380004,
15.8017106718201));
#48115=CARTESIAN_POINT('Ctrl Pts',(0.0168121393118554,33.1620765047058,
15.8171997900144));
#48116=CARTESIAN_POINT('Ctrl Pts',(0.641313157754923,33.0712966323003,15.7394663225526));
#48117=CARTESIAN_POINT('Ctrl Pts',(0.962123178563746,33.0266430018552,15.6316683128468));
#48118=CARTESIAN_POINT('Ctrl Pts',(1.53954873039134,32.932613714711,15.2974942144722));
#48119=CARTESIAN_POINT('Ctrl Pts',(1.79078766198862,32.8842420694693,15.0756968961085));
#48120=CARTESIAN_POINT('Ctrl Pts',(2.15514357154332,32.7969098596996,14.5956735449823));
#48121=CARTESIAN_POINT('Ctrl Pts',(2.28282776823589,32.759670062764,14.354628345475));
#48122=CARTESIAN_POINT('Ctrl Pts',(2.4729474163009,32.6784787274333,13.7898674555445));
#48123=CARTESIAN_POINT('Ctrl Pts',(2.51557744964497,32.6342540481868,13.4649562364397));
#48124=CARTESIAN_POINT('Ctrl Pts',(2.47995562827711,32.5556969889572,12.9058187599586));
#48125=CARTESIAN_POINT('Ctrl Pts',(2.43177343336691,32.5225404605207,12.6738279384654));
#48126=CARTESIAN_POINT('Ctrl Pts',(2.23800089721952,32.4448361464276,12.1364434811551));
#48127=CARTESIAN_POINT('Ctrl Pts',(2.06184068356837,32.402177883595,11.8469117299882));
#48128=CARTESIAN_POINT('Ctrl Pts',(1.73529844227031,32.3388144619718,11.4945361283964));
#48129=CARTESIAN_POINT('Ctrl Pts',(1.62786594145866,32.3196130685598,11.3971066779723));
#48130=CARTESIAN_POINT('Ctrl Pts',(1.31029737764301,32.2662806417064,11.1557759168687));
#48131=CARTESIAN_POINT('Ctrl Pts',(1.08569358158453,32.2320848347257,11.0337551651984));
#48132=CARTESIAN_POINT('Ctrl Pts',(0.531515737620487,32.1542676034036,10.8343171576283));
#48133=CARTESIAN_POINT('Ctrl Pts',(0.196842924385133,32.1120083433719,10.7853584650124));
#48134=CARTESIAN_POINT('Ctrl Pts',(-0.461181655561167,32.0264406794179,
10.821622218201));
#48135=CARTESIAN_POINT('Ctrl Pts',(-0.778228279605227,31.9840742082586,
10.9022175787181));
#48136=CARTESIAN_POINT('Ctrl Pts',(-1.32925164818711,31.9039851167018,11.1634697123731));
#48137=CARTESIAN_POINT('Ctrl Pts',(-1.56462668003421,31.8673414757141,11.3292957303027));
#48138=CARTESIAN_POINT('Ctrl Pts',(-2.00164294062796,31.7881785799826,11.7658744169739));
#48139=CARTESIAN_POINT('Ctrl Pts',(-2.18738722022867,31.7462406606404,12.0448226268867));
#48140=CARTESIAN_POINT('Ctrl Pts',(-2.39981857799535,31.6748115287023,12.5631252680941));
#48141=CARTESIAN_POINT('Ctrl Pts',(-2.45706011617239,31.6458531802989,12.7852356558965));
#48142=CARTESIAN_POINT('Ctrl Pts',(-2.49446628917762,31.6047725711507,13.1078128589546));
#48143=CARTESIAN_POINT('Ctrl Pts',(-2.5,31.592645110597,13.2039632545006));
#48144=CARTESIAN_POINT('Ctrl Pts',(-2.5,31.5805533683886,13.3));
#48145=CARTESIAN_POINT('Origin',(0.,70.2,13.3));
#48146=CARTESIAN_POINT('',(-2.5,29.7319333905705,13.3000000001788));
#48147=CARTESIAN_POINT('',(-2.5,30.448807333626,13.3000000006354));
#48148=CARTESIAN_POINT('',(-2.5,70.2,13.3));
#48149=CARTESIAN_POINT('',(-2.41619328710391,30.5123559175791,12.6571443227054));
#48150=CARTESIAN_POINT('Ctrl Pts',(-2.5,30.448807333626,13.3000000012709));
#48151=CARTESIAN_POINT('Ctrl Pts',(-2.50000000000077,30.4489575841864,13.2984814139764));
#48152=CARTESIAN_POINT('Ctrl Pts',(-2.49999861633713,30.44910781596,13.296962776412));
#48153=CARTESIAN_POINT('Ctrl Pts',(-2.49960317435266,30.4705706394413,13.0799691528022));
#48154=CARTESIAN_POINT('Ctrl Pts',(-2.47135580135003,30.4912362366712,12.8654425703387));
#48155=CARTESIAN_POINT('Ctrl Pts',(-2.41594587876447,30.5121662090965,12.6571893662353));
#48156=CARTESIAN_POINT('Ctrl Pts',(-2.41596675694296,30.5129552114539,12.6572678401181));
#48157=CARTESIAN_POINT('Ctrl Pts',(-2.35883570065213,30.5579490103612,12.4425178378573));
#48158=CARTESIAN_POINT('Ctrl Pts',(-2.27321578263186,30.6017824679034,12.2360288065908));
#48159=CARTESIAN_POINT('Ctrl Pts',(-2.03034648356656,30.6959711890914,11.8182291397699));
#48160=CARTESIAN_POINT('Ctrl Pts',(-1.8649380824931,30.7435817971013,11.6147117438818));
#48161=CARTESIAN_POINT('Ctrl Pts',(-1.45539675357328,30.8428791817054,11.2468160020568));
#48162=CARTESIAN_POINT('Ctrl Pts',(-1.20787754103791,30.8949023392902,11.0920196522197));
#48163=CARTESIAN_POINT('Ctrl Pts',(-0.788006455920246,30.9719008770198,
10.9218486067175));
#48164=CARTESIAN_POINT('Ctrl Pts',(-0.63129322644735,30.9989402025191,10.8755278268355));
#48165=CARTESIAN_POINT('Ctrl Pts',(-0.178217409132333,31.0759719317503,
10.7885867984338));
#48166=CARTESIAN_POINT('Ctrl Pts',(0.12259188344298,31.1253819066478,10.7852127441113));
#48167=CARTESIAN_POINT('Ctrl Pts',(0.723397487068334,31.2229670801232,10.8868619627879));
#48168=CARTESIAN_POINT('Ctrl Pts',(1.0174897166744,31.2727323769274,10.9953785562771));
#48169=CARTESIAN_POINT('Ctrl Pts',(1.56565074144212,31.3730652390623,11.3235365952355));
#48170=CARTESIAN_POINT('Ctrl Pts',(1.81140516656008,31.4219926386856,11.5459640358851));
#48171=CARTESIAN_POINT('Ctrl Pts',(2.19957391636242,31.521484104347,12.0687255044085));
#48172=CARTESIAN_POINT('Ctrl Pts',(2.34002909556593,31.5686955342603,12.3627017477311));
#48173=CARTESIAN_POINT('Ctrl Pts',(2.4602863448112,31.6402516341769,12.8287423804406));
#48174=CARTESIAN_POINT('Ctrl Pts',(2.4851996441707,31.663869639399,12.9855466181158));
#48175=CARTESIAN_POINT('Ctrl Pts',(2.50484045220785,31.7101713974724,13.2990052299316));
#48176=CARTESIAN_POINT('Ctrl Pts',(2.50004895457153,31.7325424902078,13.454913080661));
#48177=CARTESIAN_POINT('Ctrl Pts',(2.44110198011629,31.8009338979227,13.9275255961028));
#48178=CARTESIAN_POINT('Ctrl Pts',(2.3405993722713,31.8470542945225,14.2350953317938));
#48179=CARTESIAN_POINT('Ctrl Pts',(2.10419900918666,31.9162678744218,14.6600701426085));
#48180=CARTESIAN_POINT('Ctrl Pts',(2.00947244171977,31.9396073417861,14.7964860932594));
#48181=CARTESIAN_POINT('Ctrl Pts',(1.80342469173612,31.984661762764,15.0380166791454));
#48182=CARTESIAN_POINT('Ctrl Pts',(1.69458950358715,32.0062405195487,15.1442917715027));
#48183=CARTESIAN_POINT('Ctrl Pts',(1.31558573532985,32.0751809920567,15.4523304182481));
#48184=CARTESIAN_POINT('Ctrl Pts',(1.01421234932664,32.1199351068297,15.6097030337364));
#48185=CARTESIAN_POINT('Ctrl Pts',(0.391317781425657,32.2092432847418,15.7887469780546));
#48186=CARTESIAN_POINT('Ctrl Pts',(0.0785247633640879,32.252953579236,15.8181103920361));
#48187=CARTESIAN_POINT('Ctrl Pts',(-0.546924064232225,32.3381654307809,
15.7599040893123));
#48188=CARTESIAN_POINT('Ctrl Pts',(-0.853786134377966,32.3796765152074,
15.670938715195));
#48189=CARTESIAN_POINT('Ctrl Pts',(-1.27216140957349,32.4435156246173,15.457544710545));
#48190=CARTESIAN_POINT('Ctrl Pts',(-1.40174397850272,32.4644165128666,15.3756941824833));
#48191=CARTESIAN_POINT('Ctrl Pts',(-1.79011033114316,32.5309848591934,15.0773391212701));
#48192=CARTESIAN_POINT('Ctrl Pts',(-2.01300226423329,32.5745482626543,14.8202983121113));
#48193=CARTESIAN_POINT('Ctrl Pts',(-2.27863241584907,32.6466534912303,14.3486333228143));
#48194=CARTESIAN_POINT('Ctrl Pts',(-2.35671875589441,32.674078384212,14.158872179394));
#48195=CARTESIAN_POINT('Ctrl Pts',(-2.43854709728563,32.7155475527714,13.8607628203475));
#48196=CARTESIAN_POINT('Ctrl Pts',(-2.45989829234932,32.7295296661982,13.7581195672206));
#48197=CARTESIAN_POINT('Ctrl Pts',(-2.49156059793428,32.7590875296406,13.5370395037512));
#48198=CARTESIAN_POINT('Ctrl Pts',(-2.50000000000029,32.7746433674768,13.4185979467541));
#48199=CARTESIAN_POINT('Ctrl Pts',(-2.5,32.7902304403868,13.2999999999938));
#48200=CARTESIAN_POINT('',(-2.44274579319255,29.8383352895022,12.7680192277667));
#48201=CARTESIAN_POINT('Ctrl Pts',(-2.5,31.5805533683886,13.3));
#48202=CARTESIAN_POINT('Ctrl Pts',(-2.5,31.5506182064355,13.5377552779758));
#48203=CARTESIAN_POINT('Ctrl Pts',(-2.46608138989822,31.5208908684004,13.7748126054976));
#48204=CARTESIAN_POINT('Ctrl Pts',(-2.3224560244815,31.4570145149412,14.2642743785868));
#48205=CARTESIAN_POINT('Ctrl Pts',(-2.20417068662367,31.4233278057136,14.5104835825318));
#48206=CARTESIAN_POINT('Ctrl Pts',(-1.96504908934518,31.3713635771709,14.8523702419768));
#48207=CARTESIAN_POINT('Ctrl Pts',(-1.87115731336049,31.3532641804217,14.9643449271175));
#48208=CARTESIAN_POINT('Ctrl Pts',(-1.53143566875036,31.2936439297573,15.3041707551186));
#48209=CARTESIAN_POINT('Ctrl Pts',(-1.24967697024499,31.2527810574749,15.4909700005104));
#48210=CARTESIAN_POINT('Ctrl Pts',(-0.791686143764384,31.1923366036486,
15.6766929896363));
#48211=CARTESIAN_POINT('Ctrl Pts',(-0.638487345656817,31.1729425655691,
15.7223486650582));
#48212=CARTESIAN_POINT('Ctrl Pts',(-0.153681305777879,31.1127336090979,
15.8176030120288));
#48213=CARTESIAN_POINT('Ctrl Pts',(0.18427798926919,31.0722886438412,15.8155551435562));
#48214=CARTESIAN_POINT('Ctrl Pts',(0.82724309823683,30.9930546284602,15.6810741364213));
#48215=CARTESIAN_POINT('Ctrl Pts',(1.12696643462638,30.9549073499603,15.5547293621554));
#48216=CARTESIAN_POINT('Ctrl Pts',(1.52834837377316,30.8968574597102,15.284988228244));
#48217=CARTESIAN_POINT('Ctrl Pts',(1.65323449378781,30.8775727856828,15.1822459501393));
#48218=CARTESIAN_POINT('Ctrl Pts',(1.97721053338203,30.8231076043594,14.8584214110551));
#48219=CARTESIAN_POINT('Ctrl Pts',(2.14807252545898,30.7887054516615,14.612955152419));
#48220=CARTESIAN_POINT('Ctrl Pts',(2.41157262967143,30.7146758787045,14.0391347690649));
#48221=CARTESIAN_POINT('Ctrl Pts',(2.4887639286759,30.6754036010154,13.7100013568907));
#48222=CARTESIAN_POINT('Ctrl Pts',(2.50847350276491,30.5998361580507,13.0569670529847));
#48223=CARTESIAN_POINT('Ctrl Pts',(2.45712207088327,30.5639610449962,12.7395873638693));
#48224=CARTESIAN_POINT('Ctrl Pts',(2.29226579615131,30.5086627346294,12.2893613178293));
#48225=CARTESIAN_POINT('Ctrl Pts',(2.22250570281706,30.4901721477675,12.1439936308391));
#48226=CARTESIAN_POINT('Ctrl Pts',(1.98595694320881,30.4381312283265,11.7528292756899));
#48227=CARTESIAN_POINT('Ctrl Pts',(1.78880799060941,30.4055961401458,11.5285710061412));
#48228=CARTESIAN_POINT('Ctrl Pts',(1.29567724061902,30.335366437808,11.1360292397398));
#48229=CARTESIAN_POINT('Ctrl Pts',(0.995280930003226,30.2977913317661,10.9824515185561));
#48230=CARTESIAN_POINT('Ctrl Pts',(0.369242818520919,30.2268328407032,10.8073091330423));
#48231=CARTESIAN_POINT('Ctrl Pts',(0.0515386662844847,30.1936491795691,
10.780635095682));
#48232=CARTESIAN_POINT('Ctrl Pts',(-0.422449236165706,30.1417762105348,
10.8307212083397));
#48233=CARTESIAN_POINT('Ctrl Pts',(-0.580209343291639,30.1243368263708,
10.8629585586074));
#48234=CARTESIAN_POINT('Ctrl Pts',(-1.01411771751827,30.0758692849208,10.9961875778601));
#48235=CARTESIAN_POINT('Ctrl Pts',(-1.27712883285776,30.0461467858501,11.1309054093261));
#48236=CARTESIAN_POINT('Ctrl Pts',(-1.76443951752628,29.9832950364743,11.5005321456237));
#48237=CARTESIAN_POINT('Ctrl Pts',(-1.97903053815114,29.9498157858136,11.7396043951434));
#48238=CARTESIAN_POINT('Ctrl Pts',(-2.28346040715123,29.8906119947612,12.2463451969034));
#48239=CARTESIAN_POINT('Ctrl Pts',(-2.38470555547828,29.8648554638372,12.5015201389497));
#48240=CARTESIAN_POINT('Ctrl Pts',(-2.44274382522039,29.8383396165347,12.7680201090758));
#48241=CARTESIAN_POINT('Ctrl Pts',(-2.44274339219816,29.8383270426146,12.7680181207295));
#48242=CARTESIAN_POINT('Ctrl Pts',(-2.48077087610663,29.8022369430543,12.9426319349569));
#48243=CARTESIAN_POINT('Ctrl Pts',(-2.5000000000256,29.7670454411236,13.1210333618124));
#48244=CARTESIAN_POINT('Ctrl Pts',(-2.5,29.7319333905705,13.3000000003577));
#48245=CARTESIAN_POINT('Origin',(0.,70.2,13.3));
#48246=CARTESIAN_POINT('',(-2.5,27.4053098230045,13.3));
#48247=CARTESIAN_POINT('',(-2.5,28.6199701874195,13.3));
#48248=CARTESIAN_POINT('',(-2.5,70.2,13.3));
#48249=CARTESIAN_POINT('Ctrl Pts',(-2.5,28.6199701874195,13.3));
#48250=CARTESIAN_POINT('Ctrl Pts',(-2.5,28.6327850846717,13.1995694455431));
#48251=CARTESIAN_POINT('Ctrl Pts',(-2.49394822593413,28.6455754439869,13.099168590211));
#48252=CARTESIAN_POINT('Ctrl Pts',(-2.44160871681871,28.7009645375733,12.667115103329));
#48253=CARTESIAN_POINT('Ctrl Pts',(-2.33505473222711,28.74301621687,12.3462931500924));
#48254=CARTESIAN_POINT('Ctrl Pts',(-2.0887767410183,28.8052671422129,11.9170053410973));
#48255=CARTESIAN_POINT('Ctrl Pts',(-1.99588660153722,28.8253117141221,11.7860308127951));
#48256=CARTESIAN_POINT('Ctrl Pts',(-1.69523827910462,28.8828718345511,11.4383228954246));
#48257=CARTESIAN_POINT('Ctrl Pts',(-1.46025075558902,28.9199670416504,11.248815829488));
#48258=CARTESIAN_POINT('Ctrl Pts',(-0.903055295997165,28.9990247628022,
10.9448178848108));
#48259=CARTESIAN_POINT('Ctrl Pts',(-0.579421184943894,29.0402572049479,
10.8450663466309));
#48260=CARTESIAN_POINT('Ctrl Pts',(0.0606219893681992,29.1194799559106,
10.7818460006969));
#48261=CARTESIAN_POINT('Ctrl Pts',(0.369979936040267,29.1567920006692,10.8084305372208));
#48262=CARTESIAN_POINT('Ctrl Pts',(0.822222547126219,29.2139591251509,10.9335724612474));
#48263=CARTESIAN_POINT('Ctrl Pts',(0.97319420288676,29.2335108787594,10.9915528541699));
#48264=CARTESIAN_POINT('Ctrl Pts',(1.39774412380091,29.2908761978435,11.2037082359193));
#48265=CARTESIAN_POINT('Ctrl Pts',(1.64916020085886,29.3279518382367,11.3951634380007));
#48266=CARTESIAN_POINT('Ctrl Pts',(2.08210185327466,29.4059694258053,11.8764558751));
#48267=CARTESIAN_POINT('Ctrl Pts',(2.2535003910037,29.4467100927564,12.1671386423894));
#48268=CARTESIAN_POINT('Ctrl Pts',(2.4334189338219,29.5127017915693,12.6873944491853));
#48269=CARTESIAN_POINT('Ctrl Pts',(2.47730682558507,29.5380696035329,12.9002386381054));
#48270=CARTESIAN_POINT('Ctrl Pts',(2.51603813060199,29.5989771498109,13.4253962642545));
#48271=CARTESIAN_POINT('Ctrl Pts',(2.48110270569015,29.633552990786,13.7361971275792));
#48272=CARTESIAN_POINT('Ctrl Pts',(2.29169115542339,29.7088734894859,14.3541469058951));
#48273=CARTESIAN_POINT('Ctrl Pts',(2.12930782728746,29.7498210900781,14.6524344251759));
#48274=CARTESIAN_POINT('Ctrl Pts',(1.70138660914546,29.8279664515823,15.1609502155387));
#48275=CARTESIAN_POINT('Ctrl Pts',(1.44241546598459,29.8642537873569,15.3682085169965));
#48276=CARTESIAN_POINT('Ctrl Pts',(0.883153410916181,29.9325135829285,15.6581312915006));
#48277=CARTESIAN_POINT('Ctrl Pts',(0.593026387910101,29.9646864238788,15.7472409506213));
#48278=CARTESIAN_POINT('Ctrl Pts',(0.00496183693252068,30.0335247045431,
15.8168814390696));
#48279=CARTESIAN_POINT('Ctrl Pts',(-0.287967281520161,30.0680860885775,
15.8003800463128));
#48280=CARTESIAN_POINT('Ctrl Pts',(-0.79284965984856,30.1264004927931,15.6818239179714));
#48281=CARTESIAN_POINT('Ctrl Pts',(-1.00616018060319,30.1506349362041,15.5998780356437));
#48282=CARTESIAN_POINT('Ctrl Pts',(-1.48968121580609,30.2073677980581,15.3337274573262));
#48283=CARTESIAN_POINT('Ctrl Pts',(-1.74062594994233,30.2388038452988,15.1235751313124));
#48284=CARTESIAN_POINT('Ctrl Pts',(-2.15310079120443,30.3081217889657,14.6131348029968));
#48285=CARTESIAN_POINT('Ctrl Pts',(-2.30830094586534,30.3432598643754,14.3158862160448));
#48286=CARTESIAN_POINT('Ctrl Pts',(-2.46661710644016,30.4015756208221,13.770528762688));
#48287=CARTESIAN_POINT('Ctrl Pts',(-2.49999999988009,30.4254695360297,13.5358758796161));
#48288=CARTESIAN_POINT('Ctrl Pts',(-2.5,30.448807333626,13.3000000012709));
#48289=CARTESIAN_POINT('Ctrl Pts',(-2.5,29.7319333905705,13.3000000003576));
#48290=CARTESIAN_POINT('Ctrl Pts',(-2.49999999999996,29.7318724014283,13.3003108629132));
#48291=CARTESIAN_POINT('Ctrl Pts',(-2.49999994201859,29.7318114131336,13.3006217272935));
#48292=CARTESIAN_POINT('Ctrl Pts',(-2.49992634709586,29.6931068287105,13.4979073586275));
#48293=CARTESIAN_POINT('Ctrl Pts',(-2.47657528164387,29.6551154971477,13.6944516803843));
#48294=CARTESIAN_POINT('Ctrl Pts',(-2.35749764558954,29.5612157236652,14.1878924096993));
#48295=CARTESIAN_POINT('Ctrl Pts',(-2.22913470602397,29.505152474325,14.4736075773388));
#48296=CARTESIAN_POINT('Ctrl Pts',(-1.87105042885647,29.3939564136642,14.9879505733476));
#48297=CARTESIAN_POINT('Ctrl Pts',(-1.64281712267107,29.342397653508,15.2108512677702));
#48298=CARTESIAN_POINT('Ctrl Pts',(-1.1269215969022,29.2390225684145,15.5519316550608));
#48299=CARTESIAN_POINT('Ctrl Pts',(-0.846842233456649,29.1899952735646,
15.6715463120526));
#48300=CARTESIAN_POINT('Ctrl Pts',(-0.263669061310278,29.0946429065696,
15.8035750830613));
#48301=CARTESIAN_POINT('Ctrl Pts',(0.0341682228858632,29.0479609796295,
15.8172273448508));
#48302=CARTESIAN_POINT('Ctrl Pts',(0.491552894477325,28.9772728325731,15.7567720659131));
#48303=CARTESIAN_POINT('Ctrl Pts',(0.652981496791188,28.9523472598469,15.7188807557228));
#48304=CARTESIAN_POINT('Ctrl Pts',(1.09540754359596,28.8812282410761,15.5674649124578));
#48305=CARTESIAN_POINT('Ctrl Pts',(1.36130807796902,28.8353943496751,15.4185541470391));
#48306=CARTESIAN_POINT('Ctrl Pts',(1.83478909242976,28.7442973576672,15.0265806192441));
#48307=CARTESIAN_POINT('Ctrl Pts',(2.0359310493986,28.6978925545718,14.7840879845139));
#48308=CARTESIAN_POINT('Ctrl Pts',(2.34830557372873,28.6033966060118,14.2198427337845));
#48309=CARTESIAN_POINT('Ctrl Pts',(2.44977186980247,28.5566680886389,13.8994781141711));
#48310=CARTESIAN_POINT('Ctrl Pts',(2.52090137313357,28.4614182876343,13.2412808606137));
#48311=CARTESIAN_POINT('Ctrl Pts',(2.4912780919575,28.4158350410216,12.9101392951487));
#48312=CARTESIAN_POINT('Ctrl Pts',(2.35311566499084,28.3467208032282,12.4406601037354));
#48313=CARTESIAN_POINT('Ctrl Pts',(2.2932870118741,28.3240422256198,12.2918060807117));
#48314=CARTESIAN_POINT('Ctrl Pts',(2.06784326620615,28.2551238723809,11.8567887198095));
#48315=CARTESIAN_POINT('Ctrl Pts',(1.85954218222959,28.2102858168898,11.5967688571649));
#48316=CARTESIAN_POINT('Ctrl Pts',(1.35616587493274,28.1193380800673,11.1744937106368));
#48317=CARTESIAN_POINT('Ctrl Pts',(1.06675019950998,28.0754186435454,11.0154737842077));
#48318=CARTESIAN_POINT('Ctrl Pts',(0.60145295222266,28.0088892395113,10.868095770466));
#48319=CARTESIAN_POINT('Ctrl Pts',(0.443683528899947,27.9869020518249,10.8344271189726));
#48320=CARTESIAN_POINT('Ctrl Pts',(-0.0485706254989859,27.9195187716889,
10.7781879926998));
#48321=CARTESIAN_POINT('Ctrl Pts',(-0.385198572893466,27.8754074883351,
10.8073008578459));
#48322=CARTESIAN_POINT('Ctrl Pts',(-1.0166541538013,27.78673226523,10.9932276430615));
#48323=CARTESIAN_POINT('Ctrl Pts',(-1.3065173121412,27.7441862595109,11.1441144621935));
#48324=CARTESIAN_POINT('Ctrl Pts',(-1.80263394475705,27.6598205243732,11.5401044371508));
#48325=CARTESIAN_POINT('Ctrl Pts',(-2.00739589880486,27.6186293346373,11.7777936323127));
#48326=CARTESIAN_POINT('Ctrl Pts',(-2.32165701290964,27.5359838132377,12.3203420891319));
#48327=CARTESIAN_POINT('Ctrl Pts',(-2.42677007441428,27.4946455660611,12.6213064538359));
#48328=CARTESIAN_POINT('Ctrl Pts',(-2.4909986315093,27.4372189377818,13.0551428443414));
#48329=CARTESIAN_POINT('Ctrl Pts',(-2.5,27.4212781500521,13.1775175349232));
#48330=CARTESIAN_POINT('Ctrl Pts',(-2.5,27.4053098230045,13.3));
#48331=CARTESIAN_POINT('Origin',(0.,70.2,13.3));
#48332=CARTESIAN_POINT('',(-2.5,25.4505462844759,13.3));
#48333=CARTESIAN_POINT('',(-2.49999999999832,26.3929871638855,13.3));
#48334=CARTESIAN_POINT('',(-2.5,70.2,13.3));
#48335=CARTESIAN_POINT('',(-2.49999988262115,26.3931137665368,13.2992339097816));
#48336=CARTESIAN_POINT('Ctrl Pts',(-2.49999999999832,26.3929871638855,13.3));
#48337=CARTESIAN_POINT('Ctrl Pts',(-2.49999999999943,26.3930293663056,13.2997446371823));
#48338=CARTESIAN_POINT('Ctrl Pts',(-2.4999999608739,26.3930715671874,13.2994892737731));
#48339=CARTESIAN_POINT('Ctrl Pts',(-2.49999988262115,26.3931137665368,13.2992339097816));
#48340=CARTESIAN_POINT('Ctrl Pts',(-2.49999988262115,26.3931137665368,13.2992339097816));
#48341=CARTESIAN_POINT('Ctrl Pts',(-2.49990861043225,26.4423341093278,13.0013832701664));
#48342=CARTESIAN_POINT('Ctrl Pts',(-2.44659790091214,26.4898005592029,12.7058762675489));
#48343=CARTESIAN_POINT('Ctrl Pts',(-2.23996167708881,26.5875207226236,12.1516598654052));
#48344=CARTESIAN_POINT('Ctrl Pts',(-2.08974477813341,26.6360141905069,11.8966669489459));
#48345=CARTESIAN_POINT('Ctrl Pts',(-1.6917835838025,26.7326629013295,11.4321538623161));
#48346=CARTESIAN_POINT('Ctrl Pts',(-1.44078604149619,26.7819002676501,11.2323362820651));
#48347=CARTESIAN_POINT('Ctrl Pts',(-1.015987975505,26.8558398436871,11.0100557996151));
#48348=CARTESIAN_POINT('Ctrl Pts',(-0.865990378075362,26.8802140053644,
10.9492231009399));
#48349=CARTESIAN_POINT('Ctrl Pts',(-0.418968433668596,26.9508198986062,
10.8165866801885));
#48350=CARTESIAN_POINT('Ctrl Pts',(-0.113339936063998,26.9971554395426,
10.7840304409995));
#48351=CARTESIAN_POINT('Ctrl Pts',(0.351552396105956,27.0663728142287,10.819586160685));
#48352=CARTESIAN_POINT('Ctrl Pts',(0.510927143312623,27.0898813569698,10.8474471574717));
#48353=CARTESIAN_POINT('Ctrl Pts',(0.985496692595052,27.1618019364457,10.978722957087));
#48354=CARTESIAN_POINT('Ctrl Pts',(1.28382526795159,27.2097588689324,11.1294336485431));
#48355=CARTESIAN_POINT('Ctrl Pts',(1.77152336191823,27.2996259194926,11.5124608521681));
#48356=CARTESIAN_POINT('Ctrl Pts',(1.9662366539096,27.3416973668749,11.7291580730582));
#48357=CARTESIAN_POINT('Ctrl Pts',(2.29722266389161,27.4300086449687,12.2583692666568));
#48358=CARTESIAN_POINT('Ctrl Pts',(2.41596305661392,27.4732030838945,12.5751265719609));
#48359=CARTESIAN_POINT('Ctrl Pts',(2.51589625545696,27.5588168204824,13.2014270989334));
#48360=CARTESIAN_POINT('Ctrl Pts',(2.50961776146324,27.6002749760034,13.5026508389486));
#48361=CARTESIAN_POINT('Ctrl Pts',(2.39653289185163,27.6820069025001,14.0619263683701));
#48362=CARTESIAN_POINT('Ctrl Pts',(2.29953697319745,27.7213531424566,14.3179062002621));
#48363=CARTESIAN_POINT('Ctrl Pts',(1.99999732415954,27.8040697449607,14.8349079818321));
#48364=CARTESIAN_POINT('Ctrl Pts',(1.78331977387523,27.8466332134415,15.0821014183643));
#48365=CARTESIAN_POINT('Ctrl Pts',(1.39631904103432,27.9120465077539,15.3800858519101));
#48366=CARTESIAN_POINT('Ctrl Pts',(1.2580409952468,27.9337803836223,15.4665177116332));
#48367=CARTESIAN_POINT('Ctrl Pts',(0.820833682891556,27.9990181836344,15.6837341729523));
#48368=CARTESIAN_POINT('Ctrl Pts',(0.503813621442931,28.042340383823,15.7702504394689));
#48369=CARTESIAN_POINT('Ctrl Pts',(0.0177717747247502,28.1072010320218,
15.8051654697502));
#48370=CARTESIAN_POINT('Ctrl Pts',(-0.144337122208285,28.128478756645,15.8010687342534));
#48371=CARTESIAN_POINT('Ctrl Pts',(-0.620476810429327,28.1916648307116,
15.7425570502418));
#48372=CARTESIAN_POINT('Ctrl Pts',(-0.925775051887367,28.2332994033375,
15.6439372786663));
#48373=CARTESIAN_POINT('Ctrl Pts',(-1.34993803306391,28.2965893237324,15.4107457519792));
#48374=CARTESIAN_POINT('Ctrl Pts',(-1.48714088271485,28.3181478216139,15.3164316668437));
#48375=CARTESIAN_POINT('Ctrl Pts',(-1.73994854041058,28.3612382589392,15.1027168173146));
#48376=CARTESIAN_POINT('Ctrl Pts',(-1.85507293998218,28.3826618023661,14.9840175525638));
#48377=CARTESIAN_POINT('Ctrl Pts',(-2.16547247099176,28.4474831044656,14.5932015067003));
#48378=CARTESIAN_POINT('Ctrl Pts',(-2.31874752319724,28.4900088363419,14.2925147860756));
#48379=CARTESIAN_POINT('Ctrl Pts',(-2.45168825657745,28.5537149303618,13.8150600852883));
#48380=CARTESIAN_POINT('Ctrl Pts',(-2.47982687888544,28.5744064397878,13.6557030345326));
#48381=CARTESIAN_POINT('Ctrl Pts',(-2.49746876000698,28.6033840922305,13.4299158608522));
#48382=CARTESIAN_POINT('Ctrl Pts',(-2.5,28.6116823732052,13.3649517323781));
#48383=CARTESIAN_POINT('Ctrl Pts',(-2.5,28.6199701874195,13.3));
#48384=CARTESIAN_POINT('Ctrl Pts',(-2.5,27.4053098230045,13.3));
#48385=CARTESIAN_POINT('Ctrl Pts',(-2.5,27.3996223211976,13.3436250609951));
#48386=CARTESIAN_POINT('Ctrl Pts',(-2.49885811801832,27.3939321052226,13.3872638958897));
#48387=CARTESIAN_POINT('Ctrl Pts',(-2.48810867827697,27.3671441573085,13.5923251578246));
#48388=CARTESIAN_POINT('Ctrl Pts',(-2.46400345374254,27.3460475310011,13.7525747338723));
#48389=CARTESIAN_POINT('Ctrl Pts',(-2.34310063192789,27.2812148409896,14.2336317514487));
#48390=CARTESIAN_POINT('Ctrl Pts',(-2.19737174054802,27.2384858740639,14.5382961866477));
#48391=CARTESIAN_POINT('Ctrl Pts',(-1.90040500245466,27.1746169454776,14.9320791795483));
#48392=CARTESIAN_POINT('Ctrl Pts',(-1.79291441677868,27.1540661780335,15.0494804302878));
#48393=CARTESIAN_POINT('Ctrl Pts',(-1.42695493726365,27.0904234463954,15.3797729942216));
#48394=CARTESIAN_POINT('Ctrl Pts',(-1.13649652588632,27.048062452115,15.5516773622605));
#48395=CARTESIAN_POINT('Ctrl Pts',(-0.504581222342047,26.962137241801,15.7713369552786));
#48396=CARTESIAN_POINT('Ctrl Pts',(-0.169414111429522,26.9199158989573,
15.816631373289));
#48397=CARTESIAN_POINT('Ctrl Pts',(0.324975605872016,26.8567752480209,15.7839854355352));
#48398=CARTESIAN_POINT('Ctrl Pts',(0.483838868790364,26.8363454752803,15.757985874583));
#48399=CARTESIAN_POINT('Ctrl Pts',(0.797157813576045,26.7951411273092,15.6751348315224));
#48400=CARTESIAN_POINT('Ctrl Pts',(0.950731445552928,26.7744856242565,15.6179385623772));
#48401=CARTESIAN_POINT('Ctrl Pts',(1.37226598561706,26.7150874730926,15.4119486729574));
#48402=CARTESIAN_POINT('Ctrl Pts',(1.61999029041852,26.6766916919098,15.2284933504146));
#48403=CARTESIAN_POINT('Ctrl Pts',(1.94066653337549,26.6174474021038,14.8845758973231));
#48404=CARTESIAN_POINT('Ctrl Pts',(2.04071530886955,26.59681630124,14.753461742974));
#48405=CARTESIAN_POINT('Ctrl Pts',(2.20962028042095,26.556438896401,14.4799210111295));
#48406=CARTESIAN_POINT('Ctrl Pts',(2.27932506639292,26.5367862509454,14.3389005299839));
#48407=CARTESIAN_POINT('Ctrl Pts',(2.45445007565042,26.4752981207319,13.8805474580364));
#48408=CARTESIAN_POINT('Ctrl Pts',(2.50994679852911,26.4340547773478,13.5480890627087));
#48409=CARTESIAN_POINT('Ctrl Pts',(2.49323279542962,26.373164809232,13.0593982211623));
#48410=CARTESIAN_POINT('Ctrl Pts',(2.47348700883369,26.3538962325488,12.9050796679274));
#48411=CARTESIAN_POINT('Ctrl Pts',(2.37643390160687,26.2986820783243,12.4717657912131));
#48412=CARTESIAN_POINT('Ctrl Pts',(2.26494625460606,26.2630987162367,12.2029826667315));
#48413=CARTESIAN_POINT('Ctrl Pts',(1.94239856320779,26.1888780297846,11.6953858638462));
#48414=CARTESIAN_POINT('Ctrl Pts',(1.72676095872817,26.1508557958496,11.4653333277888));
#48415=CARTESIAN_POINT('Ctrl Pts',(1.34324621327224,26.0923901785833,11.1852820823339));
#48416=CARTESIAN_POINT('Ctrl Pts',(1.20315502230001,26.0724675564974,11.1025550276125));
#48417=CARTESIAN_POINT('Ctrl Pts',(0.793578013645412,26.0171259806383,10.9116792885689));
#48418=CARTESIAN_POINT('Ctrl Pts',(0.511845809783451,25.9822894612031,10.8358824036639));
#48419=CARTESIAN_POINT('Ctrl Pts',(-0.11131845983581,25.9063581622406,10.7799688051623));
#48420=CARTESIAN_POINT('Ctrl Pts',(-0.448711406021424,25.8656000665261,
10.8177372412971));
#48421=CARTESIAN_POINT('Ctrl Pts',(-1.0651316616425,25.7874832580424,11.0168796619845));
#48422=CARTESIAN_POINT('Ctrl Pts',(-1.34119636797327,25.7507366285312,11.1673172008032));
#48423=CARTESIAN_POINT('Ctrl Pts',(-1.8118219336404,25.6773856466678,11.5521269243203));
#48424=CARTESIAN_POINT('Ctrl Pts',(-2.00605564565092,25.6418943480628,11.7789606147578));
#48425=CARTESIAN_POINT('Ctrl Pts',(-2.31304622677275,25.5703443722778,12.3020020390374));
#48426=CARTESIAN_POINT('Ctrl Pts',(-2.41889024678534,25.5349304284088,12.5963374116816));
#48427=CARTESIAN_POINT('Ctrl Pts',(-2.48939769060973,25.4823025486937,13.0341472013468));
#48428=CARTESIAN_POINT('Ctrl Pts',(-2.5,25.4663859015973,13.1670681074021));
#48429=CARTESIAN_POINT('Ctrl Pts',(-2.5,25.4505462844759,13.3));
#48430=CARTESIAN_POINT('Origin',(0.,70.2,13.3));
#48431=CARTESIAN_POINT('',(-2.5,20.4,13.3));
#48432=CARTESIAN_POINT('Origin',(0.,20.4,13.3));
#48433=CARTESIAN_POINT('',(-2.5,22.6116296396575,13.3));
#48434=CARTESIAN_POINT('',(-2.5,70.2,13.3));
#48435=CARTESIAN_POINT('',(-1.80813900541952,24.1372606373433,15.0222732043098));
#48436=CARTESIAN_POINT('Ctrl Pts',(-1.81028567158556,24.1386394120584,15.0242000427015));
#48437=CARTESIAN_POINT('Ctrl Pts',(-1.62817173955969,24.114723319155,15.2154065347429));
#48438=CARTESIAN_POINT('Ctrl Pts',(-1.41694756494607,24.0913164310824,15.3765297752926));
#48439=CARTESIAN_POINT('Ctrl Pts',(-0.924156731153752,24.0383425219184,
15.6416398587418));
#48440=CARTESIAN_POINT('Ctrl Pts',(-0.641172790021728,24.0088848798015,
15.7343752869735));
#48441=CARTESIAN_POINT('Ctrl Pts',(-0.191166389328545,23.964562234863,15.797746599409));
#48442=CARTESIAN_POINT('Ctrl Pts',(-0.0319733094634541,23.9491491640395,
15.804846138491));
#48443=CARTESIAN_POINT('Ctrl Pts',(0.455698514788413,23.9006726261604,15.7800780211352));
#48444=CARTESIAN_POINT('Ctrl Pts',(0.777988740413514,23.8663730008719,15.6985549214629));
#48445=CARTESIAN_POINT('Ctrl Pts',(1.35382716141607,23.800742079636,15.4242516057205));
#48446=CARTESIAN_POINT('Ctrl Pts',(1.60549250967171,23.7697041807392,15.2410467794464));
#48447=CARTESIAN_POINT('Ctrl Pts',(1.92940593611467,23.7197133936811,14.8981184132296));
#48448=CARTESIAN_POINT('Ctrl Pts',(2.02949951422288,23.702179261639,14.7689149942455));
#48449=CARTESIAN_POINT('Ctrl Pts',(2.20391056801833,23.6669594708688,14.4915814794044));
#48450=CARTESIAN_POINT('Ctrl Pts',(2.27755631464174,23.6495142844082,14.343947630229));
#48451=CARTESIAN_POINT('Ctrl Pts',(2.44621775174173,23.5988439045661,13.9013008857712));
#48452=CARTESIAN_POINT('Ctrl Pts',(2.50172957006313,23.565231912974,13.5946162156367));
#48453=CARTESIAN_POINT('Ctrl Pts',(2.49900670227979,23.5122570362497,13.1195226833282));
#48454=CARTESIAN_POINT('Ctrl Pts',(2.48149275392758,23.4938356230605,12.9538755101879));
#48455=CARTESIAN_POINT('Ctrl Pts',(2.38193024416109,23.4394766726213,12.474916242549));
#48456=CARTESIAN_POINT('Ctrl Pts',(2.25550934280905,23.4034286357378,12.174398566632));
#48457=CARTESIAN_POINT('Ctrl Pts',(1.98432892060312,23.3482906657723,11.7705675284845));
#48458=CARTESIAN_POINT('Ctrl Pts',(1.88010313594603,23.3297164904084,11.6441219062015));
#48459=CARTESIAN_POINT('Ctrl Pts',(1.53501053736421,23.2741269355648,11.3003825521099));
#48460=CARTESIAN_POINT('Ctrl Pts',(1.2635768739027,23.2371912876301,11.1187029053315));
#48461=CARTESIAN_POINT('Ctrl Pts',(0.813131910942001,23.1805658665522,10.930198570904));
#48462=CARTESIAN_POINT('Ctrl Pts',(0.655243673772007,23.1614154088171,10.8817787103818));
#48463=CARTESIAN_POINT('Ctrl Pts',(0.335914808662987,23.1234496792875,10.8174439251418));
#48464=CARTESIAN_POINT('Ctrl Pts',(0.175384440319663,23.1046854656622,10.8009685465805));
#48465=CARTESIAN_POINT('Ctrl Pts',(-0.149484151903419,23.066510887471,10.7990976992974));
#48466=CARTESIAN_POINT('Ctrl Pts',(-0.313053856599623,23.0471883356712,
10.8142706837244));
#48467=CARTESIAN_POINT('Ctrl Pts',(-0.632630036280473,23.0086964515106,
10.875975037635));
#48468=CARTESIAN_POINT('Ctrl Pts',(-0.787958017962882,22.9896045334834,
10.9219260723622));
#48469=CARTESIAN_POINT('Ctrl Pts',(-1.09086661666943,22.9507192196918,11.0444974717313));
#48470=CARTESIAN_POINT('Ctrl Pts',(-1.23745477480971,22.9310151443303,11.1214723932316));
#48471=CARTESIAN_POINT('Ctrl Pts',(-1.51078846884569,22.8918249036477,11.3015468741404));
#48472=CARTESIAN_POINT('Ctrl Pts',(-1.63719969881383,22.8724470716651,11.4037218918722));
#48473=CARTESIAN_POINT('Ctrl Pts',(-1.8708194044265,22.8330444106825,11.633440320949));
#48474=CARTESIAN_POINT('Ctrl Pts',(-1.97700117694386,22.8131109911634,11.7608938065539));
#48475=CARTESIAN_POINT('Ctrl Pts',(-2.16077650210772,22.7734586871545,12.0321850023688));
#48476=CARTESIAN_POINT('Ctrl Pts',(-2.23845920549876,22.7538585391541,12.1750079222615));
#48477=CARTESIAN_POINT('Ctrl Pts',(-2.36644648432654,22.7140011223799,12.4769529908112));
#48478=CARTESIAN_POINT('Ctrl Pts',(-2.41579438734412,22.693833981374,12.6356146637894));
#48479=CARTESIAN_POINT('Ctrl Pts',(-2.48301959290936,22.6528949202455,12.963569463533));
#48480=CARTESIAN_POINT('Ctrl Pts',(-2.5,22.6322916274191,13.1317725807118));
#48481=CARTESIAN_POINT('Ctrl Pts',(-2.5,22.6116296396575,13.3));
#48482=CARTESIAN_POINT('',(-2.49962956580465,24.4076684122549,13.3002239646526));
#48483=CARTESIAN_POINT('Ctrl Pts',(-1.80833658952121,24.1386090163582,15.0220712193704));
#48484=CARTESIAN_POINT('Ctrl Pts',(-1.81020050232586,24.1389337537035,15.0202577426898));
#48485=CARTESIAN_POINT('Ctrl Pts',(-1.81198682056181,24.1392454317471,15.0185145328336));
#48486=CARTESIAN_POINT('Ctrl Pts',(-1.81382907906759,24.1395965832126,15.0166507577355));
#48487=CARTESIAN_POINT('Ctrl Pts',(-1.84511374165097,24.1455597284942,14.9850007070546));
#48488=CARTESIAN_POINT('Ctrl Pts',(-1.87518987859362,24.1517791058518,14.9522286304461));
#48489=CARTESIAN_POINT('Ctrl Pts',(-1.90416092244935,24.1581166532201,14.9185705131251));
#48490=CARTESIAN_POINT('Ctrl Pts',(-1.93313196630509,24.1644542005884,14.8849123958042));
#48491=CARTESIAN_POINT('Ctrl Pts',(-1.96099824777268,24.170909918477,14.8503685507711));
#48492=CARTESIAN_POINT('Ctrl Pts',(-1.98790086801484,24.1773521102019,14.8151392463294));
#48493=CARTESIAN_POINT('Ctrl Pts',(-2.03641945626578,24.1889705341666,14.7516035720648));
#48494=CARTESIAN_POINT('Ctrl Pts',(-2.08181417555863,24.200546145274,14.6858324035231));
#48495=CARTESIAN_POINT('Ctrl Pts',(-2.12395119533515,24.2120525428482,14.6180120824061));
#48496=CARTESIAN_POINT('Ctrl Pts',(-2.12856658903148,24.2133128729597,14.6105835199632));
#48497=CARTESIAN_POINT('Ctrl Pts',(-2.13314288835672,24.2145723763142,14.6031303224517));
#48498=CARTESIAN_POINT('Ctrl Pts',(-2.13767990859671,24.215831020905,14.5956526976106));
#48499=CARTESIAN_POINT('Ctrl Pts',(-2.15006608266115,24.2192671508235,14.5752386024621));
#48500=CARTESIAN_POINT('Ctrl Pts',(-2.16215964544334,24.2226968046935,14.5546425496117));
#48501=CARTESIAN_POINT('Ctrl Pts',(-2.17395700753042,24.2261192080105,14.5338686059686));
#48502=CARTESIAN_POINT('Ctrl Pts',(-2.17398855418554,24.2261283596646,14.5338130555472));
#48503=CARTESIAN_POINT('Ctrl Pts',(-2.17402009872259,24.2261375112669,14.5337575038535));
#48504=CARTESIAN_POINT('Ctrl Pts',(-2.1740516411416,24.2261466628173,14.5337019508877));
#48505=CARTESIAN_POINT('Ctrl Pts',(-2.21384369734985,24.2376917193109,14.4636196044073));
#48506=CARTESIAN_POINT('Ctrl Pts',(-2.2502669318921,24.2491559865257,14.3915106216839));
#48507=CARTESIAN_POINT('Ctrl Pts',(-2.28317904319985,24.2605980621657,14.3176173417912));
#48508=CARTESIAN_POINT('Ctrl Pts',(-2.28618364083904,24.2616426269805,14.3108715097708));
#48509=CARTESIAN_POINT('Ctrl Pts',(-2.2891589413337,24.2626870039974,14.304110814845));
#48510=CARTESIAN_POINT('Ctrl Pts',(-2.29210481557446,24.2637312360772,14.2973354467699));
#48511=CARTESIAN_POINT('Ctrl Pts',(-2.3042995770904,24.2680539464643,14.2692880859167));
#48512=CARTESIAN_POINT('Ctrl Pts',(-2.31599047958798,24.2723740128452,14.2409893710612));
#48513=CARTESIAN_POINT('Ctrl Pts',(-2.32716887971432,24.2766938806141,14.2124532790457));
#48514=CARTESIAN_POINT('Ctrl Pts',(-2.35879787736297,24.2889168361322,14.1317111355313));
#48515=CARTESIAN_POINT('Ctrl Pts',(-2.38616662427351,24.3010794544928,14.0494696349969));
#48516=CARTESIAN_POINT('Ctrl Pts',(-2.4091989526512,24.3132214044725,13.9661006403656));
#48517=CARTESIAN_POINT('Ctrl Pts',(-2.43274903125694,24.3256362967821,13.8808575705093));
#48518=CARTESIAN_POINT('Ctrl Pts',(-2.45176516544558,24.3380294312079,13.794436431863));
#48519=CARTESIAN_POINT('Ctrl Pts',(-2.46616766170601,24.350418449224,13.7072287381561));
#48520=CARTESIAN_POINT('Ctrl Pts',(-2.46874290237542,24.3526336695908,13.6916355524016));
#48521=CARTESIAN_POINT('Ctrl Pts',(-2.47117064890133,24.354848699713,13.6760171874997));
#48522=CARTESIAN_POINT('Ctrl Pts',(-2.47345045763519,24.3570635663588,13.6603758326943));
#48523=CARTESIAN_POINT('Ctrl Pts',(-2.47346714033298,24.3570797738372,13.6602613757263));
#48524=CARTESIAN_POINT('Ctrl Pts',(-2.47348381510892,24.3570959813069,13.6601469175272));
#48525=CARTESIAN_POINT('Ctrl Pts',(-2.47350048196299,24.3571121887678,13.6600324580979));
#48526=CARTESIAN_POINT('Ctrl Pts',(-2.4862662866267,24.3695261260101,13.5723634409001));
#48527=CARTESIAN_POINT('Ctrl Pts',(-2.49438449435988,24.3819369045509,13.4839724022708));
#48528=CARTESIAN_POINT('Ctrl Pts',(-2.49778878735398,24.3943638978535,13.3952617518356));
#48529=CARTESIAN_POINT('Ctrl Pts',(-2.49900315849596,24.3987968247709,13.3636171037218));
#48530=CARTESIAN_POINT('Ctrl Pts',(-2.49961772539878,24.40323159877,13.3319317884665));
#48531=CARTESIAN_POINT('Ctrl Pts',(-2.49962956580465,24.4076684122549,13.3002239646526));
#48532=CARTESIAN_POINT('',(-2.5,23.6803207434639,13.2999999993226));
#48533=CARTESIAN_POINT('',(-2.5,70.2,13.3));
#48534=CARTESIAN_POINT('',(2.5,22.5894736842105,13.3));
#48535=CARTESIAN_POINT('Ctrl Pts',(-2.5,23.6803207434639,13.2999999986451));
#48536=CARTESIAN_POINT('Ctrl Pts',(-2.50000000012045,23.6459460095297,13.5222442475586));
#48537=CARTESIAN_POINT('Ctrl Pts',(-2.4704272669999,23.6147118780889,13.7432791390963));
#48538=CARTESIAN_POINT('Ctrl Pts',(-2.3411668218586,23.5475698736697,14.2171224251415));
#48539=CARTESIAN_POINT('Ctrl Pts',(-2.22919616600022,23.5115414052313,14.4631000178917));
#48540=CARTESIAN_POINT('Ctrl Pts',(-1.8996327770728,23.4265535877506,14.9575442480085));
#48541=CARTESIAN_POINT('Ctrl Pts',(-1.66787132558335,23.3772637209859,15.1904998765396));
#48542=CARTESIAN_POINT('Ctrl Pts',(-1.26623858292357,23.3051655955838,15.4614813800414));
#48543=CARTESIAN_POINT('Ctrl Pts',(-1.12590945121923,23.28207350758,15.5378087959533));
#48544=CARTESIAN_POINT('Ctrl Pts',(-0.670759057692837,23.2135390652347,
15.7315376323321));
#48545=CARTESIAN_POINT('Ctrl Pts',(-0.339085465467693,23.1703807948407,
15.7994976518128));
#48546=CARTESIAN_POINT('Ctrl Pts',(0.260693413184836,23.0884249977271,15.8003911170477));
#48547=CARTESIAN_POINT('Ctrl Pts',(0.523401695645916,23.0513739468048,15.7588333700899));
#48548=CARTESIAN_POINT('Ctrl Pts',(1.07592400691972,22.9690407659882,15.5787750078992));
#48549=CARTESIAN_POINT('Ctrl Pts',(1.35601979032557,22.9254268943002,15.4241211559787));
#48550=CARTESIAN_POINT('Ctrl Pts',(1.71964076389121,22.8625629124352,15.1213018488941));
#48551=CARTESIAN_POINT('Ctrl Pts',(1.82983196068492,22.8419598691273,15.0105592143298));
#48552=CARTESIAN_POINT('Ctrl Pts',(2.09969541621544,22.7849831730603,14.683219524228));
#48553=CARTESIAN_POINT('Ctrl Pts',(2.23591951817411,22.7480601948783,14.4500491783475));
#48554=CARTESIAN_POINT('Ctrl Pts',(2.4431562272875,22.6693975947776,13.9128451862319));
#48555=CARTESIAN_POINT('Ctrl Pts',(2.5,22.6291961383663,13.6078280522502));
#48556=CARTESIAN_POINT('Ctrl Pts',(2.5,22.5894736842105,13.3));
#48557=CARTESIAN_POINT('',(2.5,21.6105263157895,13.3));
#48558=CARTESIAN_POINT('',(2.5,70.2,13.3));
#48559=CARTESIAN_POINT('Ctrl Pts',(-2.5,22.6116296396575,13.3));
#48560=CARTESIAN_POINT('Ctrl Pts',(-2.5,22.5924668561326,13.4560210787061));
#48561=CARTESIAN_POINT('Ctrl Pts',(-2.48539461222184,22.573251129917,13.6120627591118));
#48562=CARTESIAN_POINT('Ctrl Pts',(-2.39559058063777,22.5137915737753,14.08533547675));
#48563=CARTESIAN_POINT('Ctrl Pts',(-2.27333684123802,22.4739041219184,14.3897338451193));
#48564=CARTESIAN_POINT('Ctrl Pts',(-2.00865809026983,22.4134356942506,14.7970497810158));
#48565=CARTESIAN_POINT('Ctrl Pts',(-1.90822223056209,22.3934222341015,14.9231293121602));
#48566=CARTESIAN_POINT('Ctrl Pts',(-1.56687450718985,22.3319591699888,15.2758048587272));
#48567=CARTESIAN_POINT('Ctrl Pts',(-1.29268689868116,22.2908032340347,15.4651410527906));
#48568=CARTESIAN_POINT('Ctrl Pts',(-0.685592003802375,22.207364289261,15.7268534999989));
#48569=CARTESIAN_POINT('Ctrl Pts',(-0.358483890929012,22.1657797807692,
15.7962212509069));
#48570=CARTESIAN_POINT('Ctrl Pts',(0.285301823842494,22.0839647725545,15.8032769734437));
#48571=CARTESIAN_POINT('Ctrl Pts',(0.595840871907412,22.0445506619614,15.7480029313275));
#48572=CARTESIAN_POINT('Ctrl Pts',(1.18942160917842,21.9625008959697,15.5224287666394));
#48573=CARTESIAN_POINT('Ctrl Pts',(1.46579069100765,21.9209040823827,15.3507018085121));
#48574=CARTESIAN_POINT('Ctrl Pts',(1.94023559772861,21.8372435214935,14.9097617920686));
#48575=CARTESIAN_POINT('Ctrl Pts',(2.13296587506391,21.7954326514263,14.6439509026954));
#48576=CARTESIAN_POINT('Ctrl Pts',(2.34055789893654,21.7293522534676,14.1947481054972));
#48577=CARTESIAN_POINT('Ctrl Pts',(2.39587212153975,21.7065664559455,14.0338850769603));
#48578=CARTESIAN_POINT('Ctrl Pts',(2.47798344621124,21.65870920032,13.6823585884458));
#48579=CARTESIAN_POINT('Ctrl Pts',(2.5,21.6338674213799,13.4915574323461));
#48580=CARTESIAN_POINT('Ctrl Pts',(2.5,21.6105263157895,13.3));
#48581=CARTESIAN_POINT('Origin',(0.,70.2,13.3));
#48582=CARTESIAN_POINT('',(-2.48616900737713,26.3471379964276,13.5677880585459));
#48583=CARTESIAN_POINT('Ctrl Pts',(-2.49999999183544,24.407511587746,13.3002020465273));
#48584=CARTESIAN_POINT('Ctrl Pts',(-2.50001929365448,24.4409600114742,13.0613731584544));
#48585=CARTESIAN_POINT('Ctrl Pts',(-2.4658149491821,24.4741969076914,12.8237123231116));
#48586=CARTESIAN_POINT('Ctrl Pts',(-2.32581088600144,24.5421763645029,12.3477731262211));
#48587=CARTESIAN_POINT('Ctrl Pts',(-2.21560394886077,24.5768594070736,12.1137297679167));
#48588=CARTESIAN_POINT('Ctrl Pts',(-1.89787935016659,24.6546455782246,11.6433680242041));
#48589=CARTESIAN_POINT('Ctrl Pts',(-1.67769222506848,24.6973385022906,11.4207048187397));
#48590=CARTESIAN_POINT('Ctrl Pts',(-1.15201874668985,24.7840059525177,11.057030208371));
#48591=CARTESIAN_POINT('Ctrl Pts',(-0.847361079951804,24.827088526998,10.9251047770606));
#48592=CARTESIAN_POINT('Ctrl Pts',(-0.230843896234704,24.9107769898447,
10.7924564888713));
#48593=CARTESIAN_POINT('Ctrl Pts',(0.0732732684954316,24.950611137483,10.7829118544294));
#48594=CARTESIAN_POINT('Ctrl Pts',(0.532590161893144,25.0114370647908,10.8519798196951));
#48595=CARTESIAN_POINT('Ctrl Pts',(0.690703404405739,25.0324978888,10.8918071137798));
#48596=CARTESIAN_POINT('Ctrl Pts',(1.15528571238928,25.0964821783083,11.0583958715576));
#48597=CARTESIAN_POINT('Ctrl Pts',(1.4414980794328,25.1389826087854,11.2308055265104));
#48598=CARTESIAN_POINT('Ctrl Pts',(1.92198551185649,25.223124277075,11.6695862848393));
#48599=CARTESIAN_POINT('Ctrl Pts',(2.11460790562612,25.2636010545971,11.9285915123811));
#48600=CARTESIAN_POINT('Ctrl Pts',(2.32321013274833,25.3248334163836,12.3625507451866));
#48601=CARTESIAN_POINT('Ctrl Pts',(2.37894021841261,25.345293614433,12.514656051798));
#48602=CARTESIAN_POINT('Ctrl Pts',(2.46120545611504,25.3866200083521,12.8311493730713));
#48603=CARTESIAN_POINT('Ctrl Pts',(2.48682722270015,25.4074006379551,12.9949608230336));
#48604=CARTESIAN_POINT('Ctrl Pts',(2.5146917357811,25.4699403728579,13.4921372592396));
#48605=CARTESIAN_POINT('Ctrl Pts',(2.46686591915056,25.511042430498,13.8246000050189));
#48606=CARTESIAN_POINT('Ctrl Pts',(2.24500666145808,25.5931180216562,14.4482024106216));
#48607=CARTESIAN_POINT('Ctrl Pts',(2.07441443456947,25.6333128364487,14.7336211164078));
#48608=CARTESIAN_POINT('Ctrl Pts',(1.62923400751575,25.7144980886799,15.22539808679));
#48609=CARTESIAN_POINT('Ctrl Pts',(1.35768468883391,25.7547972660912,15.4256294544487));
#48610=CARTESIAN_POINT('Ctrl Pts',(0.908665683530526,25.8145327190637,15.6345890718155));
#48611=CARTESIAN_POINT('Ctrl Pts',(0.756292207196053,25.8338400953433,15.6883061057311));
#48612=CARTESIAN_POINT('Ctrl Pts',(0.275664118819158,25.8931857081566,15.8070887356835));
#48613=CARTESIAN_POINT('Ctrl Pts',(-0.0613030305722818,25.9326969470317,
15.821463648482));
#48614=CARTESIAN_POINT('Ctrl Pts',(-0.552179682928576,25.9912737049207,
15.7437011244677));
#48615=CARTESIAN_POINT('Ctrl Pts',(-0.710322241437892,26.0103394186011,
15.7025035173479));
#48616=CARTESIAN_POINT('Ctrl Pts',(-1.16853457910079,26.0676155842894,15.5338957579576));
#48617=CARTESIAN_POINT('Ctrl Pts',(-1.44895659615568,26.1052630866398,15.3630913338774));
#48618=CARTESIAN_POINT('Ctrl Pts',(-1.80006889063422,26.1600137487588,15.0414130139519));
#48619=CARTESIAN_POINT('Ctrl Pts',(-1.90187043698653,26.1772366660204,14.9296189547623));
#48620=CARTESIAN_POINT('Ctrl Pts',(-2.1337701667803,26.2212635145788,14.6234103165689));
#48621=CARTESIAN_POINT('Ctrl Pts',(-2.24788012884225,26.247838143168,14.4186815080764));
#48622=CARTESIAN_POINT('Ctrl Pts',(-2.41059213792532,26.2987657420784,13.9975960829663));
#48623=CARTESIAN_POINT('Ctrl Pts',(-2.46225581692207,26.3229414940952,13.7846677762047));
#48624=CARTESIAN_POINT('Ctrl Pts',(-2.48562243203351,26.3472602063278,13.5677333101648));
#48625=CARTESIAN_POINT('Ctrl Pts',(-2.48561657000623,26.3478373019899,13.5677877273336));
#48626=CARTESIAN_POINT('Ctrl Pts',(-2.49040728835277,26.355511883304,13.5233200849104));
#48627=CARTESIAN_POINT('Ctrl Pts',(-2.49400562263312,26.3631210348639,13.4787161189908));
#48628=CARTESIAN_POINT('Ctrl Pts',(-2.49880070726847,26.3781627629798,13.3893975884711));
#48629=CARTESIAN_POINT('Ctrl Pts',(-2.49999999980375,26.3855985398547,13.3447078590484));
#48630=CARTESIAN_POINT('Ctrl Pts',(-2.49999999999832,26.3929871638855,13.3));
#48631=CARTESIAN_POINT('',(-0.790532179204624,24.1655288633479,10.9282793432527));
#48632=CARTESIAN_POINT('Ctrl Pts',(-2.5,25.4505462844759,13.3));
#48633=CARTESIAN_POINT('Ctrl Pts',(-2.5,25.4346615266009,13.4333107304046));
#48634=CARTESIAN_POINT('Ctrl Pts',(-2.48933645207011,25.4188567362605,13.5666328076926));
#48635=CARTESIAN_POINT('Ctrl Pts',(-2.42324395792347,25.3702827392235,13.9757840738102));
#48636=CARTESIAN_POINT('Ctrl Pts',(-2.33212866227708,25.3385997000097,14.2433969388235));
#48637=CARTESIAN_POINT('Ctrl Pts',(-2.03959957204297,25.2680868661861,14.7836982679379));
#48638=CARTESIAN_POINT('Ctrl Pts',(-1.82362150819777,25.2286776131871,15.0423330092833));
#48639=CARTESIAN_POINT('Ctrl Pts',(-1.34493833058986,25.158314656507,15.4258879748345));
#48640=CARTESIAN_POINT('Ctrl Pts',(-1.09880443934562,25.1276257097723,15.562945456558));
#48641=CARTESIAN_POINT('Ctrl Pts',(-0.520730508196071,25.0593035631249,
15.7678037619262));
#48642=CARTESIAN_POINT('Ctrl Pts',(-0.187326421714155,25.0206568083071,
15.8151734986127));
#48643=CARTESIAN_POINT('Ctrl Pts',(0.420421962637397,24.9526566181903,15.7797283299768));
#48644=CARTESIAN_POINT('Ctrl Pts',(0.690769551352685,24.923533803137,15.7184075514967));
#48645=CARTESIAN_POINT('Ctrl Pts',(1.25685316725015,24.8582398111244,15.4870726759433));
#48646=CARTESIAN_POINT('Ctrl Pts',(1.53911953807666,24.8204500228646,15.2985012375989));
#48647=CARTESIAN_POINT('Ctrl Pts',(1.87845471199616,24.7683199088682,14.9561215064622));
#48648=CARTESIAN_POINT('Ctrl Pts',(1.971999279987,24.7529354255617,14.8435579696091));
#48649=CARTESIAN_POINT('Ctrl Pts',(2.243464174008,24.7037507866139,14.4516079119598));
#48650=CARTESIAN_POINT('Ctrl Pts',(2.37593068207173,24.6709951528344,14.1451326843892));
#48651=CARTESIAN_POINT('Ctrl Pts',(2.50416688031434,24.6057570862472,13.5442892572167));
#48652=CARTESIAN_POINT('Ctrl Pts',(2.51574993528651,24.576384292556,13.2585326566879));
#48653=CARTESIAN_POINT('Ctrl Pts',(2.43724795843491,24.5175853955505,12.6563871696382));
#48654=CARTESIAN_POINT('Ctrl Pts',(2.3337649705917,24.4882695828866,12.3471343843325));
#48655=CARTESIAN_POINT('Ctrl Pts',(2.09644986008896,24.4402255726524,11.9289542677213));
#48656=CARTESIAN_POINT('Ctrl Pts',(2.00579234730328,24.424462288069,11.7994361632438));
#48657=CARTESIAN_POINT('Ctrl Pts',(1.72843745579795,24.3834881852855,11.4736835393712));
#48658=CARTESIAN_POINT('Ctrl Pts',(1.52123163852952,24.3602284421505,11.297780355606));
#48659=CARTESIAN_POINT('Ctrl Pts',(1.00429900121169,24.3097657542319,10.9864742600211));
#48660=CARTESIAN_POINT('Ctrl Pts',(0.687370774496695,24.279429585749,10.8733916016535));
#48661=CARTESIAN_POINT('Ctrl Pts',(0.149164509496832,24.2330693451276,10.7955685681763));
#48662=CARTESIAN_POINT('Ctrl Pts',(-0.0624686035915402,24.2167113037373,
10.7918886621725));
#48663=CARTESIAN_POINT('Ctrl Pts',(-0.448560379140616,24.189229973862,10.834181355582));
#48664=CARTESIAN_POINT('Ctrl Pts',(-0.622284832998793,24.1777142215037,
10.8721998294773));
#48665=CARTESIAN_POINT('Ctrl Pts',(-0.790532179204627,24.1655288633479,
10.9282793432527));
#48666=CARTESIAN_POINT('',(-0.830840037653311,24.1597523284343,10.9410233051414));
#48667=CARTESIAN_POINT('Ctrl Pts',(-0.831036541944574,24.1603152340113,
10.940719093145));
#48668=CARTESIAN_POINT('Ctrl Pts',(-0.817567384401107,24.1620535629164,
10.9364517239282));
#48669=CARTESIAN_POINT('Ctrl Pts',(-0.804065260568294,24.1637914392606,
10.9323052309739));
#48670=CARTESIAN_POINT('Ctrl Pts',(-0.790532179204624,24.1655288633479,
10.9282793432527));
#48671=CARTESIAN_POINT('',(-2.49999972384016,23.6805025116397,13.2988249259027));
#48672=CARTESIAN_POINT('Ctrl Pts',(-0.830274846070968,24.1581332823986,
10.9418982888811));
#48673=CARTESIAN_POINT('Ctrl Pts',(-1.02912308992684,24.1232364201349,11.0119116790078));
#48674=CARTESIAN_POINT('Ctrl Pts',(-1.21842442783496,24.0883981669736,11.1068342240936));
#48675=CARTESIAN_POINT('Ctrl Pts',(-1.64597028965375,24.0073058843925,11.3939124963739));
#48676=CARTESIAN_POINT('Ctrl Pts',(-1.86507159543317,23.9652828488002,11.6076765519296));
#48677=CARTESIAN_POINT('Ctrl Pts',(-2.19064207469752,23.8826599052698,12.0677436289267));
#48678=CARTESIAN_POINT('Ctrl Pts',(-2.30650255866757,23.8431942411814,12.3014188211821));
#48679=CARTESIAN_POINT('Ctrl Pts',(-2.46088053508975,23.7614727519614,12.791239366162));
#48680=CARTESIAN_POINT('Ctrl Pts',(-2.49988005997949,23.7198878942854,13.0442370498513));
#48681=CARTESIAN_POINT('Ctrl Pts',(-2.49999972384016,23.6805025116397,13.2988249259027));
#48682=CARTESIAN_POINT('Ctrl Pts',(-2.49999972384016,23.6805025116397,13.2988249259027));
#48683=CARTESIAN_POINT('Ctrl Pts',(-2.49999990949688,23.6804414057986,13.2992199152432));
#48684=CARTESIAN_POINT('Ctrl Pts',(-2.49999999999979,23.6803818355265,13.2996050178555));
#48685=CARTESIAN_POINT('Ctrl Pts',(-2.5,23.6803207434639,13.2999999986451));
#48686=CARTESIAN_POINT('Origin',(1.6,144.5,10.3));
#48687=CARTESIAN_POINT('',(1.6,144.5,14.5));
#48688=CARTESIAN_POINT('',(1.6,144.5,12.1));
#48689=CARTESIAN_POINT('Origin',(0.,144.5,13.3));
#48690=CARTESIAN_POINT('',(1.6,144.5,10.3));
#48691=CARTESIAN_POINT('Origin',(1.6,136.,16.3));
#48692=CARTESIAN_POINT('',(1.6,136.,12.1));
#48693=CARTESIAN_POINT('',(1.6,136.,14.5));
#48694=CARTESIAN_POINT('Origin',(0.,136.,13.3));
#48695=CARTESIAN_POINT('',(1.6,136.,16.3));
#48696=CARTESIAN_POINT('Origin',(1.6,140.25,13.3));
#48697=CARTESIAN_POINT('',(1.6,132.35,14.5));
#48698=CARTESIAN_POINT('',(1.6,132.35,12.1));
#48699=CARTESIAN_POINT('Origin',(2.26918997026575,118.064918569113,12.5575400117452));
#48700=CARTESIAN_POINT('',(1.73940833428499,117.962536543046,12.7139827773687));
#48701=CARTESIAN_POINT('',(1.73940833428499,117.962536543046,12.7139827773687));
#48702=CARTESIAN_POINT('',(1.95209195497481,118.519715684653,12.6482782748721));
#48703=CARTESIAN_POINT('',(1.95209195497481,118.519715684653,12.6482782748721));
#48704=CARTESIAN_POINT('',(2.90531341659142,118.445890165984,12.3682449948735));
#48705=CARTESIAN_POINT('Ctrl Pts',(2.95532532744321,114.524755006807,12.5175939454839));
#48706=CARTESIAN_POINT('Ctrl Pts',(3.06876373495539,114.584537551976,12.9831594433255));
#48707=CARTESIAN_POINT('Ctrl Pts',(3.06785527722985,114.700312831601,13.9338767019519));
#48708=CARTESIAN_POINT('Ctrl Pts',(2.25534968607699,114.926403080468,15.609150838537));
#48709=CARTESIAN_POINT('Ctrl Pts',(0.0662652269878777,115.200811352631,
16.6410423398491));
#48710=CARTESIAN_POINT('Ctrl Pts',(-2.50595963339538,115.52278944504,15.4068000621842));
#48711=CARTESIAN_POINT('Ctrl Pts',(-2.937218093367,115.738804616394,13.546395210328));
#48712=CARTESIAN_POINT('Ctrl Pts',(-2.71348433299149,115.85500608334,12.6424604110653));
#48713=CARTESIAN_POINT('Ctrl Pts',(-2.65350431190029,115.880786019828,12.4447186453377));
#48714=CARTESIAN_POINT('Ctrl Pts',(-2.51956517014225,115.925788602732,12.1093992582891));
#48715=CARTESIAN_POINT('Ctrl Pts',(-2.14456329762995,116.015344903557,11.4921752961234));
#48716=CARTESIAN_POINT('Ctrl Pts',(-1.50208232786518,116.116660442079,10.9634323628369));
#48717=CARTESIAN_POINT('Ctrl Pts',(-0.743705841514237,116.216924112424,
10.6832072795712));
#48718=CARTESIAN_POINT('Ctrl Pts',(0.0519424989325072,116.316482211687,
10.5766342196015));
#48719=CARTESIAN_POINT('Ctrl Pts',(1.04279822899032,116.439601730527,10.7807965086205));
#48720=CARTESIAN_POINT('Ctrl Pts',(1.9954829094094,116.58519875718,11.5039772484606));
#48721=CARTESIAN_POINT('Ctrl Pts',(2.53561723147412,116.728640862891,12.5517410043371));
#48722=CARTESIAN_POINT('Ctrl Pts',(2.5694900167613,116.869918400196,13.7111768527204));
#48723=CARTESIAN_POINT('Ctrl Pts',(2.05742503005493,117.024497486579,14.8738134954349));
#48724=CARTESIAN_POINT('Ctrl Pts',(0.930701672170671,117.191464070288,15.7005591366327));
#48725=CARTESIAN_POINT('Ctrl Pts',(-0.562095627157725,117.369822261529,
15.7584322387535));
#48726=CARTESIAN_POINT('Ctrl Pts',(-1.59617390811852,117.515351376341,15.1152935972272));
#48727=CARTESIAN_POINT('Ctrl Pts',(-2.03359602972292,117.615626970315,14.4308327626405));
#48728=CARTESIAN_POINT('Ctrl Pts',(-2.17011759536166,117.665364077208,14.0554925009457));
#48729=CARTESIAN_POINT('Ctrl Pts',(-2.21671921699844,117.690134597954,13.8624602176105));
#48730=CARTESIAN_POINT('Ctrl Pts',(-2.23459322200071,117.702496092692,13.7650534213741));
#48731=CARTESIAN_POINT('Ctrl Pts',(-2.24324088520118,117.709552710981,13.7091809472188));
#48732=CARTESIAN_POINT('Ctrl Pts',(-2.30787845616854,117.769500502143,13.233386793593));
#48733=CARTESIAN_POINT('Ctrl Pts',(-2.14259558128388,117.882889231505,12.2973265421649));
#48734=CARTESIAN_POINT('Ctrl Pts',(-1.26569931155285,118.03312163484,11.395784096862));
#48735=CARTESIAN_POINT('Ctrl Pts',(-0.207382758034273,118.167589041999,
11.0848752646015));
#48736=CARTESIAN_POINT('Ctrl Pts',(0.756408994557853,118.286006106533,11.2469230615091));
#48737=CARTESIAN_POINT('Ctrl Pts',(1.56745847087833,118.40662964019,11.8126008815501));
#48738=CARTESIAN_POINT('Ctrl Pts',(1.86831064635946,118.484468543414,12.35991743902));
#48739=CARTESIAN_POINT('Ctrl Pts',(1.96892768266466,118.526537502283,12.703608403237));
#48740=CARTESIAN_POINT('Ctrl Pts',(2.7669220611078,114.591352155898,12.5327846010662));
#48741=CARTESIAN_POINT('Ctrl Pts',(2.87674269859879,114.647538874759,12.9695240152525));
#48742=CARTESIAN_POINT('Ctrl Pts',(2.88232355626827,114.756241528531,13.8620584078666));
#48743=CARTESIAN_POINT('Ctrl Pts',(2.13221229569936,114.968135572939,15.4375130757603));
#48744=CARTESIAN_POINT('Ctrl Pts',(0.0926580189939055,115.224683159866,
16.4162364195046));
#48745=CARTESIAN_POINT('Ctrl Pts',(-2.31360202512171,115.524901307596,15.2827271366528));
#48746=CARTESIAN_POINT('Ctrl Pts',(-2.72779167000299,115.725916081504,13.5548349021305));
#48747=CARTESIAN_POINT('Ctrl Pts',(-2.52648386507752,115.833973569872,12.712701434762));
#48748=CARTESIAN_POINT('Ctrl Pts',(-2.4721874848677,115.85794478792,12.5284078779757));
#48749=CARTESIAN_POINT('Ctrl Pts',(-2.35016956426982,115.899786125458,12.2156840563554));
#48750=CARTESIAN_POINT('Ctrl Pts',(-2.00623455037881,115.98303414384,11.6392046808839));
#48751=CARTESIAN_POINT('Ctrl Pts',(-1.41325953841494,116.077182179787,11.1431032941946));
#48752=CARTESIAN_POINT('Ctrl Pts',(-0.71088717098477,116.170336542424,10.8769908864139));
#48753=CARTESIAN_POINT('Ctrl Pts',(0.0273902380339246,116.262830174928,
10.7718808932291));
#48754=CARTESIAN_POINT('Ctrl Pts',(0.949387253166724,116.377212890765,10.9538151649334));
#48755=CARTESIAN_POINT('Ctrl Pts',(1.84025305635243,116.512506445318,11.6181657831876));
#48756=CARTESIAN_POINT('Ctrl Pts',(2.35077936414752,116.645857799176,12.5876989105077));
#48757=CARTESIAN_POINT('Ctrl Pts',(2.39183470744452,116.777286985799,13.6658663168934));
#48758=CARTESIAN_POINT('Ctrl Pts',(1.92487206745958,116.921229337443,14.7525882984064));
#48759=CARTESIAN_POINT('Ctrl Pts',(0.881632553648049,117.076924480568,15.5331978841402));
#48760=CARTESIAN_POINT('Ctrl Pts',(-0.512501371025649,117.24359289046,15.6006921262506));
#48761=CARTESIAN_POINT('Ctrl Pts',(-1.48703573917562,117.379936763826,15.0078964255291));
#48762=CARTESIAN_POINT('Ctrl Pts',(-1.90403082779443,117.474103647466,14.3692654859918));
#48763=CARTESIAN_POINT('Ctrl Pts',(-2.03581316980885,117.520865644744,14.0176944890301));
#48764=CARTESIAN_POINT('Ctrl Pts',(-2.08143067211384,117.544169556656,13.8365532081328));
#48765=CARTESIAN_POINT('Ctrl Pts',(-2.09914966879132,117.555803332789,13.7450628668842));
#48766=CARTESIAN_POINT('Ctrl Pts',(-2.10780582026366,117.562445575008,13.6925603576404));
#48767=CARTESIAN_POINT('Ctrl Pts',(-2.17304406469775,117.618882305616,13.2453208704162));
#48768=CARTESIAN_POINT('Ctrl Pts',(-2.02647430250429,117.725837543343,12.360927019113));
#48769=CARTESIAN_POINT('Ctrl Pts',(-1.20558819876245,117.868088734324,11.4984595098835));
#48770=CARTESIAN_POINT('Ctrl Pts',(-0.202110281410913,117.996018243275,
11.1919879778851));
#48771=CARTESIAN_POINT('Ctrl Pts',(0.717727730873791,118.108870229896,11.3359284262728));
#48772=CARTESIAN_POINT('Ctrl Pts',(1.50313989498709,118.224745568758,11.8710949030945));
#48773=CARTESIAN_POINT('Ctrl Pts',(1.79734640115767,118.299357347357,12.3917842530883));
#48774=CARTESIAN_POINT('Ctrl Pts',(1.8978404554453,118.340237099782,12.7236097563076));
#48775=CARTESIAN_POINT('Ctrl Pts',(2.57851879477238,114.657949304988,12.5479752566485));
#48776=CARTESIAN_POINT('Ctrl Pts',(2.68472166224218,114.710540197541,12.9558885871796));
#48777=CARTESIAN_POINT('Ctrl Pts',(2.69679183530668,114.812170225459,13.7902401137812));
#48778=CARTESIAN_POINT('Ctrl Pts',(2.00907490532175,115.009868065408,15.2658753129837));
#48779=CARTESIAN_POINT('Ctrl Pts',(0.119050810999923,115.2485549671,16.1914304991601));
#48780=CARTESIAN_POINT('Ctrl Pts',(-2.12124441684804,115.527013170151,15.1586542111214));
#48781=CARTESIAN_POINT('Ctrl Pts',(-2.51836524663899,115.713027546611,13.5632745939329));
#48782=CARTESIAN_POINT('Ctrl Pts',(-2.33948339716357,115.812941056406,12.7829424584588));
#48783=CARTESIAN_POINT('Ctrl Pts',(-2.29087065783513,115.835103556013,12.6120971106138));
#48784=CARTESIAN_POINT('Ctrl Pts',(-2.1807739583974,115.873783648183,12.3219688544218));
#48785=CARTESIAN_POINT('Ctrl Pts',(-1.86790580312768,115.950723384123,11.7862340656444));
#48786=CARTESIAN_POINT('Ctrl Pts',(-1.32443674896469,116.037703917496,11.3227742255522));
#48787=CARTESIAN_POINT('Ctrl Pts',(-0.678068500455315,116.123748972425,
11.0707744932568));
#48788=CARTESIAN_POINT('Ctrl Pts',(0.0028379771353343,116.209178138168,
10.9671275668568));
#48789=CARTESIAN_POINT('Ctrl Pts',(0.855976277343122,116.314824051003,11.1268338212465));
#48790=CARTESIAN_POINT('Ctrl Pts',(1.68502320329546,116.439814133456,11.7323543179146));
#48791=CARTESIAN_POINT('Ctrl Pts',(2.16594149682093,116.56307473546,12.6236568166783));
#48792=CARTESIAN_POINT('Ctrl Pts',(2.21417939812775,116.684655571401,13.6205557810665));
#48793=CARTESIAN_POINT('Ctrl Pts',(1.79231910486424,116.817961188309,14.631363101378));
#48794=CARTESIAN_POINT('Ctrl Pts',(0.832563435125419,116.962384890849,15.3658366316477));
#48795=CARTESIAN_POINT('Ctrl Pts',(-0.46290711489358,117.117363519388,15.4429520137478));
#48796=CARTESIAN_POINT('Ctrl Pts',(-1.37789757023272,117.244522151312,14.9004992538312));
#48797=CARTESIAN_POINT('Ctrl Pts',(-1.77446562586595,117.332580324617,14.3076982093431));
#48798=CARTESIAN_POINT('Ctrl Pts',(-1.90150874425604,117.37636721228,13.9798964771144));
#48799=CARTESIAN_POINT('Ctrl Pts',(-1.94614212722925,117.398204515359,13.8106461986552));
#48800=CARTESIAN_POINT('Ctrl Pts',(-1.96370611558196,117.409110572885,13.7250723123942));
#48801=CARTESIAN_POINT('Ctrl Pts',(-1.97237075532615,117.415338439035,13.6759397680619));
#48802=CARTESIAN_POINT('Ctrl Pts',(-2.03820967322699,117.468264109088,13.2572549472395));
#48803=CARTESIAN_POINT('Ctrl Pts',(-1.91035302372471,117.568785855181,12.424527496061));
#48804=CARTESIAN_POINT('Ctrl Pts',(-1.14547708597207,117.703055833809,11.601134922905));
#48805=CARTESIAN_POINT('Ctrl Pts',(-0.196837804787558,117.82444744455,11.2991006911685));
#48806=CARTESIAN_POINT('Ctrl Pts',(0.679046467189727,117.931734353258,11.4249337910364));
#48807=CARTESIAN_POINT('Ctrl Pts',(1.43882131909583,118.042861497326,11.9295889246391));
#48808=CARTESIAN_POINT('Ctrl Pts',(1.72638215595589,118.1142461513,12.4236510671564));
#48809=CARTESIAN_POINT('Ctrl Pts',(1.82675322822595,118.153936697284,12.7436111093781));
#48810=CARTESIAN_POINT('Ctrl Pts',(2.39011552843695,114.72454645408,12.5631659122308));
#48811=CARTESIAN_POINT('Ctrl Pts',(2.49270062588558,114.773541520323,12.9422531591066));
#48812=CARTESIAN_POINT('Ctrl Pts',(2.51126011434509,114.868098922389,13.7184218196959));
#48813=CARTESIAN_POINT('Ctrl Pts',(1.88593751494413,115.051600557879,15.094237550207));
#48814=CARTESIAN_POINT('Ctrl Pts',(0.14544360300595,115.272426774335,15.9666245788156));
#48815=CARTESIAN_POINT('Ctrl Pts',(-1.92888680857437,115.529125032708,15.03458128559));
#48816=CARTESIAN_POINT('Ctrl Pts',(-2.30893882327498,115.70013901172,13.5717142857354));
#48817=CARTESIAN_POINT('Ctrl Pts',(-2.1524829292496,115.791908542938,12.8531834821556));
#48818=CARTESIAN_POINT('Ctrl Pts',(-2.10955383080254,115.812262324106,12.6957863432518));
#48819=CARTESIAN_POINT('Ctrl Pts',(-2.01137835252497,115.847781170908,12.428253652488));
#48820=CARTESIAN_POINT('Ctrl Pts',(-1.72957705587654,115.918412624405,11.9332634504048));
#48821=CARTESIAN_POINT('Ctrl Pts',(-1.23561395951444,115.998225655204,11.5024451569099));
#48822=CARTESIAN_POINT('Ctrl Pts',(-0.645249829925848,116.077161402425,
11.2645581000994));
#48823=CARTESIAN_POINT('Ctrl Pts',(-0.0217142837632479,116.155526101408,
11.1623742404844));
#48824=CARTESIAN_POINT('Ctrl Pts',(0.762565301519525,116.252435211241,11.2998524775594));
#48825=CARTESIAN_POINT('Ctrl Pts',(1.5297933502385,116.367121821593,11.8465428526414));
#48826=CARTESIAN_POINT('Ctrl Pts',(1.98110362949434,116.480291671746,12.6596147228489));
#48827=CARTESIAN_POINT('Ctrl Pts',(2.03652408881097,116.592024157004,13.5752452452394));
#48828=CARTESIAN_POINT('Ctrl Pts',(1.65976614226889,116.714693039174,14.5101379043495));
#48829=CARTESIAN_POINT('Ctrl Pts',(0.783494316602796,116.847845301129,15.1984753791552));
#48830=CARTESIAN_POINT('Ctrl Pts',(-0.413312858761503,116.991134148319,
15.2852119012451));
#48831=CARTESIAN_POINT('Ctrl Pts',(-1.26875940128983,117.109107538797,14.7931020821331));
#48832=CARTESIAN_POINT('Ctrl Pts',(-1.64490042393746,117.191057001769,14.2461309326945));
#48833=CARTESIAN_POINT('Ctrl Pts',(-1.76720431870323,117.231868779816,13.9420984651988));
#48834=CARTESIAN_POINT('Ctrl Pts',(-1.81085358234464,117.252239474061,13.7847391891774));
#48835=CARTESIAN_POINT('Ctrl Pts',(-1.82826256237257,117.262417812982,13.7050817579043));
#48836=CARTESIAN_POINT('Ctrl Pts',(-1.83693569038863,117.268231303062,13.6593191784835));
#48837=CARTESIAN_POINT('Ctrl Pts',(-1.9033752817562,117.317645912561,13.2691890240628));
#48838=CARTESIAN_POINT('Ctrl Pts',(-1.79423174494513,117.411734167019,12.488127973009));
#48839=CARTESIAN_POINT('Ctrl Pts',(-1.08536597318167,117.538022933295,11.7038103359265));
#48840=CARTESIAN_POINT('Ctrl Pts',(-0.191565328164199,117.652876645827,
11.406213404452));
#48841=CARTESIAN_POINT('Ctrl Pts',(0.640365203505663,117.754598476621,11.5139391558001));
#48842=CARTESIAN_POINT('Ctrl Pts',(1.37450274320459,117.860977425892,11.9880829461835));
#48843=CARTESIAN_POINT('Ctrl Pts',(1.6554179107541,117.929134955243,12.4555178812246));
#48844=CARTESIAN_POINT('Ctrl Pts',(1.75566600100659,117.967636294783,12.7636124624487));
#48845=CARTESIAN_POINT('Ctrl Pts',(2.31548671935009,116.940942573699,14.2367878010894));
#48846=CARTESIAN_POINT('Ctrl Pts',(2.25782459523788,116.958633659998,14.3663197206516));
#48847=CARTESIAN_POINT('Ctrl Pts',(2.18932717831191,116.976291415496,14.4907161059409));
#48848=CARTESIAN_POINT('Ctrl Pts',(2.11090464171477,116.993906320744,14.607987749139));
#48849=CARTESIAN_POINT('Ctrl Pts',(2.08896395990088,116.998834534596,14.6407974479941));
#48850=CARTESIAN_POINT('Ctrl Pts',(2.06624670924219,117.003759395706,14.673049517398));
#48851=CARTESIAN_POINT('Ctrl Pts',(2.0427735176532,117.008680698696,14.7047005845127));
#48852=CARTESIAN_POINT('Ctrl Pts',(1.95793393600213,117.026467853258,14.8190976098446));
#48853=CARTESIAN_POINT('Ctrl Pts',(1.8632159759054,117.044208509281,14.9256409238034));
#48854=CARTESIAN_POINT('Ctrl Pts',(1.7604463664943,117.061893253579,15.0231276638096));
#48855=CARTESIAN_POINT('Ctrl Pts',(1.65765638941339,117.079581502774,15.120633724486));
#48856=CARTESIAN_POINT('Ctrl Pts',(1.54681285063823,117.097213818201,15.2090788045913));
#48857=CARTESIAN_POINT('Ctrl Pts',(1.4297753456656,117.114781010957,15.2873000870842));
#48858=CARTESIAN_POINT('Ctrl Pts',(1.31725506068872,117.13167017427,15.362502313921));
#48859=CARTESIAN_POINT('Ctrl Pts',(1.19901090213151,117.14849914637,15.4282543220876));
#48860=CARTESIAN_POINT('Ctrl Pts',(1.07670649422147,117.165259960218,15.4835687990835));
#48861=CARTESIAN_POINT('Ctrl Pts',(1.02706604615356,117.172062775617,15.506019628695));
#48862=CARTESIAN_POINT('Ctrl Pts',(0.976756765588284,117.17885436515,15.5267516003765));
#48863=CARTESIAN_POINT('Ctrl Pts',(0.925889782910585,117.185634205178,15.5457012048358));
#48864=CARTESIAN_POINT('Ctrl Pts',(0.912886479342423,117.187367359248,15.5505453580824));
#48865=CARTESIAN_POINT('Ctrl Pts',(0.899842705489527,117.189099753323,15.5552737754267));
#48866=CARTESIAN_POINT('Ctrl Pts',(0.886760298193248,117.190831399141,15.5598852350733));
#48867=CARTESIAN_POINT('Ctrl Pts',(0.761178174160384,117.207454009562,15.6041520801728));
#48868=CARTESIAN_POINT('Ctrl Pts',(0.632034792388793,117.224007429506,15.6376370989038));
#48869=CARTESIAN_POINT('Ctrl Pts',(0.501236200781654,117.240503740859,15.6603315069497));
#48870=CARTESIAN_POINT('Ctrl Pts',(0.363479587821818,117.257877597492,15.684233177045));
#48871=CARTESIAN_POINT('Ctrl Pts',(0.223888496440542,117.27518808512,15.6961659209278));
#48872=CARTESIAN_POINT('Ctrl Pts',(0.0846939106435335,117.292452770346,
15.6961783519871));
#48873=CARTESIAN_POINT('Ctrl Pts',(-0.0540836526485132,117.309665731131,
15.6961907458034));
#48874=CARTESIAN_POINT('Ctrl Pts',(-0.192465693473643,117.326833173632,
15.6843549295801));
#48875=CARTESIAN_POINT('Ctrl Pts',(-0.32825944952498,117.343975900692,15.6607672364423));
#48876=CARTESIAN_POINT('Ctrl Pts',(-0.392775511795997,117.352120466972,
15.6495606454799));
#48877=CARTESIAN_POINT('Ctrl Pts',(-0.456707734830717,117.360259502979,
15.6357020129467));
#48878=CARTESIAN_POINT('Ctrl Pts',(-0.519823689133548,117.36839549867,15.6192047402386));
#48879=CARTESIAN_POINT('Ctrl Pts',(-0.653936963993893,117.385683441766,
15.5841501602424));
#48880=CARTESIAN_POINT('Ctrl Pts',(-0.784361510700284,117.402957449876,
15.5371810040624));
#48881=CARTESIAN_POINT('Ctrl Pts',(-0.909380986500572,117.420243878384,
15.4796350958842));
#48882=CARTESIAN_POINT('Ctrl Pts',(-0.916037991934534,117.421164341758,
15.4765709059171));
#48883=CARTESIAN_POINT('Ctrl Pts',(-0.922679684067035,117.422084841101,
15.4734767309246));
#48884=CARTESIAN_POINT('Ctrl Pts',(-0.929305807850316,117.423005380643,
15.470352773874));
#48885=CARTESIAN_POINT('Ctrl Pts',(-1.04223429111457,117.438694060435,15.4171114305111));
#48886=CARTESIAN_POINT('Ctrl Pts',(-1.15084607653313,117.454344584733,15.3550070389703));
#48887=CARTESIAN_POINT('Ctrl Pts',(-1.25375654870144,117.469949685013,15.2849692667603));
#48888=CARTESIAN_POINT('Ctrl Pts',(-1.35637815267582,117.485510982004,15.2151280895551));
#48889=CARTESIAN_POINT('Ctrl Pts',(-1.45332936855855,117.501027110519,15.1373988742834));
#48890=CARTESIAN_POINT('Ctrl Pts',(-1.54325869101494,117.516491423543,15.0527504127095));
#48891=CARTESIAN_POINT('Ctrl Pts',(-1.59588298748066,117.525540736614,15.0032163384436));
#48892=CARTESIAN_POINT('Ctrl Pts',(-1.64610327006513,117.534572317048,14.9513137316402));
#48893=CARTESIAN_POINT('Ctrl Pts',(-1.69365429344754,117.543584920282,14.8972424084114));
#48894=CARTESIAN_POINT('Ctrl Pts',(-1.77565544949361,117.559127043912,14.803997075329));
#48895=CARTESIAN_POINT('Ctrl Pts',(-1.84971583932375,117.574612701386,14.7043016672338));
#48896=CARTESIAN_POINT('Ctrl Pts',(-1.91519240285048,117.590035579994,14.5997566402122));
#48897=CARTESIAN_POINT('Ctrl Pts',(-1.97148366797609,117.603294879229,14.5098775824752));
#48898=CARTESIAN_POINT('Ctrl Pts',(-2.02143108836489,117.616507787263,14.4164150045289));
#48899=CARTESIAN_POINT('Ctrl Pts',(-2.06465665364232,117.629670617629,14.3203898888529));
#48900=CARTESIAN_POINT('Ctrl Pts',(-2.09269581380972,117.638208960772,14.2581012043382));
#48901=CARTESIAN_POINT('Ctrl Pts',(-2.1179071968939,117.646726238826,14.1947342920141));
#48902=CARTESIAN_POINT('Ctrl Pts',(-2.140211784327,117.655221705677,14.13054504922));
#48903=CARTESIAN_POINT('Ctrl Pts',(-2.15521750441253,117.660937148652,14.0873608471916));
#48904=CARTESIAN_POINT('Ctrl Pts',(-2.16892218130902,117.666647211072,14.0437582790948));
#48905=CARTESIAN_POINT('Ctrl Pts',(-2.18129520696717,117.67235188627,13.9998107137466));
#48906=CARTESIAN_POINT('Ctrl Pts',(-2.19667226087415,117.67944159096,13.9451931852527));
#48907=CARTESIAN_POINT('Ctrl Pts',(-2.20999250553756,117.686522974354,13.8900427740209));
#48908=CARTESIAN_POINT('Ctrl Pts',(-2.22124632398131,117.693596222074,13.8345336184934));
#48909=CARTESIAN_POINT('Ctrl Pts',(-2.22687030744894,117.697131007039,13.8067934719335));
#48910=CARTESIAN_POINT('Ctrl Pts',(-2.23197823813659,117.70066376053,13.7789637472521));
#48911=CARTESIAN_POINT('Ctrl Pts',(-2.23656440171793,117.70419437115,13.7510591660253));
#48912=CARTESIAN_POINT('Ctrl Pts',(-2.2388569471652,117.705959263561,13.7371101388014));
#48913=CARTESIAN_POINT('Ctrl Pts',(-2.24101911263932,117.707723620513,13.7231424064524));
#48914=CARTESIAN_POINT('Ctrl Pts',(-2.24305093600475,117.709487539801,13.7091607254232));
#48915=CARTESIAN_POINT('Ctrl Pts',(-2.24508246270506,117.711251201541,13.6951810858495));
#48916=CARTESIAN_POINT('Ctrl Pts',(-2.24698368566634,117.713014425758,13.6811875019834));
#48917=CARTESIAN_POINT('Ctrl Pts',(-2.2487502882931,117.714777135929,13.6671806052955));
#48918=CARTESIAN_POINT('Ctrl Pts',(-2.26747755359704,117.733463138388,13.5186973717788));
#48919=CARTESIAN_POINT('Ctrl Pts',(-2.27107227506438,117.752091302631,13.368716862753));
#48920=CARTESIAN_POINT('Ctrl Pts',(-2.26019055608962,117.770660224938,13.220185355213));
#48921=CARTESIAN_POINT('Ctrl Pts',(-2.2490170609104,117.789727043733,13.0676712085682));
#48922=CARTESIAN_POINT('Ctrl Pts',(-2.22258075160084,117.808731399743,12.9166864938122));
#48923=CARTESIAN_POINT('Ctrl Pts',(-2.181646239744,117.827672698453,12.7704218019344));
#48924=CARTESIAN_POINT('Ctrl Pts',(-2.14379302181703,117.845188214709,12.6351670008991));
#48925=CARTESIAN_POINT('Ctrl Pts',(-2.09354304189675,117.862649821055,12.5039494152616));
#48926=CARTESIAN_POINT('Ctrl Pts',(-2.03153612752338,117.880057728102,12.3792736542313));
#48927=CARTESIAN_POINT('Ctrl Pts',(-2.02897425696137,117.880776951193,12.3741225647889));
#48928=CARTESIAN_POINT('Ctrl Pts',(-2.02639218492681,117.881496084643,12.3689824178837));
#48929=CARTESIAN_POINT('Ctrl Pts',(-2.02378995298469,117.882215127807,12.3638533940535));
#48930=CARTESIAN_POINT('Ctrl Pts',(-1.96229123084959,117.899208323168,12.2426388296426));
#48931=CARTESIAN_POINT('Ctrl Pts',(-1.88952855036872,117.916151065869,12.1276385950614));
#48932=CARTESIAN_POINT('Ctrl Pts',(-1.80723705440563,117.93303877345,12.020372574875));
#48933=CARTESIAN_POINT('Ctrl Pts',(-1.72431704050033,117.950055464312,11.9122872887671));
#48934=CARTESIAN_POINT('Ctrl Pts',(-1.6317232596914,117.967016278302,11.8120558463563));
#48935=CARTESIAN_POINT('Ctrl Pts',(-1.53127193155889,117.983916829116,11.7212014158956));
#48936=CARTESIAN_POINT('Ctrl Pts',(-1.43231274007286,118.00056633366,11.6316965666471));
#48937=CARTESIAN_POINT('Ctrl Pts',(-1.32572892005661,118.017157355224,11.5512930528403));
#48938=CARTESIAN_POINT('Ctrl Pts',(-1.21327869517553,118.033685950845,11.4814027134611));
#48939=CARTESIAN_POINT('Ctrl Pts',(-1.1846536335545,118.037893430809,11.4636115950035));
#48940=CARTESIAN_POINT('Ctrl Pts',(-1.15564849141823,118.042096866747,11.4465014632854));
#48941=CARTESIAN_POINT('Ctrl Pts',(-1.12629235719603,118.046296195893,11.4300950390516));
#48942=CARTESIAN_POINT('Ctrl Pts',(-1.01286248312528,118.062522084922,11.3667018613019));
#48943=CARTESIAN_POINT('Ctrl Pts',(-0.894193424257419,118.078686628009,
11.3138187460284));
#48944=CARTESIAN_POINT('Ctrl Pts',(-0.772389826872618,118.094772953157,
11.2719115286261));
#48945=CARTESIAN_POINT('Ctrl Pts',(-0.762313123950836,118.096103760482,
11.2684445819258));
#48946=CARTESIAN_POINT('Ctrl Pts',(-0.75221495837161,118.09743403271,11.2650527271387));
#48947=CARTESIAN_POINT('Ctrl Pts',(-0.742096515874733,118.098763760418,
11.2617362125407));
#48948=CARTESIAN_POINT('Ctrl Pts',(-0.64585072143041,118.111412021222,11.2301897979245));
#48949=CARTESIAN_POINT('Ctrl Pts',(-0.547391584981575,118.124036862978,
11.2053559596369));
#48950=CARTESIAN_POINT('Ctrl Pts',(-0.44777739688656,118.136631687336,11.1875956852635));
#48951=CARTESIAN_POINT('Ctrl Pts',(-0.367575533423394,118.146772094068,
11.1732964460928));
#48952=CARTESIAN_POINT('Ctrl Pts',(-0.286625952168628,118.156893052899,
11.1635817152682));
#48953=CARTESIAN_POINT('Ctrl Pts',(-0.205492391651079,118.166991426656,
11.1586182595621));
#48954=CARTESIAN_POINT('Ctrl Pts',(-0.103949228820018,118.179630102985,
11.1524062187277));
#48955=CARTESIAN_POINT('Ctrl Pts',(-0.0021185408589806,118.19223336774,
11.1536384272072));
#48956=CARTESIAN_POINT('Ctrl Pts',(0.0989456394163543,118.204814703464,
11.1620680830616));
#48957=CARTESIAN_POINT('Ctrl Pts',(0.200471484960796,118.21745351124,11.1705362459254));
#48958=CARTESIAN_POINT('Ctrl Pts',(0.301222672823428,118.230070208414,11.1862674062512));
#48959=CARTESIAN_POINT('Ctrl Pts',(0.400139050405618,118.242679170451,11.2089598970625));
#48960=CARTESIAN_POINT('Ctrl Pts',(0.498254479478169,118.255186034841,11.231468641591));
#48961=CARTESIAN_POINT('Ctrl Pts',(0.594563670688071,118.267685310577,11.2608260073517));
#48962=CARTESIAN_POINT('Ctrl Pts',(0.688056301876717,118.280191412531,11.2966931214302));
#48963=CARTESIAN_POINT('Ctrl Pts',(0.701543645072954,118.28199555567,11.3018673482209));
#48964=CARTESIAN_POINT('Ctrl Pts',(0.714972428772829,118.283799841202,11.3071769812151));
#48965=CARTESIAN_POINT('Ctrl Pts',(0.728339680957676,118.285604312653,11.3126209338532));
#48966=CARTESIAN_POINT('Ctrl Pts',(0.792100320495337,118.294211485774,11.3385881182095));
#48967=CARTESIAN_POINT('Ctrl Pts',(0.854460161502878,118.302822870294,11.3676117165583));
#48968=CARTESIAN_POINT('Ctrl Pts',(0.915102614013134,118.311430933557,11.3993855441404));
#48969=CARTESIAN_POINT('Ctrl Pts',(1.02395133490683,118.326881770994,11.4564172166247));
#48970=CARTESIAN_POINT('Ctrl Pts',(1.12769715551922,118.34222108742,11.5226262102829));
#48971=CARTESIAN_POINT('Ctrl Pts',(1.22457620944338,118.357466037869,11.5965368760917));
#48972=CARTESIAN_POINT('Ctrl Pts',(1.31633407816222,118.37190511531,11.6665405032484));
#48973=CARTESIAN_POINT('Ctrl Pts',(1.40193313080892,118.386259593316,11.7434537970661));
#48974=CARTESIAN_POINT('Ctrl Pts',(1.47983283887281,118.400545038101,11.8260342518042));
#48975=CARTESIAN_POINT('Ctrl Pts',(1.48467388906669,118.401432802086,11.8311661853679));
#48976=CARTESIAN_POINT('Ctrl Pts',(1.48948518746606,118.402320299667,11.8363200070697));
#48977=CARTESIAN_POINT('Ctrl Pts',(1.49426635716349,118.403207534653,11.8414954192839));
#48978=CARTESIAN_POINT('Ctrl Pts',(1.51684664234933,118.407397726654,11.8659376146352));
#48979=CARTESIAN_POINT('Ctrl Pts',(1.53875493098091,118.411582058567,11.8908613378136));
#48980=CARTESIAN_POINT('Ctrl Pts',(1.56000169303648,118.415765174845,11.916289301571));
#48981=CARTESIAN_POINT('Ctrl Pts',(1.60829237522143,118.425272766552,11.9740832239207));
#48982=CARTESIAN_POINT('Ctrl Pts',(1.65295011389502,118.434771772457,12.0341865167866));
#48983=CARTESIAN_POINT('Ctrl Pts',(1.69422527970214,118.44428774061,12.0968985325894));
#48984=CARTESIAN_POINT('Ctrl Pts',(1.73580640222509,118.453874246925,12.1600754081213));
#48985=CARTESIAN_POINT('Ctrl Pts',(1.77395426723288,118.463477888898,12.2258993614165));
#48986=CARTESIAN_POINT('Ctrl Pts',(1.80887719598704,118.47312326642,12.2947000711838));
#48987=CARTESIAN_POINT('Ctrl Pts',(1.84374351978064,118.482753010196,12.3633892650616));
#48988=CARTESIAN_POINT('Ctrl Pts',(1.87539495059614,118.492424267128,12.4350450843965));
#48989=CARTESIAN_POINT('Ctrl Pts',(1.90399723373718,118.502161258426,12.5100261594205));
#48990=CARTESIAN_POINT('Ctrl Pts',(1.92111149427981,118.507987415909,12.5548913069824));
#48991=CARTESIAN_POINT('Ctrl Pts',(1.93713331225682,118.513837108712,12.6009475989391));
#48992=CARTESIAN_POINT('Ctrl Pts',(1.95209195497482,118.519715684653,12.6482782748721));
#48993=CARTESIAN_POINT('Ctrl Pts',(2.40669191446941,114.731988374668,12.6249749337064));
#48994=CARTESIAN_POINT('Ctrl Pts',(2.43475306965379,114.74686978407,12.740863873503));
#48995=CARTESIAN_POINT('Ctrl Pts',(2.45447945011169,114.761614334258,12.8584224961112));
#48996=CARTESIAN_POINT('Ctrl Pts',(2.4658540228946,114.776289540321,12.9764721284355));
#48997=CARTESIAN_POINT('Ctrl Pts',(2.47720853484785,114.790938864373,13.0943135618579));
#48998=CARTESIAN_POINT('Ctrl Pts',(2.48024135459445,114.805519102271,13.2126454127005));
#48999=CARTESIAN_POINT('Ctrl Pts',(2.47489421501086,114.820100419095,13.3303250218578));
#49000=CARTESIAN_POINT('Ctrl Pts',(2.47094722867391,114.830863605166,13.4171901208925));
#49001=CARTESIAN_POINT('Ctrl Pts',(2.46243349325285,114.841627441902,13.5037005683707));
#49002=CARTESIAN_POINT('Ctrl Pts',(2.44931187061213,114.852421139954,13.5894013795713));
#49003=CARTESIAN_POINT('Ctrl Pts',(2.44260496807706,114.857938161957,13.6332059457928));
#49004=CARTESIAN_POINT('Ctrl Pts',(2.43469394423745,114.863462998683,13.6767990142332));
#49005=CARTESIAN_POINT('Ctrl Pts',(2.42560683986979,114.868999635026,13.7201269729547));
#49006=CARTESIAN_POINT('Ctrl Pts',(2.39853149953261,114.885496233639,13.8492241177696));
#49007=CARTESIAN_POINT('Ctrl Pts',(2.36102101525659,114.902033972754,13.9757830595316));
#49008=CARTESIAN_POINT('Ctrl Pts',(2.31383592171913,114.918519364437,14.0981944290528));
#49009=CARTESIAN_POINT('Ctrl Pts',(2.28825187124149,114.927457846092,14.1645666331131));
#49010=CARTESIAN_POINT('Ctrl Pts',(2.25982442869193,114.936380857678,14.2297190613628));
#49011=CARTESIAN_POINT('Ctrl Pts',(2.22868099465303,114.945272946841,14.2933935594758));
#49012=CARTESIAN_POINT('Ctrl Pts',(2.17167369366009,114.961549700482,14.4099481846006));
#49013=CARTESIAN_POINT('Ctrl Pts',(2.10556322161123,114.977723070201,14.5215497325451));
#49014=CARTESIAN_POINT('Ctrl Pts',(2.03135185048887,114.993695124257,14.6267674579025));
#49015=CARTESIAN_POINT('Ctrl Pts',(2.0135346205562,114.997529816371,14.6520289289861));
#49016=CARTESIAN_POINT('Ctrl Pts',(1.9952506603965,115.001352886589,14.6769224977211));
#49017=CARTESIAN_POINT('Ctrl Pts',(1.9765142564639,115.005162946815,14.7014285489423));
#49018=CARTESIAN_POINT('Ctrl Pts',(1.92537243181487,115.01556267094,14.7683188753307));
#49019=CARTESIAN_POINT('Ctrl Pts',(1.87079136938365,115.025943804624,14.8324693624242));
#49020=CARTESIAN_POINT('Ctrl Pts',(1.8130406021481,115.036309680939,14.8934653663168));
#49021=CARTESIAN_POINT('Ctrl Pts',(1.72389292042246,115.052311093331,14.9876225974991));
#49022=CARTESIAN_POINT('Ctrl Pts',(1.62719019971625,115.068276086599,15.0742607310478));
#49023=CARTESIAN_POINT('Ctrl Pts',(1.5243971463275,115.084218127803,15.1525367046183));
#49024=CARTESIAN_POINT('Ctrl Pts',(1.4350458707153,115.098075501142,15.2205768868849));
#49025=CARTESIAN_POINT('Ctrl Pts',(1.34109422436839,115.111915556258,15.2822992339472));
#49026=CARTESIAN_POINT('Ctrl Pts',(1.24352480822076,115.125747922801,15.3371743252976));
#49027=CARTESIAN_POINT('Ctrl Pts',(1.13138273130218,115.141646248055,15.4002453875024));
#49028=CARTESIAN_POINT('Ctrl Pts',(1.01446221224332,115.157534398343,15.454269788355));
#49029=CARTESIAN_POINT('Ctrl Pts',(0.894468315725866,115.173428041082,15.4983384961725));
#49030=CARTESIAN_POINT('Ctrl Pts',(0.790037839342134,115.18726025031,15.5366914148171));
#49031=CARTESIAN_POINT('Ctrl Pts',(0.68328027521778,115.201096640735,15.567504184207));
#49032=CARTESIAN_POINT('Ctrl Pts',(0.575318498023721,115.214948205653,15.5902098339972));
#49033=CARTESIAN_POINT('Ctrl Pts',(0.447210181395969,115.231384584439,15.6171525413901));
#49034=CARTESIAN_POINT('Ctrl Pts',(0.317407831723781,115.247842310195,15.6326803318094));
#49035=CARTESIAN_POINT('Ctrl Pts',(0.187703615051371,115.264340942193,15.637441971482));
#49036=CARTESIAN_POINT('Ctrl Pts',(0.174318219487164,115.26604359089,15.6379333697741));
#49037=CARTESIAN_POINT('Ctrl Pts',(0.16093384073973,115.267746676144,15.6383101435246));
#49038=CARTESIAN_POINT('Ctrl Pts',(0.147552427361176,115.269450220062,15.6385730299968));
#49039=CARTESIAN_POINT('Ctrl Pts',(0.0311432612617477,115.284269889801,
15.6408599629343));
#49040=CARTESIAN_POINT('Ctrl Pts',(-0.0854558591225894,115.298990932322,
15.63444536016));
#49041=CARTESIAN_POINT('Ctrl Pts',(-0.200909700546528,115.313627679424,
15.6196714832657));
#49042=CARTESIAN_POINT('Ctrl Pts',(-0.322521225697206,115.329045071486,
15.6041096476494));
#49043=CARTESIAN_POINT('Ctrl Pts',(-0.442860879206709,115.344368930949,
15.5792732160875));
#49044=CARTESIAN_POINT('Ctrl Pts',(-0.560365328594014,115.359617383775,
15.54562000471));
#49045=CARTESIAN_POINT('Ctrl Pts',(-0.677869777981319,115.3748658366,15.5119667933325));
#49046=CARTESIAN_POINT('Ctrl Pts',(-0.792537782828811,115.390038890025,
15.4694974322853));
#49047=CARTESIAN_POINT('Ctrl Pts',(-0.90282176453482,115.405155981277,15.4187194369708));
#49048=CARTESIAN_POINT('Ctrl Pts',(-1.00985159669809,115.419827012504,15.3694397480076));
#49049=CARTESIAN_POINT('Ctrl Pts',(-1.1127513980594,115.434445347986,15.3123352244253));
#49050=CARTESIAN_POINT('Ctrl Pts',(-1.21013698639887,115.449029833971,15.2479064194388));
#49051=CARTESIAN_POINT('Ctrl Pts',(-1.27702484761514,115.459046973992,15.2036544408889));
#49052=CARTESIAN_POINT('Ctrl Pts',(-1.34131205064833,115.469048167882,15.1559480279997));
#49053=CARTESIAN_POINT('Ctrl Pts',(-1.40256201138118,115.479039786204,15.1049574357649));
#49054=CARTESIAN_POINT('Ctrl Pts',(-1.49548743629538,115.494198577607,15.0275970196381));
#49055=CARTESIAN_POINT('Ctrl Pts',(-1.58141977934296,115.509335285618,14.9426779610095));
#49056=CARTESIAN_POINT('Ctrl Pts',(-1.65982151015904,115.524473068663,14.8517915593901));
#49057=CARTESIAN_POINT('Ctrl Pts',(-1.66477676469785,115.525429827747,14.8460472314339));
#49058=CARTESIAN_POINT('Ctrl Pts',(-1.66970195431248,115.526386591441,14.8402790662085));
#49059=CARTESIAN_POINT('Ctrl Pts',(-1.67459695039572,115.527343365718,14.8344874652654));
#49060=CARTESIAN_POINT('Ctrl Pts',(-1.7819615100526,115.548328806199,14.7074571930475));
#49061=CARTESIAN_POINT('Ctrl Pts',(-1.87516835190207,115.569125875581,14.5685630766246));
#49062=CARTESIAN_POINT('Ctrl Pts',(-1.9526207174621,115.58979491357,14.4216976039055));
#49063=CARTESIAN_POINT('Ctrl Pts',(-2.03666670163025,115.61222353311,14.2623292862853));
#49064=CARTESIAN_POINT('Ctrl Pts',(-2.10216154528806,115.634501390266,14.0935759022937));
#49065=CARTESIAN_POINT('Ctrl Pts',(-2.14710204093268,115.656709229068,13.9204632370897));
#49066=CARTESIAN_POINT('Ctrl Pts',(-2.19922267580225,115.682465212415,13.719692375866));
#49067=CARTESIAN_POINT('Ctrl Pts',(-2.22369540787726,115.708126986251,13.5130596298197));
#49068=CARTESIAN_POINT('Ctrl Pts',(-2.21745183639977,115.733825600408,13.3084479348659));
#49069=CARTESIAN_POINT('Ctrl Pts',(-2.21400458772954,115.748014516767,13.1954761532685));
#49070=CARTESIAN_POINT('Ctrl Pts',(-2.20119446652922,115.762214752214,13.0831210539546));
#49071=CARTESIAN_POINT('Ctrl Pts',(-2.17975849413663,115.776448986664,12.9725597778872));
#49072=CARTESIAN_POINT('Ctrl Pts',(-2.17197188526608,115.781619566948,12.9323984361389));
#49073=CARTESIAN_POINT('Ctrl Pts',(-2.16304771225363,115.786772238818,12.8924989800121));
#49074=CARTESIAN_POINT('Ctrl Pts',(-2.15303250877005,115.791934561425,12.8529191255056));
#49075=CARTESIAN_POINT('Ctrl Pts',(-2.14301730528641,115.797096884031,12.8133392709989));
#49076=CARTESIAN_POINT('Ctrl Pts',(-2.13191205941212,115.802268315464,12.7740833838265));
#49077=CARTESIAN_POINT('Ctrl Pts',(-2.11975235485977,115.807417983291,12.7352107449596));
#49078=CARTESIAN_POINT('Ctrl Pts',(-2.09543294575521,115.817717318945,12.6574654672262));
#49079=CARTESIAN_POINT('Ctrl Pts',(-2.06687614682154,115.827839259825,12.5812427758128));
#49080=CARTESIAN_POINT('Ctrl Pts',(-2.0344006165645,115.837933723714,12.5069067743895));
#49081=CARTESIAN_POINT('Ctrl Pts',(-1.99645086165813,115.849729756835,12.4200403548913));
#49082=CARTESIAN_POINT('Ctrl Pts',(-1.95315339155439,115.861487218842,12.3357571733488));
#49083=CARTESIAN_POINT('Ctrl Pts',(-1.90492117136718,115.873219467641,12.2546565754633));
#49084=CARTESIAN_POINT('Ctrl Pts',(-1.87060387681194,115.881566979663,12.196953382547));
#49085=CARTESIAN_POINT('Ctrl Pts',(-1.8337873100898,115.889901722998,12.1408615641731));
#49086=CARTESIAN_POINT('Ctrl Pts',(-1.79460654855197,115.898228438316,12.0866054254144));
#49087=CARTESIAN_POINT('Ctrl Pts',(-1.73617001600234,115.910647399857,12.0056845730842));
#49088=CARTESIAN_POINT('Ctrl Pts',(-1.67236145606815,115.923062979607,11.9287040403723));
#49089=CARTESIAN_POINT('Ctrl Pts',(-1.60371240566613,115.935469871571,11.8566413562907));
#49090=CARTESIAN_POINT('Ctrl Pts',(-1.53440342756294,115.947996031778,11.7838859290296));
#49091=CARTESIAN_POINT('Ctrl Pts',(-1.46016104345744,115.960513337421,11.7161444856533));
#49092=CARTESIAN_POINT('Ctrl Pts',(-1.38157990701867,115.973016628262,11.6544018915107));
#49093=CARTESIAN_POINT('Ctrl Pts',(-1.36418582545402,115.975784255082,11.6407350527857));
#49094=CARTESIAN_POINT('Ctrl Pts',(-1.34657932263432,115.978551196342,11.6273620180571));
#49095=CARTESIAN_POINT('Ctrl Pts',(-1.32876711287241,115.981317397953,11.6142932435803));
#49096=CARTESIAN_POINT('Ctrl Pts',(-1.24965483992903,115.993603380421,11.556248763571));
#49097=CARTESIAN_POINT('Ctrl Pts',(-1.166482404834,116.005874752867,11.5042098614192));
#49098=CARTESIAN_POINT('Ctrl Pts',(-1.08024451964533,116.018126996144,11.4583191342909));
#49099=CARTESIAN_POINT('Ctrl Pts',(-0.964456029554463,116.034577640152,
11.3967033143792));
#49100=CARTESIAN_POINT('Ctrl Pts',(-0.843308660808071,116.050928154555,
11.3462556953615));
#49101=CARTESIAN_POINT('Ctrl Pts',(-0.7190845582525,116.067193672212,11.3070695193659));
#49102=CARTESIAN_POINT('Ctrl Pts',(-0.692972217249571,116.070612740935,
11.2988324480638));
#49103=CARTESIAN_POINT('Ctrl Pts',(-0.666723753635358,116.074028054686,
11.2910929172646));
#49104=CARTESIAN_POINT('Ctrl Pts',(-0.64036007948357,116.077439754974,11.2838517103464));
#49105=CARTESIAN_POINT('Ctrl Pts',(-0.547244823989042,116.089489719715,
11.2582761085393));
#49106=CARTESIAN_POINT('Ctrl Pts',(-0.452690304569924,116.101495114013,
11.2389114682594));
#49107=CARTESIAN_POINT('Ctrl Pts',(-0.357495819040103,116.113469518491,
11.2257905671347));
#49108=CARTESIAN_POINT('Ctrl Pts',(-0.309101221454461,116.119557019073,
11.2191202151037));
#49109=CARTESIAN_POINT('Ctrl Pts',(-0.26054087605447,116.125636506673,11.2140643790259));
#49110=CARTESIAN_POINT('Ctrl Pts',(-0.211918517964794,116.131709742554,
11.2106326906361));
#49111=CARTESIAN_POINT('Ctrl Pts',(-0.182192770128042,116.135422673918,
11.2085346948223));
#49112=CARTESIAN_POINT('Ctrl Pts',(-0.152444447246134,116.139133192433,
11.2070436537523));
#49113=CARTESIAN_POINT('Ctrl Pts',(-0.12268249260673,116.142843534232,11.2061625355098));
#49114=CARTESIAN_POINT('Ctrl Pts',(-0.0153736119534298,116.156221440021,
11.2029855999399));
#49115=CARTESIAN_POINT('Ctrl Pts',(0.092054654109126,116.169589640168,11.2077469018766));
#49116=CARTESIAN_POINT('Ctrl Pts',(0.198244015014826,116.182937381495,11.2206306431426));
#49117=CARTESIAN_POINT('Ctrl Pts',(0.298709414128022,116.195565634912,11.2328199076539));
#49118=CARTESIAN_POINT('Ctrl Pts',(0.398064683415244,116.208175577783,11.2522792791066));
#49119=CARTESIAN_POINT('Ctrl Pts',(0.495155236231196,116.220758284055,11.2791220046775));
#49120=CARTESIAN_POINT('Ctrl Pts',(0.574891207390632,116.231091877544,11.3011666911056));
#49121=CARTESIAN_POINT('Ctrl Pts',(0.653099413496132,116.24140710442,11.328190295651));
#49122=CARTESIAN_POINT('Ctrl Pts',(0.729256505323708,116.251699113371,11.3597901748801));
#49123=CARTESIAN_POINT('Ctrl Pts',(0.787017445332149,116.259505032653,11.3837569347002));
#49124=CARTESIAN_POINT('Ctrl Pts',(0.843590323984023,116.267296436205,11.4103514048508));
#49125=CARTESIAN_POINT('Ctrl Pts',(0.898774149368019,116.275074539465,11.4394037618789));
#49126=CARTESIAN_POINT('Ctrl Pts',(1.00545542585605,116.290111155334,11.4955677286062));
#49127=CARTESIAN_POINT('Ctrl Pts',(1.10694903466504,116.305098342093,11.5609155026284));
#49128=CARTESIAN_POINT('Ctrl Pts',(1.20180118240028,116.320046286155,11.6342646596012));
#49129=CARTESIAN_POINT('Ctrl Pts',(1.23959813028786,116.326002784518,11.6634930358678));
#49130=CARTESIAN_POINT('Ctrl Pts',(1.27634022257083,116.331953049336,11.6939924640879));
#49131=CARTESIAN_POINT('Ctrl Pts',(1.31193413354399,116.33789771633,11.7256899934454));
#49132=CARTESIAN_POINT('Ctrl Pts',(1.37533506352807,116.348486533506,11.7821505729243));
#49133=CARTESIAN_POINT('Ctrl Pts',(1.43509262147617,116.35905738331,11.8424108497414));
#49134=CARTESIAN_POINT('Ctrl Pts',(1.49087120655567,116.369614516537,11.9059855018094));
#49135=CARTESIAN_POINT('Ctrl Pts',(1.56552512652914,116.383744157474,11.9910736585108));
#49136=CARTESIAN_POINT('Ctrl Pts',(1.63305359548156,116.397850559611,12.0821114610562));
#49137=CARTESIAN_POINT('Ctrl Pts',(1.69254649560885,116.411924456967,12.1778104866814));
#49138=CARTESIAN_POINT('Ctrl Pts',(1.75119310963197,116.425798153227,12.2721481943107));
#49139=CARTESIAN_POINT('Ctrl Pts',(1.80203048836647,116.439640264006,12.371014285989));
#49140=CARTESIAN_POINT('Ctrl Pts',(1.84422852407979,116.453442098142,12.4731477436492));
#49141=CARTESIAN_POINT('Ctrl Pts',(1.86792589212045,116.461192865153,12.5305033549833));
#49142=CARTESIAN_POINT('Ctrl Pts',(1.888899560676,116.468930933507,12.5888889728115));
#49143=CARTESIAN_POINT('Ctrl Pts',(1.90712464981553,116.476654791649,12.6480236031063));
#49144=CARTESIAN_POINT('Ctrl Pts',(1.91877508216826,116.481592286665,12.6858255586786));
#49145=CARTESIAN_POINT('Ctrl Pts',(1.92930298789426,116.486524097902,12.7239344528093));
#49146=CARTESIAN_POINT('Ctrl Pts',(1.93870540361382,116.491451661224,12.7622914012232));
#49147=CARTESIAN_POINT('Ctrl Pts',(1.97129883535493,116.508533037283,12.895255590131));
#49148=CARTESIAN_POINT('Ctrl Pts',(1.99036184829165,116.525559397266,13.0311693385362));
#49149=CARTESIAN_POINT('Ctrl Pts',(1.99561611600238,116.542540264114,13.1672079630254));
#49150=CARTESIAN_POINT('Ctrl Pts',(1.99819202915474,116.550865161256,13.2339011163522));
#49151=CARTESIAN_POINT('Ctrl Pts',(1.99744827903915,116.559179121435,13.3006244608754));
#49152=CARTESIAN_POINT('Ctrl Pts',(1.99334747419319,116.567483250863,13.3670451432938));
#49153=CARTESIAN_POINT('Ctrl Pts',(1.98912186126324,116.57604011665,13.4354873406152));
#49154=CARTESIAN_POINT('Ctrl Pts',(1.98133161838024,116.584586620847,13.5036088311572));
#49155=CARTESIAN_POINT('Ctrl Pts',(1.97009180727589,116.593123729406,13.5710791606626));
#49156=CARTESIAN_POINT('Ctrl Pts',(1.94788382248079,116.6099916265,13.7043892348148));
#49157=CARTESIAN_POINT('Ctrl Pts',(1.91220864772609,116.626819254494,13.8351278076438));
#49158=CARTESIAN_POINT('Ctrl Pts',(1.8640076007052,116.643599947005,13.9606342202399));
#49159=CARTESIAN_POINT('Ctrl Pts',(1.82897034182154,116.655797803775,14.0518646175336));
#49160=CARTESIAN_POINT('Ctrl Pts',(1.78731583833951,116.667970864599,14.1403303265684));
#49161=CARTESIAN_POINT('Ctrl Pts',(1.73942138132993,116.680116625926,14.2250166520074));
#49162=CARTESIAN_POINT('Ctrl Pts',(1.71068616549277,116.687403712888,14.2758258686033));
#49163=CARTESIAN_POINT('Ctrl Pts',(1.67970505922128,116.694680973931,14.3252748102773));
#49164=CARTESIAN_POINT('Ctrl Pts',(1.64664640176096,116.701947885141,14.3731997781275));
#49165=CARTESIAN_POINT('Ctrl Pts',(1.62704784448877,116.706256014583,14.4016117070846));
#49166=CARTESIAN_POINT('Ctrl Pts',(1.60671407341517,116.710561626033,14.4294954714279));
#49167=CARTESIAN_POINT('Ctrl Pts',(1.58567712235569,116.714865011729,14.4568188234608));
#49168=CARTESIAN_POINT('Ctrl Pts',(1.49913879255966,116.732567568032,14.5692171098222));
#49169=CARTESIAN_POINT('Ctrl Pts',(1.40070708779234,116.750230374466,14.672116242543));
#49170=CARTESIAN_POINT('Ctrl Pts',(1.29276196358478,116.767847645003,14.7631129897568));
#49171=CARTESIAN_POINT('Ctrl Pts',(1.24452040517771,116.775720947218,14.8037801799407));
#49172=CARTESIAN_POINT('Ctrl Pts',(1.19437936245796,116.783585156946,14.842070520652));
#49173=CARTESIAN_POINT('Ctrl Pts',(1.14255369257811,116.791439768281,14.8777718213301));
#49174=CARTESIAN_POINT('Ctrl Pts',(1.02080713973,116.809891471003,14.9616397250123));
#49175=CARTESIAN_POINT('Ctrl Pts',(0.88976316004629,116.82829019289,15.0312156933588));
#49176=CARTESIAN_POINT('Ctrl Pts',(0.753093529829106,116.846629914899,15.0852770787824));
#49177=CARTESIAN_POINT('Ctrl Pts',(0.723803194010996,116.850560390277,15.0968632382777));
#49178=CARTESIAN_POINT('Ctrl Pts',(0.694247095485108,116.854489153646,15.1077400735973));
#49179=CARTESIAN_POINT('Ctrl Pts',(0.664454578271815,116.858416983078,15.1178967007645));
#49180=CARTESIAN_POINT('Ctrl Pts',(0.555234271048197,116.872816529589,15.1551312161166));
#49181=CARTESIAN_POINT('Ctrl Pts',(0.442864032700579,116.887199572224,15.1826711409601));
#49182=CARTESIAN_POINT('Ctrl Pts',(0.329150962525186,116.901558454711,15.1998707026059));
#49183=CARTESIAN_POINT('Ctrl Pts',(0.214068667916537,116.916090233179,15.2172773649835));
#49184=CARTESIAN_POINT('Ctrl Pts',(0.0976124776931342,116.930597266838,
15.2240926615264));
#49185=CARTESIAN_POINT('Ctrl Pts',(-0.0182859125916594,116.945071164092,
15.2205350884505));
#49186=CARTESIAN_POINT('Ctrl Pts',(-0.10604441062489,116.956030828679,15.2178412868452));
#49187=CARTESIAN_POINT('Ctrl Pts',(-0.193482669233001,116.966971497382,
15.2092012674747));
#49188=CARTESIAN_POINT('Ctrl Pts',(-0.279765449072471,116.977889579526,
15.194729438234));
#49189=CARTESIAN_POINT('Ctrl Pts',(-0.312106818934253,116.981982003686,
15.1893049632354));
#49190=CARTESIAN_POINT('Ctrl Pts',(-0.344285911746652,116.986071254933,
15.1830612987958));
#49191=CARTESIAN_POINT('Ctrl Pts',(-0.376259037902826,116.990157145737,
15.1760050562577));
#49192=CARTESIAN_POINT('Ctrl Pts',(-0.410203973017803,116.994495016783,
15.168513649445));
#49193=CARTESIAN_POINT('Ctrl Pts',(-0.443924325172075,116.998830061935,
15.1601048276074));
#49194=CARTESIAN_POINT('Ctrl Pts',(-0.477375487000464,117.003163074823,
15.1507830465092));
#49195=CARTESIAN_POINT('Ctrl Pts',(-0.49647583620284,117.00563719096,15.1454603831268));
#49196=CARTESIAN_POINT('Ctrl Pts',(-0.515487839346988,117.008110570362,
15.1398401905004));
#49197=CARTESIAN_POINT('Ctrl Pts',(-0.53440213830564,117.010583227121,15.1339235123191));
#49198=CARTESIAN_POINT('Ctrl Pts',(-0.686067213261841,117.030410325846,
15.0864803878435));
#49199=CARTESIAN_POINT('Ctrl Pts',(-0.831453110605257,117.050190967813,
15.019976503841));
#49200=CARTESIAN_POINT('Ctrl Pts',(-0.966310415421474,117.06993608109,14.9370403466912));
#49201=CARTESIAN_POINT('Ctrl Pts',(-1.07727880405652,117.086183502073,14.8687956807383));
#49202=CARTESIAN_POINT('Ctrl Pts',(-1.1811182709215,117.102406864446,14.7894239141178));
#49203=CARTESIAN_POINT('Ctrl Pts',(-1.27543669211679,117.118612221601,14.7003788828808));
#49204=CARTESIAN_POINT('Ctrl Pts',(-1.31684386356554,117.125726611278,14.6612868070343));
#49205=CARTESIAN_POINT('Ctrl Pts',(-1.35641786923958,117.132837965838,14.6203275917402));
#49206=CARTESIAN_POINT('Ctrl Pts',(-1.39404208976212,117.139944780179,14.577698052834));
#49207=CARTESIAN_POINT('Ctrl Pts',(-1.46607112697874,117.153550297783,14.4960866705447));
#49208=CARTESIAN_POINT('Ctrl Pts',(-1.53094642551177,117.167138236835,14.4083575652026));
#49209=CARTESIAN_POINT('Ctrl Pts',(-1.58788514907687,117.180698432732,14.3159193029345));
#49210=CARTESIAN_POINT('Ctrl Pts',(-1.62663012303909,117.189925710832,14.2530180322273));
#49211=CARTESIAN_POINT('Ctrl Pts',(-1.66170150186151,117.199140305292,14.1879358397825));
#49212=CARTESIAN_POINT('Ctrl Pts',(-1.69286357661844,117.208338477689,14.1211260289112));
#49213=CARTESIAN_POINT('Ctrl Pts',(-1.71258060781417,117.214158393517,14.0788537753657));
#49214=CARTESIAN_POINT('Ctrl Pts',(-1.73073361608754,117.219971866751,14.0358891527244));
#49215=CARTESIAN_POINT('Ctrl Pts',(-1.7472697287625,117.225779773835,13.9923333288776));
#49216=CARTESIAN_POINT('Ctrl Pts',(-1.77386070669752,117.235119207604,13.9222931704911));
#49217=CARTESIAN_POINT('Ctrl Pts',(-1.79627143159348,117.244444051522,13.8507261726921));
#49218=CARTESIAN_POINT('Ctrl Pts',(-1.81438776136439,117.253761733308,13.7781403018514));
#49219=CARTESIAN_POINT('Ctrl Pts',(-1.8233312033563,117.258361569346,13.7423070214075));
#49220=CARTESIAN_POINT('Ctrl Pts',(-1.8312276588904,117.262959563972,13.7062260685609));
#49221=CARTESIAN_POINT('Ctrl Pts',(-1.83806222368246,117.267557219643,13.6699532356282));
#49222=CARTESIAN_POINT('Ctrl Pts',(-1.84085659153172,117.269437008859,13.6551227904965));
#49223=CARTESIAN_POINT('Ctrl Pts',(-1.84347304444535,117.271316482654,13.6402623089836));
#49224=CARTESIAN_POINT('Ctrl Pts',(-1.84591075327413,117.273195889375,13.6253744577075));
#49225=CARTESIAN_POINT('Ctrl Pts',(-1.85971572148554,117.283839141649,13.5410631933034));
#49226=CARTESIAN_POINT('Ctrl Pts',(-1.8678047482461,117.294492742878,13.4557528112906));
#49227=CARTESIAN_POINT('Ctrl Pts',(-1.86992137198423,117.305136545796,13.3703636749658));
#49228=CARTESIAN_POINT('Ctrl Pts',(-1.87170907388779,117.314126309256,13.2982439501414));
#49229=CARTESIAN_POINT('Ctrl Pts',(-1.86923710776832,117.323109093235,13.2260688838612));
#49230=CARTESIAN_POINT('Ctrl Pts',(-1.86237967622628,117.332073054458,13.1543969176522));
#49231=CARTESIAN_POINT('Ctrl Pts',(-1.85423887153773,117.342714627341,13.0693114924497));
#49232=CARTESIAN_POINT('Ctrl Pts',(-1.83991647495421,117.353329659416,12.9849362386533));
#49233=CARTESIAN_POINT('Ctrl Pts',(-1.81989415050543,117.363895185557,12.9020346284525));
#49234=CARTESIAN_POINT('Ctrl Pts',(-1.79972072205488,117.374540447359,12.8185073783523));
#49235=CARTESIAN_POINT('Ctrl Pts',(-1.77376174147136,117.385135449304,12.7364771470377));
#49236=CARTESIAN_POINT('Ctrl Pts',(-1.74255499710192,117.395657275435,12.6566988894436));
#49237=CARTESIAN_POINT('Ctrl Pts',(-1.7268372303829,117.400956758349,12.6165173175606));
#49238=CARTESIAN_POINT('Ctrl Pts',(-1.70978885588439,117.406237687464,12.5769065173321));
#49239=CARTESIAN_POINT('Ctrl Pts',(-1.69148196311947,117.411497193792,12.5379592168163));
#49240=CARTESIAN_POINT('Ctrl Pts',(-1.64422641244845,117.425073548391,12.4374246172718));
#49241=CARTESIAN_POINT('Ctrl Pts',(-1.58820047488711,117.438900237672,12.3410139841719));
#49242=CARTESIAN_POINT('Ctrl Pts',(-1.52439771598195,117.452848649161,12.2501830196273));
#49243=CARTESIAN_POINT('Ctrl Pts',(-1.46217654483511,117.466451297593,12.161603637053));
#49244=CARTESIAN_POINT('Ctrl Pts',(-1.39255982919765,117.480169700269,12.0783289541421));
#49245=CARTESIAN_POINT('Ctrl Pts',(-1.3164220316241,117.493891230108,12.001703326054));
#49246=CARTESIAN_POINT('Ctrl Pts',(-1.24771768854726,117.506273105126,11.9325587801331));
#49247=CARTESIAN_POINT('Ctrl Pts',(-1.17370317273219,117.518657587153,11.8688270140121));
#49248=CARTESIAN_POINT('Ctrl Pts',(-1.09498183832174,117.530966906991,11.811512383697));
#49249=CARTESIAN_POINT('Ctrl Pts',(-1.06858713662752,117.535094134097,11.7922951971337));
#49250=CARTESIAN_POINT('Ctrl Pts',(-1.04166295250224,117.539212952506,11.7737996665922));
#49251=CARTESIAN_POINT('Ctrl Pts',(-1.01423097499657,117.543320558148,11.7560645295145));
#49252=CARTESIAN_POINT('Ctrl Pts',(-0.998041927346321,117.545744671519,
11.7455980956172));
#49253=CARTESIAN_POINT('Ctrl Pts',(-0.981676013135029,117.548164880914,
11.7353965049393));
#49254=CARTESIAN_POINT('Ctrl Pts',(-0.965141588692916,117.550580691203,
11.7254609363924));
#49255=CARTESIAN_POINT('Ctrl Pts',(-0.885330420180348,117.562241734668,
11.6775022464278));
#49256=CARTESIAN_POINT('Ctrl Pts',(-0.801863080831363,117.573695835655,
11.6358450243134));
#49257=CARTESIAN_POINT('Ctrl Pts',(-0.715805975492523,117.585061449866,
11.6006923062261));
#49258=CARTESIAN_POINT('Ctrl Pts',(-0.631194966603208,117.59623607724,11.5661302914936));
#49259=CARTESIAN_POINT('Ctrl Pts',(-0.544080928567308,117.607325181313,
11.5378571908184));
#49260=CARTESIAN_POINT('Ctrl Pts',(-0.455522731807488,117.618434684624,
11.516046342729));
#49261=CARTESIAN_POINT('Ctrl Pts',(-0.366964535047849,117.629544187936,
11.4942354946396));
#49262=CARTESIAN_POINT('Ctrl Pts',(-0.276962930050188,117.64067411174,11.4788882325044));
#49263=CARTESIAN_POINT('Ctrl Pts',(-0.186613838556208,117.651923366021,
11.470139291332));
#49264=CARTESIAN_POINT('Ctrl Pts',(-0.108075132966351,117.661702123676,
11.4625340071659));
#49265=CARTESIAN_POINT('Ctrl Pts',(-0.0291274892094371,117.671636391611,
11.4599362158693));
#49266=CARTESIAN_POINT('Ctrl Pts',(0.0496472966318842,117.681644743467,
11.4623331568941));
#49267=CARTESIAN_POINT('Ctrl Pts',(0.127204302154861,117.691498376097,11.46469304358));
#49268=CARTESIAN_POINT('Ctrl Pts',(0.204594489606238,117.701423817813,11.4718936477988));
#49269=CARTESIAN_POINT('Ctrl Pts',(0.281300662862718,117.711348164116,11.4839540427299));
#49270=CARTESIAN_POINT('Ctrl Pts',(0.356745070184129,117.72110926147,11.4958160521226));
#49271=CARTESIAN_POINT('Ctrl Pts',(0.431528619424435,117.730869298819,11.5123785167616));
#49272=CARTESIAN_POINT('Ctrl Pts',(0.505184687685248,117.740563609283,11.5337014305304));
#49273=CARTESIAN_POINT('Ctrl Pts',(0.535928413375962,117.744609972722,11.54260152291));
#49274=CARTESIAN_POINT('Ctrl Pts',(0.566475946798625,117.748644942287,11.5523315502387));
#49275=CARTESIAN_POINT('Ctrl Pts',(0.59679413335784,117.752664064104,11.5628985939744));
#49276=CARTESIAN_POINT('Ctrl Pts',(0.60532443654273,117.75379488133,11.5658717298068));
#49277=CARTESIAN_POINT('Ctrl Pts',(0.613836585694016,117.754924444915,11.5689111375289));
#49278=CARTESIAN_POINT('Ctrl Pts',(0.622329766038321,117.756052622435,11.572015885102));
#49279=CARTESIAN_POINT('Ctrl Pts',(0.718273749250566,117.768797182265,11.6070889480715));
#49280=CARTESIAN_POINT('Ctrl Pts',(0.811526709167048,117.781580106972,11.6506547523446));
#49281=CARTESIAN_POINT('Ctrl Pts',(0.900544082088829,117.794340444296,11.7012952481804));
#49282=CARTESIAN_POINT('Ctrl Pts',(0.99543471658107,117.807942693669,11.7552769443722));
#49283=CARTESIAN_POINT('Ctrl Pts',(1.08551068967412,117.821519213535,11.8172964829959));
#49284=CARTESIAN_POINT('Ctrl Pts',(1.16892107576438,117.834996948096,11.8855815030142));
#49285=CARTESIAN_POINT('Ctrl Pts',(1.21514949032297,117.842466692931,11.9234270083705));
#49286=CARTESIAN_POINT('Ctrl Pts',(1.25933094458218,117.849906112872,11.9631962343358));
#49287=CARTESIAN_POINT('Ctrl Pts',(1.30115581020482,117.85730298323,12.0045832583054));
#49288=CARTESIAN_POINT('Ctrl Pts',(1.30433811149824,117.857865784084,12.0077322458263));
#49289=CARTESIAN_POINT('Ctrl Pts',(1.30750677256674,117.858428338708,12.0108905981791));
#49290=CARTESIAN_POINT('Ctrl Pts',(1.31066183021349,117.858990661359,12.0140584282958));
#49291=CARTESIAN_POINT('Ctrl Pts',(1.39218015888058,117.873519588495,12.0959067637396));
#49292=CARTESIAN_POINT('Ctrl Pts',(1.46448549790502,117.888027757926,12.1841610834581));
#49293=CARTESIAN_POINT('Ctrl Pts',(1.52832261184637,117.902711711588,12.2807762477784));
#49294=CARTESIAN_POINT('Ctrl Pts',(1.58626948775732,117.916040779715,12.3684767497641));
#49295=CARTESIAN_POINT('Ctrl Pts',(1.63723974859756,117.929514685645,12.4630655608177));
#49296=CARTESIAN_POINT('Ctrl Pts',(1.68180326677914,117.943285624186,12.5660476116433));
#49297=CARTESIAN_POINT('Ctrl Pts',(1.70234791144629,117.94963429347,12.613524330889));
#49298=CARTESIAN_POINT('Ctrl Pts',(1.72153097871086,117.956046170297,12.6627856374267));
#49299=CARTESIAN_POINT('Ctrl Pts',(1.73940833428493,117.962536543046,12.7139827773687));
#49300=CARTESIAN_POINT('Ctrl Pts',(1.89901808267227,22.3854922851854,13.1430245619172));
#49301=CARTESIAN_POINT('Ctrl Pts',(1.91613969489008,22.4388279619656,13.5964108599035));
#49302=CARTESIAN_POINT('Ctrl Pts',(1.71821761744411,22.5298182997524,14.3052845584749));
#49303=CARTESIAN_POINT('Ctrl Pts',(0.851232992570897,22.6680906574048,15.079778475839));
#49304=CARTESIAN_POINT('Ctrl Pts',(-0.20609293949006,22.7963599803505,15.2366541763624));
#49305=CARTESIAN_POINT('Ctrl Pts',(-1.31284734837634,22.9401313869705,14.7857986719247));
#49306=CARTESIAN_POINT('Ctrl Pts',(-1.98673499945204,23.0964011152393,13.6207000133225));
#49307=CARTESIAN_POINT('Ctrl Pts',(-1.72784747405538,23.2386153490056,12.4321198834099));
#49308=CARTESIAN_POINT('Ctrl Pts',(-1.16168516194224,23.3380220181386,11.849943041944));
#49309=CARTESIAN_POINT('Ctrl Pts',(-0.815536846787828,23.3878154581211,
11.6489769798242));
#49310=CARTESIAN_POINT('Ctrl Pts',(-0.603916967857474,23.4162803789959,
11.5630510794694));
#49311=CARTESIAN_POINT('Ctrl Pts',(-0.0574765629675266,23.4874854098496,
11.3968778460358));
#49312=CARTESIAN_POINT('Ctrl Pts',(0.97493037193895,23.6087644299663,11.523756852127));
#49313=CARTESIAN_POINT('Ctrl Pts',(1.94094774955337,23.7812659840327,12.6445967993243));
#49314=CARTESIAN_POINT('Ctrl Pts',(1.89788000011945,23.9555004545731,14.1415343184278));
#49315=CARTESIAN_POINT('Ctrl Pts',(1.01652133303839,24.1026054592893,15.0447532345077));
#49316=CARTESIAN_POINT('Ctrl Pts',(0.0737468811550872,24.2216732044994,
15.2763220602092));
#49317=CARTESIAN_POINT('Ctrl Pts',(-0.898370169248287,24.3417518600375,
15.156344869436));
#49318=CARTESIAN_POINT('Ctrl Pts',(-1.70997761919059,24.4634436928123,14.5022214873614));
#49319=CARTESIAN_POINT('Ctrl Pts',(-2.03808699269719,24.5869882902184,13.5494030506149));
#49320=CARTESIAN_POINT('Ctrl Pts',(-2.00577746566736,24.7118373079241,12.5318452734765));
#49321=CARTESIAN_POINT('Ctrl Pts',(-1.45608643562398,24.8281603678822,11.7018449784035));
#49322=CARTESIAN_POINT('Ctrl Pts',(-0.534872821177135,24.9570582485252,
11.2162952702369));
#49323=CARTESIAN_POINT('Ctrl Pts',(0.534301246424838,25.0874961960025,11.0852460992961));
#49324=CARTESIAN_POINT('Ctrl Pts',(1.49649042191416,25.2150609213097,11.604772215406));
#49325=CARTESIAN_POINT('Ctrl Pts',(1.96187327074999,25.3165078617568,12.2763104036369));
#49326=CARTESIAN_POINT('Ctrl Pts',(2.18730068378442,25.3845718318905,12.7752090509047));
#49327=CARTESIAN_POINT('Ctrl Pts',(2.28997050485051,25.4704763225682,13.4681040828783));
#49328=CARTESIAN_POINT('Ctrl Pts',(2.13265524663939,25.5575042190843,14.1597458020817));
#49329=CARTESIAN_POINT('Ctrl Pts',(1.89449930397993,25.6190258395685,14.5938340517913));
#49330=CARTESIAN_POINT('Ctrl Pts',(1.725122197418,25.654354604935,14.8209950885772));
#49331=CARTESIAN_POINT('Ctrl Pts',(1.34494084944462,25.7252462124837,15.2438421767498));
#49332=CARTESIAN_POINT('Ctrl Pts',(0.501632786354249,25.841769628763,15.7232686865407));
#49333=CARTESIAN_POINT('Ctrl Pts',(-0.867995626280332,26.0063411933124,
15.6711561235961));
#49334=CARTESIAN_POINT('Ctrl Pts',(-2.07840568160389,26.181656386924,14.8548222868116));
#49335=CARTESIAN_POINT('Ctrl Pts',(-2.46671766690266,26.3035423891514,13.90616329438));
#49336=CARTESIAN_POINT('Ctrl Pts',(-2.50116807429277,26.3690142660915,13.3823003528019));
#49337=CARTESIAN_POINT('Ctrl Pts',(1.89745606312038,22.1838751864406,13.1425059908936));
#49338=CARTESIAN_POINT('Ctrl Pts',(1.91889546766375,22.2371618336946,13.5972022198302));
#49339=CARTESIAN_POINT('Ctrl Pts',(1.73104184020844,22.3284542101753,14.3110046545806));
#49340=CARTESIAN_POINT('Ctrl Pts',(0.86568005728612,22.4681490366909,15.1044063130677));
#49341=CARTESIAN_POINT('Ctrl Pts',(-0.208364405618377,22.5987783158082,
15.2797778720042));
#49342=CARTESIAN_POINT('Ctrl Pts',(-1.34875877659589,22.7461331969493,14.8331662634924));
#49343=CARTESIAN_POINT('Ctrl Pts',(-2.06307172611114,22.907673614335,13.6398788074659));
#49344=CARTESIAN_POINT('Ctrl Pts',(-1.81136828346712,23.0559625763966,12.3966281499362));
#49345=CARTESIAN_POINT('Ctrl Pts',(-1.22573074374783,23.1602868256609,11.7777180850658));
#49346=CARTESIAN_POINT('Ctrl Pts',(-0.864316318410229,23.2126975916322,
11.5613857654943));
#49347=CARTESIAN_POINT('Ctrl Pts',(-0.642511578839508,23.2427032710701,
11.4678676191461));
#49348=CARTESIAN_POINT('Ctrl Pts',(-0.0684751251893176,23.3178339145423,
11.2849180188622));
#49349=CARTESIAN_POINT('Ctrl Pts',(1.02727112385617,23.4463590679339,11.4033876706341));
#49350=CARTESIAN_POINT('Ctrl Pts',(2.07500014479947,23.6304250145684,12.5840481667664));
#49351=CARTESIAN_POINT('Ctrl Pts',(2.05172154059502,23.8174703500441,14.1912761391829));
#49352=CARTESIAN_POINT('Ctrl Pts',(1.11445288131786,23.976195483412,15.1788657585492));
#49353=CARTESIAN_POINT('Ctrl Pts',(0.0975471875992922,24.1050695693536,
15.442820271682));
#49354=CARTESIAN_POINT('Ctrl Pts',(-0.957915377985352,24.2352719613535,
15.3264954005426));
#49355=CARTESIAN_POINT('Ctrl Pts',(-1.84913680784375,24.3675342639,14.6273375566598));
#49356=CARTESIAN_POINT('Ctrl Pts',(-2.21930990799663,24.5020294856332,13.5947971624621));
#49357=CARTESIAN_POINT('Ctrl Pts',(-2.19793297618546,24.6380579027441,12.4859601647338));
#49358=CARTESIAN_POINT('Ctrl Pts',(-1.60976628295625,24.7649137460929,11.5736243555951));
#49359=CARTESIAN_POINT('Ctrl Pts',(-0.611501641164774,24.9055128600071,
11.0320566514164));
#49360=CARTESIAN_POINT('Ctrl Pts',(0.552802652311208,25.047791884706,10.8753244014993));
#49361=CARTESIAN_POINT('Ctrl Pts',(1.60824932137011,25.186880522897,11.4296603515728));
#49362=CARTESIAN_POINT('Ctrl Pts',(2.12347369309861,25.2973992201485,12.1553207266224));
#49363=CARTESIAN_POINT('Ctrl Pts',(2.3750851755453,25.3715225705239,12.6957361107479));
#49364=CARTESIAN_POINT('Ctrl Pts',(2.49521255144033,25.4650159651105,13.4484599298977));
#49365=CARTESIAN_POINT('Ctrl Pts',(2.33247101541913,25.5596369978143,14.2021831444921));
#49366=CARTESIAN_POINT('Ctrl Pts',(2.07897058752978,25.6264683921513,14.6764770325329));
#49367=CARTESIAN_POINT('Ctrl Pts',(1.89778840277349,25.6648284026719,14.9250865509826));
#49368=CARTESIAN_POINT('Ctrl Pts',(1.49019255835625,25.7417767105877,15.3884618689839));
#49369=CARTESIAN_POINT('Ctrl Pts',(0.581448415540573,25.8681129363819,15.9177505457125));
#49370=CARTESIAN_POINT('Ctrl Pts',(-0.900453073796818,26.0461313544131,
15.8764698702819));
#49371=CARTESIAN_POINT('Ctrl Pts',(-2.21491668089787,26.2352800753748,15.0088027917896));
#49372=CARTESIAN_POINT('Ctrl Pts',(-2.64230284098423,26.3663838566027,13.9924904480118));
#49373=CARTESIAN_POINT('Ctrl Pts',(-2.68486387351535,26.4366806810332,13.4305008334684));
#49374=CARTESIAN_POINT('Ctrl Pts',(1.89589404356848,21.9822580876958,13.14198741987));
#49375=CARTESIAN_POINT('Ctrl Pts',(1.92165124043742,22.0354957054235,13.5979935797571));
#49376=CARTESIAN_POINT('Ctrl Pts',(1.74386606297277,22.1270901205983,14.316724750686));
#49377=CARTESIAN_POINT('Ctrl Pts',(0.880127122001338,22.2682074159771,15.1290341502964));
#49378=CARTESIAN_POINT('Ctrl Pts',(-0.210635871746706,22.4011966512656,
15.322901567646));
#49379=CARTESIAN_POINT('Ctrl Pts',(-1.38467020481544,22.552135006928,14.8805338550601));
#49380=CARTESIAN_POINT('Ctrl Pts',(-2.13940845277027,22.7189461134307,13.6590576016092));
#49381=CARTESIAN_POINT('Ctrl Pts',(-1.89488909287888,22.8733098037875,12.3611364164627));
#49382=CARTESIAN_POINT('Ctrl Pts',(-1.28977632555346,22.9825516331833,11.7054931281874));
#49383=CARTESIAN_POINT('Ctrl Pts',(-0.913095790032648,23.0375797251433,
11.4737945511643));
#49384=CARTESIAN_POINT('Ctrl Pts',(-0.681106189821558,23.0691261631444,
11.372684158823));
#49385=CARTESIAN_POINT('Ctrl Pts',(-0.0794736874111196,23.1481824192349,
11.1729581916887));
#49386=CARTESIAN_POINT('Ctrl Pts',(1.07961187577341,23.2839537059015,11.2830184891413));
#49387=CARTESIAN_POINT('Ctrl Pts',(2.20905254004556,23.4795840451043,12.5234995342084));
#49388=CARTESIAN_POINT('Ctrl Pts',(2.20556308107057,23.6794402455151,14.241017959938));
#49389=CARTESIAN_POINT('Ctrl Pts',(1.21238442959733,23.849785507535,15.3129782825907));
#49390=CARTESIAN_POINT('Ctrl Pts',(0.12134749404349,23.9884659342077,15.6093184831547));
#49391=CARTESIAN_POINT('Ctrl Pts',(-1.01746058672243,24.1287920626696,15.4966459316494));
#49392=CARTESIAN_POINT('Ctrl Pts',(-1.98829599649688,24.2716248349878,14.7524536259582));
#49393=CARTESIAN_POINT('Ctrl Pts',(-2.40053282329608,24.4170706810479,13.6401912743091));
#49394=CARTESIAN_POINT('Ctrl Pts',(-2.39008848670359,24.5642784975641,12.4400750559912));
#49395=CARTESIAN_POINT('Ctrl Pts',(-1.76344613028854,24.7016671243036,11.4454037327865));
#49396=CARTESIAN_POINT('Ctrl Pts',(-0.68813046115242,24.8539674714891,10.847818032596));
#49397=CARTESIAN_POINT('Ctrl Pts',(0.571304058197572,25.0080875734096,10.6654027037025));
#49398=CARTESIAN_POINT('Ctrl Pts',(1.72000822082606,25.1587001244841,11.2545484877396));
#49399=CARTESIAN_POINT('Ctrl Pts',(2.28507411544722,25.2782905785403,12.0343310496079));
#49400=CARTESIAN_POINT('Ctrl Pts',(2.56286966730619,25.3584733091573,12.6162631705913));
#49401=CARTESIAN_POINT('Ctrl Pts',(2.70045459803015,25.4595556076531,13.428815776917));
#49402=CARTESIAN_POINT('Ctrl Pts',(2.53228678419889,25.5617697765442,14.2446204869025));
#49403=CARTESIAN_POINT('Ctrl Pts',(2.26344187107965,25.6339109447338,14.7591200132746));
#49404=CARTESIAN_POINT('Ctrl Pts',(2.070454608129,25.6753022004089,15.0291780133881));
#49405=CARTESIAN_POINT('Ctrl Pts',(1.63544426726789,25.758307208692,15.533081561218));
#49406=CARTESIAN_POINT('Ctrl Pts',(0.661264044726898,25.8944562440005,16.1122324048843));
#49407=CARTESIAN_POINT('Ctrl Pts',(-0.932910521313303,26.0859215155139,
16.0817836169678));
#49408=CARTESIAN_POINT('Ctrl Pts',(-2.35142768019183,26.2889037638257,15.1627832967678));
#49409=CARTESIAN_POINT('Ctrl Pts',(-2.8178880150658,26.4292253240541,14.0788176016433));
#49410=CARTESIAN_POINT('Ctrl Pts',(-2.86855967273795,26.5043470959747,13.4787013141351));
#49411=CARTESIAN_POINT('Ctrl Pts',(1.89433202401659,21.780640988951,13.1414688488465));
#49412=CARTESIAN_POINT('Ctrl Pts',(1.9244070132111,21.8338295771525,13.5987849396839));
#49413=CARTESIAN_POINT('Ctrl Pts',(1.75669028573709,21.9257260310212,14.3224448467915));
#49414=CARTESIAN_POINT('Ctrl Pts',(0.894574186716559,22.0682657952632,15.1536619875252));
#49415=CARTESIAN_POINT('Ctrl Pts',(-0.212907337875024,22.2036149867232,
15.3660252632878));
#49416=CARTESIAN_POINT('Ctrl Pts',(-1.42058163303499,22.3581368169068,14.9279014466279));
#49417=CARTESIAN_POINT('Ctrl Pts',(-2.21574517942938,22.5302186125265,13.6782363957527));
#49418=CARTESIAN_POINT('Ctrl Pts',(-1.97840990229062,22.6906570311784,12.3256446829891));
#49419=CARTESIAN_POINT('Ctrl Pts',(-1.35382190735905,22.8048164407056,11.6332681713093));
#49420=CARTESIAN_POINT('Ctrl Pts',(-0.961875261655053,22.8624618586543,
11.3862033368344));
#49421=CARTESIAN_POINT('Ctrl Pts',(-0.719700800803596,22.8955490552187,
11.2775006984997));
#49422=CARTESIAN_POINT('Ctrl Pts',(-0.0904722496329132,22.9785309239276,
11.0609983645151));
#49423=CARTESIAN_POINT('Ctrl Pts',(1.13195262769064,23.1215483438691,11.1626493076482));
#49424=CARTESIAN_POINT('Ctrl Pts',(2.34310493529166,23.3287430756401,12.4629509016504));
#49425=CARTESIAN_POINT('Ctrl Pts',(2.35940462154613,23.5414101409862,14.290759780693));
#49426=CARTESIAN_POINT('Ctrl Pts',(1.31031597787682,23.7233755316578,15.4470908066323));
#49427=CARTESIAN_POINT('Ctrl Pts',(0.145147800487696,23.8718622990619,15.7758166946274));
#49428=CARTESIAN_POINT('Ctrl Pts',(-1.07700579545949,24.0223121639856,15.666796462756));
#49429=CARTESIAN_POINT('Ctrl Pts',(-2.12745518515003,24.1757154060755,14.8775696952566));
#49430=CARTESIAN_POINT('Ctrl Pts',(-2.58175573859553,24.3321118764628,13.6855853861563));
#49431=CARTESIAN_POINT('Ctrl Pts',(-2.58224399722169,24.4904990923843,12.3941899472485));
#49432=CARTESIAN_POINT('Ctrl Pts',(-1.91712597762081,24.6384205025145,11.317183109978));
#49433=CARTESIAN_POINT('Ctrl Pts',(-0.764759281140061,24.8024220829711,
10.6635794137756));
#49434=CARTESIAN_POINT('Ctrl Pts',(0.589805464083942,24.9683832621133,10.4554810059057));
#49435=CARTESIAN_POINT('Ctrl Pts',(1.831767120282,25.1305197260712,11.0794366239064));
#49436=CARTESIAN_POINT('Ctrl Pts',(2.44667453779583,25.259181936932,11.9133413725934));
#49437=CARTESIAN_POINT('Ctrl Pts',(2.75065415906708,25.3454240477907,12.5367902304347));
#49438=CARTESIAN_POINT('Ctrl Pts',(2.90569664461998,25.4540952501954,13.4091716239364));
#49439=CARTESIAN_POINT('Ctrl Pts',(2.73210255297864,25.5639025552742,14.287057829313));
#49440=CARTESIAN_POINT('Ctrl Pts',(2.44791315462951,25.6413534973164,14.8417629940163));
#49441=CARTESIAN_POINT('Ctrl Pts',(2.2431208134845,25.6857759981459,15.1332694757937));
#49442=CARTESIAN_POINT('Ctrl Pts',(1.78069597617953,25.7748377067961,15.677701253452));
#49443=CARTESIAN_POINT('Ctrl Pts',(0.74107967391322,25.9207995516194,16.3067142640562));
#49444=CARTESIAN_POINT('Ctrl Pts',(-0.96536796882979,26.1257116766147,16.2870973636537));
#49445=CARTESIAN_POINT('Ctrl Pts',(-2.48793867948582,26.3425274522765,15.3167638017459));
#49446=CARTESIAN_POINT('Ctrl Pts',(-2.99347318914736,26.4920667915054,14.165144755275));
#49447=CARTESIAN_POINT('Ctrl Pts',(-3.05225547196054,26.5720135109164,13.5269017948015));
#49448=CARTESIAN_POINT('',(1.9,21.8,13.3));
#49449=CARTESIAN_POINT('Ctrl Pts',(1.90000000000001,21.8,13.3));
#49450=CARTESIAN_POINT('Ctrl Pts',(1.90034617523604,21.8090010354302,13.3759055909997));
#49451=CARTESIAN_POINT('Ctrl Pts',(1.89706050239537,21.8178848211233,13.4497039057687));
#49452=CARTESIAN_POINT('Ctrl Pts',(1.89024211642034,21.8266870935422,13.5215832394767));
#49453=CARTESIAN_POINT('Ctrl Pts',(1.88321809876848,21.8357548284979,13.5956303395703));
#49454=CARTESIAN_POINT('Ctrl Pts',(1.87244522789137,21.8447360075938,13.6676409355473));
#49455=CARTESIAN_POINT('Ctrl Pts',(1.8579806294168,21.8536683860142,13.7377960259859));
#49456=CARTESIAN_POINT('Ctrl Pts',(1.84367989488745,21.8624995729102,13.8071563560364));
#49457=CARTESIAN_POINT('Ctrl Pts',(1.82577044097264,21.8712830015836,13.874702816309));
#49458=CARTESIAN_POINT('Ctrl Pts',(1.80425871233331,21.8800547258861,13.9405881368359));
#49459=CARTESIAN_POINT('Ctrl Pts',(1.78237724778465,21.8889772154532,14.0076058707222));
#49460=CARTESIAN_POINT('Ctrl Pts',(1.75676871234439,21.897887536015,14.0729048292138));
#49461=CARTESIAN_POINT('Ctrl Pts',(1.72738931112095,21.9068240537372,14.1366241000423));
#49462=CARTESIAN_POINT('Ctrl Pts',(1.69800990989751,21.9157605714594,14.2003433708709));
#49463=CARTESIAN_POINT('Ctrl Pts',(1.66485962352026,21.9247232267287,14.2624828718383));
#49464=CARTESIAN_POINT('Ctrl Pts',(1.62784413803072,21.9337516952225,14.323161258052));
#49465=CARTESIAN_POINT('Ctrl Pts',(1.60707419358073,21.9388177043969,14.3572088112396));
#49466=CARTESIAN_POINT('Ctrl Pts',(1.58518200176035,21.9438793654298,14.3907313388816));
#49467=CARTESIAN_POINT('Ctrl Pts',(1.56216457238228,21.9489444761508,14.4237311549527));
#49468=CARTESIAN_POINT('Ctrl Pts',(1.51717383901757,21.9588449321126,14.4882338368792));
#49469=CARTESIAN_POINT('Ctrl Pts',(1.4678811340779,21.9687589700013,14.5507411453126));
#49470=CARTESIAN_POINT('Ctrl Pts',(1.41473793359226,21.9786978113935,14.6105568327851));
#49471=CARTESIAN_POINT('Ctrl Pts',(1.36146953824052,21.9886600667297,14.6705134341828));
#49472=CARTESIAN_POINT('Ctrl Pts',(1.30433212071809,21.9986472232976,14.7277644362177));
#49473=CARTESIAN_POINT('Ctrl Pts',(1.24382892666125,22.0086641846916,14.7815892869782));
#49474=CARTESIAN_POINT('Ctrl Pts',(1.18369020234143,22.0186208041592,14.8350898981757));
#49475=CARTESIAN_POINT('Ctrl Pts',(1.12022606881676,22.0286068499976,14.885204124714));
#49476=CARTESIAN_POINT('Ctrl Pts',(1.05398172255351,22.0386211344547,14.9312252524384));
#49477=CARTESIAN_POINT('Ctrl Pts',(0.987737376290259,22.0486354189118,14.9772463801628));
#49478=CARTESIAN_POINT('Ctrl Pts',(0.918712930155135,22.0586779344765,15.0191729398781));
#49479=CARTESIAN_POINT('Ctrl Pts',(0.847504407217753,22.068741671468,15.0563205105648));
#49480=CARTESIAN_POINT('Ctrl Pts',(0.776019618274311,22.0788444524997,15.0936122017944));
#49481=CARTESIAN_POINT('Ctrl Pts',(0.7022810315133,22.0889425867954,15.1264768539342));
#49482=CARTESIAN_POINT('Ctrl Pts',(0.626749433413019,22.0990327790289,15.1543406173158));
#49483=CARTESIAN_POINT('Ctrl Pts',(0.521406870438683,22.1131053888706,15.1932017075423));
#49484=CARTESIAN_POINT('Ctrl Pts',(0.412576666681248,22.127162529881,15.2223376131965));
#49485=CARTESIAN_POINT('Ctrl Pts',(0.301790749552458,22.1412276519157,15.2418700938868));
#49486=CARTESIAN_POINT('Ctrl Pts',(0.191666938041238,22.1552087145631,15.2612858398376));
#49487=CARTESIAN_POINT('Ctrl Pts',(0.079609407275202,22.1691976620542,15.2712125593463));
#49488=CARTESIAN_POINT('Ctrl Pts',(-0.0328784186612369,22.1832177494457,
15.2717194946849));
#49489=CARTESIAN_POINT('Ctrl Pts',(-0.0916837471965429,22.190547038978,
15.2719845055773));
#49490=CARTESIAN_POINT('Ctrl Pts',(-0.150606570501646,22.1978848425051,
15.2696743612906));
#49491=CARTESIAN_POINT('Ctrl Pts',(-0.209430405166893,22.2052345084796,
15.2647934813694));
#49492=CARTESIAN_POINT('Ctrl Pts',(-0.293235601605187,22.2157054375554,
15.2578397847442));
#49493=CARTESIAN_POINT('Ctrl Pts',(-0.376827517946635,22.2261880737978,
15.2457661402555));
#49494=CARTESIAN_POINT('Ctrl Pts',(-0.459536375158249,22.2366976635983,
15.2284990899665));
#49495=CARTESIAN_POINT('Ctrl Pts',(-0.497767673881477,22.2415556108686,
15.2205175777086));
#49496=CARTESIAN_POINT('Ctrl Pts',(-0.535809564887223,22.2464192336659,
15.2114265062888));
#49497=CARTESIAN_POINT('Ctrl Pts',(-0.573592271050726,22.2512896053801,
15.2012195186864));
#49498=CARTESIAN_POINT('Ctrl Pts',(-0.655205552149098,22.2618099480483,
15.1791717134083));
#49499=CARTESIAN_POINT('Ctrl Pts',(-0.735612228619729,22.2723621681961,
15.1519150840058));
#49500=CARTESIAN_POINT('Ctrl Pts',(-0.814123694366391,22.2829457456128,
15.1196337113446));
#49501=CARTESIAN_POINT('Ctrl Pts',(-0.892191040472025,22.2934694543906,
15.0875349462999));
#49502=CARTESIAN_POINT('Ctrl Pts',(-0.968383848101112,22.3040241596809,
15.0504673884392));
#49503=CARTESIAN_POINT('Ctrl Pts',(-1.04198865827739,22.3146035515234,15.0086475436306));
#49504=CARTESIAN_POINT('Ctrl Pts',(-1.1094759609872,22.3243036596829,14.9703034664009));
#49505=CARTESIAN_POINT('Ctrl Pts',(-1.17478665200284,22.3340244571065,14.9279642837113));
#49506=CARTESIAN_POINT('Ctrl Pts',(-1.23735227846962,22.3437568153301,14.8818304976722));
#49507=CARTESIAN_POINT('Ctrl Pts',(-1.33686420100706,22.3592363323164,14.808453757089));
#49508=CARTESIAN_POINT('Ctrl Pts',(-1.43002938158697,22.3747533541792,14.7258857054826));
#49509=CARTESIAN_POINT('Ctrl Pts',(-1.5148938053479,22.3902984772833,14.634910568396));
#49510=CARTESIAN_POINT('Ctrl Pts',(-1.5439567183862,22.3956221045575,14.6037549630125));
#49511=CARTESIAN_POINT('Ctrl Pts',(-1.5720460240266,22.4009489972205,14.5716138111196));
#49512=CARTESIAN_POINT('Ctrl Pts',(-1.59908316744238,22.4062786834821,14.5385200116539));
#49513=CARTESIAN_POINT('Ctrl Pts',(-1.61008158302221,22.4084467418274,14.5250578143337));
#49514=CARTESIAN_POINT('Ctrl Pts',(-1.62090589004253,22.4106152617884,14.5114379829887));
#49515=CARTESIAN_POINT('Ctrl Pts',(-1.63156723422555,22.4127856975921,14.497686110411));
#49516=CARTESIAN_POINT('Ctrl Pts',(-1.64222799992902,22.4149560156289,14.4839349840034));
#49517=CARTESIAN_POINT('Ctrl Pts',(-1.65272582151843,22.4171282495049,14.4700518318093));
#49518=CARTESIAN_POINT('Ctrl Pts',(-1.6630471897459,22.4193010708845,14.4560281669034));
#49519=CARTESIAN_POINT('Ctrl Pts',(-1.68368930085215,22.4236465819973,14.4279816867541));
#49520=CARTESIAN_POINT('Ctrl Pts',(-1.70362563026762,22.4279944438579,14.3993731698481));
#49521=CARTESIAN_POINT('Ctrl Pts',(-1.72283016099311,22.432345792295,14.3702521569207));
#49522=CARTESIAN_POINT('Ctrl Pts',(-1.76124376446553,22.4410495182971,14.3120032437189));
#49523=CARTESIAN_POINT('Ctrl Pts',(-1.79672928601972,22.4497672159115,14.2517036122225));
#49524=CARTESIAN_POINT('Ctrl Pts',(-1.82908634094825,22.4584952742547,14.1896720330967));
#49525=CARTESIAN_POINT('Ctrl Pts',(-1.88554175016769,22.473723672097,14.0814415964326));
#49526=CARTESIAN_POINT('Ctrl Pts',(-1.93247076419735,22.4889837873255,13.9679375033174));
#49527=CARTESIAN_POINT('Ctrl Pts',(-1.96889307972031,22.5042661215331,13.8509879908307));
#49528=CARTESIAN_POINT('Ctrl Pts',(-1.97426102130403,22.5065184406433,13.8337519051436));
#49529=CARTESIAN_POINT('Ctrl Pts',(-1.979400828438,22.5087712367606,13.8164410243084));
#49530=CARTESIAN_POINT('Ctrl Pts',(-1.98430945388527,22.5110244736619,13.7990612406476));
#49531=CARTESIAN_POINT('Ctrl Pts',(-1.99959210052039,22.5180397621002,13.7449505542374));
#49532=CARTESIAN_POINT('Ctrl Pts',(-2.01263363809429,22.5250593338859,13.6901719394164));
#49533=CARTESIAN_POINT('Ctrl Pts',(-2.02341162482424,22.5320823127815,13.6349209726575));
#49534=CARTESIAN_POINT('Ctrl Pts',(-2.04842010727672,22.548377939124,13.5067205148826));
#49535=CARTESIAN_POINT('Ctrl Pts',(-2.06129275235582,22.5647344926122,13.3756303213226));
#49536=CARTESIAN_POINT('Ctrl Pts',(-2.06166334293173,22.5811476373884,13.2440592448445));
#49537=CARTESIAN_POINT('Ctrl Pts',(-2.06193254000901,22.5930701494268,13.1484859854469));
#49538=CARTESIAN_POINT('Ctrl Pts',(-2.05560612922728,22.6050225678144,13.0526595946214));
#49539=CARTESIAN_POINT('Ctrl Pts',(-2.04256085155299,22.6170039430696,12.9575039464542));
#49540=CARTESIAN_POINT('Ctrl Pts',(-2.02449774749023,22.6335939178829,12.8257469675751));
#49541=CARTESIAN_POINT('Ctrl Pts',(-1.993551370792,22.6502393264052,12.6952777357297));
#49542=CARTESIAN_POINT('Ctrl Pts',(-1.95044799723897,22.6669360972741,12.5685500336052));
#49543=CARTESIAN_POINT('Ctrl Pts',(-1.90837297422408,22.6832345203597,12.4448457723378));
#49544=CARTESIAN_POINT('Ctrl Pts',(-1.854715159545,22.6995818941742,12.3247077201271));
#49545=CARTESIAN_POINT('Ctrl Pts',(-1.79018285086913,22.7159763850598,12.2103819720975));
#49546=CARTESIAN_POINT('Ctrl Pts',(-1.77914030747185,22.7187817531118,12.1908189491723));
#49547=CARTESIAN_POINT('Ctrl Pts',(-1.76777940798862,22.7215885053195,12.1714260067366));
#49548=CARTESIAN_POINT('Ctrl Pts',(-1.75610376767816,22.7243966380861,12.1522142564495));
#49549=CARTESIAN_POINT('Ctrl Pts',(-1.75609312576069,22.724399197596,12.1521967456445));
#49550=CARTESIAN_POINT('Ctrl Pts',(-1.75608248357209,22.7244017571067,12.1521792349886));
#49551=CARTESIAN_POINT('Ctrl Pts',(-1.75607184111235,22.7244043166181,12.1521617244818));
#49552=CARTESIAN_POINT('Ctrl Pts',(-1.70602464861915,22.73644066582,12.0698168789036));
#49553=CARTESIAN_POINT('Ctrl Pts',(-1.64998124464433,22.7484933761121,11.990774269108));
#49554=CARTESIAN_POINT('Ctrl Pts',(-1.5886224448513,22.7605683218413,11.9157699396956));
#49555=CARTESIAN_POINT('Ctrl Pts',(-1.52697928682789,22.7726992271104,11.8404180138757));
#49556=CARTESIAN_POINT('Ctrl Pts',(-1.45997258035869,22.784852571806,11.7691416615236));
#49557=CARTESIAN_POINT('Ctrl Pts',(-1.3882850840447,22.7970403334136,11.7026357684154));
#49558=CARTESIAN_POINT('Ctrl Pts',(-1.33900586419685,22.8054184106878,11.6569184718689));
#49559=CARTESIAN_POINT('Ctrl Pts',(-1.28751458748217,22.8138128771267,11.6134543165319));
#49560=CARTESIAN_POINT('Ctrl Pts',(-1.23402673793582,22.8222292653591,11.5724562683856));
#49561=CARTESIAN_POINT('Ctrl Pts',(-1.21085154590683,22.8258759143669,11.5546926520379));
#49562=CARTESIAN_POINT('Ctrl Pts',(-1.18730732101797,22.8295269549272,11.5373913333772));
#49563=CARTESIAN_POINT('Ctrl Pts',(-1.16340403922038,22.8331818264926,11.520572756893));
#49564=CARTESIAN_POINT('Ctrl Pts',(-1.09738320232914,22.8432765775616,11.4741198679464));
#49565=CARTESIAN_POINT('Ctrl Pts',(-1.02862130032526,22.853400982747,11.431346416387));
#49566=CARTESIAN_POINT('Ctrl Pts',(-0.957487322430239,22.8635387970186,
11.3925497814004));
#49567=CARTESIAN_POINT('Ctrl Pts',(-0.938375761414071,22.8662625228914,
11.3821262921101));
#49568=CARTESIAN_POINT('Ctrl Pts',(-0.919093132063599,22.8689871836512,
11.3719901073133));
#49569=CARTESIAN_POINT('Ctrl Pts',(-0.89964696783731,22.8717123915825,11.3621475069002));
#49570=CARTESIAN_POINT('Ctrl Pts',(-0.840631475660235,22.8799828908688,
11.3322770449972));
#49571=CARTESIAN_POINT('Ctrl Pts',(-0.7800995080275,22.8882586795186,11.3051108697579));
#49572=CARTESIAN_POINT('Ctrl Pts',(-0.718378889207034,22.8965571443992,
11.2807095405642));
#49573=CARTESIAN_POINT('Ctrl Pts',(-0.66015096252314,22.9043860095967,11.2576890518777));
#49574=CARTESIAN_POINT('Ctrl Pts',(-0.600865963332381,22.9122346929815,
11.23712959669));
#49575=CARTESIAN_POINT('Ctrl Pts',(-0.540681088327972,22.9200672254062,
11.219278553958));
#49576=CARTESIAN_POINT('Ctrl Pts',(-0.53707101234487,22.9205370450609,11.2182077928966));
#49577=CARTESIAN_POINT('Ctrl Pts',(-0.533457713020527,22.9210068046686,
11.2171467822687));
#49578=CARTESIAN_POINT('Ctrl Pts',(-0.529841229840762,22.921476495726,11.2160955774765));
#49579=CARTESIAN_POINT('Ctrl Pts',(-0.47293739841567,22.9288668856218,11.199555315207));
#49580=CARTESIAN_POINT('Ctrl Pts',(-0.415260096998153,22.9362722510411,
11.1853241913507));
#49581=CARTESIAN_POINT('Ctrl Pts',(-0.356992449122508,22.9436918706304,
11.1734995547958));
#49582=CARTESIAN_POINT('Ctrl Pts',(-0.224657608253982,22.9605429743466,
11.1466439762051));
#49583=CARTESIAN_POINT('Ctrl Pts',(-0.0892760184599879,22.9774676839623,
11.1322046530843));
#49584=CARTESIAN_POINT('Ctrl Pts',(0.0467160701239138,22.9944573160433,
11.1303758754179));
#49585=CARTESIAN_POINT('Ctrl Pts',(0.182822450839455,23.0114612267584,11.1285455607879));
#49586=CARTESIAN_POINT('Ctrl Pts',(0.319538748472705,23.0285301696247,11.139347356567));
#49587=CARTESIAN_POINT('Ctrl Pts',(0.454409559166268,23.045654228185,11.1629271179154));
#49588=CARTESIAN_POINT('Ctrl Pts',(0.480790119540459,23.04900367243,11.1675392894792));
#49589=CARTESIAN_POINT('Ctrl Pts',(0.507100077358982,23.0523552216179,11.1726401720616));
#49590=CARTESIAN_POINT('Ctrl Pts',(0.533321083292172,23.0557087961119,11.1782306203905));
#49591=CARTESIAN_POINT('Ctrl Pts',(0.66435187770533,23.0724671741541,11.2061670347114));
#49592=CARTESIAN_POINT('Ctrl Pts',(0.793159418990842,23.0892762164664,11.2463321881611));
#49593=CARTESIAN_POINT('Ctrl Pts',(0.917520791015336,23.1061258989711,11.2979488789536));
#49594=CARTESIAN_POINT('Ctrl Pts',(0.960851012678654,23.1119966968403,11.3159332628274));
#49595=CARTESIAN_POINT('Ctrl Pts',(1.00364171995528,23.1178724184597,11.3353074568489));
#49596=CARTESIAN_POINT('Ctrl Pts',(1.04579984609325,23.1237526081734,11.3560373996693));
#49597=CARTESIAN_POINT('Ctrl Pts',(1.08675652479358,23.1294652207314,11.3761765682081));
#49598=CARTESIAN_POINT('Ctrl Pts',(1.12715108040483,23.1351882832585,11.3976071882125));
#49599=CARTESIAN_POINT('Ctrl Pts',(1.16689591677254,23.1409213493446,11.4203041172429));
#49600=CARTESIAN_POINT('Ctrl Pts',(1.28051631826157,23.1573107304568,11.4851888777472));
#49601=CARTESIAN_POINT('Ctrl Pts',(1.38882683471882,23.1737819846396,11.5604265113867));
#49602=CARTESIAN_POINT('Ctrl Pts',(1.49004567469032,23.1903219342844,11.6448777959143));
#49603=CARTESIAN_POINT('Ctrl Pts',(1.56519864906441,23.2026025177425,11.7075811940539));
#49604=CARTESIAN_POINT('Ctrl Pts',(1.63644184944928,23.214920937324,11.7753626167078));
#49605=CARTESIAN_POINT('Ctrl Pts',(1.70304958895036,23.2272712204125,11.8477376096129));
#49606=CARTESIAN_POINT('Ctrl Pts',(1.79220005105934,23.2438013331708,11.9446071943031));
#49607=CARTESIAN_POINT('Ctrl Pts',(1.87304455589512,23.2603885847949,12.0497067849583));
#49608=CARTESIAN_POINT('Ctrl Pts',(1.94426242074266,23.2770195316268,12.161347316853));
#49609=CARTESIAN_POINT('Ctrl Pts',(1.99795342908258,23.2895575697577,12.2455128944347));
#49610=CARTESIAN_POINT('Ctrl Pts',(2.04617345407436,23.3021204101728,12.3333951026968));
#49611=CARTESIAN_POINT('Ctrl Pts',(2.08837296977119,23.3147017053923,12.424259253471));
#49612=CARTESIAN_POINT('Ctrl Pts',(2.10773883103045,23.320475411883,12.4659578964122));
#49613=CARTESIAN_POINT('Ctrl Pts',(2.12583700996293,23.3262529979351,12.5082844297924));
#49614=CARTESIAN_POINT('Ctrl Pts',(2.14264366952361,23.3320336869479,12.5511537969633));
#49615=CARTESIAN_POINT('Ctrl Pts',(2.16850476118605,23.3409286686004,12.6171186384545));
#49616=CARTESIAN_POINT('Ctrl Pts',(2.19136299542564,23.3498537327965,12.68443503575));
#49617=CARTESIAN_POINT('Ctrl Pts',(2.21110758798156,23.3588032190322,12.7528101322129));
#49618=CARTESIAN_POINT('Ctrl Pts',(2.24365216241923,23.3735544589048,12.8655112887556));
#49619=CARTESIAN_POINT('Ctrl Pts',(2.26773655635913,23.3883722400078,12.9810908979152));
#49620=CARTESIAN_POINT('Ctrl Pts',(2.28254142021421,23.4032287350915,13.0982132722858));
#49621=CARTESIAN_POINT('Ctrl Pts',(2.2978253267114,23.4185659434548,13.2191253884749));
#49622=CARTESIAN_POINT('Ctrl Pts',(2.30321800020739,23.4339444271894,13.3416811846617));
#49623=CARTESIAN_POINT('Ctrl Pts',(2.29882885160258,23.4493306956133,13.464252681421));
#49624=CARTESIAN_POINT('Ctrl Pts',(2.29425118527407,23.465377817556,13.5920887298371));
#49625=CARTESIAN_POINT('Ctrl Pts',(2.27903224885156,23.4814334301426,13.7199407845635));
#49626=CARTESIAN_POINT('Ctrl Pts',(2.25334613239327,23.4974549071042,13.8459290279421));
#49627=CARTESIAN_POINT('Ctrl Pts',(2.22930897513146,23.5124478610573,13.9638292649883));
#49628=CARTESIAN_POINT('Ctrl Pts',(2.19610540563927,23.527410870655,14.0800958534789));
#49629=CARTESIAN_POINT('Ctrl Pts',(2.15392753614281,23.5423053741867,14.1931793929172));
#49630=CARTESIAN_POINT('Ctrl Pts',(2.15103411638287,23.5433271434545,14.200936971748));
#49631=CARTESIAN_POINT('Ctrl Pts',(2.14809848387044,23.5443485889938,14.2086795723589));
#49632=CARTESIAN_POINT('Ctrl Pts',(2.14512070981644,23.5453696977673,14.2164066955463));
#49633=CARTESIAN_POINT('Ctrl Pts',(2.10996949583209,23.5574234037735,14.3076217292327));
#49634=CARTESIAN_POINT('Ctrl Pts',(2.06897791375395,23.569504711142,14.3968612204971));
#49635=CARTESIAN_POINT('Ctrl Pts',(2.02223032330238,23.5816177990558,14.483331947589));
#49636=CARTESIAN_POINT('Ctrl Pts',(1.95119959217953,23.6000230576446,14.6147200877418));
#49637=CARTESIAN_POINT('Ctrl Pts',(1.86687763322092,23.6185015297287,14.7397136812518));
#49638=CARTESIAN_POINT('Ctrl Pts',(1.77116245925139,23.6370695232595,14.856132200404));
#49639=CARTESIAN_POINT('Ctrl Pts',(1.67390402864993,23.6559368964808,14.9744277850653));
#49640=CARTESIAN_POINT('Ctrl Pts',(1.56488382774509,23.674896701891,15.0838687275083));
#49641=CARTESIAN_POINT('Ctrl Pts',(1.44612313093434,23.6939696171635,15.1822113192552));
#49642=CARTESIAN_POINT('Ctrl Pts',(1.3302949809633,23.7125715667133,15.2781255465315));
#49643=CARTESIAN_POINT('Ctrl Pts',(1.20520292293797,23.7312811333672,15.363482535802));
#49644=CARTESIAN_POINT('Ctrl Pts',(1.07272586484995,23.750120643866,15.4362494088806));
#49645=CARTESIAN_POINT('Ctrl Pts',(1.04594961399663,23.7539284840034,15.4509570426059));
#49646=CARTESIAN_POINT('Ctrl Pts',(1.01887164069649,23.7577416424881,15.4651505066664));
#49647=CARTESIAN_POINT('Ctrl Pts',(0.991507402002442,23.7615603184461,15.4788132733641));
#49648=CARTESIAN_POINT('Ctrl Pts',(0.989372951962116,23.7618581806721,15.4798789888498));
#49649=CARTESIAN_POINT('Ctrl Pts',(0.987236734171534,23.7621560594999,15.4809414585348));
#49650=CARTESIAN_POINT('Ctrl Pts',(0.985098755439263,23.7624539548253,15.4820006743314));
#49651=CARTESIAN_POINT('Ctrl Pts',(0.853241280819933,23.7808263196765,15.547326637546));
#49652=CARTESIAN_POINT('Ctrl Pts',(0.714684835416255,23.7992617702816,15.6002802227186));
#49653=CARTESIAN_POINT('Ctrl Pts',(0.571892893158105,23.8177343014512,15.6402853378414));
#49654=CARTESIAN_POINT('Ctrl Pts',(0.430589480859245,23.8360142663203,15.6798734209423));
#49655=CARTESIAN_POINT('Ctrl Pts',(0.285137078569464,23.8543305250424,15.7067808395966));
#49656=CARTESIAN_POINT('Ctrl Pts',(0.137946779997347,23.872654112305,15.7204051672449));
#49657=CARTESIAN_POINT('Ctrl Pts',(0.0166372293009362,23.8877558286513,
15.7316339036602));
#49658=CARTESIAN_POINT('Ctrl Pts',(-0.105853298504911,23.9029507858283,
15.7339466020836));
#49659=CARTESIAN_POINT('Ctrl Pts',(-0.228084068191911,23.9182050932659,
15.7269919643805));
#49660=CARTESIAN_POINT('Ctrl Pts',(-0.308748575019462,23.9282719625951,
15.7224023473641));
#49661=CARTESIAN_POINT('Ctrl Pts',(-0.389299231225943,23.9383646229679,
15.7137774593658));
#49662=CARTESIAN_POINT('Ctrl Pts',(-0.469317257680067,23.948472685808,15.7010278929291));
#49663=CARTESIAN_POINT('Ctrl Pts',(-0.566247339062064,23.960717118683,15.6855836665833));
#49664=CARTESIAN_POINT('Ctrl Pts',(-0.662395564656194,23.9729841799441,
15.664086476296));
#49665=CARTESIAN_POINT('Ctrl Pts',(-0.75705030671739,23.9852545166603,15.6368308527521));
#49666=CARTESIAN_POINT('Ctrl Pts',(-0.879291061645446,24.001100898899,15.6016318978399));
#49667=CARTESIAN_POINT('Ctrl Pts',(-0.999240921484818,24.0168963352913,
15.5566670380693));
#49668=CARTESIAN_POINT('Ctrl Pts',(-1.11539944299005,24.0327012286101,15.5026136497645));
#49669=CARTESIAN_POINT('Ctrl Pts',(-1.23256398476096,24.0486430042064,15.4480921184137));
#49670=CARTESIAN_POINT('Ctrl Pts',(-1.34587113347849,24.0645944091951,15.3843253628821));
#49671=CARTESIAN_POINT('Ctrl Pts',(-1.45383298371875,24.0806237318463,15.3120172562257));
#49672=CARTESIAN_POINT('Ctrl Pts',(-1.56239279217184,24.0967418346092,15.2393086634149));
#49673=CARTESIAN_POINT('Ctrl Pts',(-1.66554821936208,24.1129387350077,15.1579650704219));
#49674=CARTESIAN_POINT('Ctrl Pts',(-1.76183724711987,24.1292900331302,15.06869090456));
#49675=CARTESIAN_POINT('Ctrl Pts',(-1.77787018829626,24.1320126631854,15.0538259974863));
#49676=CARTESIAN_POINT('Ctrl Pts',(-1.79371286406918,24.1347395874191,15.0387411663101));
#49677=CARTESIAN_POINT('Ctrl Pts',(-1.80935864822686,24.1374711708594,15.0234395982253));
#49678=CARTESIAN_POINT('',(1.9,22.4,13.3));
#49679=CARTESIAN_POINT('',(1.9,22.4,13.3));
#49680=CARTESIAN_POINT('Ctrl Pts',(1.9,22.4,13.3));
#49681=CARTESIAN_POINT('Ctrl Pts',(1.89077819837431,22.4422021414379,13.6519691914269));
#49682=CARTESIAN_POINT('Ctrl Pts',(1.71537787585695,22.5206083204434,14.2515774145128));
#49683=CARTESIAN_POINT('Ctrl Pts',(0.776895987153429,22.6819257904964,15.2190094254541));
#49684=CARTESIAN_POINT('Ctrl Pts',(-1.01219784483332,22.8782378453878,15.2495646232149));
#49685=CARTESIAN_POINT('Ctrl Pts',(-2.18535724516091,23.1134574970354,13.4517991919584));
#49686=CARTESIAN_POINT('Ctrl Pts',(-1.37199074496505,23.3213768149546,11.7396096714547));
#49687=CARTESIAN_POINT('Ctrl Pts',(0.123403026550972,23.504121058761,11.3105725465261));
#49688=CARTESIAN_POINT('Ctrl Pts',(1.35501251051576,23.661466918215,11.8220255257895));
#49689=CARTESIAN_POINT('Ctrl Pts',(1.94832765695265,23.8068375246815,12.9042814161785));
#49690=CARTESIAN_POINT('Ctrl Pts',(1.84336678935325,23.9401410891422,14.0034773628334));
#49691=CARTESIAN_POINT('Ctrl Pts',(1.27754402361024,24.0611907458831,14.8296511355055));
#49692=CARTESIAN_POINT('Ctrl Pts',(0.371246325431991,24.1834651264945,15.2797269167144));
#49693=CARTESIAN_POINT('Ctrl Pts',(-0.765145428848119,24.3208689298072,
15.2281627669602));
#49694=CARTESIAN_POINT('Ctrl Pts',(-1.81032562534546,24.4742008762416,14.4542829226342));
#49695=CARTESIAN_POINT('Ctrl Pts',(-2.17704469672661,24.6445536494329,13.0553638368446));
#49696=CARTESIAN_POINT('Ctrl Pts',(-1.57203155460298,24.8182979987203,11.709895265911));
#49697=CARTESIAN_POINT('Ctrl Pts',(-0.23180116439731,24.99574025007,11.0244995821736));
#49698=CARTESIAN_POINT('Ctrl Pts',(1.27630691611381,25.1771408957878,11.3398317849377));
#49699=CARTESIAN_POINT('Ctrl Pts',(2.27577079055389,25.3627495865527,12.5571271706314));
#49700=CARTESIAN_POINT('Ctrl Pts',(2.29218789520766,25.5527742410498,14.1699219694977));
#49701=CARTESIAN_POINT('Ctrl Pts',(1.26950162628108,25.74739985761,15.4673025113756));
#49702=CARTESIAN_POINT('Ctrl Pts',(-0.379485062712953,25.9467742695935,
15.8456532640155));
#49703=CARTESIAN_POINT('Ctrl Pts',(-1.90561289077789,26.1465422559426,15.107782139803));
#49704=CARTESIAN_POINT('Ctrl Pts',(-2.41085879002264,26.2813144727143,14.08936731534));
#49705=CARTESIAN_POINT('Ctrl Pts',(-2.48616900737713,26.3471379964276,13.5677880585459));
#49706=CARTESIAN_POINT('Ctrl Pts',(-2.53714261746217,33.794702538555,11.5837945911968));
#49707=CARTESIAN_POINT('Ctrl Pts',(-2.20302045656255,33.8670105940936,11.110489816432));
#49708=CARTESIAN_POINT('Ctrl Pts',(-1.27342212310457,34.00910827188,10.375303523525));
#49709=CARTESIAN_POINT('Ctrl Pts',(0.463317385363586,34.2188326311658,10.1881891863586));
#49710=CARTESIAN_POINT('Ctrl Pts',(2.00461530565732,34.4242135651314,10.9298496609176));
#49711=CARTESIAN_POINT('Ctrl Pts',(2.9101807189669,34.626789103856,12.3532946652702));
#49712=CARTESIAN_POINT('Ctrl Pts',(2.9285690247221,34.8264375311958,14.0157823092848));
#49713=CARTESIAN_POINT('Ctrl Pts',(2.07948629363936,35.0230507318404,15.4164655904329));
#49714=CARTESIAN_POINT('Ctrl Pts',(0.644202929896784,35.2165344443341,16.1458951292022));
#49715=CARTESIAN_POINT('Ctrl Pts',(-1.11292611387905,35.4279525102656,15.997334529376));
#49716=CARTESIAN_POINT('Ctrl Pts',(-2.16612159687256,35.5936923565744,15.0466138670219));
#49717=CARTESIAN_POINT('Ctrl Pts',(-2.52608715609147,35.7161456129446,14.1285591261768));
#49718=CARTESIAN_POINT('Ctrl Pts',(-2.65004752744008,35.7972859707521,13.488171032948));
#49719=CARTESIAN_POINT('Ctrl Pts',(-2.55248073601967,35.9379787039982,12.3436775763336));
#49720=CARTESIAN_POINT('Ctrl Pts',(-1.53423707359805,36.1352271943492,10.9940745150984));
#49721=CARTESIAN_POINT('Ctrl Pts',(0.414031698965699,36.3659328772203,10.6302615404033));
#49722=CARTESIAN_POINT('Ctrl Pts',(2.04980546711222,36.590686252149,11.6566868060208));
#49723=CARTESIAN_POINT('Ctrl Pts',(2.51010674367927,36.7913391087015,13.3133883571633));
#49724=CARTESIAN_POINT('Ctrl Pts',(1.96182694676073,36.9695819315518,14.6953200830345));
#49725=CARTESIAN_POINT('Ctrl Pts',(0.913154495044754,37.1268632725084,15.4780580828442));
#49726=CARTESIAN_POINT('Ctrl Pts',(-0.367392365969926,37.281098280273,15.5856567059268));
#49727=CARTESIAN_POINT('Ctrl Pts',(-1.48957786961239,37.4323952581935,15.0136248643657));
#49728=CARTESIAN_POINT('Ctrl Pts',(-2.12989204619479,37.580873057395,13.9555713790989));
#49729=CARTESIAN_POINT('Ctrl Pts',(-2.11563312293493,37.7266668431562,12.7413002907563));
#49730=CARTESIAN_POINT('Ctrl Pts',(-1.4734213597753,37.8699258077578,11.7360649626158));
#49731=CARTESIAN_POINT('Ctrl Pts',(-0.416200202780098,38.0108006676585,
11.2271354294049));
#49732=CARTESIAN_POINT('Ctrl Pts',(0.731872469631232,38.1494725717998,11.3527537042491));
#49733=CARTESIAN_POINT('Ctrl Pts',(1.62909612187799,38.2861087083245,12.0527247864151));
#49734=CARTESIAN_POINT('Ctrl Pts',(2.01607881421587,38.420910106321,13.1070091406949));
#49735=CARTESIAN_POINT('Ctrl Pts',(1.79172084866822,38.5540703969794,14.1931449414799));
#49736=CARTESIAN_POINT('Ctrl Pts',(1.03692345394962,38.6857972959208,14.9894180523881));
#49737=CARTESIAN_POINT('Ctrl Pts',(-0.015088982985104,38.8163035818771,
15.2648321582235));
#49738=CARTESIAN_POINT('Ctrl Pts',(-1.04426227167881,38.9458044926218,14.9462196494202));
#49739=CARTESIAN_POINT('Ctrl Pts',(-1.82985905407118,39.0888382556108,14.0491931927851));
#49740=CARTESIAN_POINT('Ctrl Pts',(-1.92248310902473,39.2453849714331,12.7108350899886));
#49741=CARTESIAN_POINT('Ctrl Pts',(-1.01321098977672,39.4157297322394,11.5639384682371));
#49742=CARTESIAN_POINT('Ctrl Pts',(0.431328930297244,39.5861937286102,11.3330209300884));
#49743=CARTESIAN_POINT('Ctrl Pts',(1.45502419956615,39.728797825825,12.00370853134));
#49744=CARTESIAN_POINT('Ctrl Pts',(1.84542351138279,39.8434880354635,12.8539190362301));
#49745=CARTESIAN_POINT('Ctrl Pts',(1.90901377452895,39.9586677453586,13.7914090498871));
#49746=CARTESIAN_POINT('Ctrl Pts',(1.44201319640107,40.0747166553859,14.6691796791337));
#49747=CARTESIAN_POINT('Ctrl Pts',(0.612739553103985,40.1918981421937,15.1463780893102));
#49748=CARTESIAN_POINT('Ctrl Pts',(0.0790120767017547,40.25828434609,15.230428162705));
#49749=CARTESIAN_POINT('Ctrl Pts',(-0.276763612704706,40.3027552942086,
15.202780730348));
#49750=CARTESIAN_POINT('Ctrl Pts',(-0.5115856699662,40.3324632619737,15.1625337767236));
#49751=CARTESIAN_POINT('Ctrl Pts',(-0.79725179899804,40.3697101209255,15.0717252071008));
#49752=CARTESIAN_POINT('Ctrl Pts',(-1.11514470712696,40.4145899651528,14.9003327976856));
#49753=CARTESIAN_POINT('Ctrl Pts',(-1.68066644673384,40.5047478080795,14.4466263558439));
#49754=CARTESIAN_POINT('Ctrl Pts',(-2.17634554015148,40.6414894617506,13.3813510245936));
#49755=CARTESIAN_POINT('Ctrl Pts',(-1.74732493907859,40.8068384562209,12.0329549479021));
#49756=CARTESIAN_POINT('Ctrl Pts',(-0.493115687221394,40.9962690026588,
11.0836019300558));
#49757=CARTESIAN_POINT('Ctrl Pts',(0.766873073701429,41.1375762814092,11.1873998032218));
#49758=CARTESIAN_POINT('Ctrl Pts',(1.63769882242631,41.2747095576386,11.8683492876489));
#49759=CARTESIAN_POINT('Ctrl Pts',(2.12293894185963,41.3743602909584,12.5220924979612));
#49760=CARTESIAN_POINT('Ctrl Pts',(2.29726804509882,41.5136636354595,13.6710807665245));
#49761=CARTESIAN_POINT('Ctrl Pts',(1.79017023846489,41.6685969694184,14.8567246269234));
#49762=CARTESIAN_POINT('Ctrl Pts',(0.71282329412476,41.8265976614803,15.6134221495628));
#49763=CARTESIAN_POINT('Ctrl Pts',(-0.626664005515929,41.9877563906676,
15.6898056909252));
#49764=CARTESIAN_POINT('Ctrl Pts',(-1.82898756958588,42.1521456502828,15.0362175564882));
#49765=CARTESIAN_POINT('Ctrl Pts',(-2.5759705941618,42.3335725612856,13.7232903735765));
#49766=CARTESIAN_POINT('Ctrl Pts',(-2.46701467117438,42.4619079332118,12.6396216068561));
#49767=CARTESIAN_POINT('Ctrl Pts',(-2.20984257971657,42.5339741612212,12.1210770352365));
#49768=CARTESIAN_POINT('Ctrl Pts',(-2.40023872834448,33.8617379370758,11.7171990219698));
#49769=CARTESIAN_POINT('Ctrl Pts',(-2.08972378175159,33.9296563314948,11.2703464575275));
#49770=CARTESIAN_POINT('Ctrl Pts',(-1.22264220293187,34.062963020044,10.574517277758));
#49771=CARTESIAN_POINT('Ctrl Pts',(0.401620283615534,34.2592803421303,10.3876332565902));
#49772=CARTESIAN_POINT('Ctrl Pts',(1.84648101894249,34.4511554191802,11.0698597282399));
#49773=CARTESIAN_POINT('Ctrl Pts',(2.70086130924968,34.6400836730942,12.3909315353159));
#49774=CARTESIAN_POINT('Ctrl Pts',(2.72977180381108,34.8260078761717,13.9388082726507));
#49775=CARTESIAN_POINT('Ctrl Pts',(1.95023745713216,35.0088847893345,15.2475926736166));
#49776=CARTESIAN_POINT('Ctrl Pts',(0.622012464087979,35.1886854204671,15.9359219413486));
#49777=CARTESIAN_POINT('Ctrl Pts',(-1.01071028039656,35.3850305540958,15.8111919221846));
#49778=CARTESIAN_POINT('Ctrl Pts',(-1.99566752188188,35.5389014813403,14.9368171104688));
#49779=CARTESIAN_POINT('Ctrl Pts',(-2.33707413395951,35.6526009429733,14.08734522877));
#49780=CARTESIAN_POINT('Ctrl Pts',(-2.45723222087079,35.72794749456,13.4937395625812));
#49781=CARTESIAN_POINT('Ctrl Pts',(-2.37578369332297,35.8586209988653,12.4301500330078));
#49782=CARTESIAN_POINT('Ctrl Pts',(-1.44087298808843,36.0419421060423,11.167583556436));
#49783=CARTESIAN_POINT('Ctrl Pts',(0.36908873702616,36.2566957249332,10.8120654899176));
#49784=CARTESIAN_POINT('Ctrl Pts',(1.90430675260224,36.4663895638823,11.7545860581376));
#49785=CARTESIAN_POINT('Ctrl Pts',(2.35071958929505,36.6541730382628,13.3003264205421));
#49786=CARTESIAN_POINT('Ctrl Pts',(1.84928551059103,36.8215462219214,14.6030222361114));
#49787=CARTESIAN_POINT('Ctrl Pts',(0.86921171423766,36.9697311952702,15.3506845341415));
#49788=CARTESIAN_POINT('Ctrl Pts',(-0.340491125387667,37.1155991148782,
15.4655045756358));
#49789=CARTESIAN_POINT('Ctrl Pts',(-1.41209004722825,37.2592980591129,14.9341478868308));
#49790=CARTESIAN_POINT('Ctrl Pts',(-2.03444167603858,37.4009824323719,13.9317371260455));
#49791=CARTESIAN_POINT('Ctrl Pts',(-2.03438454184915,37.5408199942793,12.767224166747));
#49792=CARTESIAN_POINT('Ctrl Pts',(-1.42675985213229,37.6789883174979,11.7905291103843));
#49793=CARTESIAN_POINT('Ctrl Pts',(-0.407448290021044,37.8156610740227,
11.2843509198806));
#49794=CARTESIAN_POINT('Ctrl Pts',(0.714623696940499,37.9510407034962,11.3928816172433));
#49795=CARTESIAN_POINT('Ctrl Pts',(1.60483188112312,38.08530868396,12.0691957199895));
#49796=CARTESIAN_POINT('Ctrl Pts',(2.00125500268751,38.2186781833416,13.1069546625132));
#49797=CARTESIAN_POINT('Ctrl Pts',(1.79220751461922,38.3513491921946,14.1917552318724));
#49798=CARTESIAN_POINT('Ctrl Pts',(1.04587569520604,38.4835318537754,15.0007847356739));
#49799=CARTESIAN_POINT('Ctrl Pts',(-0.013271108315001,38.6154367303176,
15.2936923811263));
#49800=CARTESIAN_POINT('Ctrl Pts',(-1.06519193510901,38.7472727137213,14.9839418685836));
#49801=CARTESIAN_POINT('Ctrl Pts',(-1.88328876777746,38.8939284090276,14.0759218299553));
#49802=CARTESIAN_POINT('Ctrl Pts',(-1.99949277300357,39.0557570565816,12.6943472018712));
#49803=CARTESIAN_POINT('Ctrl Pts',(-1.06936178982378,39.2334335463509,11.4843618678959));
#49804=CARTESIAN_POINT('Ctrl Pts',(0.446044403009374,39.412736616575,11.2189550970895));
#49805=CARTESIAN_POINT('Ctrl Pts',(1.54131410052628,39.5639017725726,11.9136852163027));
#49806=CARTESIAN_POINT('Ctrl Pts',(1.96963148607505,39.6861138284552,12.8137954486716));
#49807=CARTESIAN_POINT('Ctrl Pts',(2.05127330681957,39.8092486198186,13.8147372274146));
#49808=CARTESIAN_POINT('Ctrl Pts',(1.56333544279269,39.933877636358,14.7642723274395));
#49809=CARTESIAN_POINT('Ctrl Pts',(0.676407604025829,40.0602090961192,15.2906307544418));
#49810=CARTESIAN_POINT('Ctrl Pts',(0.101053978248039,40.1319449413606,15.389076917094));
#49811=CARTESIAN_POINT('Ctrl Pts',(-0.284182044219036,40.1800626930222,
15.3642008365041));
#49812=CARTESIAN_POINT('Ctrl Pts',(-0.538878969923101,40.2122223538578,
15.3239558518647));
#49813=CARTESIAN_POINT('Ctrl Pts',(-0.849543410497253,40.252572700832,15.2296458276861));
#49814=CARTESIAN_POINT('Ctrl Pts',(-1.19656882044088,40.3012377839666,15.0483186351474));
#49815=CARTESIAN_POINT('Ctrl Pts',(-1.8164799946024,40.3990797829461,14.5640427909459));
#49816=CARTESIAN_POINT('Ctrl Pts',(-2.37071699481453,40.5477712211053,13.4130859800096));
#49817=CARTESIAN_POINT('Ctrl Pts',(-1.92218168690635,40.7279584153765,11.9380100336219));
#49818=CARTESIAN_POINT('Ctrl Pts',(-0.567095654611867,40.9346017873572,
10.8855790573643));
#49819=CARTESIAN_POINT('Ctrl Pts',(0.809297734590367,41.0888438713821,10.9822321946955));
#49820=CARTESIAN_POINT('Ctrl Pts',(1.768006429168,41.2384680537974,11.7138499166356));
#49821=CARTESIAN_POINT('Ctrl Pts',(2.30552670588767,41.3471689506707,12.4206370433311));
#49822=CARTESIAN_POINT('Ctrl Pts',(2.50974914981252,41.4990127984438,13.6706870932952));
#49823=CARTESIAN_POINT('Ctrl Pts',(1.97209080071686,41.6676811835294,14.9673314840827));
#49824=CARTESIAN_POINT('Ctrl Pts',(0.810223789912052,41.8394078589309,15.8022801288837));
#49825=CARTESIAN_POINT('Ctrl Pts',(-0.641625837636128,42.0142173167945,
15.9004073151369));
#49826=CARTESIAN_POINT('Ctrl Pts',(-1.94982840906498,42.1921184914192,15.2065402529954));
#49827=CARTESIAN_POINT('Ctrl Pts',(-2.7701221386624,42.3879448295554,13.797659693616));
#49828=CARTESIAN_POINT('Ctrl Pts',(-2.66398655743805,42.5260201441487,12.6306928713517));
#49829=CARTESIAN_POINT('Ctrl Pts',(-2.39344664640429,42.6034004278108,12.0713137073846));
#49830=CARTESIAN_POINT('Ctrl Pts',(-2.26333483922681,33.9287733355967,11.8506034527428));
#49831=CARTESIAN_POINT('Ctrl Pts',(-1.97642710694064,33.9923020688959,11.430203098623));
#49832=CARTESIAN_POINT('Ctrl Pts',(-1.17186228275916,34.1168177682079,10.7737310319911));
#49833=CARTESIAN_POINT('Ctrl Pts',(0.339923181867489,34.2997280530948,10.5870773268218));
#49834=CARTESIAN_POINT('Ctrl Pts',(1.6883467322277,34.4780972732292,11.209869795562));
#49835=CARTESIAN_POINT('Ctrl Pts',(2.49154189953247,34.6533782423325,12.4285684053618));
#49836=CARTESIAN_POINT('Ctrl Pts',(2.53097458290008,34.8255782211476,13.8618342360166));
#49837=CARTESIAN_POINT('Ctrl Pts',(1.82098862062497,34.9947188468287,15.0787197568002));
#49838=CARTESIAN_POINT('Ctrl Pts',(0.599821998279183,35.1608363966002,15.725948753495));
#49839=CARTESIAN_POINT('Ctrl Pts',(-0.908494446914065,35.342108597926,15.6250493149932));
#49840=CARTESIAN_POINT('Ctrl Pts',(-1.8252134468912,35.4841106061063,14.8270203539157));
#49841=CARTESIAN_POINT('Ctrl Pts',(-2.14806111182756,35.5890562730018,14.0461313313633));
#49842=CARTESIAN_POINT('Ctrl Pts',(-2.26441691430149,35.6586090183679,13.4993080922143));
#49843=CARTESIAN_POINT('Ctrl Pts',(-2.19908665062627,35.7792632937322,12.5166224896819));
#49844=CARTESIAN_POINT('Ctrl Pts',(-1.3475089025788,35.9486570177353,11.3410925977736));
#49845=CARTESIAN_POINT('Ctrl Pts',(0.324145775086629,36.1474585726462,10.9938694394317));
#49846=CARTESIAN_POINT('Ctrl Pts',(1.75880803809227,36.3420928756156,11.8524853102545));
#49847=CARTESIAN_POINT('Ctrl Pts',(2.19133243491085,36.517006967824,13.2872644839208));
#49848=CARTESIAN_POINT('Ctrl Pts',(1.73674407442132,36.673510512291,14.5107243891885));
#49849=CARTESIAN_POINT('Ctrl Pts',(0.825268933430571,36.8125991180322,15.223310985439));
#49850=CARTESIAN_POINT('Ctrl Pts',(-0.313589884805409,36.9500999494832,
15.3453524453448));
#49851=CARTESIAN_POINT('Ctrl Pts',(-1.33460222484412,37.0862008600325,14.8546709092959));
#49852=CARTESIAN_POINT('Ctrl Pts',(-1.9389913058824,37.2210918073491,13.9079028729921));
#49853=CARTESIAN_POINT('Ctrl Pts',(-1.95313596076338,37.3549731454022,12.7931480427377));
#49854=CARTESIAN_POINT('Ctrl Pts',(-1.38009834448925,37.4880508272381,11.8449932581528));
#49855=CARTESIAN_POINT('Ctrl Pts',(-0.398696377261994,37.6205214803867,
11.3415664103564));
#49856=CARTESIAN_POINT('Ctrl Pts',(0.697374924249768,37.7526088351928,11.4330095302377));
#49857=CARTESIAN_POINT('Ctrl Pts',(1.58056764036826,37.8845086595957,12.0856666535639));
#49858=CARTESIAN_POINT('Ctrl Pts',(1.98643119115913,38.0164462603624,13.1069001843313));
#49859=CARTESIAN_POINT('Ctrl Pts',(1.79269418057024,38.1486279874099,14.1903655222649));
#49860=CARTESIAN_POINT('Ctrl Pts',(1.05482793646247,38.2812664116301,15.0121514189598));
#49861=CARTESIAN_POINT('Ctrl Pts',(-0.0114532336448994,38.4145698787582,
15.3225526040293));
#49862=CARTESIAN_POINT('Ctrl Pts',(-1.0861215985392,38.5487409348208,15.021664087747));
#49863=CARTESIAN_POINT('Ctrl Pts',(-1.93671848148375,38.6990185624443,14.1026504671256));
#49864=CARTESIAN_POINT('Ctrl Pts',(-2.07650243698238,38.86612914173,12.6778593137538));
#49865=CARTESIAN_POINT('Ctrl Pts',(-1.12551258987084,39.0511373604624,11.4047852675546));
#49866=CARTESIAN_POINT('Ctrl Pts',(0.4607598757215,39.2392795045397,11.1048892640904));
#49867=CARTESIAN_POINT('Ctrl Pts',(1.62760400148641,39.3990057193203,11.8236619012656));
#49868=CARTESIAN_POINT('Ctrl Pts',(2.0938394607673,39.5287396214468,12.7736718611132));
#49869=CARTESIAN_POINT('Ctrl Pts',(2.19353283911017,39.6598294942784,13.8380654049421));
#49870=CARTESIAN_POINT('Ctrl Pts',(1.6846576891843,39.79303861733,14.8593649757452));
#49871=CARTESIAN_POINT('Ctrl Pts',(0.740075654947661,39.9285200500448,15.4348834195735));
#49872=CARTESIAN_POINT('Ctrl Pts',(0.123095879794312,40.0056055366311,15.5477256714831));
#49873=CARTESIAN_POINT('Ctrl Pts',(-0.291600475733375,40.0573700918359,
15.5256209426602));
#49874=CARTESIAN_POINT('Ctrl Pts',(-0.566172269880012,40.0919814457418,
15.4853779270059));
#49875=CARTESIAN_POINT('Ctrl Pts',(-0.901835021996476,40.1354352807384,
15.3875664482714));
#49876=CARTESIAN_POINT('Ctrl Pts',(-1.27799293375482,40.18788560278,15.1963044726091));
#49877=CARTESIAN_POINT('Ctrl Pts',(-1.95229354247097,40.2934117578129,14.6814592260479));
#49878=CARTESIAN_POINT('Ctrl Pts',(-2.56508844947758,40.45405298046,13.4448209354256));
#49879=CARTESIAN_POINT('Ctrl Pts',(-2.09703843473412,40.6490783745322,11.8430651193419));
#49880=CARTESIAN_POINT('Ctrl Pts',(-0.641075622002351,40.8729345720558,
10.6875561846728));
#49881=CARTESIAN_POINT('Ctrl Pts',(0.851722395479298,41.0401114613552,10.7770645861692));
#49882=CARTESIAN_POINT('Ctrl Pts',(1.89831403590967,41.2022265499563,11.5593505456222));
#49883=CARTESIAN_POINT('Ctrl Pts',(2.48811446991572,41.319977610383,12.319181588701));
#49884=CARTESIAN_POINT('Ctrl Pts',(2.72223025452621,41.4843619614282,13.6702934200658));
#49885=CARTESIAN_POINT('Ctrl Pts',(2.15401136296883,41.6667653976404,15.0779383412421));
#49886=CARTESIAN_POINT('Ctrl Pts',(0.907624285699337,41.8522180563816,15.9911381082045));
#49887=CARTESIAN_POINT('Ctrl Pts',(-0.656587669756328,42.0406782429216,
16.1110089393486));
#49888=CARTESIAN_POINT('Ctrl Pts',(-2.07066924854409,42.2320913325556,15.3768629495027));
#49889=CARTESIAN_POINT('Ctrl Pts',(-2.964273683163,42.4423170978249,13.8720290136556));
#49890=CARTESIAN_POINT('Ctrl Pts',(-2.86095844370172,42.5901323550855,12.6217641358473));
#49891=CARTESIAN_POINT('Ctrl Pts',(-2.57705071309201,42.6728266944004,12.0215503795327));
#49892=CARTESIAN_POINT('Ctrl Pts',(-2.12643095010913,33.9958087341176,11.9840078835159));
#49893=CARTESIAN_POINT('Ctrl Pts',(-1.86313043212967,34.0549478062971,11.5900597397185));
#49894=CARTESIAN_POINT('Ctrl Pts',(-1.12108236258647,34.1706725163719,10.9729447862239));
#49895=CARTESIAN_POINT('Ctrl Pts',(0.278226080119438,34.3401757640595,10.7865213970534));
#49896=CARTESIAN_POINT('Ctrl Pts',(1.53021244551289,34.5050391272781,11.3498798628842));
#49897=CARTESIAN_POINT('Ctrl Pts',(2.28222248981525,34.6666728115709,12.4662052754075));
#49898=CARTESIAN_POINT('Ctrl Pts',(2.33217736198906,34.8251485661237,13.7848601993824));
#49899=CARTESIAN_POINT('Ctrl Pts',(1.69173978411777,34.9805529043229,14.9098468399839));
#49900=CARTESIAN_POINT('Ctrl Pts',(0.577631532470381,35.1329873727333,15.5159755656414));
#49901=CARTESIAN_POINT('Ctrl Pts',(-0.806278613431565,35.2991866417561,
15.4389067078018));
#49902=CARTESIAN_POINT('Ctrl Pts',(-1.65475937190052,35.4293197308722,14.7172235973626));
#49903=CARTESIAN_POINT('Ctrl Pts',(-1.95904808969561,35.5255116030304,14.0049174339565));
#49904=CARTESIAN_POINT('Ctrl Pts',(-2.0716016077322,35.5892705421757,13.5048766218472));
#49905=CARTESIAN_POINT('Ctrl Pts',(-2.02238960792956,35.6999055885991,12.603094946356));
#49906=CARTESIAN_POINT('Ctrl Pts',(-1.25414481706918,35.8553719294284,11.5146016391112));
#49907=CARTESIAN_POINT('Ctrl Pts',(0.27920281314709,36.0382214203591,11.175673388946));
#49908=CARTESIAN_POINT('Ctrl Pts',(1.61330932358228,36.2177961873488,11.9503845623713));
#49909=CARTESIAN_POINT('Ctrl Pts',(2.03194528052665,36.3798408973854,13.2742025472996));
#49910=CARTESIAN_POINT('Ctrl Pts',(1.62420263825162,36.5254748026605,14.4184265422655));
#49911=CARTESIAN_POINT('Ctrl Pts',(0.781326152623479,36.6554670407941,15.0959374367363));
#49912=CARTESIAN_POINT('Ctrl Pts',(-0.286688644223147,36.7846007840884,
15.2252003150539));
#49913=CARTESIAN_POINT('Ctrl Pts',(-1.25711440246,36.913103660952,14.7751939317609));
#49914=CARTESIAN_POINT('Ctrl Pts',(-1.84354093572621,37.0412011823262,13.8840686199387));
#49915=CARTESIAN_POINT('Ctrl Pts',(-1.87188737967761,37.1691262965253,12.8190719187284));
#49916=CARTESIAN_POINT('Ctrl Pts',(-1.33343683684623,37.2971133369783,11.8994574059213));
#49917=CARTESIAN_POINT('Ctrl Pts',(-0.38994446450294,37.4253818867507,11.3987819008321));
#49918=CARTESIAN_POINT('Ctrl Pts',(0.680126151559037,37.5541769668892,11.4731374432319));
#49919=CARTESIAN_POINT('Ctrl Pts',(1.5563033996134,37.6837086352313,12.1021375871384));
#49920=CARTESIAN_POINT('Ctrl Pts',(1.97160737963077,37.8142143373832,13.1068457061496));
#49921=CARTESIAN_POINT('Ctrl Pts',(1.79318084652126,37.9459067826252,14.1889758126573));
#49922=CARTESIAN_POINT('Ctrl Pts',(1.06378017771889,38.0790009694848,15.0235181022458));
#49923=CARTESIAN_POINT('Ctrl Pts',(-0.00963535897479482,38.2137030271988,
15.3514128269322));
#49924=CARTESIAN_POINT('Ctrl Pts',(-1.10705126196939,38.3502091559204,15.0593863069105));
#49925=CARTESIAN_POINT('Ctrl Pts',(-1.99014819519003,38.5041087158611,14.1293791042958));
#49926=CARTESIAN_POINT('Ctrl Pts',(-2.1535121009612,38.6765012268785,12.6613714256366));
#49927=CARTESIAN_POINT('Ctrl Pts',(-1.18166338991789,38.8688411745739,11.3252086672135));
#49928=CARTESIAN_POINT('Ctrl Pts',(0.47547534843363,39.0658223925045,10.9908234310914));
#49929=CARTESIAN_POINT('Ctrl Pts',(1.71389390244653,39.2341096660681,11.7336385862284));
#49930=CARTESIAN_POINT('Ctrl Pts',(2.21804743545955,39.3713654144385,12.7335482735547));
#49931=CARTESIAN_POINT('Ctrl Pts',(2.33579237140079,39.5104103687383,13.8613935824697));
#49932=CARTESIAN_POINT('Ctrl Pts',(1.80597993557594,39.6521995983019,14.954457624051));
#49933=CARTESIAN_POINT('Ctrl Pts',(0.803743705869504,39.7968310039704,15.579136084705));
#49934=CARTESIAN_POINT('Ctrl Pts',(0.145137781340595,39.8792661319018,15.7063744258721));
#49935=CARTESIAN_POINT('Ctrl Pts',(-0.299018907247705,39.9346774906494,
15.6870410488163));
#49936=CARTESIAN_POINT('Ctrl Pts',(-0.593465569836916,39.971740537626,15.6468000021472));
#49937=CARTESIAN_POINT('Ctrl Pts',(-0.954126633495691,40.0182978606449,
15.5454870688567));
#49938=CARTESIAN_POINT('Ctrl Pts',(-1.35941704706874,40.0745334215935,15.3442903100708));
#49939=CARTESIAN_POINT('Ctrl Pts',(-2.08810709033953,40.1877437326795,14.7988756611499));
#49940=CARTESIAN_POINT('Ctrl Pts',(-2.75945990414063,40.3603347398146,13.4765558908418));
#49941=CARTESIAN_POINT('Ctrl Pts',(-2.27189518256189,40.5701983336878,11.7481202050619));
#49942=CARTESIAN_POINT('Ctrl Pts',(-0.71505558939283,40.8112673567543,10.4895333119812));
#49943=CARTESIAN_POINT('Ctrl Pts',(0.894147056368231,40.9913790513282,10.5718969776429));
#49944=CARTESIAN_POINT('Ctrl Pts',(2.02862164265135,41.165985046115,11.4048511746087));
#49945=CARTESIAN_POINT('Ctrl Pts',(2.67070223394375,41.2927862700951,12.217726134071));
#49946=CARTESIAN_POINT('Ctrl Pts',(2.9347113592399,41.4697111244126,13.6698997468364));
#49947=CARTESIAN_POINT('Ctrl Pts',(2.33593192522078,41.6658496117512,15.1885451984014));
#49948=CARTESIAN_POINT('Ctrl Pts',(1.00502478148663,41.8650282538322,16.1799960875252));
#49949=CARTESIAN_POINT('Ctrl Pts',(-0.671549501876531,42.0671391690486,
16.3216105635603));
#49950=CARTESIAN_POINT('Ctrl Pts',(-2.1915100880232,42.272064173692,15.54718564601));
#49951=CARTESIAN_POINT('Ctrl Pts',(-3.15842522766362,42.4966893660946,13.9463983336952));
#49952=CARTESIAN_POINT('Ctrl Pts',(-3.05793032996539,42.6542445660225,12.6128354003429));
#49953=CARTESIAN_POINT('Ctrl Pts',(-2.76065477977972,42.7422529609897,11.9717870516811));
#49954=CARTESIAN_POINT('Ctrl Pts',(-2.10782919047724,33.9999546381749,11.9560483405783));
#49955=CARTESIAN_POINT('Ctrl Pts',(-2.03273535221384,34.0164964355435,11.847021833405));
#49956=CARTESIAN_POINT('Ctrl Pts',(-1.9492165505024,34.0329315510199,11.7440383142592));
#49957=CARTESIAN_POINT('Ctrl Pts',(-1.85841109175917,34.0493013566143,11.6484909358993));
#49958=CARTESIAN_POINT('Ctrl Pts',(-1.76710699104391,34.065761054075,11.552418876162));
#49959=CARTESIAN_POINT('Ctrl Pts',(-1.66843721253304,34.0821547324428,11.4638653656978));
#49960=CARTESIAN_POINT('Ctrl Pts',(-1.56358057298744,34.0985279043319,11.3841998154946));
#49961=CARTESIAN_POINT('Ctrl Pts',(-1.54652083475084,34.1011917511587,11.3712385625035));
#49962=CARTESIAN_POINT('Ctrl Pts',(-1.52929735445489,34.1038550623631,11.358512463993));
#49963=CARTESIAN_POINT('Ctrl Pts',(-1.51191522969689,34.1065180422329,11.3460272877833));
#49964=CARTESIAN_POINT('Ctrl Pts',(-1.40365743100421,34.1231033758838,11.2682682271638));
#49965=CARTESIAN_POINT('Ctrl Pts',(-1.28924662839032,34.1396755903245,11.1998585707924));
#49966=CARTESIAN_POINT('Ctrl Pts',(-1.17049154474186,34.1562860535771,11.1411548406653));
#49967=CARTESIAN_POINT('Ctrl Pts',(-1.1348996732179,34.1612643455026,11.1235608517895));
#49968=CARTESIAN_POINT('Ctrl Pts',(-1.09891749700162,34.1662460952939,11.1068383518619));
#49969=CARTESIAN_POINT('Ctrl Pts',(-1.06259342015375,34.1712327416556,11.0909960745263));
#49970=CARTESIAN_POINT('Ctrl Pts',(-0.93062390262081,34.189349797107,11.0334392725913));
#49971=CARTESIAN_POINT('Ctrl Pts',(-0.79383698357811,34.2072493013734,10.9875977444433));
#49972=CARTESIAN_POINT('Ctrl Pts',(-0.654538430841714,34.225032705138,10.9539518906291));
#49973=CARTESIAN_POINT('Ctrl Pts',(-0.51123900890397,34.2433268756767,10.9193396760192));
#49974=CARTESIAN_POINT('Ctrl Pts',(-0.365282556606137,34.2614981852811,
10.8976324138633));
#49975=CARTESIAN_POINT('Ctrl Pts',(-0.219137538585945,34.2796641606059,
10.8893180979243));
#49976=CARTESIAN_POINT('Ctrl Pts',(-0.143501639810857,34.2890657802398,
10.8850151065034));
#49977=CARTESIAN_POINT('Ctrl Pts',(-0.0678144599389599,34.2984660849497,
10.8842989483639));
#49978=CARTESIAN_POINT('Ctrl Pts',(0.0075869599259221,34.3078820684392,
10.8872355795483));
#49979=CARTESIAN_POINT('Ctrl Pts',(0.0908171073773173,34.3182756882892,
10.8904771132877));
#49980=CARTESIAN_POINT('Ctrl Pts',(0.173699009113757,34.328688403995,10.8981692516035));
#49981=CARTESIAN_POINT('Ctrl Pts',(0.255827425286371,34.3391437244705,10.9101052218915));
#49982=CARTESIAN_POINT('Ctrl Pts',(0.404667353738437,34.3580917235193,10.9317365773525));
#49983=CARTESIAN_POINT('Ctrl Pts',(0.550960479222043,34.3768611210909,10.9674728990995));
#49984=CARTESIAN_POINT('Ctrl Pts',(0.692327527943376,34.3955106167962,11.0161108799022));
#49985=CARTESIAN_POINT('Ctrl Pts',(0.835342138318517,34.4143774629681,11.0653157118404));
#49986=CARTESIAN_POINT('Ctrl Pts',(0.973316893376609,34.4331216111008,11.1277245401747));
#49987=CARTESIAN_POINT('Ctrl Pts',(1.10380084494927,34.4518066391112,11.2021423942935));
#49988=CARTESIAN_POINT('Ctrl Pts',(1.22566726657539,34.4692576549195,11.2716454824299));
#49989=CARTESIAN_POINT('Ctrl Pts',(1.34100105104289,34.4866571411023,11.3516243731409));
#49990=CARTESIAN_POINT('Ctrl Pts',(1.44779387776708,34.5040588762033,11.4411450268477));
#49991=CARTESIAN_POINT('Ctrl Pts',(1.44978479354124,34.5043832930202,11.4428139412031));
#49992=CARTESIAN_POINT('Ctrl Pts',(1.45177270423769,34.5047077106641,11.4444861388728));
#49993=CARTESIAN_POINT('Ctrl Pts',(1.45375759680208,34.5050321288439,11.4461616137071));
#49994=CARTESIAN_POINT('Ctrl Pts',(1.58859138980106,34.5270698625166,11.5599766538967));
#49995=CARTESIAN_POINT('Ctrl Pts',(1.70950255399661,34.5491105540052,11.6889128162493));
#49996=CARTESIAN_POINT('Ctrl Pts',(1.8145138197773,34.5710601364776,11.8290114666171));
#49997=CARTESIAN_POINT('Ctrl Pts',(1.92639920057061,34.5944465548293,11.978281078106));
#49998=CARTESIAN_POINT('Ctrl Pts',(2.02023435097168,34.6177295466144,12.1402246339982));
#49999=CARTESIAN_POINT('Ctrl Pts',(2.09357098283322,34.640788687189,12.3100512487185));
#50000=CARTESIAN_POINT('Ctrl Pts',(2.12046074090695,34.6492435984073,12.3723202194688));
#50001=CARTESIAN_POINT('Ctrl Pts',(2.14459417887735,34.6576683536396,12.4356488050096));
#50002=CARTESIAN_POINT('Ctrl Pts',(2.16584912590779,34.6660568151005,12.4997999582565));
#50003=CARTESIAN_POINT('Ctrl Pts',(2.1925649769702,34.6766004728527,12.5804330764277));
#50004=CARTESIAN_POINT('Ctrl Pts',(2.21476956359949,34.6871683815634,12.6623760906023));
#50005=CARTESIAN_POINT('Ctrl Pts',(2.23220764994495,34.6977437180901,12.7451481318184));
#50006=CARTESIAN_POINT('Ctrl Pts',(2.26060785934909,34.7149670398428,12.8799532507274));
#50007=CARTESIAN_POINT('Ctrl Pts',(2.27636242604132,34.7322101696369,13.0169582802029));
#50008=CARTESIAN_POINT('Ctrl Pts',(2.27987051823402,34.7493987123355,13.1539104307647));
#50009=CARTESIAN_POINT('Ctrl Pts',(2.28339206483647,34.7666531773884,13.2913878270299));
#50010=CARTESIAN_POINT('Ctrl Pts',(2.27457274402304,34.783852614774,13.4288102577253));
#50011=CARTESIAN_POINT('Ctrl Pts',(2.25386591578396,34.8009197707479,13.5638866209621));
#50012=CARTESIAN_POINT('Ctrl Pts',(2.24413352999502,34.8089414795457,13.6273736631499));
#50013=CARTESIAN_POINT('Ctrl Pts',(2.23177583441848,34.8169339396777,13.6903424211484));
#50014=CARTESIAN_POINT('Ctrl Pts',(2.21684385546882,34.8248889990484,13.7525557655596));
#50015=CARTESIAN_POINT('Ctrl Pts',(2.19007127872373,34.8391521746284,13.8641023692237));
#50016=CARTESIAN_POINT('Ctrl Pts',(2.1549944411202,34.8534168700116,13.9734539700032));
#50017=CARTESIAN_POINT('Ctrl Pts',(2.11185539310998,34.8676662265314,14.0791836053381));
#50018=CARTESIAN_POINT('Ctrl Pts',(2.0933089549537,34.873792342467,14.1246391319079));
#50019=CARTESIAN_POINT('Ctrl Pts',(2.07327301275871,34.8799156238577,14.1694252158986));
#50020=CARTESIAN_POINT('Ctrl Pts',(2.05176971917693,34.886034734027,14.2134289597084));
#50021=CARTESIAN_POINT('Ctrl Pts',(2.00178921632222,34.9002574949319,14.3157076750474));
#50022=CARTESIAN_POINT('Ctrl Pts',(1.94387841983718,34.9144577161843,14.4137577970048));
#50023=CARTESIAN_POINT('Ctrl Pts',(1.87908721990913,34.9286187143673,14.5066422832625));
#50024=CARTESIAN_POINT('Ctrl Pts',(1.81413095811237,34.9428157890673,14.5997634017618));
#50025=CARTESIAN_POINT('Ctrl Pts',(1.74226018673928,34.9569734394458,14.6876916058643));
#50026=CARTESIAN_POINT('Ctrl Pts',(1.66456928421305,34.9710749335319,14.7695187972507));
#50027=CARTESIAN_POINT('Ctrl Pts',(1.64740712450417,34.9741899970177,14.7875946759114));
#50028=CARTESIAN_POINT('Ctrl Pts',(1.62996106027555,34.9773023205237,14.8053730065465));
#50029=CARTESIAN_POINT('Ctrl Pts',(1.6122430516455,34.9804117242923,14.8228443067699));
#50030=CARTESIAN_POINT('Ctrl Pts',(1.52088799773868,34.9964439858645,14.912927318188));
#50031=CARTESIAN_POINT('Ctrl Pts',(1.42202916652567,35.0124052328162,14.995098404239));
#50032=CARTESIAN_POINT('Ctrl Pts',(1.31718349483541,35.0283135985736,15.0679803984461));
#50033=CARTESIAN_POINT('Ctrl Pts',(1.2258607493309,35.0421701137166,15.1314621206911));
#50034=CARTESIAN_POINT('Ctrl Pts',(1.12999721080024,35.0559865271651,15.1878964571));
#50035=CARTESIAN_POINT('Ctrl Pts',(1.03061700120121,35.0697753328408,15.2363970979685));
#50036=CARTESIAN_POINT('Ctrl Pts',(0.915725435099798,35.0857163082637,15.2924677644401));
#50037=CARTESIAN_POINT('Ctrl Pts',(0.796134489436802,35.1016203778816,15.3379334682777));
#50038=CARTESIAN_POINT('Ctrl Pts',(0.673885991351223,35.117507612992,15.3726835629812));
#50039=CARTESIAN_POINT('Ctrl Pts',(0.634695361371716,35.1226007696554,15.38382380703));
#50040=CARTESIAN_POINT('Ctrl Pts',(0.595231663506183,35.1276922011631,15.3938631791469));
#50041=CARTESIAN_POINT('Ctrl Pts',(0.555562200299993,35.1327825820645,15.4027991621468));
#50042=CARTESIAN_POINT('Ctrl Pts',(0.427915219441533,35.1491622277912,15.4315530488584));
#50043=CARTESIAN_POINT('Ctrl Pts',(0.29792052998284,35.1654493899942,15.4489072536342));
#50044=CARTESIAN_POINT('Ctrl Pts',(0.167804766505765,35.1816687993293,15.4547071197683));
#50045=CARTESIAN_POINT('Ctrl Pts',(0.0376874216217125,35.1978884057927,
15.460507056393));
#50046=CARTESIAN_POINT('Ctrl Pts',(-0.0925495030302005,35.2140402692686,
15.4547524213929));
#50047=CARTESIAN_POINT('Ctrl Pts',(-0.220677358214982,35.2301498780449,
15.437339170878));
#50048=CARTESIAN_POINT('Ctrl Pts',(-0.271299343155901,35.2365146171697,
15.4304593764409));
#50049=CARTESIAN_POINT('Ctrl Pts',(-0.321592212096991,35.2428727678739,
15.4217602732624));
#50050=CARTESIAN_POINT('Ctrl Pts',(-0.371419217300234,35.2492259284662,
15.4112376094421));
#50051=CARTESIAN_POINT('Ctrl Pts',(-0.457972173071773,35.2602618080162,
15.3929590142803));
#50052=CARTESIAN_POINT('Ctrl Pts',(-0.543119017933009,35.2712826251268,
15.3691775932306));
#50053=CARTESIAN_POINT('Ctrl Pts',(-0.626284090550383,35.2822968674306,
15.3403038136358));
#50054=CARTESIAN_POINT('Ctrl Pts',(-0.773088044699655,35.301739336141,15.2893354818309));
#50055=CARTESIAN_POINT('Ctrl Pts',(-0.913980015554586,35.321099528776,15.2223949186247));
#50056=CARTESIAN_POINT('Ctrl Pts',(-1.04581618355905,35.340384350165,15.1415968138546));
#50057=CARTESIAN_POINT('Ctrl Pts',(-1.18127774119407,35.3601994887845,15.0585768255479));
#50058=CARTESIAN_POINT('Ctrl Pts',(-1.30717699825575,35.3799350595191,14.9609275733912));
#50059=CARTESIAN_POINT('Ctrl Pts',(-1.42012179785065,35.3995989528989,14.8509929840464));
#50060=CARTESIAN_POINT('Ctrl Pts',(-1.46858614366081,35.4080366829419,14.80382031232));
#50061=CARTESIAN_POINT('Ctrl Pts',(-1.51466562117316,35.4164612198121,14.7543861378517));
#50062=CARTESIAN_POINT('Ctrl Pts',(-1.55809436667318,35.4248732044062,14.7028777079071));
#50063=CARTESIAN_POINT('Ctrl Pts',(-1.64900693489217,35.4424826267938,14.5950513454996));
#50064=CARTESIAN_POINT('Ctrl Pts',(-1.72830137475248,35.4600370350596,14.4781348494354));
#50065=CARTESIAN_POINT('Ctrl Pts',(-1.79511211395845,35.4775425369219,14.3549260254373));
#50066=CARTESIAN_POINT('Ctrl Pts',(-1.85648490514971,35.4936232078328,14.2417455769341));
#50067=CARTESIAN_POINT('Ctrl Pts',(-1.9073467947352,35.5096393678861,14.123213423905));
#50068=CARTESIAN_POINT('Ctrl Pts',(-1.94703030634917,35.5256205098076,14.0014818662496));
#50069=CARTESIAN_POINT('Ctrl Pts',(-1.9746954648963,35.5367616817212,13.9166173291721));
#50070=CARTESIAN_POINT('Ctrl Pts',(-1.99692889193797,35.547884525986,13.8302101887822));
#50071=CARTESIAN_POINT('Ctrl Pts',(-2.01352118408605,35.5589884385217,13.742879251034));
#50072=CARTESIAN_POINT('Ctrl Pts',(-2.02072924056195,35.5638122222368,13.7049407717833));
#50073=CARTESIAN_POINT('Ctrl Pts',(-2.02687204406997,35.5686324306605,13.6668278286596));
#50074=CARTESIAN_POINT('Ctrl Pts',(-2.03192934439831,35.5734490038586,13.6285909314804));
#50075=CARTESIAN_POINT('Ctrl Pts',(-2.04014579325388,35.5812743503423,13.5664685559697));
#50076=CARTESIAN_POINT('Ctrl Pts',(-2.04549409264654,35.589082667069,13.5040325687331));
#50077=CARTESIAN_POINT('Ctrl Pts',(-2.04788332093059,35.5968769086578,13.4415650199189));
#50078=CARTESIAN_POINT('Ctrl Pts',(-2.05154446858571,35.6088204594296,13.3458425134561));
#50079=CARTESIAN_POINT('Ctrl Pts',(-2.0482546344716,35.6207309551597,13.2500464480908));
#50080=CARTESIAN_POINT('Ctrl Pts',(-2.03835097321585,35.6326192116472,13.1551583079904));
#50081=CARTESIAN_POINT('Ctrl Pts',(-2.0284473119601,35.6445074681347,13.06027016789));
#50082=CARTESIAN_POINT('Ctrl Pts',(-2.0119302656843,35.6563734905405,12.966291131447));
#50083=CARTESIAN_POINT('Ctrl Pts',(-1.98918917550094,35.6682281905391,12.8741894258666));
#50084=CARTESIAN_POINT('Ctrl Pts',(-1.96162155315965,35.6825989128702,12.7625402034258));
#50085=CARTESIAN_POINT('Ctrl Pts',(-1.92481653315395,35.69693732528,12.6532517716315));
#50086=CARTESIAN_POINT('Ctrl Pts',(-1.87932281509479,35.7112429296544,12.54797575677));
#50087=CARTESIAN_POINT('Ctrl Pts',(-1.83301509,35.7258045004151,12.4408160660861));
#50088=CARTESIAN_POINT('Ctrl Pts',(-1.77770530153866,35.7403320813291,12.3378150814881));
#50089=CARTESIAN_POINT('Ctrl Pts',(-1.71402428391801,35.754825300147,12.2407074433751));
#50090=CARTESIAN_POINT('Ctrl Pts',(-1.69861786353295,35.7583316609148,12.2172140830101));
#50091=CARTESIAN_POINT('Ctrl Pts',(-1.68272169122856,35.7618360110277,12.1940655747937));
#50092=CARTESIAN_POINT('Ctrl Pts',(-1.66634511075174,35.7653383462395,12.1712862720119));
#50093=CARTESIAN_POINT('Ctrl Pts',(-1.59611327140501,35.7803582977047,12.0735960163649));
#50094=CARTESIAN_POINT('Ctrl Pts',(-1.51704280174011,35.7953411852278,11.9826996171978));
#50095=CARTESIAN_POINT('Ctrl Pts',(-1.43083543098776,35.8102867488178,11.8996820965413));
#50096=CARTESIAN_POINT('Ctrl Pts',(-1.34462806023541,35.8252323124077,11.8166645758849));
#50097=CARTESIAN_POINT('Ctrl Pts',(-1.25128529133472,35.8401405559852,11.7415269159067));
#50098=CARTESIAN_POINT('Ctrl Pts',(-1.15253542916576,35.855011268336,11.6753007627733));
#50099=CARTESIAN_POINT('Ctrl Pts',(-1.06327096491324,35.868453577438,11.6154359493029));
#50100=CARTESIAN_POINT('Ctrl Pts',(-0.969313042202289,35.8818470131201,
11.5626566717203));
#50101=CARTESIAN_POINT('Ctrl Pts',(-0.871894961021909,35.8952019643656,
11.5178284930221));
#50102=CARTESIAN_POINT('Ctrl Pts',(-0.785413590500806,35.907057612444,11.4780329819136));
#50103=CARTESIAN_POINT('Ctrl Pts',(-0.696206613574874,35.9188829352861,
11.4445035168071));
#50104=CARTESIAN_POINT('Ctrl Pts',(-0.605160422711497,35.9306851646132,
11.4178206318541));
#50105=CARTESIAN_POINT('Ctrl Pts',(-0.502376287738908,35.9440089722392,
11.3876977104835));
#50106=CARTESIAN_POINT('Ctrl Pts',(-0.397248796987259,35.9573033556558,
11.3663019080391));
#50107=CARTESIAN_POINT('Ctrl Pts',(-0.2912851877516,35.9705786660213,11.3535055397407));
#50108=CARTESIAN_POINT('Ctrl Pts',(-0.186014828194546,35.983767124828,11.3407928896007));
#50109=CARTESIAN_POINT('Ctrl Pts',(-0.0799206249175964,35.9969367649317,
11.3365673951363));
#50110=CARTESIAN_POINT('Ctrl Pts',(0.0255194181043174,36.0100975095415,
11.3406537309221));
#50111=CARTESIAN_POINT('Ctrl Pts',(0.0995112658213549,36.0193329743905,
11.3435212898353));
#50112=CARTESIAN_POINT('Ctrl Pts',(0.173180945864884,36.0285640540735,11.3504809179512));
#50113=CARTESIAN_POINT('Ctrl Pts',(0.246023155369535,36.0377940886885,11.361457586701));
#50114=CARTESIAN_POINT('Ctrl Pts',(0.349173102021139,36.0508644991635,11.3770013600661));
#50115=CARTESIAN_POINT('Ctrl Pts',(0.451060390357706,36.0638869807897,11.4006369620851));
#50116=CARTESIAN_POINT('Ctrl Pts',(0.550226705112536,36.0768748402712,11.4322888224452));
#50117=CARTESIAN_POINT('Ctrl Pts',(0.591720584632716,36.0823093134376,11.4455328205066));
#50118=CARTESIAN_POINT('Ctrl Pts',(0.632737888490082,36.0877377222362,11.4601797002687));
#50119=CARTESIAN_POINT('Ctrl Pts',(0.673171354865221,36.0931610280814,11.4762212759687));
#50120=CARTESIAN_POINT('Ctrl Pts',(0.769601574921968,36.1060951300264,11.514479006841));
#50121=CARTESIAN_POINT('Ctrl Pts',(0.862709909997599,36.1190002327184,11.5606731839098));
#50122=CARTESIAN_POINT('Ctrl Pts',(0.951463450775792,36.1318891699932,11.6138795055761));
#50123=CARTESIAN_POINT('Ctrl Pts',(1.04120770432058,36.1449219802289,11.667679743628));
#50124=CARTESIAN_POINT('Ctrl Pts',(1.12649832144998,36.1579382696876,11.7286487883445));
#50125=CARTESIAN_POINT('Ctrl Pts',(1.20629091800974,36.1709508742725,11.7957833557257));
#50126=CARTESIAN_POINT('Ctrl Pts',(1.28445287897005,36.1836975542329,11.8615459660551));
#50127=CARTESIAN_POINT('Ctrl Pts',(1.35733834381253,36.1964407026541,11.9332237535062));
#50128=CARTESIAN_POINT('Ctrl Pts',(1.4240025218212,36.2091918877558,12.0098410593243));
#50129=CARTESIAN_POINT('Ctrl Pts',(1.4388154544048,36.2120252302032,12.0268655996355));
#50130=CARTESIAN_POINT('Ctrl Pts',(1.4533213947603,36.2148589673348,12.0441339234977));
#50131=CARTESIAN_POINT('Ctrl Pts',(1.46751030002944,36.2176932223302,12.0616351716412));
#50132=CARTESIAN_POINT('Ctrl Pts',(1.52735459729779,36.229647209989,12.1354498794426));
#50133=CARTESIAN_POINT('Ctrl Pts',(1.58173333528113,36.2415626030895,12.2135799447662));
#50134=CARTESIAN_POINT('Ctrl Pts',(1.62985222800578,36.2534408955121,12.2952946960849));
#50135=CARTESIAN_POINT('Ctrl Pts',(1.69177523284277,36.2687267742489,12.4004513747749));
#50136=CARTESIAN_POINT('Ctrl Pts',(1.74332943193823,36.2839512176407,12.5115451983607));
#50137=CARTESIAN_POINT('Ctrl Pts',(1.78392093449125,36.2991174457196,12.6263368155275));
#50138=CARTESIAN_POINT('Ctrl Pts',(1.82514202908956,36.314518908662,12.7429089011296));
#50139=CARTESIAN_POINT('Ctrl Pts',(1.85505715911335,36.3298603418756,12.8632928281798));
#50140=CARTESIAN_POINT('Ctrl Pts',(1.87309126705035,36.3451449889762,12.9851207938013));
#50141=CARTESIAN_POINT('Ctrl Pts',(1.87843564658592,36.3496745701153,13.0212243198866));
#50142=CARTESIAN_POINT('Ctrl Pts',(1.88273694666996,36.3541991630102,13.0574546029022));
#50143=CARTESIAN_POINT('Ctrl Pts',(1.88598108934285,36.3587188488552,13.0937499627023));
#50144=CARTESIAN_POINT('Ctrl Pts',(1.89453315073255,36.3706334391511,13.1894301397075));
#50145=CARTESIAN_POINT('Ctrl Pts',(1.89573743070339,36.3825139356724,13.2855620769068));
#50146=CARTESIAN_POINT('Ctrl Pts',(1.88981146057019,36.394361687848,13.3810517445343));
#50147=CARTESIAN_POINT('Ctrl Pts',(1.88326688185853,36.4074462199883,13.4865095230737));
#50148=CARTESIAN_POINT('Ctrl Pts',(1.86796407409775,36.4206150563038,13.5914000038421));
#50149=CARTESIAN_POINT('Ctrl Pts',(1.8441512360903,36.4338077285074,13.6942046335211));
#50150=CARTESIAN_POINT('Ctrl Pts',(1.8265451487186,36.4435617670394,13.770213519643));
#50151=CARTESIAN_POINT('Ctrl Pts',(1.8042883809506,36.4533288725361,13.8450820123745));
#50152=CARTESIAN_POINT('Ctrl Pts',(1.77749860781857,36.4630853279683,13.9182020409971));
#50153=CARTESIAN_POINT('Ctrl Pts',(1.74141677072747,36.4762258213109,14.0166838365633));
#50154=CARTESIAN_POINT('Ctrl Pts',(1.69711118751256,36.4893469045138,14.111991885435));
#50155=CARTESIAN_POINT('Ctrl Pts',(1.64527973583635,36.502392924998,14.2028247163159));
#50156=CARTESIAN_POINT('Ctrl Pts',(1.62833313638777,36.506658398497,14.232523047193));
#50157=CARTESIAN_POINT('Ctrl Pts',(1.61058227251594,36.5109158659881,14.2617433029065));
#50158=CARTESIAN_POINT('Ctrl Pts',(1.5920521732993,36.5151634364617,14.290441034415));
#50159=CARTESIAN_POINT('Ctrl Pts',(1.57688560628607,36.5186399997266,14.3139296333135));
#50160=CARTESIAN_POINT('Ctrl Pts',(1.56119702690944,36.5221099333285,14.3370681966813));
#50161=CARTESIAN_POINT('Ctrl Pts',(1.54500959542846,36.5255722087906,14.3598383941216));
#50162=CARTESIAN_POINT('Ctrl Pts',(1.48382006123124,36.5386598331634,14.4459112078718));
#50163=CARTESIAN_POINT('Ctrl Pts',(1.41543631336881,36.5518084567257,14.5266569385406));
#50164=CARTESIAN_POINT('Ctrl Pts',(1.34101407134697,36.5649854886612,14.6011690475079));
#50165=CARTESIAN_POINT('Ctrl Pts',(1.26616099598456,36.5782388029625,14.676112510059));
#50166=CARTESIAN_POINT('Ctrl Pts',(1.1851985792311,36.5915208413091,14.74475116306));
#50167=CARTESIAN_POINT('Ctrl Pts',(1.09925484292431,36.6048002565126,14.8061412973413));
#50168=CARTESIAN_POINT('Ctrl Pts',(1.01654823758621,36.61757949325,14.8652191292561));
#50169=CARTESIAN_POINT('Ctrl Pts',(0.929227554730378,36.6303563005821,14.9175851595059));
#50170=CARTESIAN_POINT('Ctrl Pts',(0.838266607600032,36.6431044985123,14.9623631944754));
#50171=CARTESIAN_POINT('Ctrl Pts',(0.807317111196533,36.6474420776431,14.9775989376813));
#50172=CARTESIAN_POINT('Ctrl Pts',(0.775945965359559,36.6517763601189,14.9919558429113));
#50173=CARTESIAN_POINT('Ctrl Pts',(0.744190943597326,36.6561063637833,15.0053981067694));
#50174=CARTESIAN_POINT('Ctrl Pts',(0.708189246510862,36.6610154292369,15.0206380368567));
#50175=CARTESIAN_POINT('Ctrl Pts',(0.671721621828844,36.6658870487025,15.0347110946733));
#50176=CARTESIAN_POINT('Ctrl Pts',(0.634846570587766,36.6707297013909,15.0475611518812));
#50177=CARTESIAN_POINT('Ctrl Pts',(0.540748903266454,36.6830871709072,15.0803518970467));
#50178=CARTESIAN_POINT('Ctrl Pts',(0.443994601445002,36.6952565152842,15.1051789905932));
#50179=CARTESIAN_POINT('Ctrl Pts',(0.345878901046004,36.7073738930339,15.1221280130944));
#50180=CARTESIAN_POINT('Ctrl Pts',(0.244089875378566,36.719944929777,15.1397115851363));
#50181=CARTESIAN_POINT('Ctrl Pts',(0.140835280574491,36.732460125289,15.1488145233718));
#50182=CARTESIAN_POINT('Ctrl Pts',(0.0376199817696723,36.7450631920612,
15.14954271623));
#50183=CARTESIAN_POINT('Ctrl Pts',(-0.0583978346931932,36.7567874128522,
15.1502201302279));
#50184=CARTESIAN_POINT('Ctrl Pts',(-0.154380541120703,36.7685876183003,
15.1436489919699));
#50185=CARTESIAN_POINT('Ctrl Pts',(-0.249074603876776,36.7805724777801,
15.1299423721303));
#50186=CARTESIAN_POINT('Ctrl Pts',(-0.256172857822581,36.7814708612016,
15.1289149257886));
#50187=CARTESIAN_POINT('Ctrl Pts',(-0.26326385474469,36.7823702789282,15.1278474033987));
#50188=CARTESIAN_POINT('Ctrl Pts',(-0.270347059162533,36.7832707751351,
15.1267398619482));
#50189=CARTESIAN_POINT('Ctrl Pts',(-0.359741935093517,36.7946356520945,
15.1127619326497));
#50190=CARTESIAN_POINT('Ctrl Pts',(-0.448245687484448,36.8061249358034,
15.0924190560047));
#50191=CARTESIAN_POINT('Ctrl Pts',(-0.534788423534536,36.8176479233723,
15.0658468746533));
#50192=CARTESIAN_POINT('Ctrl Pts',(-0.620971637574773,36.8291230413241,
15.0393850813539));
#50193=CARTESIAN_POINT('Ctrl Pts',(-0.705209039686781,36.8406315682017,
15.0067466198686));
#50194=CARTESIAN_POINT('Ctrl Pts',(-0.786477085132356,36.8520882771613,
14.9681038614056));
#50195=CARTESIAN_POINT('Ctrl Pts',(-0.841873113264734,36.8598976955907,
14.9417631844127));
#50196=CARTESIAN_POINT('Ctrl Pts',(-0.895890180580959,36.86768312773,14.9126334644819));
#50197=CARTESIAN_POINT('Ctrl Pts',(-0.948216350538084,36.8754187988796,
14.880775906438));
#50198=CARTESIAN_POINT('Ctrl Pts',(-1.02405932632251,36.8866310913166,14.8346006942018));
#50199=CARTESIAN_POINT('Ctrl Pts',(-1.0963476335419,36.8977386382427,14.7826952561138));
#50200=CARTESIAN_POINT('Ctrl Pts',(-1.16459156201923,36.9086668288595,14.7259270744155));
#50201=CARTESIAN_POINT('Ctrl Pts',(-1.17419518179789,36.9102046973541,14.7179383779158));
#50202=CARTESIAN_POINT('Ctrl Pts',(-1.1837187927073,36.911739021452,14.7098533772982));
#50203=CARTESIAN_POINT('Ctrl Pts',(-1.193161112349,36.913269600617,14.7016744800817));
#50204=CARTESIAN_POINT('Ctrl Pts',(-1.26635192657766,36.9251336699959,14.6382769072937));
#50205=CARTESIAN_POINT('Ctrl Pts',(-1.3344343809947,36.9370717143419,14.5690871425987));
#50206=CARTESIAN_POINT('Ctrl Pts',(-1.3968207555326,36.9490735856253,14.4951213528827));
#50207=CARTESIAN_POINT('Ctrl Pts',(-1.46021206049806,36.961268785111,14.4199641095324));
#50208=CARTESIAN_POINT('Ctrl Pts',(-1.51772331354799,36.9735298768924,14.3398747979504));
#50209=CARTESIAN_POINT('Ctrl Pts',(-1.56871064427456,36.9858473584534,14.2558725847206));
#50210=CARTESIAN_POINT('Ctrl Pts',(-1.6184835382327,36.9978714572801,14.1738711700211));
#50211=CARTESIAN_POINT('Ctrl Pts',(-1.6620403903747,37.0099492915742,14.0881398681812));
#50212=CARTESIAN_POINT('Ctrl Pts',(-1.69874329383057,37.0220731469179,13.9995984580638));
#50213=CARTESIAN_POINT('Ctrl Pts',(-1.71835034527889,37.0285498294986,13.9522987673032));
#50214=CARTESIAN_POINT('Ctrl Pts',(-1.736000678138,37.0350396648645,13.9041967447192));
#50215=CARTESIAN_POINT('Ctrl Pts',(-1.75159108002485,37.0415416140855,13.8554309174612));
#50216=CARTESIAN_POINT('Ctrl Pts',(-1.77850249502875,37.0527649715775,13.7712536509049));
#50217=CARTESIAN_POINT('Ctrl Pts',(-1.79941306612529,37.0638700466476,13.6851522039074));
#50218=CARTESIAN_POINT('Ctrl Pts',(-1.81371393571048,37.0748991615949,13.5979485978916));
#50219=CARTESIAN_POINT('Ctrl Pts',(-1.81575584668309,37.0764739239333,13.5854974669367));
#50220=CARTESIAN_POINT('Ctrl Pts',(-1.81766306122867,37.0780471322918,13.5730239342238));
#50221=CARTESIAN_POINT('Ctrl Pts',(-1.81943386595458,37.0796189044161,13.5605304574353));
#50222=CARTESIAN_POINT('Ctrl Pts',(-1.83173154207434,37.0905343623632,13.4737672311418));
#50223=CARTESIAN_POINT('Ctrl Pts',(-1.837446673463,37.1013808239721,13.3860398430746));
#50224=CARTESIAN_POINT('Ctrl Pts',(-1.83681903068068,37.1121958285686,13.2983067064745));
#50225=CARTESIAN_POINT('Ctrl Pts',(-1.83618756062209,37.1230767815225,13.2100385857045));
#50226=CARTESIAN_POINT('Ctrl Pts',(-1.82913541383387,37.1339259064831,13.1217657421755));
#50227=CARTESIAN_POINT('Ctrl Pts',(-1.81595528194813,37.1447779413162,13.0344833715383));
#50228=CARTESIAN_POINT('Ctrl Pts',(-1.8062316911794,37.1527839875864,12.970091143846));
#50229=CARTESIAN_POINT('Ctrl Pts',(-1.79317382057122,37.1607915453244,12.9062385215738));
#50230=CARTESIAN_POINT('Ctrl Pts',(-1.77691737143006,37.1688132973504,12.8433259136689));
#50231=CARTESIAN_POINT('Ctrl Pts',(-1.75273331561296,37.1807469304006,12.7497333949117));
#50232=CARTESIAN_POINT('Ctrl Pts',(-1.72125565569971,37.1928665653301,12.6578643564013));
#50233=CARTESIAN_POINT('Ctrl Pts',(-1.68292786097389,37.2050732623165,12.5689297780961));
#50234=CARTESIAN_POINT('Ctrl Pts',(-1.64473503304942,37.2172369748615,12.4803083724023));
#50235=CARTESIAN_POINT('Ctrl Pts',(-1.59974186674591,37.2294871164617,12.3946005856137));
#50236=CARTESIAN_POINT('Ctrl Pts',(-1.54838160112248,37.2417338157826,12.3129542055393));
#50237=CARTESIAN_POINT('Ctrl Pts',(-1.49815382222756,37.2537104770832,12.2331081168134));
#50238=CARTESIAN_POINT('Ctrl Pts',(-1.44183803035782,37.2656838525028,12.1571454414428));
#50239=CARTESIAN_POINT('Ctrl Pts',(-1.37981186334457,37.2775776440079,12.086099646022));
#50240=CARTESIAN_POINT('Ctrl Pts',(-1.3695906542137,37.2795376060076,12.0743921043855));
#50241=CARTESIAN_POINT('Ctrl Pts',(-1.35921428973727,37.2814954242028,12.0628180105673));
#50242=CARTESIAN_POINT('Ctrl Pts',(-1.34868434603657,37.2834507778102,12.0513819113163));
#50243=CARTESIAN_POINT('Ctrl Pts',(-1.32238196798846,37.2883349871907,12.0228160790149));
#50244=CARTESIAN_POINT('Ctrl Pts',(-1.2951214512437,37.2932038028834,11.9951112983189));
#50245=CARTESIAN_POINT('Ctrl Pts',(-1.26697452896051,37.2980523861965,11.9682910254143));
#50246=CARTESIAN_POINT('Ctrl Pts',(-1.20317523033163,37.3090424408677,11.9074987802398));
#50247=CARTESIAN_POINT('Ctrl Pts',(-1.13496692031192,37.3199204173598,11.8514198724786));
#50248=CARTESIAN_POINT('Ctrl Pts',(-1.06311008949083,37.3307657155399,11.8003937600291));
#50249=CARTESIAN_POINT('Ctrl Pts',(-0.990911241118183,37.3416626341754,
11.7491247781704));
#50250=CARTESIAN_POINT('Ctrl Pts',(-0.915027598556622,37.3525265792606,
11.7029574649945));
#50251=CARTESIAN_POINT('Ctrl Pts',(-0.836246103777801,37.3634314369721,
11.6622863877922));
#50252=CARTESIAN_POINT('Ctrl Pts',(-0.758385854858158,37.3742087767299,
11.6220909052909));
#50253=CARTESIAN_POINT('Ctrl Pts',(-0.677694116748348,37.3850260769621,
11.5872648057675));
#50254=CARTESIAN_POINT('Ctrl Pts',(-0.594963973008873,37.3959480907742,
11.5582258127621));
#50255=CARTESIAN_POINT('Ctrl Pts',(-0.521009688641192,37.4057115177287,
11.5322672219825));
#50256=CARTESIAN_POINT('Ctrl Pts',(-0.445426620962867,37.4155585399473,
11.5109340972001));
#50257=CARTESIAN_POINT('Ctrl Pts',(-0.368812822755948,37.4255308710731,
11.4945403116791));
#50258=CARTESIAN_POINT('Ctrl Pts',(-0.269224375159485,37.4384936662743,
11.4732304211831));
#50259=CARTESIAN_POINT('Ctrl Pts',(-0.167801264918345,37.4514022987213,
11.4598028010033));
#50260=CARTESIAN_POINT('Ctrl Pts',(-0.0658556672410014,37.4642758852663,
11.4548878867486));
#50261=CARTESIAN_POINT('Ctrl Pts',(-0.00409324698879404,37.4720751809737,
11.4519102495909));
#50262=CARTESIAN_POINT('Ctrl Pts',(0.0578599822949168,37.4798615625061,
11.4520566539944));
#50263=CARTESIAN_POINT('Ctrl Pts',(0.119705201033959,37.4876387920326,11.4554612490146));
#50264=CARTESIAN_POINT('Ctrl Pts',(0.22093662297219,37.5003689596958,11.4610340645377));
#50265=CARTESIAN_POINT('Ctrl Pts',(0.321879291848365,37.5130747556518,11.4753394587183));
#50266=CARTESIAN_POINT('Ctrl Pts',(0.421078028215027,37.5257702555449,11.4976990787541));
#50267=CARTESIAN_POINT('Ctrl Pts',(0.455550372083947,37.5301820419641,11.5054692232024));
#50268=CARTESIAN_POINT('Ctrl Pts',(0.489811969198873,37.5345925600645,11.5142115624586));
#50269=CARTESIAN_POINT('Ctrl Pts',(0.523801452546336,37.5390023199556,11.5238962113574));
#50270=CARTESIAN_POINT('Ctrl Pts',(0.565740826890602,37.5444434903597,11.5358460286407));
#50271=CARTESIAN_POINT('Ctrl Pts',(0.607265893251684,37.5498835092932,11.5492305637103));
#50272=CARTESIAN_POINT('Ctrl Pts',(0.648266270211475,37.5553232976998,11.5640317540731));
#50273=CARTESIAN_POINT('Ctrl Pts',(0.736204072212425,37.566990581547,11.595777417016));
#50274=CARTESIAN_POINT('Ctrl Pts',(0.821827069603859,37.5786698796599,11.6340755837756));
#50275=CARTESIAN_POINT('Ctrl Pts',(0.904090269375511,37.59036064197,11.6787707765648));
#50276=CARTESIAN_POINT('Ctrl Pts',(1.02468526577214,37.6074988938562,11.7442923783056));
#50277=CARTESIAN_POINT('Ctrl Pts',(1.13805853563312,37.6246617858551,11.8235628872294));
#50278=CARTESIAN_POINT('Ctrl Pts',(1.24183702425236,37.6418456265658,11.914126941895));
#50279=CARTESIAN_POINT('Ctrl Pts',(1.32864768216617,37.6562199014029,11.9898837318951));
#50280=CARTESIAN_POINT('Ctrl Pts',(1.40874436015618,37.6706088341558,12.0735421237424));
#50281=CARTESIAN_POINT('Ctrl Pts',(1.48013748955479,37.6850107467071,12.1641253724113));
#50282=CARTESIAN_POINT('Ctrl Pts',(1.49411662122227,37.6878307131873,12.1818620253733));
#50283=CARTESIAN_POINT('Ctrl Pts',(1.5077749468182,37.6906422060092,12.1998510629921));
#50284=CARTESIAN_POINT('Ctrl Pts',(1.52109707091888,37.6934467053931,12.2180881367112));
#50285=CARTESIAN_POINT('Ctrl Pts',(1.5689807848348,37.7035269182152,12.2836376552436));
#50286=CARTESIAN_POINT('Ctrl Pts',(1.61252495621774,37.7135173702108,12.3523942733967));
#50287=CARTESIAN_POINT('Ctrl Pts',(1.65151456542215,37.7234819098149,12.4237792308908));
#50288=CARTESIAN_POINT('Ctrl Pts',(1.68902135207338,37.7330674857833,12.4924493310911));
#50289=CARTESIAN_POINT('Ctrl Pts',(1.7223122370472,37.742629045399,12.5635522396304));
#50290=CARTESIAN_POINT('Ctrl Pts',(1.75116010543387,37.7522166977056,12.6365343098017));
#50291=CARTESIAN_POINT('Ctrl Pts',(1.77986975086396,37.7617584113096,12.7091666904438));
#50292=CARTESIAN_POINT('Ctrl Pts',(1.80417787447923,37.7713259690187,12.7836607272367));
#50293=CARTESIAN_POINT('Ctrl Pts',(1.82384013888311,37.78096218026,12.8594239654089));
#50294=CARTESIAN_POINT('Ctrl Pts',(1.84333888420058,37.7905182529971,12.9345571268395));
#50295=CARTESIAN_POINT('Ctrl Pts',(1.85826770420485,37.8001418387852,13.0109386128204));
#50296=CARTESIAN_POINT('Ctrl Pts',(1.86838300661926,37.8098682229002,13.0879401454036));
#50297=CARTESIAN_POINT('Ctrl Pts',(1.8697816564832,37.8112130967617,13.0985872005937));
#50298=CARTESIAN_POINT('Ctrl Pts',(1.87108828362893,37.8125599258635,13.1092460295507));
#50299=CARTESIAN_POINT('Ctrl Pts',(1.87230225335561,37.8139087937046,13.1199148935139));
#50300=CARTESIAN_POINT('Ctrl Pts',(1.88155220003328,37.8241866081605,13.2012072195101));
#50301=CARTESIAN_POINT('Ctrl Pts',(1.88565818101676,37.8345296782578,13.2833068905848));
#50302=CARTESIAN_POINT('Ctrl Pts',(1.88447514247342,37.8448953804118,13.3654266858299));
#50303=CARTESIAN_POINT('Ctrl Pts',(1.88330137449124,37.8551798545482,13.446902971539));
#50304=CARTESIAN_POINT('Ctrl Pts',(1.87692181961835,37.8654866069461,13.5283980941142));
#50305=CARTESIAN_POINT('Ctrl Pts',(1.86523687322021,37.8757788587898,13.6091711708453));
#50306=CARTESIAN_POINT('Ctrl Pts',(1.85565474609755,37.8842189202315,13.6754083501145));
#50307=CARTESIAN_POINT('Ctrl Pts',(1.84250587208248,37.8926493189246,13.7411603284638));
#50308=CARTESIAN_POINT('Ctrl Pts',(1.82575174022672,37.9010522336897,13.8060388875534));
#50309=CARTESIAN_POINT('Ctrl Pts',(1.80541874857518,37.9112500999378,13.8847761931739));
#50310=CARTESIAN_POINT('Ctrl Pts',(1.77977617891474,37.9214073576267,13.962225480692));
#50311=CARTESIAN_POINT('Ctrl Pts',(1.74934969868926,37.931496497684,14.0378577509446));
#50312=CARTESIAN_POINT('Ctrl Pts',(1.73443711073289,37.936441374232,14.0749265434609));
#50313=CARTESIAN_POINT('Ctrl Pts',(1.71837553799444,37.9413699612472,14.1115596261691));
#50314=CARTESIAN_POINT('Ctrl Pts',(1.7012272587251,37.9462794415417,14.1476992722481));
#50315=CARTESIAN_POINT('Ctrl Pts',(1.65536953948287,37.9594083138579,14.2443434729503));
#50316=CARTESIAN_POINT('Ctrl Pts',(1.60109742222298,37.9726277492245,14.3371931665222));
#50317=CARTESIAN_POINT('Ctrl Pts',(1.53941338370294,37.9859333601115,14.4250707321891));
#50318=CARTESIAN_POINT('Ctrl Pts',(1.47592002794693,37.9996292513967,14.5155259240626));
#50319=CARTESIAN_POINT('Ctrl Pts',(1.40457296024107,38.013416443659,14.6007146775164));
#50320=CARTESIAN_POINT('Ctrl Pts',(1.32641016648189,38.0272918876079,14.6793479109264));
#50321=CARTESIAN_POINT('Ctrl Pts',(1.25019104527154,38.040822291184,14.7560257733748));
#50322=CARTESIAN_POINT('Ctrl Pts',(1.16748988153653,38.0544366217045,14.8264716092764));
#50323=CARTESIAN_POINT('Ctrl Pts',(1.07923056703853,38.0681336113904,14.8894621550906));
#50324=CARTESIAN_POINT('Ctrl Pts',(1.05532560088906,38.0718434303104,14.906523095049));
#50325=CARTESIAN_POINT('Ctrl Pts',(1.03101271994426,38.0755593216332,14.923036887145));
#50326=CARTESIAN_POINT('Ctrl Pts',(1.00630993556873,38.0792812792025,14.9389786380786));
#50327=CARTESIAN_POINT('Ctrl Pts',(0.931813705546694,38.09050559315,14.9870542042356));
#50328=CARTESIAN_POINT('Ctrl Pts',(0.854050897258177,38.1016783441784,15.0302224781016));
#50329=CARTESIAN_POINT('Ctrl Pts',(0.773446603681667,38.1128295662079,15.0677543178446));
#50330=CARTESIAN_POINT('Ctrl Pts',(0.692845204371131,38.1239803878293,15.1052848099284));
#50331=CARTESIAN_POINT('Ctrl Pts',(0.609401976885697,38.135109688761,15.1371780828391));
#50332=CARTESIAN_POINT('Ctrl Pts',(0.523968011596957,38.1462410762626,15.1632326981605));
#50333=CARTESIAN_POINT('Ctrl Pts',(0.437199628779924,38.157546328088,15.1896942679673));
#50334=CARTESIAN_POINT('Ctrl Pts',(0.348377553615163,38.1688537548445,15.2101321372207));
#50335=CARTESIAN_POINT('Ctrl Pts',(0.25844726538386,38.1801811519831,15.2243277362019));
#50336=CARTESIAN_POINT('Ctrl Pts',(0.168516977152557,38.1915085491216,15.2385233351831));
#50337=CARTESIAN_POINT('Ctrl Pts',(0.0774787389347745,38.2028559191199,
15.2464753286676));
#50338=CARTESIAN_POINT('Ctrl Pts',(-0.0136685470148311,38.214234012426,
15.247977050252));
#50339=CARTESIAN_POINT('Ctrl Pts',(-0.0294357107357523,38.2162022581957,
15.2482368263917));
#50340=CARTESIAN_POINT('Ctrl Pts',(-0.0452102629264591,38.2181716841655,
15.2483052034339));
#50341=CARTESIAN_POINT('Ctrl Pts',(-0.0609870846454569,38.2201422176861,
15.2481816691172));
#50342=CARTESIAN_POINT('Ctrl Pts',(-0.167861317030268,38.2334908668084,
15.2473448316664));
#50343=CARTESIAN_POINT('Ctrl Pts',(-0.274836074129024,38.2468898222752,
15.2376990938252));
#50344=CARTESIAN_POINT('Ctrl Pts',(-0.380578198734069,38.2603198260231,
15.2193486574701));
#50345=CARTESIAN_POINT('Ctrl Pts',(-0.417366157078181,38.2649921590246,
15.2129644932522));
#50346=CARTESIAN_POINT('Ctrl Pts',(-0.454005326035501,38.2696683063962,
15.2055269746925));
#50347=CARTESIAN_POINT('Ctrl Pts',(-0.490440916802775,38.2743476382891,
15.1970410556936));
#50348=CARTESIAN_POINT('Ctrl Pts',(-0.595332394070263,38.2878185886577,
15.172611629382));
#50349=CARTESIAN_POINT('Ctrl Pts',(-0.698532919360637,38.3013154565255,
15.1394935750653));
#50350=CARTESIAN_POINT('Ctrl Pts',(-0.798523269889506,38.3148278959151,
15.0980935250948));
#50351=CARTESIAN_POINT('Ctrl Pts',(-0.832977639475209,38.319483971009,15.0838280223238));
#50352=CARTESIAN_POINT('Ctrl Pts',(-0.86705130550624,38.324141951439,15.0685791480927));
#50353=CARTESIAN_POINT('Ctrl Pts',(-0.900683525930329,38.3288015922403,
15.0523633011244));
#50354=CARTESIAN_POINT('Ctrl Pts',(-0.953802916976569,38.3361611206551,
15.0267516731856));
#50355=CARTESIAN_POINT('Ctrl Pts',(-1.00582088986153,38.3435247625456,14.9987280011649));
#50356=CARTESIAN_POINT('Ctrl Pts',(-1.05656606986707,38.3508919848372,14.9684465575659));
#50357=CARTESIAN_POINT('Ctrl Pts',(-1.1512670174672,38.3646407375684,14.9119351528727));
#50358=CARTESIAN_POINT('Ctrl Pts',(-1.24147956422147,38.3784414699224,14.8472740887571));
#50359=CARTESIAN_POINT('Ctrl Pts',(-1.32593793858643,38.3922798854461,14.7754679152784));
#50360=CARTESIAN_POINT('Ctrl Pts',(-1.41011964597831,38.4060729693782,14.7038969629582));
#50361=CARTESIAN_POINT('Ctrl Pts',(-1.4885842459314,38.4199034898599,14.6252288770287));
#50362=CARTESIAN_POINT('Ctrl Pts',(-1.56012293710475,38.4337598646462,14.5404830745007));
#50363=CARTESIAN_POINT('Ctrl Pts',(-1.63166162827809,38.4476162394325,14.4557372719726));
#50364=CARTESIAN_POINT('Ctrl Pts',(-1.69627398786503,38.4614984682388,14.3649148501332));
#50365=CARTESIAN_POINT('Ctrl Pts',(-1.75280334582966,38.475397552503,14.2690424737355));
#50366=CARTESIAN_POINT('Ctrl Pts',(-1.77188593180274,38.4800894591506,14.2366788854882));
#50367=CARTESIAN_POINT('Ctrl Pts',(-1.79004790890814,38.4847833082817,14.2037398383331));
#50368=CARTESIAN_POINT('Ctrl Pts',(-1.80727197431892,38.489478839319,14.1702942128208));
#50369=CARTESIAN_POINT('Ctrl Pts',(-1.83527483310092,38.4971128263836,14.1159183668308));
#50370=CARTESIAN_POINT('Ctrl Pts',(-1.86084066759219,38.5047597895004,14.0601450907728));
#50371=CARTESIAN_POINT('Ctrl Pts',(-1.88387488847079,38.5124193040841,14.0032558925948));
#50372=CARTESIAN_POINT('Ctrl Pts',(-1.92103627323572,38.5247764908133,13.9114758669711));
#50373=CARTESIAN_POINT('Ctrl Pts',(-1.95160763534726,38.5371663818236,13.8167906890215));
#50374=CARTESIAN_POINT('Ctrl Pts',(-1.97513569698453,38.5495856892822,13.7201224936645));
#50375=CARTESIAN_POINT('Ctrl Pts',(-2.00432522563287,38.5649934069449,13.6001934021287));
#50376=CARTESIAN_POINT('Ctrl Pts',(-2.02267215165502,38.5804464493681,13.4772121624051));
#50377=CARTESIAN_POINT('Ctrl Pts',(-2.02968898387652,38.5959385938295,13.3532907829735));
#50378=CARTESIAN_POINT('Ctrl Pts',(-2.03397888163678,38.6054100638217,13.2775286682056));
#50379=CARTESIAN_POINT('Ctrl Pts',(-2.03403471424584,38.6148961174031,13.201415701224));
#50380=CARTESIAN_POINT('Ctrl Pts',(-2.02975445317098,38.6243950291442,13.1254368311003));
#50381=CARTESIAN_POINT('Ctrl Pts',(-2.02280967740017,38.6398071292369,13.0021601881341));
#50382=CARTESIAN_POINT('Ctrl Pts',(-2.00444757115455,38.6552531620673,12.879237787665));
#50383=CARTESIAN_POINT('Ctrl Pts',(-1.97526544816996,38.6707239507206,12.7587251172616));
#50384=CARTESIAN_POINT('Ctrl Pts',(-1.97096571892869,38.6730034354035,12.7409686348717));
#50385=CARTESIAN_POINT('Ctrl Pts',(-1.96643117940809,38.6752834546776,12.723264432834));
#50386=CARTESIAN_POINT('Ctrl Pts',(-1.96166382899896,38.6775639762411,12.7056190442356));
#50387=CARTESIAN_POINT('Ctrl Pts',(-1.93445889617108,38.6905777953698,12.6049254575796));
#50388=CARTESIAN_POINT('Ctrl Pts',(-1.89963150194229,38.7036474933163,12.5058494960527));
#50389=CARTESIAN_POINT('Ctrl Pts',(-1.85744175271546,38.7167644025515,12.4096604907267));
#50390=CARTESIAN_POINT('Ctrl Pts',(-1.81471393547527,38.7300485986139,12.3122447365351));
#50391=CARTESIAN_POINT('Ctrl Pts',(-1.76443465003305,38.7433812228378,12.2177913129304));
#50392=CARTESIAN_POINT('Ctrl Pts',(-1.70692567539847,38.7567514050638,12.1276292830182));
#50393=CARTESIAN_POINT('Ctrl Pts',(-1.67917225935526,38.7632037584964,12.0841177381966));
#50394=CARTESIAN_POINT('Ctrl Pts',(-1.64973585385529,38.7696648309556,12.0416056773222));
#50395=CARTESIAN_POINT('Ctrl Pts',(-1.61865694793425,38.7761332434927,12.000241932981));
#50396=CARTESIAN_POINT('Ctrl Pts',(-1.55453211870822,38.7894794613539,11.9148964884287));
#50397=CARTESIAN_POINT('Ctrl Pts',(-1.48341208340305,38.8028570449867,11.8344414834723));
#50398=CARTESIAN_POINT('Ctrl Pts',(-1.40637875111882,38.8162525285523,11.7597475756211));
#50399=CARTESIAN_POINT('Ctrl Pts',(-1.3303324971104,38.8294763670595,11.6860107694763));
#50400=CARTESIAN_POINT('Ctrl Pts',(-1.24852441498115,38.8427176444261,11.6178893151297));
#50401=CARTESIAN_POINT('Ctrl Pts',(-1.16203176929779,38.8559616492614,11.5561868610373));
#50402=CARTESIAN_POINT('Ctrl Pts',(-1.13104879439214,38.8607058522653,11.5340841080037));
#50403=CARTESIAN_POINT('Ctrl Pts',(-1.09946498277994,38.8654503891011,11.5128046402907));
#50404=CARTESIAN_POINT('Ctrl Pts',(-1.06733066340167,38.8701945297612,11.4923839582497));
#50405=CARTESIAN_POINT('Ctrl Pts',(-0.972607256998674,38.8841789916224,
11.4321892318196));
#50406=CARTESIAN_POINT('Ctrl Pts',(-0.872839454613605,38.8982274412983,
11.3791452675653));
#50407=CARTESIAN_POINT('Ctrl Pts',(-0.769176366339235,38.9123291835519,
11.3342590985451));
#50408=CARTESIAN_POINT('Ctrl Pts',(-0.676647765071094,38.9249162529503,
11.2941941679623));
#50409=CARTESIAN_POINT('Ctrl Pts',(-0.581016842324058,38.9375457468101,
11.2606292273347));
#50410=CARTESIAN_POINT('Ctrl Pts',(-0.483133214779234,38.9502083200589,
11.2342672004245));
#50411=CARTESIAN_POINT('Ctrl Pts',(-0.374104051159969,38.964312719387,11.2049034567891));
#50412=CARTESIAN_POINT('Ctrl Pts',(-0.26228009898579,38.9784582001722,11.1844779374543));
#50413=CARTESIAN_POINT('Ctrl Pts',(-0.149211834206222,38.9926293412044,
11.1730342926814));
#50414=CARTESIAN_POINT('Ctrl Pts',(-0.0367979066216767,39.0067184724464,
11.161656873409));
#50415=CARTESIAN_POINT('Ctrl Pts',(0.0768447085266355,39.0208329632453,
11.1591580928637));
#50416=CARTESIAN_POINT('Ctrl Pts',(0.190172257764394,39.0349552099529,11.1655346303781));
#50417=CARTESIAN_POINT('Ctrl Pts',(0.27616395271878,39.0456710150605,11.1703730767442));
#50418=CARTESIAN_POINT('Ctrl Pts',(0.361973669224714,39.056391235503,11.1803206866011));
#50419=CARTESIAN_POINT('Ctrl Pts',(0.446926283662682,39.0671072570587,11.1953559052037));
#50420=CARTESIAN_POINT('Ctrl Pts',(0.557762231489612,39.0810882323814,11.2149720490461));
#50421=CARTESIAN_POINT('Ctrl Pts',(0.667456695819849,39.0951569273598,11.2430588959332));
#50422=CARTESIAN_POINT('Ctrl Pts',(0.774587654394998,39.1092997002696,11.279716904837));
#50423=CARTESIAN_POINT('Ctrl Pts',(0.821213735347596,39.1154549898643,11.2956713900152));
#50424=CARTESIAN_POINT('Ctrl Pts',(0.867353625063725,39.1216242526135,11.3132491260835));
#50425=CARTESIAN_POINT('Ctrl Pts',(0.912887566933807,39.1278060923235,11.3324566821536));
#50426=CARTESIAN_POINT('Ctrl Pts',(1.01816490605173,39.1420988947647,11.3768657605458));
#50427=CARTESIAN_POINT('Ctrl Pts',(1.12020465598396,39.1564592462259,11.429990595082));
#50428=CARTESIAN_POINT('Ctrl Pts',(1.21778291735022,39.1708665109701,11.4909839652763));
#50429=CARTESIAN_POINT('Ctrl Pts',(1.31590359196629,39.1853538621105,11.5523163824232));
#50430=CARTESIAN_POINT('Ctrl Pts',(1.4095117775228,39.1998886500518,11.621605329692));
#50431=CARTESIAN_POINT('Ctrl Pts',(1.49734755732802,39.2144451458915,11.6979392701371));
#50432=CARTESIAN_POINT('Ctrl Pts',(1.58390229667661,39.2287893425961,11.7731599186396));
#50433=CARTESIAN_POINT('Ctrl Pts',(1.66485035258449,39.2431546018885,11.8552214353057));
#50434=CARTESIAN_POINT('Ctrl Pts',(1.73899121814928,39.2575118529509,11.9432022807421));
#50435=CARTESIAN_POINT('Ctrl Pts',(1.75952788815997,39.2614887437665,11.9675725598888));
#50436=CARTESIAN_POINT('Ctrl Pts',(1.77954236860206,39.2654649943525,11.992396721077));
#50437=CARTESIAN_POINT('Ctrl Pts',(1.79900945011226,39.2694399279205,12.0176545279864));
#50438=CARTESIAN_POINT('Ctrl Pts',(1.8648746565806,39.2828887759161,12.1031121589189));
#50439=CARTESIAN_POINT('Ctrl Pts',(1.92466113418795,39.2963712277619,12.1936984375978));
#50440=CARTESIAN_POINT('Ctrl Pts',(1.97742211730071,39.3099037258777,12.2885951626925));
#50441=CARTESIAN_POINT('Ctrl Pts',(2.02834600704809,39.3229650337117,12.3801876630783));
#50442=CARTESIAN_POINT('Ctrl Pts',(2.07272547499223,39.3360729971241,12.4757945953722));
#50443=CARTESIAN_POINT('Ctrl Pts',(2.11032929023137,39.34924701252,12.5742859751103));
#50444=CARTESIAN_POINT('Ctrl Pts',(2.13229742930302,39.3569432688841,12.6318246135086));
#50445=CARTESIAN_POINT('Ctrl Pts',(2.15195409073792,39.3646621538228,12.6903478973526));
#50446=CARTESIAN_POINT('Ctrl Pts',(2.16926057692105,39.3724082463288,12.7496340491348));
#50447=CARTESIAN_POINT('Ctrl Pts',(2.20499938889948,39.3884043382394,12.8720630973567));
#50448=CARTESIAN_POINT('Ctrl Pts',(2.23050054750311,39.4044245201669,12.997856234636));
#50449=CARTESIAN_POINT('Ctrl Pts',(2.24524477699743,39.4204386971286,13.125211320992));
#50450=CARTESIAN_POINT('Ctrl Pts',(2.25984430316941,39.436295707206,13.2513165146955));
#50451=CARTESIAN_POINT('Ctrl Pts',(2.26389576834546,39.4521468097985,13.3789539579255));
#50452=CARTESIAN_POINT('Ctrl Pts',(2.25686901755235,39.4679566252646,13.5063310262745));
#50453=CARTESIAN_POINT('Ctrl Pts',(2.25557898741884,39.4708591244363,13.5297159820424));
#50454=CARTESIAN_POINT('Ctrl Pts',(2.25391552734149,39.4737602156173,13.553092027494));
#50455=CARTESIAN_POINT('Ctrl Pts',(2.25187531184562,39.4766596578138,13.5764478840497));
#50456=CARTESIAN_POINT('Ctrl Pts',(2.24737834603513,39.4830504986117,13.6279279794702));
#50457=CARTESIAN_POINT('Ctrl Pts',(2.24110742310709,39.4894581531109,13.67930762029));
#50458=CARTESIAN_POINT('Ctrl Pts',(2.23303044536404,39.4958822443291,13.7304716656013));
#50459=CARTESIAN_POINT('Ctrl Pts',(2.20765171897598,39.5160674247897,13.8912345583772));
#50460=CARTESIAN_POINT('Ctrl Pts',(2.16444241364464,39.5364153426137,14.0498730313516));
#50461=CARTESIAN_POINT('Ctrl Pts',(2.10488708145267,39.5569100664321,14.2029025809024));
#50462=CARTESIAN_POINT('Ctrl Pts',(2.04252350325459,39.578371189466,14.3631480186957));
#50463=CARTESIAN_POINT('Ctrl Pts',(1.96223410268545,39.5999933319345,14.5172425693329));
#50464=CARTESIAN_POINT('Ctrl Pts',(1.86573413249446,39.6217510677722,14.6611277667625));
#50465=CARTESIAN_POINT('Ctrl Pts',(1.76992981325946,39.6433519559994,14.8039757216422));
#50466=CARTESIAN_POINT('Ctrl Pts',(1.65814643351817,39.6650864667814,14.9367591694373));
#50467=CARTESIAN_POINT('Ctrl Pts',(1.53209748668832,39.6869228001303,15.0554700291448));
#50468=CARTESIAN_POINT('Ctrl Pts',(1.52660601812724,39.6878741253186,15.0606418054296));
#50469=CARTESIAN_POINT('Ctrl Pts',(1.52108748071761,39.6888256427,15.0657868687584));
#50470=CARTESIAN_POINT('Ctrl Pts',(1.51554219727787,39.689777349341,15.070905040698));
#50471=CARTESIAN_POINT('Ctrl Pts',(1.40993244337401,39.7079025732794,15.168380469115));
#50472=CARTESIAN_POINT('Ctrl Pts',(1.29452495950882,39.7260673948832,15.2560975042179));
#50473=CARTESIAN_POINT('Ctrl Pts',(1.17156908372708,39.7442254101507,15.3327459533929));
#50474=CARTESIAN_POINT('Ctrl Pts',(1.04861320794535,39.7623834254181,15.4093944025679));
#50475=CARTESIAN_POINT('Ctrl Pts',(0.918109393126689,39.7805346191256,15.474972521862));
#50476=CARTESIAN_POINT('Ctrl Pts',(0.78236694783971,39.7986269225969,15.5281863917256));
#50477=CARTESIAN_POINT('Ctrl Pts',(0.674184584539994,39.8130459065993,15.570596134603));
#50478=CARTESIAN_POINT('Ctrl Pts',(0.562639589759075,39.8274689786143,15.6052257702722));
#50479=CARTESIAN_POINT('Ctrl Pts',(0.448917494117073,39.8419532158612,15.631536517183));
#50480=CARTESIAN_POINT('Ctrl Pts',(0.344470930111066,39.8552560731831,15.655701276861));
#50481=CARTESIAN_POINT('Ctrl Pts',(0.23818767329683,39.8686106077482,15.6728499352464));
#50482=CARTESIAN_POINT('Ctrl Pts',(0.130950146145734,39.8820659530989,15.6825787805095));
#50483=CARTESIAN_POINT('Ctrl Pts',(0.0619357240280919,39.8907253553478,
15.6888399341516));
#50484=CARTESIAN_POINT('Ctrl Pts',(-0.00747466447897276,39.8994266059004,
15.6920281986405));
#50485=CARTESIAN_POINT('Ctrl Pts',(-0.0770187597906271,39.9081837908669,
15.6922092589488));
#50486=CARTESIAN_POINT('Ctrl Pts',(-0.15083418087625,39.917478832997,15.6924014397923));
#50487=CARTESIAN_POINT('Ctrl Pts',(-0.224814304867329,39.9267837732083,
15.689126374746));
#50488=CARTESIAN_POINT('Ctrl Pts',(-0.298585723235663,39.9360898120054,
15.6824440425789));
#50489=CARTESIAN_POINT('Ctrl Pts',(-0.372357141603997,39.9453958508025,
15.6757617104117));
#50490=CARTESIAN_POINT('Ctrl Pts',(-0.445920003627971,39.9547015994929,
15.6656731457466));
#50491=CARTESIAN_POINT('Ctrl Pts',(-0.518996000608588,39.963993101745,15.6522066196876));
#50492=CARTESIAN_POINT('Ctrl Pts',(-0.649050855860098,39.9805293794613,
15.6282399662074));
#50493=CARTESIAN_POINT('Ctrl Pts',(-0.777562113765256,39.9970209905262,
15.5935741587819));
#50494=CARTESIAN_POINT('Ctrl Pts',(-0.902740062950962,40.0134430802308,
15.5484535570547));
#50495=CARTESIAN_POINT('Ctrl Pts',(-0.918233577649619,40.0154756737497,
15.5428688936964));
#50496=CARTESIAN_POINT('Ctrl Pts',(-0.933675976443711,40.0175071990136,
15.5371240271856));
#50497=CARTESIAN_POINT('Ctrl Pts',(-0.949063819652945,40.0195376061761,
15.5312193878286));
#50498=CARTESIAN_POINT('Ctrl Pts',(-1.03061029609617,40.030297564384,15.4999282882454));
#50499=CARTESIAN_POINT('Ctrl Pts',(-1.11064181727098,40.0410300409155,15.4641445833943));
#50500=CARTESIAN_POINT('Ctrl Pts',(-1.1886437811041,40.0518269270513,15.4240795684269));
#50501=CARTESIAN_POINT('Ctrl Pts',(-1.24428110356763,40.0595281413031,15.3955019525862));
#50502=CARTESIAN_POINT('Ctrl Pts',(-1.29888698283431,40.0672622641483,15.3647461915998));
#50503=CARTESIAN_POINT('Ctrl Pts',(-1.35229042157928,40.0750646633413,15.3318856940637));
#50504=CARTESIAN_POINT('Ctrl Pts',(-1.36651191821623,40.0771424657542,15.3231348445645));
#50505=CARTESIAN_POINT('Ctrl Pts',(-1.38064702607825,40.0792256896704,15.3142366233478));
#50506=CARTESIAN_POINT('Ctrl Pts',(-1.39469212530709,40.0813134338249,15.3051904271304));
#50507=CARTESIAN_POINT('Ctrl Pts',(-1.46302294019609,40.091470518302,15.2611797762189));
#50508=CARTESIAN_POINT('Ctrl Pts',(-1.52922710773669,40.1017351285523,15.2136648644734));
#50509=CARTESIAN_POINT('Ctrl Pts',(-1.59298260229315,40.1119994019961,15.1628259031572));
#50510=CARTESIAN_POINT('Ctrl Pts',(-1.63432250007387,40.118654891345,15.1298612547186));
#50511=CARTESIAN_POINT('Ctrl Pts',(-1.67463186284525,40.1253101017758,15.0954994458754));
#50512=CARTESIAN_POINT('Ctrl Pts',(-1.71381313588905,40.131934140182,15.0597958761118));
#50513=CARTESIAN_POINT('Ctrl Pts',(-1.79641772214658,40.1458993819772,14.9845232170294));
#50514=CARTESIAN_POINT('Ctrl Pts',(-1.87416648810312,40.1598005498757,14.9032238652839));
#50515=CARTESIAN_POINT('Ctrl Pts',(-1.94629403927576,40.1736911961933,14.8167859073364));
#50516=CARTESIAN_POINT('Ctrl Pts',(-2.01881835699388,40.1876582535863,14.729872462707));
#50517=CARTESIAN_POINT('Ctrl Pts',(-2.08565956552004,40.201614679656,14.6377649500271));
#50518=CARTESIAN_POINT('Ctrl Pts',(-2.14609222190778,40.2156200980235,14.5413667041427));
#50519=CARTESIAN_POINT('Ctrl Pts',(-2.20645007732472,40.2296081810802,14.4450877759055));
#50520=CARTESIAN_POINT('Ctrl Pts',(-2.26041556080545,40.2436451498221,14.3445297159776));
#50521=CARTESIAN_POINT('Ctrl Pts',(-2.30731486398802,40.2577953963599,14.24057637183));
#50522=CARTESIAN_POINT('Ctrl Pts',(-2.33681844803083,40.2666970848632,14.1751810244055));
#50523=CARTESIAN_POINT('Ctrl Pts',(-2.36352658682643,40.2756437014626,14.1084416141264));
#50524=CARTESIAN_POINT('Ctrl Pts',(-2.38728043808747,40.2846522490296,14.040572526374));
#50525=CARTESIAN_POINT('Ctrl Pts',(-0.846350554922702,36.2086580169322,
10.9476201968673));
#50526=CARTESIAN_POINT('Ctrl Pts',(-0.320239388270522,36.2776098215264,
10.7790676939286));
#50527=CARTESIAN_POINT('Ctrl Pts',(0.832775930125362,36.4139226702905,10.808549500351));
#50528=CARTESIAN_POINT('Ctrl Pts',(2.13906229672172,36.6136666354338,11.8831979032289));
#50529=CARTESIAN_POINT('Ctrl Pts',(2.49776983260815,36.808758111583,13.495739293786));
#50530=CARTESIAN_POINT('Ctrl Pts',(1.80437349953285,36.9993052263523,14.952542053131));
#50531=CARTESIAN_POINT('Ctrl Pts',(0.394900147917386,37.185448210336,15.6574645158721));
#50532=CARTESIAN_POINT('Ctrl Pts',(-1.11565382654404,37.3673476166458,15.3516804870708));
#50533=CARTESIAN_POINT('Ctrl Pts',(-2.09311765211965,37.5452064656626,14.2088709500021));
#50534=CARTESIAN_POINT('Ctrl Pts',(-2.1720579761826,37.7385796988706,12.5707062008505));
#50535=CARTESIAN_POINT('Ctrl Pts',(-0.949636867934553,37.9462055979747,
11.2027877013928));
#50536=CARTESIAN_POINT('Ctrl Pts',(0.673815046857492,38.1301938802853,11.2772200756772));
#50537=CARTESIAN_POINT('Ctrl Pts',(1.57727284316267,38.2749046007684,12.0503331491926));
#50538=CARTESIAN_POINT('Ctrl Pts',(1.94325033553157,38.3822910046209,12.8523955445105));
#50539=CARTESIAN_POINT('Ctrl Pts',(1.92810669679268,38.4886294217223,13.7248605615257));
#50540=CARTESIAN_POINT('Ctrl Pts',(1.42241170095239,38.6291577761382,14.7650632826532));
#50541=CARTESIAN_POINT('Ctrl Pts',(0.0401515959749049,38.8027238580628,
15.4262990840038));
#50542=CARTESIAN_POINT('Ctrl Pts',(-1.46965088290585,38.9913613874058,14.7220128335763));
#50543=CARTESIAN_POINT('Ctrl Pts',(-1.97854444794942,39.1617067135922,13.370700241503));
#50544=CARTESIAN_POINT('Ctrl Pts',(-1.59936214624478,39.3145198762853,12.1352956525774));
#50545=CARTESIAN_POINT('Ctrl Pts',(-0.537697718828742,39.467221677783,11.3957752654928));
#50546=CARTESIAN_POINT('Ctrl Pts',(0.431453487286904,39.581964807185,11.4476593843084));
#50547=CARTESIAN_POINT('Ctrl Pts',(0.981899433556111,39.6586655307137,11.7263662420974));
#50548=CARTESIAN_POINT('Ctrl Pts',(1.31369659088836,39.7098688329335,11.9697816194113));
#50549=CARTESIAN_POINT('Ctrl Pts',(1.77927598222622,39.7996585507031,12.5319575286557));
#50550=CARTESIAN_POINT('Ctrl Pts',(1.99002909214103,39.9285999970237,13.6022652497978));
#50551=CARTESIAN_POINT('Ctrl Pts',(1.39274427027988,40.0847604456334,14.7825804722783));
#50552=CARTESIAN_POINT('Ctrl Pts',(0.182808632813018,40.2427406148847,15.3521158945863));
#50553=CARTESIAN_POINT('Ctrl Pts',(-1.13947383359755,40.4028817003577,15.0538629730217));
#50554=CARTESIAN_POINT('Ctrl Pts',(-2.01284312485354,40.5655300227019,13.9883677995854));
#50555=CARTESIAN_POINT('Ctrl Pts',(-2.04026673680089,40.703437009905,12.8220937324209));
#50556=CARTESIAN_POINT('Ctrl Pts',(-1.67504874026637,40.8013405748775,12.11478228846));
#50557=CARTESIAN_POINT('Ctrl Pts',(-1.37512744085228,40.8577000030924,11.7753778421044));
#50558=CARTESIAN_POINT('Ctrl Pts',(-0.84520156220626,40.942653269374,11.3441539863298));
#50559=CARTESIAN_POINT('Ctrl Pts',(0.20619225565922,41.07169276057,11.0515151341635));
#50560=CARTESIAN_POINT('Ctrl Pts',(1.58303660030943,41.2474326928145,11.6176574340441));
#50561=CARTESIAN_POINT('Ctrl Pts',(2.33325522018996,41.4270957461375,12.9390680613749));
#50562=CARTESIAN_POINT('Ctrl Pts',(2.08870142664571,41.6313181674013,14.6528956012928));
#50563=CARTESIAN_POINT('Ctrl Pts',(0.478042449382701,41.8621181773002,15.897365670719));
#50564=CARTESIAN_POINT('Ctrl Pts',(-1.761592798532,42.1219415711064,15.3873242298046));
#50565=CARTESIAN_POINT('Ctrl Pts',(-2.59367583188875,42.3340558257298,13.7054240007776));
#50566=CARTESIAN_POINT('Ctrl Pts',(-2.43193369746059,42.4594565353203,12.6998858182967));
#50567=CARTESIAN_POINT('Ctrl Pts',(-2.34562647967194,42.4937495273014,12.438593281029));
#50568=CARTESIAN_POINT('Ctrl Pts',(-1.50589870835376,49.9431019076281,10.6371826091256));
#50569=CARTESIAN_POINT('Ctrl Pts',(-0.997967678553802,50.0151271970462,
10.363255806184));
#50570=CARTESIAN_POINT('Ctrl Pts',(0.158195592874908,50.1568524066829,10.118721243365));
#50571=CARTESIAN_POINT('Ctrl Pts',(1.79381557388335,50.3661150852637,10.7207619811602));
#50572=CARTESIAN_POINT('Ctrl Pts',(2.84419434848047,50.5712195350034,12.067783810989));
#50573=CARTESIAN_POINT('Ctrl Pts',(3.02341717505406,50.7735159459258,13.7431013283951));
#50574=CARTESIAN_POINT('Ctrl Pts',(2.30286206288198,50.9728836506257,15.2388199884596));
#50575=CARTESIAN_POINT('Ctrl Pts',(0.92205760400918,51.1692158544984,16.1161415454293));
#50576=CARTESIAN_POINT('Ctrl Pts',(-0.685453262226371,51.3624197803939,
16.1320659429518));
#50577=CARTESIAN_POINT('Ctrl Pts',(-2.19238056120144,51.5735293389412,15.2219934660806));
#50578=CARTESIAN_POINT('Ctrl Pts',(-2.90735272931905,51.8010880510178,13.4061487489255));
#50579=CARTESIAN_POINT('Ctrl Pts',(-2.16425376166143,52.0434177919142,11.4615023835655));
#50580=CARTESIAN_POINT('Ctrl Pts',(-0.502081140238918,52.2600779708778,
10.630409517392));
#50581=CARTESIAN_POINT('Ctrl Pts',(1.07593746233167,52.4526832569537,10.9256670839091));
#50582=CARTESIAN_POINT('Ctrl Pts',(2.12276587212965,52.6226828382186,11.8771254661021));
#50583=CARTESIAN_POINT('Ctrl Pts',(2.50200021911292,52.7893692149562,13.2132811311121));
#50584=CARTESIAN_POINT('Ctrl Pts',(2.12706423374028,52.9527900207895,14.5212359218611));
#50585=CARTESIAN_POINT('Ctrl Pts',(1.13781104018586,53.1130091141584,15.4174536119083));
#50586=CARTESIAN_POINT('Ctrl Pts',(0.0654657851665619,53.2439207055765,
15.6121783318573));
#50587=CARTESIAN_POINT('Ctrl Pts',(-0.746623315045519,53.3471366675035,
15.4169819595003));
#50588=CARTESIAN_POINT('Ctrl Pts',(-1.24224768410671,53.4174127398507,15.1386872585679));
#50589=CARTESIAN_POINT('Ctrl Pts',(-1.53955280475257,53.4680994158948,14.8585927685747));
#50590=CARTESIAN_POINT('Ctrl Pts',(-1.72953687809877,53.5059325452741,14.6222034008512));
#50591=CARTESIAN_POINT('Ctrl Pts',(-1.83900671316259,53.5310650918408,14.4524985484517));
#50592=CARTESIAN_POINT('Ctrl Pts',(-1.92953388679311,53.5561097283772,14.2734012151605));
#50593=CARTESIAN_POINT('Ctrl Pts',(-2.16406279700829,53.6310687712466,13.719290031839));
#50594=CARTESIAN_POINT('Ctrl Pts',(-2.17177819037875,53.7358927560662,12.832395135736));
#50595=CARTESIAN_POINT('Ctrl Pts',(-1.45710175821801,53.9054769110698,11.6357747936092));
#50596=CARTESIAN_POINT('Ctrl Pts',(-0.413266964323039,54.0361204336834,
11.1919935846092));
#50597=CARTESIAN_POINT('Ctrl Pts',(0.711216260265478,54.1763643967519,11.3652778255788));
#50598=CARTESIAN_POINT('Ctrl Pts',(1.52066824573736,54.2918677043501,11.880340058231));
#50599=CARTESIAN_POINT('Ctrl Pts',(2.01443006791509,54.428455762762,12.9067219771098));
#50600=CARTESIAN_POINT('Ctrl Pts',(1.89256617764797,54.5632269584251,14.0220272624448));
#50601=CARTESIAN_POINT('Ctrl Pts',(1.38063078199914,54.6630909695851,14.6774342504526));
#50602=CARTESIAN_POINT('Ctrl Pts',(0.930736007320949,54.7292209179053,14.9598721955184));
#50603=CARTESIAN_POINT('Ctrl Pts',(0.608667091714335,54.773198599464,15.1048739140154));
#50604=CARTESIAN_POINT('Ctrl Pts',(0.175602575225595,54.8279616001322,15.1990651595965));
#50605=CARTESIAN_POINT('Ctrl Pts',(-0.352406871985372,54.893380841766,15.1649979748017));
#50606=CARTESIAN_POINT('Ctrl Pts',(-1.01514487004226,54.9802401150033,14.930429326385));
#50607=CARTESIAN_POINT('Ctrl Pts',(-1.66780664136042,55.088200471646,14.3122806208394));
#50608=CARTESIAN_POINT('Ctrl Pts',(-1.94015073865359,55.2169934028641,13.2743783173256));
#50609=CARTESIAN_POINT('Ctrl Pts',(-1.62596701268505,55.3452548126108,12.253428093674));
#50610=CARTESIAN_POINT('Ctrl Pts',(-0.822759016554036,55.4732131481038,
11.552987892603));
#50611=CARTESIAN_POINT('Ctrl Pts',(0.22864918135393,55.6011019347585,11.3811964479907));
#50612=CARTESIAN_POINT('Ctrl Pts',(0.994467824367534,55.7006917801432,11.6991450082289));
#50613=CARTESIAN_POINT('Ctrl Pts',(1.36698632717851,55.7648487863085,12.0567353290565));
#50614=CARTESIAN_POINT('Ctrl Pts',(1.50893253971056,55.7933864622217,12.2363773760104));
#50615=CARTESIAN_POINT('Ctrl Pts',(1.69571438886681,55.8362209424235,12.5244913797639));
#50616=CARTESIAN_POINT('Ctrl Pts',(1.95466728844487,55.929201785116,13.2382690435808));
#50617=CARTESIAN_POINT('Ctrl Pts',(1.74920409027378,56.0442438038412,14.2008603846282));
#50618=CARTESIAN_POINT('Ctrl Pts',(1.17286032909157,56.1456895858431,14.7965620237573));
#50619=CARTESIAN_POINT('Ctrl Pts',(0.768526008089416,56.2039055636691,15.0317400892323));
#50620=CARTESIAN_POINT('Ctrl Pts',(0.104606995860322,56.2915081081481,15.2699416184091));
#50621=CARTESIAN_POINT('Ctrl Pts',(-1.02326211770975,56.4239720744945,15.1364144040356));
#50622=CARTESIAN_POINT('Ctrl Pts',(-2.02993586215422,56.6033780628028,13.9721301674421));
#50623=CARTESIAN_POINT('Ctrl Pts',(-1.99001292699949,56.7860310929108,12.4035952810077));
#50624=CARTESIAN_POINT('Ctrl Pts',(-1.0032412314103,56.9516808788094,11.3821713282861));
#50625=CARTESIAN_POINT('Ctrl Pts',(0.197329230236401,57.0992917294341,11.1593006877948));
#50626=CARTESIAN_POINT('Ctrl Pts',(1.20762964212908,57.2277551469465,11.4805246362353));
#50627=CARTESIAN_POINT('Ctrl Pts',(1.99047227458886,57.3637094919575,12.2871144386262));
#50628=CARTESIAN_POINT('Ctrl Pts',(2.28235856496914,57.5075737399963,13.4485263777013));
#50629=CARTESIAN_POINT('Ctrl Pts',(1.89658779363131,57.6598213116464,14.6569347041676));
#50630=CARTESIAN_POINT('Ctrl Pts',(0.914041736627156,57.8150355469431,15.4962660713587));
#50631=CARTESIAN_POINT('Ctrl Pts',(-0.38890798366212,57.9733172811768,15.6958293398159));
#50632=CARTESIAN_POINT('Ctrl Pts',(-1.62534529857286,58.1347548824581,15.1683265160832));
#50633=CARTESIAN_POINT('Ctrl Pts',(-2.41372763907556,58.2994204314994,14.0465052931711));
#50634=CARTESIAN_POINT('Ctrl Pts',(-2.49386038142991,58.4673719419849,12.6500189571622));
#50635=CARTESIAN_POINT('Ctrl Pts',(-2.04000962209625,58.5815575858371,11.8147420052546));
#50636=CARTESIAN_POINT('Ctrl Pts',(-1.71585603698212,58.6392095497043,11.4856667176634));
#50637=CARTESIAN_POINT('Ctrl Pts',(-1.44314689269042,50.0096600245596,10.8164178498533));
#50638=CARTESIAN_POINT('Ctrl Pts',(-0.967833206190739,50.0773357805971,
10.5555388260198));
#50639=CARTESIAN_POINT('Ctrl Pts',(0.115434306511918,50.2103396991322,10.3183871031536));
#50640=CARTESIAN_POINT('Ctrl Pts',(1.65093114637839,50.4062957717865,10.8710554596649));
#50641=CARTESIAN_POINT('Ctrl Pts',(2.64169322568085,50.5979836964062,12.1226297867223));
#50642=CARTESIAN_POINT('Ctrl Pts',(2.82051984598436,50.7867229952345,13.6842352127829));
#50643=CARTESIAN_POINT('Ctrl Pts',(2.15988775952974,50.9724571312247,15.082582164639));
#50644=CARTESIAN_POINT('Ctrl Pts',(0.881537136075658,51.1551438493973,15.9087514070269));
#50645=CARTESIAN_POINT('Ctrl Pts',(-0.612562908279529,51.33475498818,15.9353575960212));
#50646=CARTESIAN_POINT('Ctrl Pts',(-2.0192227121573,51.530891439638,15.1012354462255));
#50647=CARTESIAN_POINT('Ctrl Pts',(-2.69711124774285,51.7422379283989,13.4205467389996));
#50648=CARTESIAN_POINT('Ctrl Pts',(-2.02247298214849,51.9673511700767,11.6084678588967));
#50649=CARTESIAN_POINT('Ctrl Pts',(-0.484267511851704,52.1687924756556,
10.8220839616332));
#50650=CARTESIAN_POINT('Ctrl Pts',(0.987164463079186,52.3481129585181,11.0834955949316));
#50651=CARTESIAN_POINT('Ctrl Pts',(1.97144859362409,52.5066367477731,11.9614279805005));
#50652=CARTESIAN_POINT('Ctrl Pts',(2.33773697406492,52.6623825463245,13.2062234102142));
#50653=CARTESIAN_POINT('Ctrl Pts',(1.99873683538971,52.8154495056158,14.4345354278471));
#50654=CARTESIAN_POINT('Ctrl Pts',(1.07824398048702,52.9659507012417,15.2856626082588));
#50655=CARTESIAN_POINT('Ctrl Pts',(0.0697049573621546,53.0893317916579,
15.4797027775451));
#50656=CARTESIAN_POINT('Ctrl Pts',(-0.699607585085375,53.1868862908566,
15.3031285416865));
#50657=CARTESIAN_POINT('Ctrl Pts',(-1.17161314368012,53.2534397586931,15.044498237106));
#50658=CARTESIAN_POINT('Ctrl Pts',(-1.45641635268664,53.3015314616841,14.7817377808518));
#50659=CARTESIAN_POINT('Ctrl Pts',(-1.6391690146498,53.337466301464,14.5591301402832));
#50660=CARTESIAN_POINT('Ctrl Pts',(-1.74490480360317,53.3613577519319,14.3989309299869));
#50661=CARTESIAN_POINT('Ctrl Pts',(-1.83280603061363,53.3851861785151,14.2294653625524));
#50662=CARTESIAN_POINT('Ctrl Pts',(-2.06159148754384,53.4565465193291,13.7044345680607));
#50663=CARTESIAN_POINT('Ctrl Pts',(-2.07877019877502,53.5566611884873,12.8575983361216));
#50664=CARTESIAN_POINT('Ctrl Pts',(-1.40603614418218,53.7194678026363,11.7012894016199));
#50665=CARTESIAN_POINT('Ctrl Pts',(-0.403405186271102,53.8456725193569,
11.2598606725744));
#50666=CARTESIAN_POINT('Ctrl Pts',(0.691219352687192,53.9819685221532,11.4153747691577));
#50667=CARTESIAN_POINT('Ctrl Pts',(1.48757896395445,54.0947462754909,11.9083621144659));
#50668=CARTESIAN_POINT('Ctrl Pts',(1.98557800160514,54.2289819014901,12.9105081365746));
#50669=CARTESIAN_POINT('Ctrl Pts',(1.87938366711896,54.3623306653876,14.0153323317459));
#50670=CARTESIAN_POINT('Ctrl Pts',(1.37812277860126,54.4618301452917,14.6748860962729));
#50671=CARTESIAN_POINT('Ctrl Pts',(0.93151130558792,54.5280104671103,14.9630837165789));
#50672=CARTESIAN_POINT('Ctrl Pts',(0.610531160974068,54.5720998812823,15.1124430650131));
#50673=CARTESIAN_POINT('Ctrl Pts',(0.176535664765444,54.6271491611219,15.2126589477959));
#50674=CARTESIAN_POINT('Ctrl Pts',(-0.356437580665123,54.6931459505594,
15.185131838619));
#50675=CARTESIAN_POINT('Ctrl Pts',(-1.03027121446636,54.7810865292972,14.9564103073955));
#50676=CARTESIAN_POINT('Ctrl Pts',(-1.70305637580998,54.890979739731,14.3365617953708));
#50677=CARTESIAN_POINT('Ctrl Pts',(-1.99697946426401,55.0230112459747,13.276794154045));
#50678=CARTESIAN_POINT('Ctrl Pts',(-1.68750568280781,55.1554149288954,12.218662248392));
#50679=CARTESIAN_POINT('Ctrl Pts',(-0.863245869663355,55.2883998181656,
11.4792032203492));
#50680=CARTESIAN_POINT('Ctrl Pts',(0.23369382995798,55.4221752650644,11.2840552404368));
#50681=CARTESIAN_POINT('Ctrl Pts',(1.04417672785527,55.5269917049279,11.6072605812333));
#50682=CARTESIAN_POINT('Ctrl Pts',(1.44269341168101,55.5947748560472,11.9797147371851));
#50683=CARTESIAN_POINT('Ctrl Pts',(1.59535621613771,55.6249683503327,12.1677271002977));
#50684=CARTESIAN_POINT('Ctrl Pts',(1.79714499201008,55.6703301088737,12.4701299601362));
#50685=CARTESIAN_POINT('Ctrl Pts',(2.08224613391108,55.7690189750693,13.2236988047189));
#50686=CARTESIAN_POINT('Ctrl Pts',(1.87781477739677,55.8917577693071,14.2535363827309));
#50687=CARTESIAN_POINT('Ctrl Pts',(1.26887003484619,56.0004790852983,14.9001774851111));
#50688=CARTESIAN_POINT('Ctrl Pts',(0.838066930964846,56.063002212917,15.1583893894994));
#50689=CARTESIAN_POINT('Ctrl Pts',(0.127712822964686,56.1572085860953,15.4238835554972));
#50690=CARTESIAN_POINT('Ctrl Pts',(-1.0907223837963,56.3001117619415,15.2967205489644));
#50691=CARTESIAN_POINT('Ctrl Pts',(-2.19800052179846,56.4944516616297,14.0505820561347));
#50692=CARTESIAN_POINT('Ctrl Pts',(-2.17705412607774,56.6929311041823,12.345920491215));
#50693=CARTESIAN_POINT('Ctrl Pts',(-1.11681994234011,56.8733219428292,11.2201611370152));
#50694=CARTESIAN_POINT('Ctrl Pts',(0.188678422475607,57.0342316102921,10.9612004285832));
#50695=CARTESIAN_POINT('Ctrl Pts',(1.29443431864757,57.1743272227455,11.2981696268465));
#50696=CARTESIAN_POINT('Ctrl Pts',(2.15840176208839,57.3225935604102,12.1675464585855));
#50697=CARTESIAN_POINT('Ctrl Pts',(2.49115674000038,57.4794296539054,13.4297720046328));
#50698=CARTESIAN_POINT('Ctrl Pts',(2.08583932942016,57.6452671332937,14.7505474672967));
#50699=CARTESIAN_POINT('Ctrl Pts',(1.0271187815923,57.8141257639239,15.675240097315));
#50700=CARTESIAN_POINT('Ctrl Pts',(-0.385530753414024,57.9860425989135,
15.9070961282611));
#50701=CARTESIAN_POINT('Ctrl Pts',(-1.73158520520778,58.1610409781782,15.3493347285684));
#50702=CARTESIAN_POINT('Ctrl Pts',(-2.59642604963151,58.3391292245915,14.1448963194587));
#50703=CARTESIAN_POINT('Ctrl Pts',(-2.6977480214632,58.5203013328294,12.6395458443079));
#50704=CARTESIAN_POINT('Ctrl Pts',(-2.21829017326044,58.6431246926601,11.7364920572358));
#50705=CARTESIAN_POINT('Ctrl Pts',(-1.87373118021481,58.7050409812207,11.3796721415008));
#50706=CARTESIAN_POINT('Ctrl Pts',(-1.38039507702709,50.076218141491,10.9956530905807));
#50707=CARTESIAN_POINT('Ctrl Pts',(-0.937698733827671,50.139544364148,10.7478218458557));
#50708=CARTESIAN_POINT('Ctrl Pts',(0.0726730201489353,50.2638269915814,
10.5180529629421));
#50709=CARTESIAN_POINT('Ctrl Pts',(1.50804671887345,50.4464764583093,11.0213489381696));
#50710=CARTESIAN_POINT('Ctrl Pts',(2.43919210288125,50.6247478578092,12.1774757624556));
#50711=CARTESIAN_POINT('Ctrl Pts',(2.61762251691468,50.7999300445433,13.6253690971706));
#50712=CARTESIAN_POINT('Ctrl Pts',(2.01691345617751,50.9720306118236,14.9263443408183));
#50713=CARTESIAN_POINT('Ctrl Pts',(0.84101666814214,51.141071844296,15.7013612686244));
#50714=CARTESIAN_POINT('Ctrl Pts',(-0.539672554332687,51.3070901959662,
15.7386492490906));
#50715=CARTESIAN_POINT('Ctrl Pts',(-1.84606486311318,51.488253540335,14.9804774263704));
#50716=CARTESIAN_POINT('Ctrl Pts',(-2.48686976616666,51.6833878057799,13.4349447290737));
#50717=CARTESIAN_POINT('Ctrl Pts',(-1.88069220263553,51.8912845482392,11.7554333342278));
#50718=CARTESIAN_POINT('Ctrl Pts',(-0.466453883464498,52.0775069804336,
11.0137584058744));
#50719=CARTESIAN_POINT('Ctrl Pts',(0.898391463826697,52.2435426600827,11.2413241059542));
#50720=CARTESIAN_POINT('Ctrl Pts',(1.82013131511852,52.3905906573276,12.0457304948989));
#50721=CARTESIAN_POINT('Ctrl Pts',(2.17347372901692,52.535395877693,13.1991656893163));
#50722=CARTESIAN_POINT('Ctrl Pts',(1.87040943703913,52.6781089904421,14.3478349338331));
#50723=CARTESIAN_POINT('Ctrl Pts',(1.01867692078817,52.818892288325,15.1538716046093));
#50724=CARTESIAN_POINT('Ctrl Pts',(0.0739441295577446,52.9347428777394,
15.3472272232332));
#50725=CARTESIAN_POINT('Ctrl Pts',(-0.652591855125238,53.0266359142099,
15.1892751238726));
#50726=CARTESIAN_POINT('Ctrl Pts',(-1.10097860325353,53.0894667775354,14.9503092156441));
#50727=CARTESIAN_POINT('Ctrl Pts',(-1.37327990062071,53.1349635074734,14.7048827931288));
#50728=CARTESIAN_POINT('Ctrl Pts',(-1.54880115120083,53.169000057654,14.4960568797151));
#50729=CARTESIAN_POINT('Ctrl Pts',(-1.65080289404375,53.1916504120229,14.3453633115221));
#50730=CARTESIAN_POINT('Ctrl Pts',(-1.73607817443418,53.2142626286529,14.1855295099443));
#50731=CARTESIAN_POINT('Ctrl Pts',(-1.95912017807941,53.2820242674115,13.6895791042823));
#50732=CARTESIAN_POINT('Ctrl Pts',(-1.9857622071713,53.3774296209084,12.8828015365073));
#50733=CARTESIAN_POINT('Ctrl Pts',(-1.35497053014638,53.5334586942027,11.7668040096305));
#50734=CARTESIAN_POINT('Ctrl Pts',(-0.393543408219166,53.6552246050305,
11.3277277605396));
#50735=CARTESIAN_POINT('Ctrl Pts',(0.671222445108904,53.7875726475542,11.4654717127364));
#50736=CARTESIAN_POINT('Ctrl Pts',(1.45448968217153,53.8976248466317,11.9363841707008));
#50737=CARTESIAN_POINT('Ctrl Pts',(1.95672593529519,54.029508040218,12.9142942960394));
#50738=CARTESIAN_POINT('Ctrl Pts',(1.86620115658996,54.1614343723501,14.0086374010468));
#50739=CARTESIAN_POINT('Ctrl Pts',(1.37561477520337,54.2605693209982,14.6723379420933));
#50740=CARTESIAN_POINT('Ctrl Pts',(0.932286603854889,54.3268000163154,14.9662952376396));
#50741=CARTESIAN_POINT('Ctrl Pts',(0.612395230233797,54.3710011631004,15.1200122160106));
#50742=CARTESIAN_POINT('Ctrl Pts',(0.177468754305291,54.4263367221115,15.2262527359952));
#50743=CARTESIAN_POINT('Ctrl Pts',(-0.360468289344878,54.492911059353,15.2052657024364));
#50744=CARTESIAN_POINT('Ctrl Pts',(-1.04539755889047,54.5819329435911,14.9823912884061));
#50745=CARTESIAN_POINT('Ctrl Pts',(-1.73830611025955,54.6937590078159,14.360842969902));
#50746=CARTESIAN_POINT('Ctrl Pts',(-2.05380818987441,54.829029089085,13.2792099907643));
#50747=CARTESIAN_POINT('Ctrl Pts',(-1.74904435293057,54.96557504518,12.1838964031099));
#50748=CARTESIAN_POINT('Ctrl Pts',(-0.903732722772673,55.1035864882273,
11.4054185480954));
#50749=CARTESIAN_POINT('Ctrl Pts',(0.238738478562035,55.2432485953703,11.1869140328831));
#50750=CARTESIAN_POINT('Ctrl Pts',(1.09388563134303,55.3532916297124,11.5153761542378));
#50751=CARTESIAN_POINT('Ctrl Pts',(1.51840049618351,55.4247009257859,11.9026941453137));
#50752=CARTESIAN_POINT('Ctrl Pts',(1.68177989256486,55.4565502384435,12.0990768245851));
#50753=CARTESIAN_POINT('Ctrl Pts',(1.89857559515335,55.504439275324,12.4157685405086));
#50754=CARTESIAN_POINT('Ctrl Pts',(2.20982497937729,55.6088361650228,13.2091285658572));
#50755=CARTESIAN_POINT('Ctrl Pts',(2.00642546451976,55.7392717347732,14.3062123808336));
#50756=CARTESIAN_POINT('Ctrl Pts',(1.36487974060081,55.8552685847536,15.0037929464649));
#50757=CARTESIAN_POINT('Ctrl Pts',(0.907607853840278,55.9220988621651,15.2850386897666));
#50758=CARTESIAN_POINT('Ctrl Pts',(0.150818650069051,56.0229090640423,15.5778254925855));
#50759=CARTESIAN_POINT('Ctrl Pts',(-1.15818264988283,56.1762514493885,15.4570266938932));
#50760=CARTESIAN_POINT('Ctrl Pts',(-2.36606518144271,56.3855252604566,14.1290339448272));
#50761=CARTESIAN_POINT('Ctrl Pts',(-2.36409532515597,56.5998311154537,12.2882457014221));
#50762=CARTESIAN_POINT('Ctrl Pts',(-1.23039865326991,56.7949630068492,11.0581509457444));
#50763=CARTESIAN_POINT('Ctrl Pts',(0.180027614714824,56.9691714911501,10.7631001693718));
#50764=CARTESIAN_POINT('Ctrl Pts',(1.38123899516607,57.1208992985444,11.1158146174577));
#50765=CARTESIAN_POINT('Ctrl Pts',(2.32633124958793,57.2814776288627,12.047978478545));
#50766=CARTESIAN_POINT('Ctrl Pts',(2.69995491503163,57.4512855678146,13.4110176315643));
#50767=CARTESIAN_POINT('Ctrl Pts',(2.27509086520902,57.630712954941,14.8441602304258));
#50768=CARTESIAN_POINT('Ctrl Pts',(1.14019582655745,57.8132159809048,15.8542141232712));
#50769=CARTESIAN_POINT('Ctrl Pts',(-0.382153523165924,57.9987679166501,
16.1183629167064));
#50770=CARTESIAN_POINT('Ctrl Pts',(-1.83782511184269,58.1873270738983,15.5303429410537));
#50771=CARTESIAN_POINT('Ctrl Pts',(-2.77912446018748,58.3788380176838,14.2432873457464));
#50772=CARTESIAN_POINT('Ctrl Pts',(-2.9016356614965,58.573230723674,12.6290727314537));
#50773=CARTESIAN_POINT('Ctrl Pts',(-2.39657072442463,58.704691799483,11.6582421092171));
#50774=CARTESIAN_POINT('Ctrl Pts',(-2.0316063234475,58.770872412737,11.2736775653382));
#50775=CARTESIAN_POINT('Ctrl Pts',(-1.31764326136376,50.1427762584224,11.1748883313082));
#50776=CARTESIAN_POINT('Ctrl Pts',(-0.907564261464606,50.2017529476989,
10.9401048656914));
#50777=CARTESIAN_POINT('Ctrl Pts',(0.0299117337859448,50.3173142840308,
10.7177188227307));
#50778=CARTESIAN_POINT('Ctrl Pts',(1.36516229136849,50.4866571448322,11.1716424166742));
#50779=CARTESIAN_POINT('Ctrl Pts',(2.23669098008163,50.6515120192122,12.2323217381889));
#50780=CARTESIAN_POINT('Ctrl Pts',(2.41472518784499,50.8131370938521,13.5665029815585));
#50781=CARTESIAN_POINT('Ctrl Pts',(1.87393915282527,50.9716040924225,14.7701065169977));
#50782=CARTESIAN_POINT('Ctrl Pts',(0.800496200208616,51.1269998391949,15.4939711302219));
#50783=CARTESIAN_POINT('Ctrl Pts',(-0.466782200385848,51.2794254037523,
15.5419409021598));
#50784=CARTESIAN_POINT('Ctrl Pts',(-1.67290701406904,51.4456156410318,14.8597194065153));
#50785=CARTESIAN_POINT('Ctrl Pts',(-2.27662828459044,51.624537683161,13.4493427191478));
#50786=CARTESIAN_POINT('Ctrl Pts',(-1.73891142312258,51.8152179264018,11.902398809559));
#50787=CARTESIAN_POINT('Ctrl Pts',(-0.448640255077288,51.9862214852115,
11.2054328501155));
#50788=CARTESIAN_POINT('Ctrl Pts',(0.809618464574202,52.138972361647,11.3991526169767));
#50789=CARTESIAN_POINT('Ctrl Pts',(1.66881403661296,52.2745445668821,12.1300330092972));
#50790=CARTESIAN_POINT('Ctrl Pts',(2.00921048396892,52.4084092090614,13.1921079684185));
#50791=CARTESIAN_POINT('Ctrl Pts',(1.74208203868856,52.5407684752683,14.2611344398192));
#50792=CARTESIAN_POINT('Ctrl Pts',(0.95910986108932,52.6718338754084,15.0220806009597));
#50793=CARTESIAN_POINT('Ctrl Pts',(0.0781833017533357,52.7801539638208,
15.2147516689212));
#50794=CARTESIAN_POINT('Ctrl Pts',(-0.605576125165097,52.866385537563,15.0754217060589));
#50795=CARTESIAN_POINT('Ctrl Pts',(-1.03034406282696,52.9254937963779,14.8561201941823));
#50796=CARTESIAN_POINT('Ctrl Pts',(-1.29014344855479,52.9683955532627,14.6280278054059));
#50797=CARTESIAN_POINT('Ctrl Pts',(-1.45843328775186,53.0005338138439,14.4329836191468));
#50798=CARTESIAN_POINT('Ctrl Pts',(-1.55670098448433,53.021943072114,14.2917956930573));
#50799=CARTESIAN_POINT('Ctrl Pts',(-1.63935031825471,53.0433390787907,14.1415936573363));
#50800=CARTESIAN_POINT('Ctrl Pts',(-1.85664886861498,53.1075020154939,13.674723640504));
#50801=CARTESIAN_POINT('Ctrl Pts',(-1.89275421556756,53.1981980533294,12.9080047368929));
#50802=CARTESIAN_POINT('Ctrl Pts',(-1.30390491611055,53.3474495857692,11.8323186176413));
#50803=CARTESIAN_POINT('Ctrl Pts',(-0.383681630167233,53.4647766907041,
11.3955948485047));
#50804=CARTESIAN_POINT('Ctrl Pts',(0.651225537530613,53.5931767729554,11.5155686563152));
#50805=CARTESIAN_POINT('Ctrl Pts',(1.42140040038861,53.7005034177724,11.9644062269358));
#50806=CARTESIAN_POINT('Ctrl Pts',(1.92787386898523,53.830034178946,12.9180804555043));
#50807=CARTESIAN_POINT('Ctrl Pts',(1.85301864606095,53.9605380793125,14.0019424703478));
#50808=CARTESIAN_POINT('Ctrl Pts',(1.3731067718055,54.059308496705,14.6697897879136));
#50809=CARTESIAN_POINT('Ctrl Pts',(0.933061902121851,54.1255895655204,14.9695067587001));
#50810=CARTESIAN_POINT('Ctrl Pts',(0.614259299493522,54.1699024449187,15.1275813670082));
#50811=CARTESIAN_POINT('Ctrl Pts',(0.178401843845132,54.2255242831011,15.2398465241946));
#50812=CARTESIAN_POINT('Ctrl Pts',(-0.364498998024635,54.2926761681464,
15.2253995662538));
#50813=CARTESIAN_POINT('Ctrl Pts',(-1.06052390331458,54.3827793578848,15.0083722694167));
#50814=CARTESIAN_POINT('Ctrl Pts',(-1.77355584470913,54.4965382759009,14.3851241444334));
#50815=CARTESIAN_POINT('Ctrl Pts',(-2.11063691548484,54.6350469321954,13.2816258274837));
#50816=CARTESIAN_POINT('Ctrl Pts',(-1.81058302305334,54.7757351614645,12.1491305578278));
#50817=CARTESIAN_POINT('Ctrl Pts',(-0.944219575881998,54.918773158289,11.3316338758417));
#50818=CARTESIAN_POINT('Ctrl Pts',(0.24378312716608,55.0643219256763,11.0897728253293));
#50819=CARTESIAN_POINT('Ctrl Pts',(1.14359453483077,55.179591554497,11.4234917272422));
#50820=CARTESIAN_POINT('Ctrl Pts',(1.594107580686,55.2546269955245,11.8256735534423));
#50821=CARTESIAN_POINT('Ctrl Pts',(1.76820356899201,55.2881321265545,12.0304265488723));
#50822=CARTESIAN_POINT('Ctrl Pts',(2.00000619829663,55.3385484417741,12.3614071208809));
#50823=CARTESIAN_POINT('Ctrl Pts',(2.3374038248435,55.4486533549761,13.1945583269953));
#50824=CARTESIAN_POINT('Ctrl Pts',(2.13503615164275,55.586785700239,14.3588883789362));
#50825=CARTESIAN_POINT('Ctrl Pts',(1.46088944635544,55.710058084209,15.1074084078187));
#50826=CARTESIAN_POINT('Ctrl Pts',(0.977148776715703,55.781195511413,15.4116879900337));
#50827=CARTESIAN_POINT('Ctrl Pts',(0.173924477173412,55.8886095419895,15.7317674296736));
#50828=CARTESIAN_POINT('Ctrl Pts',(-1.22564291596938,56.0523911368355,15.6173328388221));
#50829=CARTESIAN_POINT('Ctrl Pts',(-2.53412984108696,56.2765988592834,14.2074858335199));
#50830=CARTESIAN_POINT('Ctrl Pts',(-2.55113652423423,56.5067311267252,12.2305709116292));
#50831=CARTESIAN_POINT('Ctrl Pts',(-1.34397736419971,56.7166040708691,10.8961407544736));
#50832=CARTESIAN_POINT('Ctrl Pts',(0.171376806954028,56.9041113720079,10.5649999101602));
#50833=CARTESIAN_POINT('Ctrl Pts',(1.46804367168455,57.0674713743434,10.9334596080689));
#50834=CARTESIAN_POINT('Ctrl Pts',(2.49426073708746,57.2403616973154,11.9284104985044));
#50835=CARTESIAN_POINT('Ctrl Pts',(2.90875309006288,57.4231414817237,13.3922632584958));
#50836=CARTESIAN_POINT('Ctrl Pts',(2.46434240099787,57.6161587765882,14.937772993555));
#50837=CARTESIAN_POINT('Ctrl Pts',(1.25327287152259,57.8123061978857,16.0331881492274));
#50838=CARTESIAN_POINT('Ctrl Pts',(-0.378776292917826,58.0114932343869,
16.3296297051516));
#50839=CARTESIAN_POINT('Ctrl Pts',(-1.94406501847761,58.2136131696184,15.7113511535389));
#50840=CARTESIAN_POINT('Ctrl Pts',(-2.96182287074345,58.4185468107759,14.3416783720341));
#50841=CARTESIAN_POINT('Ctrl Pts',(-3.10552330152979,58.6261601145185,12.6185996185993));
#50842=CARTESIAN_POINT('Ctrl Pts',(-2.57485127558882,58.766258906306,11.5799921611984));
#50843=CARTESIAN_POINT('Ctrl Pts',(-2.1894814666802,58.8367038442533,11.1676829891756));
#50844=CARTESIAN_POINT('Ctrl Pts',(-1.29179640210147,50.1461249705794,11.1593417706458));
#50845=CARTESIAN_POINT('Ctrl Pts',(-1.17586424793724,50.1627439522706,11.0949541057819));
#50846=CARTESIAN_POINT('Ctrl Pts',(-1.05506647233865,50.1792583497506,11.0397640939357));
#50847=CARTESIAN_POINT('Ctrl Pts',(-0.806845719013178,50.2121678519162,
10.9492055679426));
#50848=CARTESIAN_POINT('Ctrl Pts',(-0.679414851388805,50.2285627637462,
10.9138653769205));
#50849=CARTESIAN_POINT('Ctrl Pts',(-0.529965369448136,50.2475136893414,
10.8852859534053));
#50850=CARTESIAN_POINT('Ctrl Pts',(-0.509490630910326,50.2501040671278,
10.8816456967675));
#50851=CARTESIAN_POINT('Ctrl Pts',(-0.35763717065511,50.2692794071308,10.8566918042585));
#50852=CARTESIAN_POINT('Ctrl Pts',(-0.224930869811676,50.2858350211732,
10.8461950652809));
#50853=CARTESIAN_POINT('Ctrl Pts',(-0.0521410480261596,50.3074751348745,
10.8463357374599));
#50854=CARTESIAN_POINT('Ctrl Pts',(-0.0116722601119271,50.3125494626139,
10.8473628673328));
#50855=CARTESIAN_POINT('Ctrl Pts',(0.193236338609998,50.3383118287223,10.8575462627135));
#50856=CARTESIAN_POINT('Ctrl Pts',(0.356593166603047,50.3587994429838,10.8821914828471));
#50857=CARTESIAN_POINT('Ctrl Pts',(0.680754099283437,50.4004080786556,10.9644180392955));
#50858=CARTESIAN_POINT('Ctrl Pts',(0.841169971214191,50.4215200682444,11.0233226785241));
#50859=CARTESIAN_POINT('Ctrl Pts',(1.02106458037202,50.4465567330081,11.1121586059517));
#50860=CARTESIAN_POINT('Ctrl Pts',(1.04899253268544,50.450485635207,11.1266537702159));
#50861=CARTESIAN_POINT('Ctrl Pts',(1.15005120124451,50.4648734370134,11.1817332145071));
#50862=CARTESIAN_POINT('Ctrl Pts',(1.2211901834219,50.4753360438438,11.2256500811951));
#50863=CARTESIAN_POINT('Ctrl Pts',(1.418399848808,50.5054907842792,11.3621121143303));
#50864=CARTESIAN_POINT('Ctrl Pts',(1.53778885079935,50.5250399263045,11.4635464474702));
#50865=CARTESIAN_POINT('Ctrl Pts',(1.75695410848228,50.5643650866753,11.6889686450017));
#50866=CARTESIAN_POINT('Ctrl Pts',(1.85622983574385,50.5841363126383,11.8134137692257));
#50867=CARTESIAN_POINT('Ctrl Pts',(2.01079050490025,50.6195700815444,12.051823621597));
#50868=CARTESIAN_POINT('Ctrl Pts',(2.07090096760105,50.6352647387523,12.1629203938869));
#50869=CARTESIAN_POINT('Ctrl Pts',(2.1224071124382,50.6512188039548,12.2801085395122));
#50870=CARTESIAN_POINT('Ctrl Pts',(2.12339031658304,50.6515244779251,12.2823553349035));
#50871=CARTESIAN_POINT('Ctrl Pts',(2.19638114822366,50.6743013862446,12.4498845871826));
#50872=CARTESIAN_POINT('Ctrl Pts',(2.24857224748294,50.6967310898809,12.6229960356089));
#50873=CARTESIAN_POINT('Ctrl Pts',(2.29457780293144,50.7289582945877,12.8768626019824));
#50874=CARTESIAN_POINT('Ctrl Pts',(2.3047165576568,50.7388180282312,12.9552293374338));
#50875=CARTESIAN_POINT('Ctrl Pts',(2.32423796476578,50.7700886808865,13.2047365765726));
#50876=CARTESIAN_POINT('Ctrl Pts',(2.31867125305314,50.7914312158333,13.376466475896));
#50877=CARTESIAN_POINT('Ctrl Pts',(2.28267958031064,50.8232467749868,13.6287825259408));
#50878=CARTESIAN_POINT('Ctrl Pts',(2.26609809947773,50.833822646406,13.7119840627583));
#50879=CARTESIAN_POINT('Ctrl Pts',(2.20724046855379,50.8632383604427,13.9400923928012));
#50880=CARTESIAN_POINT('Ctrl Pts',(2.15500951480601,50.8820368501375,14.0820711253277));
#50881=CARTESIAN_POINT('Ctrl Pts',(2.04534812313239,50.9135193781906,14.3092231015875));
#50882=CARTESIAN_POINT('Ctrl Pts',(1.99489994162873,50.9262398524308,14.3980630649955));
#50883=CARTESIAN_POINT('Ctrl Pts',(1.89729738157964,50.9483522867086,14.5459858768816));
#50884=CARTESIAN_POINT('Ctrl Pts',(1.85262945323311,50.9577594047374,14.6068481547701));
#50885=CARTESIAN_POINT('Ctrl Pts',(1.78652888145326,50.9708331892289,14.6881566921951));
#50886=CARTESIAN_POINT('Ctrl Pts',(1.7674606261628,50.9745163949834,14.7106999398698));
#50887=CARTESIAN_POINT('Ctrl Pts',(1.66758140032378,50.9933823288577,14.8242170465195));
#50888=CARTESIAN_POINT('Ctrl Pts',(1.58001302620175,51.0085365102027,14.9089121159274));
#50889=CARTESIAN_POINT('Ctrl Pts',(1.46837758706177,51.026560523629,15.0004222798649));
#50890=CARTESIAN_POINT('Ctrl Pts',(1.45013318498345,51.0294685360955,15.0148993419957));
#50891=CARTESIAN_POINT('Ctrl Pts',(1.3332453445594,51.0478721224418,15.1046435322073));
#50892=CARTESIAN_POINT('Ctrl Pts',(1.2286840050754,51.063325503062,15.171574111418));
#50893=CARTESIAN_POINT('Ctrl Pts',(1.03797613055253,51.0902744474102,15.2727381849875));
#50894=CARTESIAN_POINT('Ctrl Pts',(0.953761854894311,51.1017936342927,15.3109637342375));
#50895=CARTESIAN_POINT('Ctrl Pts',(0.83654647437363,51.1174529760332,15.3558387378948));
#50896=CARTESIAN_POINT('Ctrl Pts',(0.805065623226275,51.121623155736,15.3671002953147));
#50897=CARTESIAN_POINT('Ctrl Pts',(0.751497073195426,51.1286671720629,15.3849433348014));
#50898=CARTESIAN_POINT('Ctrl Pts',(0.729504660089768,51.1315444632091,15.3918983640672));
#50899=CARTESIAN_POINT('Ctrl Pts',(0.59077613133458,51.1496119923445,15.4334553885158));
#50900=CARTESIAN_POINT('Ctrl Pts',(0.471527395855336,51.1647775623704,15.4589347154352));
#50901=CARTESIAN_POINT('Ctrl Pts',(0.255444467995113,51.1919823954698,15.4868218740711));
#50902=CARTESIAN_POINT('Ctrl Pts',(0.158948751454997,51.2040344282913,15.4928509746133));
#50903=CARTESIAN_POINT('Ctrl Pts',(-0.0606144237304076,51.2314718057864,
15.4915853832341));
#50904=CARTESIAN_POINT('Ctrl Pts',(-0.183507513308038,51.2468396234302,
15.4800566095026));
#50905=CARTESIAN_POINT('Ctrl Pts',(-0.346682219876221,51.2675349729358,
15.4508484975454));
#50906=CARTESIAN_POINT('Ctrl Pts',(-0.388853073455517,51.2729104729639,
15.4420071485642));
#50907=CARTESIAN_POINT('Ctrl Pts',(-0.460714312994654,51.2821326748638,
15.4247369920905));
#50908=CARTESIAN_POINT('Ctrl Pts',(-0.4905775182599,51.2859838954058,15.4168935616789));
#50909=CARTESIAN_POINT('Ctrl Pts',(-0.662388445407937,51.3082698972205,
15.3679111806786));
#50910=CARTESIAN_POINT('Ctrl Pts',(-0.800135864393537,51.326651692665,15.3132516977476));
#50911=CARTESIAN_POINT('Ctrl Pts',(-1.05111869021365,51.3619071966508,15.1832536191353));
#50912=CARTESIAN_POINT('Ctrl Pts',(-1.16541856053576,51.378789975927,15.1097891701591));
#50913=CARTESIAN_POINT('Ctrl Pts',(-1.34032287189366,51.4066220560649,14.9717203670751));
#50914=CARTESIAN_POINT('Ctrl Pts',(-1.40583084792222,51.4176049990611,14.9128329597658));
#50915=CARTESIAN_POINT('Ctrl Pts',(-1.55710172033224,51.4445494309785,14.7589776593018));
#50916=CARTESIAN_POINT('Ctrl Pts',(-1.63849547777328,51.4605055280583,14.6597068329473));
#50917=CARTESIAN_POINT('Ctrl Pts',(-1.78396947503599,51.492695415786,14.446550254468));
#50918=CARTESIAN_POINT('Ctrl Pts',(-1.84762121195314,51.5089274427981,14.3323886904574));
#50919=CARTESIAN_POINT('Ctrl Pts',(-1.95039781399511,51.5405318486693,14.1008765240707));
#50920=CARTESIAN_POINT('Ctrl Pts',(-1.99053792233632,51.5559086533289,13.9839319099237));
#50921=CARTESIAN_POINT('Ctrl Pts',(-2.05051883101226,51.5873985547467,13.7390920925521));
#50922=CARTESIAN_POINT('Ctrl Pts',(-2.06913373203656,51.6035060902381,13.6109490311358));
#50923=CARTESIAN_POINT('Ctrl Pts',(-2.07658307411553,51.6209979176689,13.4710355237018));
#50924=CARTESIAN_POINT('Ctrl Pts',(-2.07710333853888,51.6224437457318,13.4594649641365));
#50925=CARTESIAN_POINT('Ctrl Pts',(-2.08161127178146,51.6377785645872,13.3367015492881));
#50926=CARTESIAN_POINT('Ctrl Pts',(-2.0768906847889,51.6516451125443,13.225232731368));
#50927=CARTESIAN_POINT('Ctrl Pts',(-2.04996245357585,51.6795430946767,13.002999483218));
#50928=CARTESIAN_POINT('Ctrl Pts',(-2.02747647562859,51.6935736212083,12.8922761942963));
#50929=CARTESIAN_POINT('Ctrl Pts',(-1.96986329330764,51.7194408597748,12.6929337032827));
#50930=CARTESIAN_POINT('Ctrl Pts',(-1.93717477217231,51.7312872218979,12.603511469113));
#50931=CARTESIAN_POINT('Ctrl Pts',(-1.85250536853668,51.7570978496006,12.414821694989));
#50932=CARTESIAN_POINT('Ctrl Pts',(-1.79808195042894,51.7710509339456,12.3167695391442));
#50933=CARTESIAN_POINT('Ctrl Pts',(-1.69222557680776,51.7948861173685,12.1578491771332));
#50934=CARTESIAN_POINT('Ctrl Pts',(-1.64440025423007,51.8047897740442,12.0943729990204));
#50935=CARTESIAN_POINT('Ctrl Pts',(-1.51889540976364,51.8290393881842,11.9461348902174));
#50936=CARTESIAN_POINT('Ctrl Pts',(-1.43727839884043,51.8433817647499,11.864518711087));
#50937=CARTESIAN_POINT('Ctrl Pts',(-1.26018468176299,51.8723019326257,11.7146941756349));
#50938=CARTESIAN_POINT('Ctrl Pts',(-1.16445722035746,51.8868784620027,11.646799062312));
#50939=CARTESIAN_POINT('Ctrl Pts',(-1.0403118987082,51.9048138851257,11.5742565394263));
#50940=CARTESIAN_POINT('Ctrl Pts',(-1.0165580949766,51.9082050026956,11.5610270483265));
#50941=CARTESIAN_POINT('Ctrl Pts',(-0.886230181033722,51.9266059286065,
11.4919699006493));
#50942=CARTESIAN_POINT('Ctrl Pts',(-0.774980714599116,51.9415806150534,
11.4456417155808));
#50943=CARTESIAN_POINT('Ctrl Pts',(-0.546665599177198,51.9714506849704,
11.3734376767949));
#50944=CARTESIAN_POINT('Ctrl Pts',(-0.429601728614386,51.9863460715534,
11.3475620219376));
#50945=CARTESIAN_POINT('Ctrl Pts',(-0.20907029431664,52.0141170173263,11.3185983547831));
#50946=CARTESIAN_POINT('Ctrl Pts',(-0.105507065200747,52.0270354059357,
11.3129390984546));
#50947=CARTESIAN_POINT('Ctrl Pts',(0.0968600497403189,52.0523391978825,
11.3175607270828));
#50948=CARTESIAN_POINT('Ctrl Pts',(0.195690778708763,52.0647257440447,11.3272285239059));
#50949=CARTESIAN_POINT('Ctrl Pts',(0.394666389716627,52.0900046130345,11.3624215846142));
#50950=CARTESIAN_POINT('Ctrl Pts',(0.494666261615732,52.1028943938056,11.388646349898));
#50951=CARTESIAN_POINT('Ctrl Pts',(0.650436010770195,52.1234862819425,11.4427582385991));
#50952=CARTESIAN_POINT('Ctrl Pts',(0.708009702836697,52.1312170896882,11.465854397369));
#50953=CARTESIAN_POINT('Ctrl Pts',(0.908378342693344,52.1586620965296,11.557219078334));
#50954=CARTESIAN_POINT('Ctrl Pts',(1.04433397233415,52.1783760941834,11.6399044718939));
#50955=CARTESIAN_POINT('Ctrl Pts',(1.25596480420899,52.2119564581144,11.8058424032475));
#50956=CARTESIAN_POINT('Ctrl Pts',(1.33764786615372,52.2258487508522,11.8818722370674));
#50957=CARTESIAN_POINT('Ctrl Pts',(1.47438965523274,52.2513576139545,12.0335455604943));
#50958=CARTESIAN_POINT('Ctrl Pts',(1.5316168485671,52.262985037636,12.1073305051343));
#50959=CARTESIAN_POINT('Ctrl Pts',(1.67651718649737,52.2955324176947,12.3244608194884));
#50960=CARTESIAN_POINT('Ctrl Pts',(1.751625979797,52.3164404623527,12.4761088530483));
#50961=CARTESIAN_POINT('Ctrl Pts',(1.85747547577759,52.3568550308588,12.7825292048041));
#50962=CARTESIAN_POINT('Ctrl Pts',(1.89071205140988,52.3763669053139,12.9365034058105));
#50963=CARTESIAN_POINT('Ctrl Pts',(1.90496519311471,52.3971496326665,13.1022334456341));
#50964=CARTESIAN_POINT('Ctrl Pts',(1.9057728968132,52.3984581090635,13.1126750815767));
#50965=CARTESIAN_POINT('Ctrl Pts',(1.90809346985574,52.4026904974495,13.1464687856724));
#50966=CARTESIAN_POINT('Ctrl Pts',(1.90924527016826,52.4056137288121,13.1698392143514));
#50967=CARTESIAN_POINT('Ctrl Pts',(1.91309537134773,52.4215488005786,13.2973190082068));
#50968=CARTESIAN_POINT('Ctrl Pts',(1.90743589505222,52.4344232528633,13.4013571204969));
#50969=CARTESIAN_POINT('Ctrl Pts',(1.87915170135077,52.460524475602,13.6106265793392));
#50970=CARTESIAN_POINT('Ctrl Pts',(1.85591940311975,52.4737471623773,13.7157662255528));
#50971=CARTESIAN_POINT('Ctrl Pts',(1.7926210353516,52.5003841586456,13.9216751125366));
#50972=CARTESIAN_POINT('Ctrl Pts',(1.7523861734177,52.5137990825969,14.0223908190224));
#50973=CARTESIAN_POINT('Ctrl Pts',(1.68896709292507,52.5316406160847,14.1496679706925));
#50974=CARTESIAN_POINT('Ctrl Pts',(1.67285356038215,52.5359612550644,14.1799816478008));
#50975=CARTESIAN_POINT('Ctrl Pts',(1.61463063172757,52.5509024881449,14.2828327404829));
#50976=CARTESIAN_POINT('Ctrl Pts',(1.5685788779595,52.5614898243686,14.3532338477688));
#50977=CARTESIAN_POINT('Ctrl Pts',(1.467961958202,52.5825407647531,14.4867185085709));
#50978=CARTESIAN_POINT('Ctrl Pts',(1.4134602066283,52.5930047153806,14.5498495048677));
#50979=CARTESIAN_POINT('Ctrl Pts',(1.34293420300396,52.6055738417265,14.620898234876));
#50980=CARTESIAN_POINT('Ctrl Pts',(1.33078705314162,52.6077073105751,14.6327913976951));
#50981=CARTESIAN_POINT('Ctrl Pts',(1.25778486523938,52.6203483968795,14.7022350773085));
#50982=CARTESIAN_POINT('Ctrl Pts',(1.19305604375341,52.6308261052914,14.7555888359258));
#50983=CARTESIAN_POINT('Ctrl Pts',(1.05770518068061,52.6516236232434,14.8526032457158));
#50984=CARTESIAN_POINT('Ctrl Pts',(0.987135813715497,52.6619440270014,14.8963380206378));
#50985=CARTESIAN_POINT('Ctrl Pts',(0.828435187824385,52.6843151760371,14.9810847293576));
#50986=CARTESIAN_POINT('Ctrl Pts',(0.739230858262599,52.6964132353955,15.0203306293797));
#50987=CARTESIAN_POINT('Ctrl Pts',(0.55667191136831,52.7205449514636,15.0849210004443));
#50988=CARTESIAN_POINT('Ctrl Pts',(0.463342791847309,52.7325785749457,15.1103445647152));
#50989=CARTESIAN_POINT('Ctrl Pts',(0.278547995135265,52.7560859638772,15.1461123668855));
#50990=CARTESIAN_POINT('Ctrl Pts',(0.187197112947158,52.767559680129,15.1571043406759));
#50991=CARTESIAN_POINT('Ctrl Pts',(0.0333489091256805,52.7868272388106,
15.1641428131738));
#50992=CARTESIAN_POINT('Ctrl Pts',(-0.0290093074805301,52.7946215233249,
15.1638501338707));
#50993=CARTESIAN_POINT('Ctrl Pts',(-0.130161023150543,52.8072974862492,
15.1580738250435));
#50994=CARTESIAN_POINT('Ctrl Pts',(-0.16903749864418,52.812180450813,15.154568420337));
#50995=CARTESIAN_POINT('Ctrl Pts',(-0.282951798217108,52.8265496495956,
15.1404086688194));
#50996=CARTESIAN_POINT('Ctrl Pts',(-0.357502667492476,52.836032692471,15.1261265810317));
#50997=CARTESIAN_POINT('Ctrl Pts',(-0.487431559665585,52.8528096790146,
15.0927052855356));
#50998=CARTESIAN_POINT('Ctrl Pts',(-0.543311667052286,52.8601106545406,
15.0754124712946));
#50999=CARTESIAN_POINT('Ctrl Pts',(-0.672468927188591,52.8772555493765,
15.0287275110183));
#51000=CARTESIAN_POINT('Ctrl Pts',(-0.744968824082721,52.8869749370748,
14.9972904130696));
#51001=CARTESIAN_POINT('Ctrl Pts',(-0.88625594940133,52.9064666469949,14.9254612112881));
#51002=CARTESIAN_POINT('Ctrl Pts',(-0.954992927424705,52.9162383603264,
14.8849712410689));
#51003=CARTESIAN_POINT('Ctrl Pts',(-1.03237681943862,52.927810179237,14.8326387508207));
#51004=CARTESIAN_POINT('Ctrl Pts',(-1.04377042911234,52.9295293459953,14.8247515713228));
#51005=CARTESIAN_POINT('Ctrl Pts',(-1.12772375223892,52.9423197256733,14.7652693977536));
#51006=CARTESIAN_POINT('Ctrl Pts',(-1.19671876868382,52.9535337352294,14.7087197105301));
#51007=CARTESIAN_POINT('Ctrl Pts',(-1.29040020935121,52.9698180030159,14.6202129638619));
#51008=CARTESIAN_POINT('Ctrl Pts',(-1.31856185527217,52.9748705118411,14.5918639537878));
#51009=CARTESIAN_POINT('Ctrl Pts',(-1.37505353547673,52.9853433031168,14.5312336301288));
#51010=CARTESIAN_POINT('Ctrl Pts',(-1.40327439448105,52.9907017870527,14.4988476507206));
#51011=CARTESIAN_POINT('Ctrl Pts',(-1.47406010616561,53.0047365927575,14.4115649842979));
#51012=CARTESIAN_POINT('Ctrl Pts',(-1.51472285237196,53.0134194689159,14.3551075209223));
#51013=CARTESIAN_POINT('Ctrl Pts',(-1.56993877475166,53.0263273541817,14.267892303756));
#51014=CARTESIAN_POINT('Ctrl Pts',(-1.5871878131941,53.0305548494566,14.2388040871341));
#51015=CARTESIAN_POINT('Ctrl Pts',(-1.61596633367774,53.03796972398,14.1869558536698));
#51016=CARTESIAN_POINT('Ctrl Pts',(-1.62786167879273,53.0411579930626,14.1643930901733));
#51017=CARTESIAN_POINT('Ctrl Pts',(-1.65847188291452,53.0497088701303,14.1032180448185));
#51018=CARTESIAN_POINT('Ctrl Pts',(-1.67633651634066,53.0550296808571,14.064167328875));
#51019=CARTESIAN_POINT('Ctrl Pts',(-1.72761725199409,53.0712352593059,13.941490778788));
#51020=CARTESIAN_POINT('Ctrl Pts',(-1.75613310696713,53.0823149282675,13.8558862008896));
#51021=CARTESIAN_POINT('Ctrl Pts',(-1.80125458925947,53.1049138539715,13.6792179862168));
#51022=CARTESIAN_POINT('Ctrl Pts',(-1.81751391322657,53.1164368270852,13.5880682666396));
#51023=CARTESIAN_POINT('Ctrl Pts',(-1.83659901735704,53.1394540437642,13.4053349580862));
#51024=CARTESIAN_POINT('Ctrl Pts',(-1.8395484580033,53.1509475590332,13.3137620309028));
#51025=CARTESIAN_POINT('Ctrl Pts',(-1.83232956546884,53.1733429593277,13.1360677270543));
#51026=CARTESIAN_POINT('Ctrl Pts',(-1.8228506889041,53.184243814313,13.0499143095028));
#51027=CARTESIAN_POINT('Ctrl Pts',(-1.79514578072454,53.2036006190261,12.8986188081948));
#51028=CARTESIAN_POINT('Ctrl Pts',(-1.77933056012774,53.2120616708149,12.8330613116409));
#51029=CARTESIAN_POINT('Ctrl Pts',(-1.75553580489027,53.2223153072095,12.7546790551827));
#51030=CARTESIAN_POINT('Ctrl Pts',(-1.75116778966746,53.2241201943003,12.740898178659));
#51031=CARTESIAN_POINT('Ctrl Pts',(-1.72018614796545,53.2364149462963,12.6471902915767));
#51032=CARTESIAN_POINT('Ctrl Pts',(-1.68798199364942,53.246766229533,12.5691261348581));
#51033=CARTESIAN_POINT('Ctrl Pts',(-1.61338950991954,53.2672915820224,12.4187346356801));
#51034=CARTESIAN_POINT('Ctrl Pts',(-1.57108010244899,53.2774664081388,12.3463690886902));
#51035=CARTESIAN_POINT('Ctrl Pts',(-1.48230345323922,53.296791016633,12.2154954163202));
#51036=CARTESIAN_POINT('Ctrl Pts',(-1.43677168397069,53.3059333969882,12.1563347568848));
#51037=CARTESIAN_POINT('Ctrl Pts',(-1.32189492162835,53.3276685152984,12.0241407949197));
#51038=CARTESIAN_POINT('Ctrl Pts',(-1.24956792870111,53.3402656824691,11.9531049964235));
#51039=CARTESIAN_POINT('Ctrl Pts',(-1.09319962842738,53.3657518310656,11.8222453555277));
#51040=CARTESIAN_POINT('Ctrl Pts',(-1.0089838251504,53.3786421421447,11.7626301584854));
#51041=CARTESIAN_POINT('Ctrl Pts',(-0.835660084156748,53.4038730474459,
11.6605321070325));
#51042=CARTESIAN_POINT('Ctrl Pts',(-0.746904437412114,53.4162141446784,
11.6174379818867));
#51043=CARTESIAN_POINT('Ctrl Pts',(-0.55687120493277,53.4416891463299,11.5443386851595));
#51044=CARTESIAN_POINT('Ctrl Pts',(-0.455153850915069,53.4548165153692,
11.5154912212315));
#51045=CARTESIAN_POINT('Ctrl Pts',(-0.253404567611201,53.4802178240072,
11.4763900477341));
#51046=CARTESIAN_POINT('Ctrl Pts',(-0.153553967050764,53.4925010753352,
11.4652586462183));
#51047=CARTESIAN_POINT('Ctrl Pts',(-0.0480126903616401,53.5053244641644,
11.4616570030259));
#51048=CARTESIAN_POINT('Ctrl Pts',(-0.0426079119451699,53.5059807100768,
11.4614950504468));
#51049=CARTESIAN_POINT('Ctrl Pts',(0.0513733894600363,53.5173845659481,
11.4590691863365));
#51050=CARTESIAN_POINT('Ctrl Pts',(0.140254137527553,53.5283771592707,11.4632546135913));
#51051=CARTESIAN_POINT('Ctrl Pts',(0.310685215532395,53.5499414985786,11.4835636241241));
#51052=CARTESIAN_POINT('Ctrl Pts',(0.392326816791214,53.5604918787679,11.4988643053244));
#51053=CARTESIAN_POINT('Ctrl Pts',(0.582550331029838,53.5856968951546,11.5478513516785));
#51054=CARTESIAN_POINT('Ctrl Pts',(0.690080426533256,53.6001540354735,11.5858565329136));
#51055=CARTESIAN_POINT('Ctrl Pts',(0.838421464801602,53.6208203533813,11.6543071758409));
#51056=CARTESIAN_POINT('Ctrl Pts',(0.882775666748859,53.6271001355276,11.6770034415749));
#51057=CARTESIAN_POINT('Ctrl Pts',(1.02543888640962,53.6477191786957,11.7577221125681));
#51058=CARTESIAN_POINT('Ctrl Pts',(1.11946751763241,53.6619956713904,11.823522325871));
#51059=CARTESIAN_POINT('Ctrl Pts',(1.25746426902585,53.6844652997591,11.9401938591112));
#51060=CARTESIAN_POINT('Ctrl Pts',(1.30587427989571,53.6926955982797,11.9857312680104));
#51061=CARTESIAN_POINT('Ctrl Pts',(1.41651485955325,53.7125031119117,12.1012932274944));
#51062=CARTESIAN_POINT('Ctrl Pts',(1.4763566033618,53.7241420850694,12.1739261982714));
#51063=CARTESIAN_POINT('Ctrl Pts',(1.58916731369618,53.7484867988033,12.333991562844));
#51064=CARTESIAN_POINT('Ctrl Pts',(1.64111509444718,53.7611989419891,12.4221570457005));
#51065=CARTESIAN_POINT('Ctrl Pts',(1.7009760206621,53.7783822065853,12.5461529278465));
#51066=CARTESIAN_POINT('Ctrl Pts',(1.71552967964692,53.7828269823785,12.5786597637478));
#51067=CARTESIAN_POINT('Ctrl Pts',(1.75544958828922,53.7958795401923,12.6752638704256));
#51068=CARTESIAN_POINT('Ctrl Pts',(1.77820933196254,53.8044958945969,12.7404933543574));
#51069=CARTESIAN_POINT('Ctrl Pts',(1.81016291687527,53.818835618921,12.8507253527809));
#51070=CARTESIAN_POINT('Ctrl Pts',(1.82134356595601,53.8245549610328,12.8951328802289));
#51071=CARTESIAN_POINT('Ctrl Pts',(1.83566011474081,53.8331932585586,12.9626944877087));
#51072=CARTESIAN_POINT('Ctrl Pts',(1.84007397545403,53.8361016976207,12.985597685492));
#51073=CARTESIAN_POINT('Ctrl Pts',(1.85783388420497,53.8490750701629,13.0883439639632));
#51074=CARTESIAN_POINT('Ctrl Pts',(1.86630207219487,53.8590657291333,13.1690460907899));
#51075=CARTESIAN_POINT('Ctrl Pts',(1.87260437825337,53.8786337609155,13.3281044480159));
#51076=CARTESIAN_POINT('Ctrl Pts',(1.87081981580395,53.8882126943262,13.4064365546596));
#51077=CARTESIAN_POINT('Ctrl Pts',(1.8576294032269,53.9073808205236,13.5621825064978));
#51078=CARTESIAN_POINT('Ctrl Pts',(1.846264239738,53.9169697910096,13.6395986515081));
#51079=CARTESIAN_POINT('Ctrl Pts',(1.81420647608039,53.9362077923623,13.7920280038178));
#51080=CARTESIAN_POINT('Ctrl Pts',(1.7935810874306,53.9458558834466,13.867054064916));
#51081=CARTESIAN_POINT('Ctrl Pts',(1.76504038369673,53.95689471959,13.950259512124));
#51082=CARTESIAN_POINT('Ctrl Pts',(1.76161259861716,53.9581910207318,13.959989761124));
#51083=CARTESIAN_POINT('Ctrl Pts',(1.72936900531379,53.9701216179985,14.0491502227609));
#51084=CARTESIAN_POINT('Ctrl Pts',(1.69532154673149,53.9808329901845,14.1269135916044));
#51085=CARTESIAN_POINT('Ctrl Pts',(1.61731520646525,54.0022769951949,14.2770750666882));
#51086=CARTESIAN_POINT('Ctrl Pts',(1.57340457294557,54.0130092894204,14.3494961122909));
#51087=CARTESIAN_POINT('Ctrl Pts',(1.48890474205988,54.0316556374554,14.469719730799));
#51088=CARTESIAN_POINT('Ctrl Pts',(1.45046576971118,54.0395706510287,14.5189981605161));
#51089=CARTESIAN_POINT('Ctrl Pts',(1.35457793571589,54.0580987293182,14.6297651066965));
#51090=CARTESIAN_POINT('Ctrl Pts',(1.29514743632753,54.0687001937351,14.6895977819501));
#51091=CARTESIAN_POINT('Ctrl Pts',(1.20499617301088,54.0837609105672,14.7692549802991));
#51092=CARTESIAN_POINT('Ctrl Pts',(1.17730528186333,54.0882638247712,14.7923831782251));
#51093=CARTESIAN_POINT('Ctrl Pts',(1.07963596307844,54.1037564082215,14.8695287126092));
#51094=CARTESIAN_POINT('Ctrl Pts',(1.00629893197122,54.1148030853843,14.9194748670905));
#51095=CARTESIAN_POINT('Ctrl Pts',(0.867063621703206,54.1349395177051,15.0008702222197));
#51096=CARTESIAN_POINT('Ctrl Pts',(0.802214373268047,54.1440219150142,15.0340303763525));
#51097=CARTESIAN_POINT('Ctrl Pts',(0.720984782991892,54.1551055669021,15.0699821747632));
#51098=CARTESIAN_POINT('Ctrl Pts',(0.706253100245556,54.1571043616304,15.0762865178801));
#51099=CARTESIAN_POINT('Ctrl Pts',(0.605461147890766,54.1707071055754,15.1179645308399));
#51100=CARTESIAN_POINT('Ctrl Pts',(0.516785170310873,54.1823182943499,15.1474599833267));
#51101=CARTESIAN_POINT('Ctrl Pts',(0.343916787107568,54.2045478640552,15.1914614216871));
#51102=CARTESIAN_POINT('Ctrl Pts',(0.260032551484708,54.2151620925175,15.2070720870098));
#51103=CARTESIAN_POINT('Ctrl Pts',(0.0938161801991205,54.2360529814985,
15.2265141889014));
#51104=CARTESIAN_POINT('Ctrl Pts',(0.0115174049717453,54.2463306464609,
15.2307636250779));
#51105=CARTESIAN_POINT('Ctrl Pts',(-0.0783049134808558,54.2575614895967,
15.2293221490236));
#51106=CARTESIAN_POINT('Ctrl Pts',(-0.0858120862299798,54.25850024603,15.22915538111));
#51107=CARTESIAN_POINT('Ctrl Pts',(-0.17502821521666,54.269658490363,15.2266208581259));
#51108=CARTESIAN_POINT('Ctrl Pts',(-0.256683691118636,54.2798906327115,
15.2187874177528));
#51109=CARTESIAN_POINT('Ctrl Pts',(-0.345476748668277,54.29111444431,15.2044954604915));
#51110=CARTESIAN_POINT('Ctrl Pts',(-0.353343031094722,54.2921096211492,
15.2031790943686));
#51111=CARTESIAN_POINT('Ctrl Pts',(-0.423608049976724,54.3010071105924,
15.1909732193392));
#51112=CARTESIAN_POINT('Ctrl Pts',(-0.485548963003283,54.3088688662889,
15.1772294827954));
#51113=CARTESIAN_POINT('Ctrl Pts',(-0.608046839776311,54.324586298138,15.1439180214162));
#51114=CARTESIAN_POINT('Ctrl Pts',(-0.668602551159439,54.3324419655529,
15.1243446958));
#51115=CARTESIAN_POINT('Ctrl Pts',(-0.778230478913236,54.3469472519682,
15.0829453712371));
#51116=CARTESIAN_POINT('Ctrl Pts',(-0.827599995327668,54.3535904692277,
15.0619685912211));
#51117=CARTESIAN_POINT('Ctrl Pts',(-0.950976246159398,54.3705827952107,
15.0033180862864));
#51118=CARTESIAN_POINT('Ctrl Pts',(-1.02383873525204,54.3809722959893,14.9628079756871));
#51119=CARTESIAN_POINT('Ctrl Pts',(-1.16412019588339,54.4018334782146,14.8728024421635));
#51120=CARTESIAN_POINT('Ctrl Pts',(-1.23153866919633,54.4123051632831,14.8233071516301));
#51121=CARTESIAN_POINT('Ctrl Pts',(-1.35968369748512,54.4332789078702,14.7161609033528));
#51122=CARTESIAN_POINT('Ctrl Pts',(-1.42041521979204,54.4437809388632,14.6585166132706));
#51123=CARTESIAN_POINT('Ctrl Pts',(-1.51506550555719,54.4612668319717,14.5563869130981));
#51124=CARTESIAN_POINT('Ctrl Pts',(-1.55114464821752,54.4682489634417,14.5139754319317));
#51125=CARTESIAN_POINT('Ctrl Pts',(-1.62147125016784,54.482594105633,14.4236617534963));
#51126=CARTESIAN_POINT('Ctrl Pts',(-1.65550906414146,54.4899569418111,14.3755861175269));
#51127=CARTESIAN_POINT('Ctrl Pts',(-1.76160584561978,54.514421556358,14.2108807721874));
#51128=CARTESIAN_POINT('Ctrl Pts',(-1.82389696878703,54.5315630777004,14.087480370682));
#51129=CARTESIAN_POINT('Ctrl Pts',(-1.92267203028798,54.5660298041196,13.8291421681136));
#51130=CARTESIAN_POINT('Ctrl Pts',(-1.95901400714649,54.5833555000449,13.6941433984061));
#51131=CARTESIAN_POINT('Ctrl Pts',(-1.98984229918007,54.6077633743642,13.5008599846904));
#51132=CARTESIAN_POINT('Ctrl Pts',(-1.99636526435242,54.6147998337516,13.4447789288554));
#51133=CARTESIAN_POINT('Ctrl Pts',(-2.00694691888882,54.6330408434406,13.2989647806689));
#51134=CARTESIAN_POINT('Ctrl Pts',(-2.00729272169291,54.6442604477564,13.20885705357));
#51135=CARTESIAN_POINT('Ctrl Pts',(-1.99196859307335,54.674595210111,12.966254759167));
#51136=CARTESIAN_POINT('Ctrl Pts',(-1.96495212694323,54.6937563833621,12.8141054799532));
#51137=CARTESIAN_POINT('Ctrl Pts',(-1.87744779962502,54.7322103694805,12.5187919464199));
#51138=CARTESIAN_POINT('Ctrl Pts',(-1.81696027218507,54.7515031833634,12.3756296837104));
#51139=CARTESIAN_POINT('Ctrl Pts',(-1.69954010945417,54.7811954145858,12.1689580027143));
#51140=CARTESIAN_POINT('Ctrl Pts',(-1.65407764507147,54.791551087009,12.0994101835497));
#51141=CARTESIAN_POINT('Ctrl Pts',(-1.50902585055616,54.8218798868502,11.9044555190775));
#51142=CARTESIAN_POINT('Ctrl Pts',(-1.3982346508918,54.8418997417864,11.7867995231772));
#51143=CARTESIAN_POINT('Ctrl Pts',(-1.18973149493884,54.8759202504295,11.6110120890975));
#51144=CARTESIAN_POINT('Ctrl Pts',(-1.09843392202422,54.8898832191871,11.5456933353741));
#51145=CARTESIAN_POINT('Ctrl Pts',(-0.959593076632585,54.9100805965764,
11.4626167398557));
#51146=CARTESIAN_POINT('Ctrl Pts',(-0.916028734927509,54.9162844128338,
11.4386436928017));
#51147=CARTESIAN_POINT('Ctrl Pts',(-0.768957068956217,54.9368373000166,
11.3646436217929));
#51148=CARTESIAN_POINT('Ctrl Pts',(-0.661605311957139,54.9512219289493,
11.3215767122849));
#51149=CARTESIAN_POINT('Ctrl Pts',(-0.495999003212708,54.9728560242593,
11.2703959610723));
#51150=CARTESIAN_POINT('Ctrl Pts',(-0.440040968124541,54.9800760518959,
11.2555729359028));
#51151=CARTESIAN_POINT('Ctrl Pts',(-0.326923092939371,54.9945349639386,
11.2306037560387));
#51152=CARTESIAN_POINT('Ctrl Pts',(-0.269763200048498,55.001773849506,11.2204578986548));
#51153=CARTESIAN_POINT('Ctrl Pts',(-0.0970750496432848,55.0235230128508,
11.1971594092239));
#51154=CARTESIAN_POINT('Ctrl Pts',(0.0196137485806436,55.0380596792661,
11.191162174232));
#51155=CARTESIAN_POINT('Ctrl Pts',(0.168443546981575,55.0566436786176,11.1958270484659));
#51156=CARTESIAN_POINT('Ctrl Pts',(0.200602780793859,55.0606618969659,11.1975685142009));
#51157=CARTESIAN_POINT('Ctrl Pts',(0.264575114192646,55.0686690219848,11.2024978272794));
#51158=CARTESIAN_POINT('Ctrl Pts',(0.296397193709932,55.072658933182,11.2056739484811));
#51159=CARTESIAN_POINT('Ctrl Pts',(0.380623964693239,55.0832492211649,11.2160156172632));
#51160=CARTESIAN_POINT('Ctrl Pts',(0.432920832162374,55.0898554904921,11.2244319236168));
#51161=CARTESIAN_POINT('Ctrl Pts',(0.618413676359414,55.1134677494716,11.261540930968));
#51162=CARTESIAN_POINT('Ctrl Pts',(0.749768860398253,55.130524332922,11.3013299973599));
#51163=CARTESIAN_POINT('Ctrl Pts',(0.968347650589545,55.1600202312374,11.3910724311691));
#51164=CARTESIAN_POINT('Ctrl Pts',(1.05774505411059,55.1724345570082,11.4351879672249));
#51165=CARTESIAN_POINT('Ctrl Pts',(1.18549892263016,55.1908918000413,11.5097053571938));
#51166=CARTESIAN_POINT('Ctrl Pts',(1.22638227727023,55.1969157625829,11.5354312678751));
#51167=CARTESIAN_POINT('Ctrl Pts',(1.29171644184769,55.206760855601,11.5796700588564));
#51168=CARTESIAN_POINT('Ctrl Pts',(1.31668857015409,55.2105785964763,11.5973627140674));
#51169=CARTESIAN_POINT('Ctrl Pts',(1.40526456338941,55.2243333496964,11.6629867641403));
#51170=CARTESIAN_POINT('Ctrl Pts',(1.4667630061718,55.2342899411088,11.7140195135995));
#51171=CARTESIAN_POINT('Ctrl Pts',(1.56724222383337,55.2514051041058,11.8073478064762));
#51172=CARTESIAN_POINT('Ctrl Pts',(1.60765111814264,55.2585536663766,11.8479970395813));
#51173=CARTESIAN_POINT('Ctrl Pts',(1.66181615272736,55.2685602592642,11.9070945871655));
#51174=CARTESIAN_POINT('Ctrl Pts',(1.67696921794576,55.271409807239,11.9241720121809));
#51175=CARTESIAN_POINT('Ctrl Pts',(1.71727003150136,55.279131600391,11.9711047855904));
#51176=CARTESIAN_POINT('Ctrl Pts',(1.74188994587628,55.2840060844735,12.0014384181443));
#51177=CARTESIAN_POINT('Ctrl Pts',(1.8065848918423,55.2972694829167,12.0857520585659));
#51178=CARTESIAN_POINT('Ctrl Pts',(1.84511050502288,55.3056915931741,12.1409711044007));
#51179=CARTESIAN_POINT('Ctrl Pts',(1.93595186696758,55.3270212045074,12.2843722563573));
#51180=CARTESIAN_POINT('Ctrl Pts',(1.98486260872712,55.3399222266209,12.3749086425223));
#51181=CARTESIAN_POINT('Ctrl Pts',(2.06981939645706,55.3657345378285,12.5622729693026));
#51182=CARTESIAN_POINT('Ctrl Pts',(2.10587792485611,55.37864579455,12.6590943828494));
#51183=CARTESIAN_POINT('Ctrl Pts',(2.15349014491728,55.3997321409488,12.8212008163602));
#51184=CARTESIAN_POINT('Ctrl Pts',(2.16918594921391,55.4079207826309,12.8851389193291));
#51185=CARTESIAN_POINT('Ctrl Pts',(2.20276718436149,55.4294576717754,13.055456523819));
#51186=CARTESIAN_POINT('Ctrl Pts',(2.21599272358748,55.4428802470817,13.1628683822018));
#51187=CARTESIAN_POINT('Ctrl Pts',(2.22817911102804,55.4751762881486,13.4220030672915));
#51188=CARTESIAN_POINT('Ctrl Pts',(2.2193936360582,55.4940986489574,13.574391865939));
#51189=CARTESIAN_POINT('Ctrl Pts',(2.17101642313604,55.5323481640879,13.8774680825458));
#51190=CARTESIAN_POINT('Ctrl Pts',(2.13104402819563,55.5516774345543,14.0281115650887));
#51191=CARTESIAN_POINT('Ctrl Pts',(2.02727527647819,55.5882953250669,14.3028298501184));
#51192=CARTESIAN_POINT('Ctrl Pts',(1.96664700474721,55.6055699943675,14.4279898314726));
#51193=CARTESIAN_POINT('Ctrl Pts',(1.8678683021456,55.6293181129264,14.5909387234281));
#51194=CARTESIAN_POINT('Ctrl Pts',(1.83951777143476,55.635779799292,14.6342803451875));
#51195=CARTESIAN_POINT('Ctrl Pts',(1.75150366139421,55.6548565937528,14.759004427163));
#51196=CARTESIAN_POINT('Ctrl Pts',(1.6875562492725,55.6675184735274,14.8376445410234));
#51197=CARTESIAN_POINT('Ctrl Pts',(1.54892405178738,55.6929987854296,14.9866582924729));
#51198=CARTESIAN_POINT('Ctrl Pts',(1.47416437906414,55.7058176847556,15.0569660321525));
#51199=CARTESIAN_POINT('Ctrl Pts',(1.37408466664728,55.722016130923,15.1393251494684));
#51200=CARTESIAN_POINT('Ctrl Pts',(1.35287448981891,55.7253990507332,15.1561677880244));
#51201=CARTESIAN_POINT('Ctrl Pts',(1.26256883969667,55.7396021042372,15.2253432039206));
#51202=CARTESIAN_POINT('Ctrl Pts',(1.19071055364304,55.7503933195221,15.2742371749297));
#51203=CARTESIAN_POINT('Ctrl Pts',(1.06865975664079,55.7680903490432,15.3476607002243));
#51204=CARTESIAN_POINT('Ctrl Pts',(1.02004049247093,55.7749885396146,15.3746024109667));
#51205=CARTESIAN_POINT('Ctrl Pts',(0.883799957013692,55.7939812750692,15.4438491266533));
#51206=CARTESIAN_POINT('Ctrl Pts',(0.794172374943345,55.8061191550956,15.4826152506759));
#51207=CARTESIAN_POINT('Ctrl Pts',(0.666120248972946,55.823082662627,15.5284752501652));
#51208=CARTESIAN_POINT('Ctrl Pts',(0.629658995114581,55.8278720505244,15.5405059382731));
#51209=CARTESIAN_POINT('Ctrl Pts',(0.585625974941044,55.833612963806,15.5537945321524));
#51210=CARTESIAN_POINT('Ctrl Pts',(0.578357476081339,55.834559224075,15.5559480889085));
#51211=CARTESIAN_POINT('Ctrl Pts',(0.407324793040697,55.8567938866377,15.6056873667656));
#51212=CARTESIAN_POINT('Ctrl Pts',(0.237401599318956,55.8781731093593,15.6349311711548));
#51213=CARTESIAN_POINT('Ctrl Pts',(-0.103907242058289,55.9208364668511,
15.6562180332499));
#51214=CARTESIAN_POINT('Ctrl Pts',(-0.275242125909403,55.9421181369697,
15.648747758641));
#51215=CARTESIAN_POINT('Ctrl Pts',(-0.603645192470279,55.9836529641875,
15.5989882287064));
#51216=CARTESIAN_POINT('Ctrl Pts',(-0.760968353342703,56.0038954620483,
15.5587124997302));
#51217=CARTESIAN_POINT('Ctrl Pts',(-0.922015525945914,56.0254597460298,
15.4988425221125));
#51218=CARTESIAN_POINT('Ctrl Pts',(-0.931193005698925,56.0266916328361,
15.4953639618438));
#51219=CARTESIAN_POINT('Ctrl Pts',(-1.00552057873781,56.0366939590796,15.466645674492));
#51220=CARTESIAN_POINT('Ctrl Pts',(-1.06963654225242,56.045480904963,15.4384593514847));
#51221=CARTESIAN_POINT('Ctrl Pts',(-1.25098158552824,56.070889733718,15.34893816718));
#51222=CARTESIAN_POINT('Ctrl Pts',(-1.36511778035346,56.0874951412478,15.2801181361817));
#51223=CARTESIAN_POINT('Ctrl Pts',(-1.58345993447679,56.1210626324979,15.1226711204873));
#51224=CARTESIAN_POINT('Ctrl Pts',(-1.68743798665633,56.1380255455942,15.033697291398));
#51225=CARTESIAN_POINT('Ctrl Pts',(-1.87912994352279,56.1719567677729,14.8397418486595));
#51226=CARTESIAN_POINT('Ctrl Pts',(-1.96692908706153,56.1889245573967,14.7348514382924));
#51227=CARTESIAN_POINT('Ctrl Pts',(-2.07860482722401,56.2131959329734,14.5756209362927));
#51228=CARTESIAN_POINT('Ctrl Pts',(-2.11016737775064,56.2204354673342,14.5269723536886));
#51229=CARTESIAN_POINT('Ctrl Pts',(-2.20918486750619,56.2445761630928,14.3612863809782));
#51230=CARTESIAN_POINT('Ctrl Pts',(-2.26868842527496,56.261550098513,14.2391634980653));
#51231=CARTESIAN_POINT('Ctrl Pts',(-2.36017442714328,56.2932809676468,14.00443926774));
#51232=CARTESIAN_POINT('Ctrl Pts',(-2.39475962923237,56.3078402829316,13.8926888555084));
#51233=CARTESIAN_POINT('Ctrl Pts',(-2.44824801252212,56.3370191898033,13.6638749836948));
#51234=CARTESIAN_POINT('Ctrl Pts',(-2.46703334575657,56.3516384295017,13.5467792574595));
#51235=CARTESIAN_POINT('Ctrl Pts',(-2.4879153038017,56.3809581310081,13.3104745764312));
#51236=CARTESIAN_POINT('Ctrl Pts',(-2.48999639793424,56.3956586714332,13.1912644177639));
#51237=CARTESIAN_POINT('Ctrl Pts',(-2.48034706819867,56.4174897145385,13.0157293520969));
#51238=CARTESIAN_POINT('Ctrl Pts',(-2.47529036441297,56.4245455467382,12.9592240236162));
#51239=CARTESIAN_POINT('Ctrl Pts',(-2.46826046448302,56.4316304354619,12.9028993853228));
#51240=CARTESIAN_POINT('Ctrl Pts',(0.286897399705336,52.3546462541016,10.8159730008272));
#51241=CARTESIAN_POINT('Ctrl Pts',(0.378604545572326,52.366273264052,10.8299117351835));
#51242=CARTESIAN_POINT('Ctrl Pts',(0.46941326367117,52.3777703139944,10.8490035483265));
#51243=CARTESIAN_POINT('Ctrl Pts',(0.558740568487378,52.389208221275,10.8730280161214));
#51244=CARTESIAN_POINT('Ctrl Pts',(0.619668574418693,52.3970097427031,10.8894145277184));
#51245=CARTESIAN_POINT('Ctrl Pts',(0.679906668173053,52.4047836614174,10.9080949961699));
#51246=CARTESIAN_POINT('Ctrl Pts',(0.739263037046509,52.4125512777111,10.9289874100517));
#51247=CARTESIAN_POINT('Ctrl Pts',(0.832526775312518,52.4247561505278,10.9618146307359));
#51248=CARTESIAN_POINT('Ctrl Pts',(0.923624974476453,52.4369502239068,11.0001090003664));
#51249=CARTESIAN_POINT('Ctrl Pts',(1.0118830480884,52.4492374792539,11.0435763649142));
#51250=CARTESIAN_POINT('Ctrl Pts',(1.10141442806073,52.4617020038269,11.087670836643));
#51251=CARTESIAN_POINT('Ctrl Pts',(1.1880363424801,52.4742672637596,11.1370966569693));
#51252=CARTESIAN_POINT('Ctrl Pts',(1.2712048670289,52.4868467571487,11.19139013783));
#51253=CARTESIAN_POINT('Ctrl Pts',(1.31745190903785,52.4938417635213,11.2215808007496));
#51254=CARTESIAN_POINT('Ctrl Pts',(1.36263174845131,52.5008412749167,11.2532772805539));
#51255=CARTESIAN_POINT('Ctrl Pts',(1.40665451137732,52.5078312137426,11.2864057567896));
#51256=CARTESIAN_POINT('Ctrl Pts',(1.48277798855463,52.5199181072795,11.3436910028085));
#51257=CARTESIAN_POINT('Ctrl Pts',(1.55543851145377,52.531973226489,11.4052548403952));
#51258=CARTESIAN_POINT('Ctrl Pts',(1.62411723972848,52.5439090053706,11.4706603829727));
#51259=CARTESIAN_POINT('Ctrl Pts',(1.65458644294996,52.5492042937588,11.4996774428204));
#51260=CARTESIAN_POINT('Ctrl Pts',(1.68427259471252,52.5544761708037,11.5294507960024));
#51261=CARTESIAN_POINT('Ctrl Pts',(1.71313348876987,52.5597173654126,11.5599433789351));
#51262=CARTESIAN_POINT('Ctrl Pts',(1.7131342012995,52.5597174948094,11.5599441317485));
#51263=CARTESIAN_POINT('Ctrl Pts',(1.71313491382864,52.5597176242061,11.5599448845624));
#51264=CARTESIAN_POINT('Ctrl Pts',(1.71313562635727,52.5597177536029,11.5599456373767));
#51265=CARTESIAN_POINT('Ctrl Pts',(1.77093737997985,52.5702146764983,11.6210154470465));
#51266=CARTESIAN_POINT('Ctrl Pts',(1.82547359849269,52.5805903254852,11.6850091277299));
#51267=CARTESIAN_POINT('Ctrl Pts',(1.87646608175138,52.5909392249462,11.7515532965285));
#51268=CARTESIAN_POINT('Ctrl Pts',(1.91162048389922,52.5980737936157,11.7974290868616));
#51269=CARTESIAN_POINT('Ctrl Pts',(1.94509008894011,52.6051955239253,11.8445161270279));
#51270=CARTESIAN_POINT('Ctrl Pts',(1.97677937323057,52.6123336839022,11.8926783920446));
#51271=CARTESIAN_POINT('Ctrl Pts',(1.98769496610871,52.6147924724155,11.9092682169265));
#51272=CARTESIAN_POINT('Ctrl Pts',(1.99839982660474,52.617253371613,11.9259864059183));
#51273=CARTESIAN_POINT('Ctrl Pts',(2.00889043434765,52.6197176754979,11.9428279934674));
#51274=CARTESIAN_POINT('Ctrl Pts',(2.06611700706165,52.6331605254181,12.034699347169));
#51275=CARTESIAN_POINT('Ctrl Pts',(2.11697020498068,52.6467081567378,12.1302489683145));
#51276=CARTESIAN_POINT('Ctrl Pts',(2.1612007237327,52.6602925392306,12.228530179788));
#51277=CARTESIAN_POINT('Ctrl Pts',(2.17484117486492,52.6644818888196,12.2588395702302));
#51278=CARTESIAN_POINT('Ctrl Pts',(2.18785176832704,52.6686747752264,12.2894091277353));
#51279=CARTESIAN_POINT('Ctrl Pts',(2.2002251301063,52.6728693150193,12.3202120767204));
#51280=CARTESIAN_POINT('Ctrl Pts',(2.25218578100817,52.6904838503222,12.4495658697733));
#51281=CARTESIAN_POINT('Ctrl Pts',(2.29312496909258,52.7079624405621,12.5829731053493));
#51282=CARTESIAN_POINT('Ctrl Pts',(2.32233770635006,52.7252560733271,12.718421779341));
#51283=CARTESIAN_POINT('Ctrl Pts',(2.33286794707285,52.7314898649223,12.7672466166078));
#51284=CARTESIAN_POINT('Ctrl Pts',(2.34184912297622,52.7377170578108,12.8163384484872));
#51285=CARTESIAN_POINT('Ctrl Pts',(2.3492445571228,52.7439361194972,12.8655905848478));
#51286=CARTESIAN_POINT('Ctrl Pts',(2.35424968762134,52.7481450969152,12.898923769206));
#51287=CARTESIAN_POINT('Ctrl Pts',(2.358528548211,52.7523503502017,12.9323303676679));
#51288=CARTESIAN_POINT('Ctrl Pts',(2.36207060378534,52.7565514078527,12.9657772649005));
#51289=CARTESIAN_POINT('Ctrl Pts',(2.3629356126977,52.7575773523172,12.9739453649175));
#51290=CARTESIAN_POINT('Ctrl Pts',(2.36375668195591,52.7586030458296,12.9821158624631));
#51291=CARTESIAN_POINT('Ctrl Pts',(2.36453366611607,52.7596284837788,12.9902882932491));
#51292=CARTESIAN_POINT('Ctrl Pts',(2.37188172323651,52.7693262060883,13.067576211469));
#51293=CARTESIAN_POINT('Ctrl Pts',(2.3752920055037,52.7790097070089,13.1451059550479));
#51294=CARTESIAN_POINT('Ctrl Pts',(2.37487726394704,52.7886735986088,13.2224778137936));
#51295=CARTESIAN_POINT('Ctrl Pts',(2.37413425718948,52.8059863965374,13.3610889873552));
#51296=CARTESIAN_POINT('Ctrl Pts',(2.36112302584554,52.8232395554245,13.4992196296424));
#51297=CARTESIAN_POINT('Ctrl Pts',(2.33650449061312,52.8404407532392,13.6348826289493));
#51298=CARTESIAN_POINT('Ctrl Pts',(2.30880269869488,52.8597962509611,13.787536234955));
#51299=CARTESIAN_POINT('Ctrl Pts',(2.26639959314252,52.879086427903,13.9370694808791));
#51300=CARTESIAN_POINT('Ctrl Pts',(2.21021589336869,52.8983129681719,14.080571485906));
#51301=CARTESIAN_POINT('Ctrl Pts',(2.17849703195257,52.9091674325228,14.1615864462719));
#51302=CARTESIAN_POINT('Ctrl Pts',(2.1423853790687,52.9200015916103,14.2406785161887));
#51303=CARTESIAN_POINT('Ctrl Pts',(2.10205519678664,52.930813691901,14.317308941313));
#51304=CARTESIAN_POINT('Ctrl Pts',(2.07500136436392,52.9380665415746,14.3687132881939));
#51305=CARTESIAN_POINT('Ctrl Pts',(2.04604966208516,52.9453094014196,14.4190095405316));
#51306=CARTESIAN_POINT('Ctrl Pts',(2.01525326350672,52.9525419488395,14.4680373158271));
#51307=CARTESIAN_POINT('Ctrl Pts',(2.01218499602166,52.9532625327748,14.4729219885728));
#51308=CARTESIAN_POINT('Ctrl Pts',(2.0090983916613,52.9539830205944,14.4777941129881));
#51309=CARTESIAN_POINT('Ctrl Pts',(2.00599346816136,52.9547034198318,14.4826535828735));
#51310=CARTESIAN_POINT('Ctrl Pts',(1.98586676221557,52.9593731850012,14.514153592918));
#51311=CARTESIAN_POINT('Ctrl Pts',(1.96496839544559,52.9640396745915,14.5451249036443));
#51312=CARTESIAN_POINT('Ctrl Pts',(1.94333277185748,52.9687031081194,14.5755436631792));
#51313=CARTESIAN_POINT('Ctrl Pts',(1.87430998326427,52.9835805709854,14.6725867458569));
#51314=CARTESIAN_POINT('Ctrl Pts',(1.79779191505982,52.9984243439752,14.7639865514538));
#51315=CARTESIAN_POINT('Ctrl Pts',(1.71500292316759,53.0132242563846,14.8488720449154));
#51316=CARTESIAN_POINT('Ctrl Pts',(1.64583799177366,53.0255886408642,14.9197884698823));
#51317=CARTESIAN_POINT('Ctrl Pts',(1.57230333098493,53.0379215660797,14.9861549462414));
#51318=CARTESIAN_POINT('Ctrl Pts',(1.49509560112678,53.0502225028627,15.0475082024516));
#51319=CARTESIAN_POINT('Ctrl Pts',(1.41657636869863,53.0627323916538,15.1099036464497));
#51320=CARTESIAN_POINT('Ctrl Pts',(1.33425890477864,53.0752091530701,15.1671144271994));
#51321=CARTESIAN_POINT('Ctrl Pts',(1.24886044937028,53.0876542281749,15.2186643420193));
#51322=CARTESIAN_POINT('Ctrl Pts',(1.15388791611956,53.1014945289572,15.275993552201));
#51323=CARTESIAN_POINT('Ctrl Pts',(1.05510126433165,53.1152963125072,15.3263271268123));
#51324=CARTESIAN_POINT('Ctrl Pts',(0.953422201694293,53.1290688673279,15.3690181733183));
#51325=CARTESIAN_POINT('Ctrl Pts',(0.913600253053039,53.1344627995348,15.3857378461527));
#51326=CARTESIAN_POINT('Ctrl Pts',(0.873335769951871,53.1398520704015,15.4012842727042));
#51327=CARTESIAN_POINT('Ctrl Pts',(0.832685060509524,53.1452370532317,15.4156166726461));
#51328=CARTESIAN_POINT('Ctrl Pts',(0.791075003150014,53.1507491204876,15.4302873141149));
#51329=CARTESIAN_POINT('Ctrl Pts',(0.749052457409756,53.1562577204812,15.4436884918247));
#51330=CARTESIAN_POINT('Ctrl Pts',(0.706698280387312,53.161762047546,15.4558206545638));
#51331=CARTESIAN_POINT('Ctrl Pts',(0.608132708228648,53.1745715786153,15.4840543175924));
#51332=CARTESIAN_POINT('Ctrl Pts',(0.507777250054708,53.1873570674503,15.505409762825));
#51333=CARTESIAN_POINT('Ctrl Pts',(0.406676257051895,53.2001067683875,15.5199270150308));
#51334=CARTESIAN_POINT('Ctrl Pts',(0.335339323040758,53.2091029666186,15.5301703987195));
#51335=CARTESIAN_POINT('Ctrl Pts',(0.263638041361633,53.2180805540776,15.5370104696948));
#51336=CARTESIAN_POINT('Ctrl Pts',(0.191906243718386,53.2270396901202,15.5404768058473));
#51337=CARTESIAN_POINT('Ctrl Pts',(0.106801154506927,53.2376691194279,15.5445893871179));
#51338=CARTESIAN_POINT('Ctrl Pts',(0.0216491506267357,53.2482730711808,
15.5439538001737));
#51339=CARTESIAN_POINT('Ctrl Pts',(-0.0630107385862956,53.2588537959295,
15.5386149146513));
#51340=CARTESIAN_POINT('Ctrl Pts',(-0.114508583652721,53.2652899551174,
15.5353673188653));
#51341=CARTESIAN_POINT('Ctrl Pts',(-0.165824675143732,53.2717175497265,
15.5303795993431));
#51342=CARTESIAN_POINT('Ctrl Pts',(-0.216852813418056,53.278138981017,15.5236574306784));
#51343=CARTESIAN_POINT('Ctrl Pts',(-0.287558469935319,53.2870366506269,
15.5143430530678));
#51344=CARTESIAN_POINT('Ctrl Pts',(-0.357702850727178,53.2959214332314,
15.5016988676326));
#51345=CARTESIAN_POINT('Ctrl Pts',(-0.426950888544439,53.3047932471048,
15.4857425202606));
#51346=CARTESIAN_POINT('Ctrl Pts',(-0.471181986881598,53.3104599791052,
15.4755506535744));
#51347=CARTESIAN_POINT('Ctrl Pts',(-0.515047377913757,53.3161214201456,
15.4640074957561));
#51348=CARTESIAN_POINT('Ctrl Pts',(-0.558459593907759,53.3217775493788,
15.4511177477559));
#51349=CARTESIAN_POINT('Ctrl Pts',(-0.583013376677091,53.3249766343673,
15.4438273557522));
#51350=CARTESIAN_POINT('Ctrl Pts',(-0.607420694881155,53.3281738270904,
15.4361066036092));
#51351=CARTESIAN_POINT('Ctrl Pts',(-0.63166339466273,53.3313688080905,15.4279574015993));
#51352=CARTESIAN_POINT('Ctrl Pts',(-0.666425076872119,53.33595010123,15.4162722356285));
#51353=CARTESIAN_POINT('Ctrl Pts',(-0.700865438636589,53.3405291103146,
15.4037002662725));
#51354=CARTESIAN_POINT('Ctrl Pts',(-0.734940871487638,53.3451046241908,
15.3902736918485));
#51355=CARTESIAN_POINT('Ctrl Pts',(-0.815017811682377,53.3558570378908,
15.3587213708003));
#51356=CARTESIAN_POINT('Ctrl Pts',(-0.893067261237862,53.3665885123108,
15.3224546218366));
#51357=CARTESIAN_POINT('Ctrl Pts',(-0.968688727694473,53.3772595662987,
15.281965743812));
#51358=CARTESIAN_POINT('Ctrl Pts',(-1.00974331905814,53.3830528387837,15.2599844940432));
#51359=CARTESIAN_POINT('Ctrl Pts',(-1.05008317632462,53.3888284125057,15.2367586482058));
#51360=CARTESIAN_POINT('Ctrl Pts',(-1.08965021009618,53.3945807528981,15.2123647107976));
#51361=CARTESIAN_POINT('Ctrl Pts',(-1.15120498421712,53.4035297182302,15.1744148529499));
#51362=CARTESIAN_POINT('Ctrl Pts',(-1.21082688378749,53.4124647514594,15.1335317623874));
#51363=CARTESIAN_POINT('Ctrl Pts',(-1.26819795552164,53.421416990598,15.0898744137285));
#51364=CARTESIAN_POINT('Ctrl Pts',(-1.34233226310685,53.4329849817443,15.0334608377572));
#51365=CARTESIAN_POINT('Ctrl Pts',(-1.41271035693283,53.4445822067216,14.9724115105954));
#51366=CARTESIAN_POINT('Ctrl Pts',(-1.47880049445705,53.4561712566132,14.907331404647));
#51367=CARTESIAN_POINT('Ctrl Pts',(-1.50721428041528,53.4611536760092,14.8793518562632));
#51368=CARTESIAN_POINT('Ctrl Pts',(-1.53483606346469,53.4661346659615,14.8506269439165));
#51369=CARTESIAN_POINT('Ctrl Pts',(-1.56162593402063,53.4711116247684,14.8212029673402));
#51370=CARTESIAN_POINT('Ctrl Pts',(-1.57469113672623,53.4735388472342,14.8068531324811));
#51371=CARTESIAN_POINT('Ctrl Pts',(-1.58755822840402,53.4759650578836,14.7923373233404));
#51372=CARTESIAN_POINT('Ctrl Pts',(-1.60022243656977,53.478389924412,14.7776611398467));
#51373=CARTESIAN_POINT('Ctrl Pts',(-1.63324791992227,53.4847134456395,14.7393888651568));
#51374=CARTESIAN_POINT('Ctrl Pts',(-1.66489365639477,53.4910279397085,14.7000259269526));
#51375=CARTESIAN_POINT('Ctrl Pts',(-1.69510025535646,53.4973261597594,14.6596621725213));
#51376=CARTESIAN_POINT('Ctrl Pts',(-1.72025473141081,53.5025709880718,14.626049348529));
#51377=CARTESIAN_POINT('Ctrl Pts',(-1.74441120426201,53.5078044085106,14.5917424672605));
#51378=CARTESIAN_POINT('Ctrl Pts',(-1.76752626686844,53.5130197475694,14.5568082706509));
#51379=CARTESIAN_POINT('Ctrl Pts',(-1.76753172518083,53.5130209791019,14.5568000214083));
#51380=CARTESIAN_POINT('Ctrl Pts',(-1.76753718343626,53.5130222106335,14.5567917721293));
#51381=CARTESIAN_POINT('Ctrl Pts',(-1.76754264163471,53.5130234421644,14.5567835228138));
#51382=CARTESIAN_POINT('Ctrl Pts',(-1.79994554156808,53.5203344938398,14.5078110007303));
#51383=CARTESIAN_POINT('Ctrl Pts',(-1.83034051010383,53.527617509957,14.4575510638308));
#51384=CARTESIAN_POINT('Ctrl Pts',(-1.8585993480451,53.5348876682701,14.4061925809449));
#51385=CARTESIAN_POINT('Ctrl Pts',(-1.88277887985237,53.5411083424727,14.3622479547331));
#51386=CARTESIAN_POINT('Ctrl Pts',(-1.90539461130247,53.5473201288166,14.3174991724067));
#51387=CARTESIAN_POINT('Ctrl Pts',(-1.92647365191702,53.5535208525157,14.2720316941406));
#51388=CARTESIAN_POINT('Ctrl Pts',(-1.94753705207156,53.5597169753331,14.2265979523375));
#51389=CARTESIAN_POINT('Ctrl Pts',(-1.96706590250326,53.5659011887381,14.1804465192646));
#51390=CARTESIAN_POINT('Ctrl Pts',(-1.98486750734344,53.5720962182315,14.1337424961699));
#51391=CARTESIAN_POINT('Ctrl Pts',(-2.01310453648316,53.5819228170071,14.0596602506135));
#51392=CARTESIAN_POINT('Ctrl Pts',(-2.03699332425505,53.5917802249531,13.9841826632899));
#51393=CARTESIAN_POINT('Ctrl Pts',(-2.05656808333809,53.6016504734671,13.9077925559741));
#51394=CARTESIAN_POINT('Ctrl Pts',(-2.06538702068936,53.606097276767,13.8733768286685));
#51395=CARTESIAN_POINT('Ctrl Pts',(-2.07333014721432,53.6105467503804,13.8387751935792));
#51396=CARTESIAN_POINT('Ctrl Pts',(-2.08039942415651,53.6149975654674,13.8040285817165));
#51397=CARTESIAN_POINT('Ctrl Pts',(-2.09572783431339,53.6246483288685,13.7286870266254));
#51398=CARTESIAN_POINT('Ctrl Pts',(-2.10695004179422,53.6343045627027,13.6526660854498));
#51399=CARTESIAN_POINT('Ctrl Pts',(-2.11410726864506,53.6439395872891,13.5764221390983));
#51400=CARTESIAN_POINT('Ctrl Pts',(-2.11770578382013,53.6487838912226,13.5380881581207));
#51401=CARTESIAN_POINT('Ctrl Pts',(-2.12027678461537,53.6536229360829,13.4996969874888));
#51402=CARTESIAN_POINT('Ctrl Pts',(-2.12182529008515,53.6584539546973,13.4613016906794));
#51403=CARTESIAN_POINT('Ctrl Pts',(-2.12479825068366,53.6677289803731,13.3875869335736));
#51404=CARTESIAN_POINT('Ctrl Pts',(-2.12400355021684,53.6769730620142,13.3138636726511));
#51405=CARTESIAN_POINT('Ctrl Pts',(-2.11948894684724,53.6861613022635,13.2405350020391));
#51406=CARTESIAN_POINT('Ctrl Pts',(-2.11867825173027,53.6878112504193,13.2273672461296));
#51407=CARTESIAN_POINT('Ctrl Pts',(-2.11774762931345,53.6894594143941,13.2142120817822));
#51408=CARTESIAN_POINT('Ctrl Pts',(-2.11669738116017,53.6911056716687,13.201071667521));
#51409=CARTESIAN_POINT('Ctrl Pts',(-2.11669666944272,53.6911067872812,13.2010627627093));
#51410=CARTESIAN_POINT('Ctrl Pts',(-2.11669595767028,53.691107902893,13.201053857904));
#51411=CARTESIAN_POINT('Ctrl Pts',(-2.11669524584283,53.6911090185039,13.201044953105));
#51412=CARTESIAN_POINT('Ctrl Pts',(-2.11084161280211,53.7002831194977,13.1278173393418));
#51413=CARTESIAN_POINT('Ctrl Pts',(-2.10126801495813,53.7094026193869,13.0550147556555));
#51414=CARTESIAN_POINT('Ctrl Pts',(-2.08801392842047,53.7184963324333,12.9829836038374));
#51415=CARTESIAN_POINT('Ctrl Pts',(-2.07475984188281,53.7275900454798,12.9109524520193));
#51416=CARTESIAN_POINT('Ctrl Pts',(-2.05782432908718,53.7366579745326,12.8396929553331));
#51417=CARTESIAN_POINT('Ctrl Pts',(-2.03726016858693,53.7457218987084,12.769606170018));
#51418=CARTESIAN_POINT('Ctrl Pts',(-2.02874434142801,53.7494753615187,12.7405825223052));
#51419=CARTESIAN_POINT('Ctrl Pts',(-2.01960546756002,53.7532284872154,12.7117575053214));
#51420=CARTESIAN_POINT('Ctrl Pts',(-2.00984647418317,53.7569830676624,12.6831574839871));
#51421=CARTESIAN_POINT('Ctrl Pts',(-1.97716131346694,53.7695580393416,12.5873692958306));
#51422=CARTESIAN_POINT('Ctrl Pts',(-1.93752131365257,53.7821490605221,12.494099342539));
#51423=CARTESIAN_POINT('Ctrl Pts',(-1.89151142633677,53.7947329481063,12.404322229798));
#51424=CARTESIAN_POINT('Ctrl Pts',(-1.87157864015484,53.8001846445826,12.3654282420772));
#51425=CARTESIAN_POINT('Ctrl Pts',(-1.85045034272277,53.8056350850442,12.3271891462092));
#51426=CARTESIAN_POINT('Ctrl Pts',(-1.82817385043466,53.8110827658278,12.2896811929973));
#51427=CARTESIAN_POINT('Ctrl Pts',(-1.77544770939433,53.8239768598184,12.2009037676465));
#51428=CARTESIAN_POINT('Ctrl Pts',(-1.71629124316072,53.8368545379083,12.1162262276396));
#51429=CARTESIAN_POINT('Ctrl Pts',(-1.65131768918288,53.8497001526603,12.0367107283857));
#51430=CARTESIAN_POINT('Ctrl Pts',(-1.62547657818727,53.8548090767732,12.0050860331629));
#51431=CARTESIAN_POINT('Ctrl Pts',(-1.59871560076123,53.8599129587562,11.974277362838));
#51432=CARTESIAN_POINT('Ctrl Pts',(-1.57107423804931,53.8650109319293,11.9443494144863));
#51433=CARTESIAN_POINT('Ctrl Pts',(-1.57107126173674,53.8650114808588,11.9443461919633));
#51434=CARTESIAN_POINT('Ctrl Pts',(-1.57106828541389,53.8650120297884,11.9443429694505));
#51435=CARTESIAN_POINT('Ctrl Pts',(-1.57106530908085,53.8650125787178,11.944339746948));
#51436=CARTESIAN_POINT('Ctrl Pts',(-1.56919139572923,53.8653581872944,11.9423108441458));
#51437=CARTESIAN_POINT('Ctrl Pts',(-1.56731342907328,53.8657037692991,11.9402860230933));
#51438=CARTESIAN_POINT('Ctrl Pts',(-1.56543142240293,53.8660493257425,11.9382653056425));
#51439=CARTESIAN_POINT('Ctrl Pts',(-1.514776842156,53.8753500454827,11.8838772974168));
#51440=CARTESIAN_POINT('Ctrl Pts',(-1.46119442488989,53.8846325486842,11.8324655478395));
#51441=CARTESIAN_POINT('Ctrl Pts',(-1.4051361512904,53.8938900984857,11.7841100430016));
#51442=CARTESIAN_POINT('Ctrl Pts',(-1.36898430674358,53.8998602698773,11.7529256953286));
#51443=CARTESIAN_POINT('Ctrl Pts',(-1.33180186061339,53.9058201818434,11.7230118660596));
#51444=CARTESIAN_POINT('Ctrl Pts',(-1.29369935058448,53.9117693222334,11.6943859268918));
#51445=CARTESIAN_POINT('Ctrl Pts',(-1.21962533799752,53.923334877883,11.6387350478125));
#51446=CARTESIAN_POINT('Ctrl Pts',(-1.14201854121693,53.9348676699908,11.5880125932902));
#51447=CARTESIAN_POINT('Ctrl Pts',(-1.06155834882649,53.9463802354961,11.5426610760724));
#51448=CARTESIAN_POINT('Ctrl Pts',(-1.03502675166717,53.9501764823255,11.5277064985398));
#51449=CARTESIAN_POINT('Ctrl Pts',(-1.00818516350613,53.953970483159,11.5133362450871));
#51450=CARTESIAN_POINT('Ctrl Pts',(-0.98105881327435,53.9577625495424,11.4995670617175));
#51451=CARTESIAN_POINT('Ctrl Pts',(-0.899330135635023,53.9691876239953,
11.4580820429312));
#51452=CARTESIAN_POINT('Ctrl Pts',(-0.815015032667117,53.9805951916943,
11.422055145314));
#51453=CARTESIAN_POINT('Ctrl Pts',(-0.728915015204727,53.9919791178223,
11.3918916048773));
#51454=CARTESIAN_POINT('Ctrl Pts',(-0.666116891336237,54.0002821266273,
11.3698914496568));
#51455=CARTESIAN_POINT('Ctrl Pts',(-0.602366337967937,54.0085729746407,
11.3510094364104));
#51456=CARTESIAN_POINT('Ctrl Pts',(-0.537994295480503,54.0168471244047,
11.3353972583123));
#51457=CARTESIAN_POINT('Ctrl Pts',(-0.537978733718646,54.0168491246574,
11.3353934841118));
#51458=CARTESIAN_POINT('Ctrl Pts',(-0.537963171919938,54.0168511249091,
11.3353897100994));
#51459=CARTESIAN_POINT('Ctrl Pts',(-0.537947610084269,54.0168531251599,
11.3353859362753));
#51460=CARTESIAN_POINT('Ctrl Pts',(-0.418471797387094,54.0322100276408,
11.3064124448631));
#51461=CARTESIAN_POINT('Ctrl Pts',(-0.296820149650447,54.0475135210664,
11.2885263070439));
#51462=CARTESIAN_POINT('Ctrl Pts',(-0.174817987250954,54.0627784164899,
11.2814679421645));
#51463=CARTESIAN_POINT('Ctrl Pts',(-0.12956541297104,54.0684404129697,11.2788498805275));
#51464=CARTESIAN_POINT('Ctrl Pts',(-0.0842647042719535,54.0740970713534,
11.2777220117312));
#51465=CARTESIAN_POINT('Ctrl Pts',(-0.0390095089471808,54.0797490490657,
11.2780728087121));
#51466=CARTESIAN_POINT('Ctrl Pts',(0.0320295530716223,54.0886212060049,
11.2786234700958));
#51467=CARTESIAN_POINT('Ctrl Pts',(0.103004028875918,54.097489027784,11.2830798353659));
#51468=CARTESIAN_POINT('Ctrl Pts',(0.173464121690939,54.1063436422542,11.291277655428));
#51469=CARTESIAN_POINT('Ctrl Pts',(0.244046248390177,54.1152135925401,11.2994896737657));
#51470=CARTESIAN_POINT('Ctrl Pts',(0.314112023364961,54.1240702865772,11.3114552314023));
#51471=CARTESIAN_POINT('Ctrl Pts',(0.383259896863854,54.1329111150333,11.3269979817466));
#51472=CARTESIAN_POINT('Ctrl Pts',(0.427669540820878,54.1385890632355,11.3369801832804));
#51473=CARTESIAN_POINT('Ctrl Pts',(0.471701620791059,54.1442605950328,11.3484376963137));
#51474=CARTESIAN_POINT('Ctrl Pts',(0.51526103274021,54.14992639429,11.3613239412686));
#51475=CARTESIAN_POINT('Ctrl Pts',(0.556277498627599,54.1552614310033,11.3734579027468));
#51476=CARTESIAN_POINT('Ctrl Pts',(0.596880229991585,54.1605918796447,11.3868250567179));
#51477=CARTESIAN_POINT('Ctrl Pts',(0.636970441946457,54.165916285565,11.401479821767));
#51478=CARTESIAN_POINT('Ctrl Pts',(0.636982682653804,54.165917911261,11.4014842962929));
#51479=CARTESIAN_POINT('Ctrl Pts',(0.636994923314774,54.1659195369565,11.4014887709393));
#51480=CARTESIAN_POINT('Ctrl Pts',(0.637007163929467,54.1659211626517,11.4014932457064));
#51481=CARTESIAN_POINT('Ctrl Pts',(0.738398353557972,54.1793870852429,11.4385585372037));
#51482=CARTESIAN_POINT('Ctrl Pts',(0.83660966707235,54.1928275875312,11.4838997993307));
#51483=CARTESIAN_POINT('Ctrl Pts',(0.930414541120341,54.2062363306581,11.5366246031919));
#51484=CARTESIAN_POINT('Ctrl Pts',(1.03306360519614,54.2209092881817,11.594320451354));
#51485=CARTESIAN_POINT('Ctrl Pts',(1.13043985693448,54.2355445307112,11.6608551719195));
#51486=CARTESIAN_POINT('Ctrl Pts',(1.22101709910568,54.2501438905498,11.7350820030085));
#51487=CARTESIAN_POINT('Ctrl Pts',(1.28576061236064,54.2605793357518,11.7881384408873));
#51488=CARTESIAN_POINT('Ctrl Pts',(1.34703310260344,54.2709968101427,11.8451265234236));
#51489=CARTESIAN_POINT('Ctrl Pts',(1.40428453585257,54.2813987634094,11.9056414349209));
#51490=CARTESIAN_POINT('Ctrl Pts',(1.44154360268005,54.2881683244475,11.9450243639338));
#51491=CARTESIAN_POINT('Ctrl Pts',(1.47710198632334,54.2949318149268,11.9859043278642));
#51492=CARTESIAN_POINT('Ctrl Pts',(1.51079846717546,54.3016883029445,12.0281608435957));
#51493=CARTESIAN_POINT('Ctrl Pts',(1.52887923112574,54.3053136804882,12.0508347272472));
#51494=CARTESIAN_POINT('Ctrl Pts',(1.54642332042148,54.3089369194602,12.0739041582257));
#51495=CARTESIAN_POINT('Ctrl Pts',(1.56340511917397,54.3125576318131,12.0973485954084));
#51496=CARTESIAN_POINT('Ctrl Pts',(1.56341365864612,54.3125594525255,12.0973603846847));
#51497=CARTESIAN_POINT('Ctrl Pts',(1.56342219797969,54.3125612732381,12.0973721740608));
#51498=CARTESIAN_POINT('Ctrl Pts',(1.56343073717471,54.3125630939508,12.0973839635368));
#51499=CARTESIAN_POINT('Ctrl Pts',(1.60414875847956,54.3212449215193,12.1536005193228));
#51500=CARTESIAN_POINT('Ctrl Pts',(1.64171168012391,54.3299293102567,12.2120857444096));
#51501=CARTESIAN_POINT('Ctrl Pts',(1.67607898341393,54.3386175999711,12.2723487961211));
#51502=CARTESIAN_POINT('Ctrl Pts',(1.6971750047835,54.3439508186974,12.3093406606258));
#51503=CARTESIAN_POINT('Ctrl Pts',(1.71706799479513,54.3492856053713,12.347002490196));
#51504=CARTESIAN_POINT('Ctrl Pts',(1.73575785935933,54.3546231997247,12.3852233581526));
#51505=CARTESIAN_POINT('Ctrl Pts',(1.76142165479252,54.3619524625515,12.4377059501558));
#51506=CARTESIAN_POINT('Ctrl Pts',(1.78490977422095,54.3693010491427,12.4911998775491));
#51507=CARTESIAN_POINT('Ctrl Pts',(1.80606354150889,54.3766506970259,12.54555450817));
#51508=CARTESIAN_POINT('Ctrl Pts',(1.82704768297592,54.3839414102503,12.599473285039));
#51509=CARTESIAN_POINT('Ctrl Pts',(1.84573402483613,54.3912331563084,12.6542391567784));
#51510=CARTESIAN_POINT('Ctrl Pts',(1.86195192454017,54.3985016771668,12.7096572714523));
#51511=CARTESIAN_POINT('Ctrl Pts',(1.88236246291403,54.407649250318,12.7794020335238));
#51512=CARTESIAN_POINT('Ctrl Pts',(1.89886396325648,54.4167604367007,12.8501851518565));
#51513=CARTESIAN_POINT('Ctrl Pts',(1.91126977912049,54.4258110530799,12.921567490084));
#51514=CARTESIAN_POINT('Ctrl Pts',(1.92317449250243,54.434496092025,12.990066513965));
#51515=CARTESIAN_POINT('Ctrl Pts',(1.93130616693919,54.44312573541,13.0591253496143));
#51516=CARTESIAN_POINT('Ctrl Pts',(1.93572931569931,54.4517206464745,13.1283203272785));
#51517=CARTESIAN_POINT('Ctrl Pts',(1.9386919849011,54.4574776037202,13.1746678141848));
#51518=CARTESIAN_POINT('Ctrl Pts',(1.9399909490566,54.4632191137398,13.2210774921035));
#51519=CARTESIAN_POINT('Ctrl Pts',(1.93964393421203,54.4689530231657,13.2674349060169));
#51520=CARTESIAN_POINT('Ctrl Pts',(1.93913709339929,54.4773278214175,13.3351433332291));
#51521=CARTESIAN_POINT('Ctrl Pts',(1.93512117200686,54.4856868461961,13.4027379628502));
#51522=CARTESIAN_POINT('Ctrl Pts',(1.92766189460317,54.4940511799848,13.4698207365016));
#51523=CARTESIAN_POINT('Ctrl Pts',(1.9226554375866,54.49966508537,13.5148448058131));
#51524=CARTESIAN_POINT('Ctrl Pts',(1.91609819964657,54.5052815165365,13.5596393322053));
#51525=CARTESIAN_POINT('Ctrl Pts',(1.90801160717522,54.510908482447,13.6040969579081));
#51526=CARTESIAN_POINT('Ctrl Pts',(1.89950815886185,54.5168255128836,13.6508463302349));
#51527=CARTESIAN_POINT('Ctrl Pts',(1.88931363287462,54.5227535003215,13.6972182478163));
#51528=CARTESIAN_POINT('Ctrl Pts',(1.87745482154452,54.5286995303713,13.7430796443201));
#51529=CARTESIAN_POINT('Ctrl Pts',(1.87745390524781,54.5286999898042,13.7430831879001));
#51530=CARTESIAN_POINT('Ctrl Pts',(1.87745298894106,54.5287004492373,13.7430867314775));
#51531=CARTESIAN_POINT('Ctrl Pts',(1.87745207262426,54.5287009086705,13.7430902750522));
#51532=CARTESIAN_POINT('Ctrl Pts',(1.8628892767985,54.5360025666133,13.7994074304433));
#51533=CARTESIAN_POINT('Ctrl Pts',(1.84578665227882,54.543345664524,13.8550660333931));
#51534=CARTESIAN_POINT('Ctrl Pts',(1.82617215597624,54.5506964228564,13.9098241588855));
#51535=CARTESIAN_POINT('Ctrl Pts',(1.81753531532175,54.553933178337,13.9339357749638));
#51536=CARTESIAN_POINT('Ctrl Pts',(1.80841181690004,54.5571713405063,13.9578722294145));
#51537=CARTESIAN_POINT('Ctrl Pts',(1.79880597984343,54.5604076548173,13.9816103365177));
#51538=CARTESIAN_POINT('Ctrl Pts',(1.76115590409911,54.5730923878837,14.0746518408859));
#51539=CARTESIAN_POINT('Ctrl Pts',(1.71607964918136,54.5857501826966,14.1646657427447));
#51540=CARTESIAN_POINT('Ctrl Pts',(1.66435797001852,54.598350653071,14.2506283426667));
#51541=CARTESIAN_POINT('Ctrl Pts',(1.61168717432495,54.6111823478549,14.3381683957173));
#51542=CARTESIAN_POINT('Ctrl Pts',(1.55212566300802,54.6239543178497,14.4215061875728));
#51543=CARTESIAN_POINT('Ctrl Pts',(1.48654463182221,54.6366428235215,14.4995805360594));
#51544=CARTESIAN_POINT('Ctrl Pts',(1.42169839649399,54.6491891621484,14.5767801086113));
#51545=CARTESIAN_POINT('Ctrl Pts',(1.35096774966186,54.6616535771729,14.6488328300364));
#51546=CARTESIAN_POINT('Ctrl Pts',(1.27522614131539,54.6740255661475,14.7147439947356));
#51547=CARTESIAN_POINT('Ctrl Pts',(1.235482709428,54.6805174444143,14.7493291579244));
#51548=CARTESIAN_POINT('Ctrl Pts',(1.19436001237438,54.6869841095851,14.7822239216797));
#51549=CARTESIAN_POINT('Ctrl Pts',(1.15198645237769,54.6934259532847,14.8132889771581));
#51550=CARTESIAN_POINT('Ctrl Pts',(1.1045291109289,54.7006406592484,14.8480810726317));
#51551=CARTESIAN_POINT('Ctrl Pts',(1.05549789251919,54.7078251990735,14.8805815184628));
#51552=CARTESIAN_POINT('Ctrl Pts',(1.00517136700043,54.715021033663,14.9106936329748));
#51553=CARTESIAN_POINT('Ctrl Pts',(0.979758885777928,54.7186545849463,14.9258988063246));
#51554=CARTESIAN_POINT('Ctrl Pts',(0.954015563949888,54.7222911175633,14.9404956120231));
#51555=CARTESIAN_POINT('Ctrl Pts',(0.927973476651595,54.7259365878508,14.9544748801754));
#51556=CARTESIAN_POINT('Ctrl Pts',(0.893796745032809,54.7307207765456,14.9728207865691));
#51557=CARTESIAN_POINT('Ctrl Pts',(0.859108679011762,54.735519788836,14.9901008160229));
#51558=CARTESIAN_POINT('Ctrl Pts',(0.823979210983868,54.7403413047258,15.0062811231433));
#51559=CARTESIAN_POINT('Ctrl Pts',(0.779141519510945,54.7464952732894,15.0269329479312));
#51560=CARTESIAN_POINT('Ctrl Pts',(0.733494641480898,54.7526971847942,15.0458314250729));
#51561=CARTESIAN_POINT('Ctrl Pts',(0.68717595580574,54.7589200776843,15.0629043571269));
#51562=CARTESIAN_POINT('Ctrl Pts',(0.621138160611772,54.7677922233465,15.0872456952696));
#51563=CARTESIAN_POINT('Ctrl Pts',(0.553739777889215,54.7767067860648,15.1078753309841));
#51564=CARTESIAN_POINT('Ctrl Pts',(0.485420860759286,54.7856209161682,15.1247012912355));
#51565=CARTESIAN_POINT('Ctrl Pts',(0.452329342757525,54.7899386382455,15.1328512530608));
#51566=CARTESIAN_POINT('Ctrl Pts',(0.41902263846378,54.7942561695393,15.1401088905563));
#51567=CARTESIAN_POINT('Ctrl Pts',(0.385555037498852,54.7985681399962,15.1464645876144));
#51568=CARTESIAN_POINT('Ctrl Pts',(0.315694081238318,54.8075690355132,15.1597315999303));
#51569=CARTESIAN_POINT('Ctrl Pts',(0.245123721470782,54.8165460827816,15.1690684576352));
#51570=CARTESIAN_POINT('Ctrl Pts',(0.174308308039462,54.825453119872,15.1743969078876));
#51571=CARTESIAN_POINT('Ctrl Pts',(0.0811955562954068,54.8371646766248,
15.1814031038764));
#51572=CARTESIAN_POINT('Ctrl Pts',(-0.0123431206148276,54.8487535530874,
15.1814778415116));
#51573=CARTESIAN_POINT('Ctrl Pts',(-0.105269596113297,54.8602467086059,
15.1747487460213));
#51574=CARTESIAN_POINT('Ctrl Pts',(-0.117388982246299,54.8617456354604,
15.1738711435282));
#51575=CARTESIAN_POINT('Ctrl Pts',(-0.129498009966489,54.8632429406556,
15.1728777664557));
#51576=CARTESIAN_POINT('Ctrl Pts',(-0.141594422119124,54.8647386897927,
15.1717688530728));
#51577=CARTESIAN_POINT('Ctrl Pts',(-0.210698118429061,54.8732835205096,
15.1654339156816));
#51578=CARTESIAN_POINT('Ctrl Pts',(-0.279387638366443,54.8817780342576,
15.1553310248002));
#51579=CARTESIAN_POINT('Ctrl Pts',(-0.347233554303374,54.8902407042179,
15.1415196819552));
#51580=CARTESIAN_POINT('Ctrl Pts',(-0.404438769885582,54.8973761205918,
15.1298744585984));
#51581=CARTESIAN_POINT('Ctrl Pts',(-0.461046174909015,54.9044895283375,
15.1155926501386));
#51582=CARTESIAN_POINT('Ctrl Pts',(-0.516811919155424,54.9116423589655,
15.0988271178759));
#51583=CARTESIAN_POINT('Ctrl Pts',(-0.558034649440151,54.9169298201433,
15.0864338283416));
#51584=CARTESIAN_POINT('Ctrl Pts',(-0.598798584235844,54.9222389603687,
15.0726833773101));
#51585=CARTESIAN_POINT('Ctrl Pts',(-0.639022928620526,54.9275968903586,
15.0576333803174));
#51586=CARTESIAN_POINT('Ctrl Pts',(-0.691423284760062,54.9345766794376,
15.038027710806));
#51587=CARTESIAN_POINT('Ctrl Pts',(-0.742858689603912,54.94156918436,15.0160690950034));
#51588=CARTESIAN_POINT('Ctrl Pts',(-0.79304668132035,54.9485513112826,14.9917571192118));
#51589=CARTESIAN_POINT('Ctrl Pts',(-0.793050137497275,54.9485517921041,
14.9917554449768));
#51590=CARTESIAN_POINT('Ctrl Pts',(-0.793053593668232,54.9485522729256,
14.9917537707307));
#51591=CARTESIAN_POINT('Ctrl Pts',(-0.793057049833323,54.948552753747,14.9917520964735));
#51592=CARTESIAN_POINT('Ctrl Pts',(-0.843325930740229,54.9555461564257,
14.967400528705));
#51593=CARTESIAN_POINT('Ctrl Pts',(-0.892436597767239,54.9625420879354,
14.9406429966578));
#51594=CARTESIAN_POINT('Ctrl Pts',(-0.940209835462784,54.9695356076179,
14.9116696924882));
#51595=CARTESIAN_POINT('Ctrl Pts',(-0.99948060200036,54.9782122494444,14.875723417333));
#51596=CARTESIAN_POINT('Ctrl Pts',(-1.05669633444349,54.986885757279,14.8363641429508));
#51597=CARTESIAN_POINT('Ctrl Pts',(-1.11154495611551,54.9955493130894,14.7939676217205));
#51598=CARTESIAN_POINT('Ctrl Pts',(-1.18011836431855,55.0063807529865,14.7409622066692));
#51599=CARTESIAN_POINT('Ctrl Pts',(-1.24507317015746,55.0172647628307,14.6833216989991));
#51600=CARTESIAN_POINT('Ctrl Pts',(-1.30585067138259,55.0281499189929,14.6216377858003));
#51601=CARTESIAN_POINT('Ctrl Pts',(-1.32326904095905,55.0312695219563,14.6039596454464));
#51602=CARTESIAN_POINT('Ctrl Pts',(-1.34034407033215,55.0343891732573,14.5859496246742));
#51603=CARTESIAN_POINT('Ctrl Pts',(-1.35706209430618,55.0375075526115,14.5676222358385));
#51604=CARTESIAN_POINT('Ctrl Pts',(-1.4148722599396,55.0482907664203,14.5042469597972));
#51605=CARTESIAN_POINT('Ctrl Pts',(-1.46834378222509,55.0590039229693,14.436999571369));
#51606=CARTESIAN_POINT('Ctrl Pts',(-1.51691811043868,55.0695959792902,14.3664663840971));
#51607=CARTESIAN_POINT('Ctrl Pts',(-1.53174347091961,55.0728287785684,14.344938964869));
#51608=CARTESIAN_POINT('Ctrl Pts',(-1.54611232790725,55.0760502512918,14.323105646365));
#51609=CARTESIAN_POINT('Ctrl Pts',(-1.56000801185874,55.0792588263726,14.3009836527408));
#51610=CARTESIAN_POINT('Ctrl Pts',(-1.56785142348161,55.0810699049182,14.2884969048758));
#51611=CARTESIAN_POINT('Ctrl Pts',(-1.57554417590168,55.08287693321,14.275918244921));
#51612=CARTESIAN_POINT('Ctrl Pts',(-1.58311073051578,55.0846979624443,14.2632682439016));
#51613=CARTESIAN_POINT('Ctrl Pts',(-1.62534322423445,55.0948619815549,14.1926626491703));
#51614=CARTESIAN_POINT('Ctrl Pts',(-1.66310508793709,55.1050900365467,14.1194240766291));
#51615=CARTESIAN_POINT('Ctrl Pts',(-1.69586650256542,55.1153377196764,14.0440500537282));
#51616=CARTESIAN_POINT('Ctrl Pts',(-1.70752168791717,55.1189834305731,14.0172350270395));
#51617=CARTESIAN_POINT('Ctrl Pts',(-1.71854371166593,55.1226315743923,13.9901501189781));
#51618=CARTESIAN_POINT('Ctrl Pts',(-1.72890790254973,55.1262799825131,13.9628190815204));
#51619=CARTESIAN_POINT('Ctrl Pts',(-1.75333580604556,55.1348791064089,13.8984011300426));
#51620=CARTESIAN_POINT('Ctrl Pts',(-1.77410160560406,55.1434784421197,13.832624048792));
#51621=CARTESIAN_POINT('Ctrl Pts',(-1.79091349418602,55.1520644111161,13.7659367660082));
#51622=CARTESIAN_POINT('Ctrl Pts',(-1.79246644812194,55.1528575173922,13.759776703873));
#51623=CARTESIAN_POINT('Ctrl Pts',(-1.79398570053851,55.1536505096524,13.7536088842887));
#51624=CARTESIAN_POINT('Ctrl Pts',(-1.7954710437966,55.154443377217,13.7474336659534));
#51625=CARTESIAN_POINT('Ctrl Pts',(-1.80135087869247,55.1575819987772,13.7229886334265));
#51626=CARTESIAN_POINT('Ctrl Pts',(-1.80670183139332,55.1607199865764,13.6984173801498));
#51627=CARTESIAN_POINT('Ctrl Pts',(-1.81155592987185,55.1638573620779,13.6737506746323));
#51628=CARTESIAN_POINT('Ctrl Pts',(-1.81330583161973,55.1649883854591,13.6648583311229));
#51629=CARTESIAN_POINT('Ctrl Pts',(-1.81499116133037,55.1661193291232,13.6559535835665));
#51630=CARTESIAN_POINT('Ctrl Pts',(-1.81661341753146,55.1672501939202,13.6470378741801));
#51631=CARTESIAN_POINT('Ctrl Pts',(-1.82273579646637,55.1715180665328,13.6133900747136));
#51632=CARTESIAN_POINT('Ctrl Pts',(-1.82795995185744,55.175784914625,13.5795853653127));
#51633=CARTESIAN_POINT('Ctrl Pts',(-1.83223365124789,55.1800507599276,13.5456737987172));
#51634=CARTESIAN_POINT('Ctrl Pts',(-1.84078126599194,55.188582666099,13.4778489518705));
#51635=CARTESIAN_POINT('Ctrl Pts',(-1.8455267573646,55.1971103793718,13.4095981151255));
#51636=CARTESIAN_POINT('Ctrl Pts',(-1.84652897031419,55.2056346992264,13.3412881479247));
#51637=CARTESIAN_POINT('Ctrl Pts',(-1.84753119218581,55.2141590949674,13.2729775726064));
#51638=CARTESIAN_POINT('Ctrl Pts',(-1.8447901515034,55.2226801902056,13.2046070996695));
#51639=CARTESIAN_POINT('Ctrl Pts',(-1.83824820549194,55.2311986099251,13.1366853948064));
#51640=CARTESIAN_POINT('Ctrl Pts',(-1.83170648471668,55.2397167363594,13.0687660284565));
#51641=CARTESIAN_POINT('Ctrl Pts',(-1.82136420101102,55.2482319227119,13.0012975276562));
#51642=CARTESIAN_POINT('Ctrl Pts',(-1.80738596135678,55.2567441298735,12.9345246763386));
#51643=CARTESIAN_POINT('Ctrl Pts',(-1.7958763752515,55.2637530225307,12.8795443711826));
#51644=CARTESIAN_POINT('Ctrl Pts',(-1.78190396256387,55.27075866633,12.8250453163076));
#51645=CARTESIAN_POINT('Ctrl Pts',(-1.76553466932195,55.2777622567396,12.7712659931012));
#51646=CARTESIAN_POINT('Ctrl Pts',(-1.73900282001386,55.2891138894959,12.6840988272306));
#51647=CARTESIAN_POINT('Ctrl Pts',(-1.70617317211776,55.3004606173606,12.5988184176065));
#51648=CARTESIAN_POINT('Ctrl Pts',(-1.66731880928453,55.3118054938855,12.5164595315625));
#51649=CARTESIAN_POINT('Ctrl Pts',(-1.63622777574238,55.320883597626,12.4505564333834));
#51650=CARTESIAN_POINT('Ctrl Pts',(-1.60127815679782,55.3299605556722,12.3865240861352));
#51651=CARTESIAN_POINT('Ctrl Pts',(-1.56261594941289,55.3390359058805,12.3249085851209));
#51652=CARTESIAN_POINT('Ctrl Pts',(-1.53459200795931,55.3456140890757,12.2802471622522));
#51653=CARTESIAN_POINT('Ctrl Pts',(-1.50461590022783,55.352191706902,12.2368539906714));
#51654=CARTESIAN_POINT('Ctrl Pts',(-1.4727569997285,55.3587661371559,12.1949514660604));
#51655=CARTESIAN_POINT('Ctrl Pts',(-1.46117279727529,55.3611566631905,12.1797153053396));
#51656=CARTESIAN_POINT('Ctrl Pts',(-1.44933381467607,55.3635479861347,12.1646684157009));
#51657=CARTESIAN_POINT('Ctrl Pts',(-1.43724904690904,55.3659398809156,12.1498168760294));
#51658=CARTESIAN_POINT('Ctrl Pts',(-1.39109517265427,55.375074951864,12.093096208516));
#51659=CARTESIAN_POINT('Ctrl Pts',(-1.34135318348424,55.3842183341153,12.0392277203063));
#51660=CARTESIAN_POINT('Ctrl Pts',(-1.28855352533096,55.3933571845613,11.9885318653594));
#51661=CARTESIAN_POINT('Ctrl Pts',(-1.27681760630921,55.3953885009095,11.977263564215));
#51662=CARTESIAN_POINT('Ctrl Pts',(-1.26493077684308,55.3974195934414,11.966151872421));
#51663=CARTESIAN_POINT('Ctrl Pts',(-1.25289910879172,55.3994503212419,11.9552000687445));
#51664=CARTESIAN_POINT('Ctrl Pts',(-1.18633035288021,55.4106859223814,11.8946059813228));
#51665=CARTESIAN_POINT('Ctrl Pts',(-1.11533190320657,55.4219097733954,11.8389101339942));
#51666=CARTESIAN_POINT('Ctrl Pts',(-1.04084807000666,55.4331806272757,11.7884745408066));
#51667=CARTESIAN_POINT('Ctrl Pts',(-1.02245212373735,55.4359642920454,11.7760180059791));
#51668=CARTESIAN_POINT('Ctrl Pts',(-1.00384339555138,55.4387508482516,11.7638821670127));
#51669=CARTESIAN_POINT('Ctrl Pts',(-0.985035741393843,55.4415412284531,
11.752072159837));
#51670=CARTESIAN_POINT('Ctrl Pts',(-0.936512183150477,55.4487403812605,
11.721602460307));
#51671=CARTESIAN_POINT('Ctrl Pts',(-0.886691372514162,55.4560121312427,
11.693252979208));
#51672=CARTESIAN_POINT('Ctrl Pts',(-0.835685478204693,55.4632411084962,
11.6672298356327));
#51673=CARTESIAN_POINT('Ctrl Pts',(-0.817858458691767,55.4657677011636,
11.6581345125414));
#51674=CARTESIAN_POINT('Ctrl Pts',(-0.799887020170616,55.4682890112393,
11.6493236758217));
#51675=CARTESIAN_POINT('Ctrl Pts',(-0.781777121593457,55.4707999286012,
11.6408070442452));
#51676=CARTESIAN_POINT('Ctrl Pts',(-0.716426553116967,55.4798607124755,
11.6100743091801));
#51677=CARTESIAN_POINT('Ctrl Pts',(-0.649259766796169,55.4887874631735,
11.5831662722903));
#51678=CARTESIAN_POINT('Ctrl Pts',(-0.580774250314715,55.4976838882126,
11.5602168129255));
#51679=CARTESIAN_POINT('Ctrl Pts',(-0.542986589613307,55.5025925916597,
11.5475541883545));
#51680=CARTESIAN_POINT('Ctrl Pts',(-0.504796551051388,55.5074921845024,
11.53609645761));
#51681=CARTESIAN_POINT('Ctrl Pts',(-0.466281015117716,55.5124009729648,
11.5258653905635));
#51682=CARTESIAN_POINT('Ctrl Pts',(-0.393893962647231,55.521626671618,11.5066368696778));
#51683=CARTESIAN_POINT('Ctrl Pts',(-0.320375910066749,55.5309460030142,
11.491681157064));
#51684=CARTESIAN_POINT('Ctrl Pts',(-0.246275569710484,55.5402915980726,
11.481338529198));
#51685=CARTESIAN_POINT('Ctrl Pts',(-0.212808585785349,55.5445124812438,
11.4766673420095));
#51686=CARTESIAN_POINT('Ctrl Pts',(-0.179223385183204,55.5487386688748,
11.4729367241748));
#51687=CARTESIAN_POINT('Ctrl Pts',(-0.145572996244575,55.5529636959111,
11.4701755549305));
#51688=CARTESIAN_POINT('Ctrl Pts',(-0.120424406205636,55.5561212663342,
11.4681119974043));
#51689=CARTESIAN_POINT('Ctrl Pts',(-0.0952411304475411,55.5592779727016,
11.4665900555687));
#51690=CARTESIAN_POINT('Ctrl Pts',(-0.0700489944315699,55.5624330172247,
11.4656184500148));
#51691=CARTESIAN_POINT('Ctrl Pts',(-0.0700341519148885,55.5624348760905,
11.4656178775714));
#51692=CARTESIAN_POINT('Ctrl Pts',(-0.0700193093888145,55.562436734963,
11.4656173053121));
#51693=CARTESIAN_POINT('Ctrl Pts',(-0.0700044668533595,55.5624385938423,
11.465616733237));
#51694=CARTESIAN_POINT('Ctrl Pts',(0.00238493529662621,55.5715046429639,
11.462826632086));
#51695=CARTESIAN_POINT('Ctrl Pts',(0.075001165013121,55.5807303128564,11.4644191143735));
#51696=CARTESIAN_POINT('Ctrl Pts',(0.147334995159917,55.5900284904859,11.4702925062558));
#51697=CARTESIAN_POINT('Ctrl Pts',(0.17072954618932,55.5930357512738,11.4721921065649));
#51698=CARTESIAN_POINT('Ctrl Pts',(0.194094231384653,55.5960505570346,11.4745392584708));
#51699=CARTESIAN_POINT('Ctrl Pts',(0.21741095317351,55.5990698478536,11.4773297641015));
#51700=CARTESIAN_POINT('Ctrl Pts',(0.315510529343815,55.6117727977951,11.4890701546313));
#51701=CARTESIAN_POINT('Ctrl Pts',(0.412796477800318,55.6243902239284,11.5088324041391));
#51702=CARTESIAN_POINT('Ctrl Pts',(0.508054631261452,55.6368958253134,11.5361404005733));
#51703=CARTESIAN_POINT('Ctrl Pts',(0.604937458395263,55.6496147157513,11.5639141480351));
#51704=CARTESIAN_POINT('Ctrl Pts',(0.699722509577989,55.6622180924772,11.5994929288359));
#51705=CARTESIAN_POINT('Ctrl Pts',(0.791131408574685,55.6747007094324,11.6423601989366));
#51706=CARTESIAN_POINT('Ctrl Pts',(0.881175096093966,55.6869968958308,11.6845872371804));
#51707=CARTESIAN_POINT('Ctrl Pts',(0.967942559080783,55.6991759410771,11.7338864645313));
#51708=CARTESIAN_POINT('Ctrl Pts',(1.05021417244992,55.7112528001152,11.7897532406534));
#51709=CARTESIAN_POINT('Ctrl Pts',(1.08566836928764,55.7164572116976,11.8138285151766));
#51710=CARTESIAN_POINT('Ctrl Pts',(1.12028768546031,55.7216428988617,11.839123331228));
#51711=CARTESIAN_POINT('Ctrl Pts',(1.15397469145896,55.7268122444113,11.8655966986872));
#51712=CARTESIAN_POINT('Ctrl Pts',(1.2108410677276,55.7355385155766,11.910285872759));
#51713=CARTESIAN_POINT('Ctrl Pts',(1.26516494342727,55.7444350125964,11.9581902961626));
#51714=CARTESIAN_POINT('Ctrl Pts',(1.31639363809883,55.7534138154864,12.0091358894873));
#51715=CARTESIAN_POINT('Ctrl Pts',(1.33567634726397,55.7567934769415,12.0283120380428));
#51716=CARTESIAN_POINT('Ctrl Pts',(1.35452053906315,55.7601847572048,12.0479185383536));
#51717=CARTESIAN_POINT('Ctrl Pts',(1.37289698704502,55.7635828157681,12.0679441978291));
#51718=CARTESIAN_POINT('Ctrl Pts',(1.37795301575926,55.7645177451781,12.0734539845643));
#51719=CARTESIAN_POINT('Ctrl Pts',(1.38297317089069,55.7654525783454,12.0789957082114));
#51720=CARTESIAN_POINT('Ctrl Pts',(1.38795682403215,55.7663872885772,12.0845689660414));
#51721=CARTESIAN_POINT('Ctrl Pts',(1.39949629048309,55.7685515759092,12.0974736405694));
#51722=CARTESIAN_POINT('Ctrl Pts',(1.41084700069948,55.7707165090372,12.1105551753011));
#51723=CARTESIAN_POINT('Ctrl Pts',(1.42200470289133,55.7728817995221,12.1238052629277));
#51724=CARTESIAN_POINT('Ctrl Pts',(1.45566265210831,55.7794135419839,12.1637750316837));
#51725=CARTESIAN_POINT('Ctrl Pts',(1.48756365211122,55.7859485648259,12.2052793343133));
#51726=CARTESIAN_POINT('Ctrl Pts',(1.51761462390527,55.7924819067513,12.2481011209081));
#51727=CARTESIAN_POINT('Ctrl Pts',(1.54766559569933,55.7990152486767,12.2909229075029));
#51728=CARTESIAN_POINT('Ctrl Pts',(1.57587332813735,55.8055479803492,12.3350678823099));
#51729=CARTESIAN_POINT('Ctrl Pts',(1.60218878834419,55.8120850137067,12.3803850023654));
#51730=CARTESIAN_POINT('Ctrl Pts',(1.64845076863821,55.8235769696136,12.4600514683331));
#51731=CARTESIAN_POINT('Ctrl Pts',(1.68885348102637,55.8350806624248,12.5433328066042));
#51732=CARTESIAN_POINT('Ctrl Pts',(1.72305341899742,55.8466891972649,12.6291521935411));
#51733=CARTESIAN_POINT('Ctrl Pts',(1.73239851669919,55.8498612174115,12.6526022523193));
#51734=CARTESIAN_POINT('Ctrl Pts',(1.74128074819349,55.8530410970104,12.6762419566786));
#51735=CARTESIAN_POINT('Ctrl Pts',(1.74969366836096,55.8562308054419,12.7000497027787));
#51736=CARTESIAN_POINT('Ctrl Pts',(1.78454516205636,55.8694445411099,12.7986760413855));
#51737=CARTESIAN_POINT('Ctrl Pts',(1.8111965418513,55.8826079458639,12.9002677257654));
#51738=CARTESIAN_POINT('Ctrl Pts',(1.82902797094738,55.8956085399769,13.0034160787279));
#51739=CARTESIAN_POINT('Ctrl Pts',(1.83028611148198,55.8965258290142,13.0106939656118));
#51740=CARTESIAN_POINT('Ctrl Pts',(1.83150033296328,55.8974423047915,13.0179795834037));
#51741=CARTESIAN_POINT('Ctrl Pts',(1.83267041346338,55.8983579265671,13.0252724285714));
#51742=CARTESIAN_POINT('Ctrl Pts',(1.84206444066225,55.9057090240887,13.083823259781));
#51743=CARTESIAN_POINT('Ctrl Pts',(1.84861496845924,55.9130059892496,13.1428471078161));
#51744=CARTESIAN_POINT('Ctrl Pts',(1.85226648614548,55.920319285591,13.2020811701997));
#51745=CARTESIAN_POINT('Ctrl Pts',(1.85226753774617,55.9203213917474,13.2020982290191));
#51746=CARTESIAN_POINT('Ctrl Pts',(1.85226858910766,55.920323497907,13.2021152878546));
#51747=CARTESIAN_POINT('Ctrl Pts',(1.85226964022996,55.9203256040698,13.2021323467061));
#51748=CARTESIAN_POINT('Ctrl Pts',(1.85902336759589,55.9338582340013,13.3117397944665));
#51749=CARTESIAN_POINT('Ctrl Pts',(1.85589972572324,55.9475221773674,13.4220160755468));
#51750=CARTESIAN_POINT('Ctrl Pts',(1.84323309485339,55.9612356686241,13.5312848453473));
#51751=CARTESIAN_POINT('Ctrl Pts',(1.84011107204006,55.9646157175884,13.55821699452));
#51752=CARTESIAN_POINT('Ctrl Pts',(1.83640946560615,55.9679987528036,13.5850877443923));
#51753=CARTESIAN_POINT('Ctrl Pts',(1.83213361865251,55.9713835039069,13.6118716542082));
#51754=CARTESIAN_POINT('Ctrl Pts',(1.81019802534562,55.9887476716263,13.7492762337592));
#51755=CARTESIAN_POINT('Ctrl Pts',(1.77316380370024,56.0061759019501,13.8843946461673));
#51756=CARTESIAN_POINT('Ctrl Pts',(1.721841056594,56.0236692220895,14.0139129323168));
#51757=CARTESIAN_POINT('Ctrl Pts',(1.67792950830242,56.0386364406309,14.1247282880327));
#51758=CARTESIAN_POINT('Ctrl Pts',(1.62354173049666,56.0536231692044,14.2314457018421));
#51759=CARTESIAN_POINT('Ctrl Pts',(1.55912072822312,56.0686012394853,14.3320167736881));
#51760=CARTESIAN_POINT('Ctrl Pts',(1.55558827495383,56.0694225451382,14.3375314754003));
#51761=CARTESIAN_POINT('Ctrl Pts',(1.55202564578714,56.0702438242641,14.3430276865584));
#51762=CARTESIAN_POINT('Ctrl Pts',(1.54843291093098,56.0710650720493,14.3485050657812));
#51763=CARTESIAN_POINT('Ctrl Pts',(1.54236165712056,56.0724528738062,14.3577611230214));
#51764=CARTESIAN_POINT('Ctrl Pts',(1.53620441579189,56.0738406055688,14.3669634397666));
#51765=CARTESIAN_POINT('Ctrl Pts',(1.52996196036076,56.0752287214057,14.3761102651033));
#51766=CARTESIAN_POINT('Ctrl Pts',(1.5299561689752,56.0752300092185,14.3761187509936));
#51767=CARTESIAN_POINT('Ctrl Pts',(1.52995037751575,56.0752312970319,14.3761272368371));
#51768=CARTESIAN_POINT('Ctrl Pts',(1.52994458598239,56.0752325848458,14.3761357226337));
#51769=CARTESIAN_POINT('Ctrl Pts',(1.48073277321199,56.0861753961918,14.448241227112));
#51770=CARTESIAN_POINT('Ctrl Pts',(1.42618104474603,56.0971582812265,14.5169620994692));
#51771=CARTESIAN_POINT('Ctrl Pts',(1.36700329858654,56.1081536370437,14.5816650405516));
#51772=CARTESIAN_POINT('Ctrl Pts',(1.34777982439549,56.1117254009666,14.6026833354125));
#51773=CARTESIAN_POINT('Ctrl Pts',(1.32806857343291,56.1152984746277,14.623277826765));
#51774=CARTESIAN_POINT('Ctrl Pts',(1.30789502252752,56.1188718941239,14.6434274028874));
#51775=CARTESIAN_POINT('Ctrl Pts',(1.23332838239186,56.1320801729677,14.7179054260498));
#51776=CARTESIAN_POINT('Ctrl Pts',(1.1524419907,56.1452918989564,14.78630148597));
#51777=CARTESIAN_POINT('Ctrl Pts',(1.06649397803563,56.1584436465506,14.8476206408121));
#51778=CARTESIAN_POINT('Ctrl Pts',(1.00092954881442,56.1684763023101,14.8943972359063));
#51779=CARTESIAN_POINT('Ctrl Pts',(0.932411137742052,56.1784705523755,14.937067035271));
#51780=CARTESIAN_POINT('Ctrl Pts',(0.861396890224984,56.1884804284716,14.9752810838156));
#51781=CARTESIAN_POINT('Ctrl Pts',(0.829645719418002,56.1929559428478,14.9923669620019));
#51782=CARTESIAN_POINT('Ctrl Pts',(0.797395108893155,56.1974346009196,15.0085616334312));
#51783=CARTESIAN_POINT('Ctrl Pts',(0.764683860406484,56.2019213265822,15.0238312852542));
#51784=CARTESIAN_POINT('Ctrl Pts',(0.697830046211415,56.2110910996011,15.0550387295744));
#51785=CARTESIAN_POINT('Ctrl Pts',(0.629059785282966,56.22029826175,15.0823759652349));
#51786=CARTESIAN_POINT('Ctrl Pts',(0.558876386431781,56.2295436592919,15.1054854320513));
#51787=CARTESIAN_POINT('Ctrl Pts',(0.553821518874132,56.2302095469641,15.1071498611898));
#51788=CARTESIAN_POINT('Ctrl Pts',(0.548759327893151,56.2308756330845,15.1087923805333));
#51789=CARTESIAN_POINT('Ctrl Pts',(0.543690004547129,56.2315419180171,15.1104128666647));
#51790=CARTESIAN_POINT('Ctrl Pts',(0.543678051144725,56.2315434891088,15.1104166877511));
#51791=CARTESIAN_POINT('Ctrl Pts',(0.543666097701438,56.2315450602015,15.1104205087153));
#51792=CARTESIAN_POINT('Ctrl Pts',(0.54365414421728,56.231546631295,15.1104243295572));
#51793=CARTESIAN_POINT('Ctrl Pts',(0.507541019102652,56.2362931216487,15.1219676201155));
#51794=CARTESIAN_POINT('Ctrl Pts',(0.471054633796932,56.2410479110577,15.1323946376915));
#51795=CARTESIAN_POINT('Ctrl Pts',(0.434265931366752,56.2457936695816,15.14169693376));
#51796=CARTESIAN_POINT('Ctrl Pts',(0.335571148175681,56.2585253392966,15.1666526411651));
#51797=CARTESIAN_POINT('Ctrl Pts',(0.234687921336243,56.2711916404696,15.1835209071129));
#51798=CARTESIAN_POINT('Ctrl Pts',(0.132892379707592,56.2838529014418,15.192323894123));
#51799=CARTESIAN_POINT('Ctrl Pts',(0.108514262031127,56.286885035315,15.1944320439477));
#51800=CARTESIAN_POINT('Ctrl Pts',(0.0840837083974954,56.2899168895166,
15.1960774334646));
#51801=CARTESIAN_POINT('Ctrl Pts',(0.0596180681824553,56.292949310042,15.1972599649554));
#51802=CARTESIAN_POINT('Ctrl Pts',(-0.0685561533320207,56.308836004064,
15.2034551861683));
#51803=CARTESIAN_POINT('Ctrl Pts',(-0.197691698140074,56.3247402671585,
15.1969458271626));
#51804=CARTESIAN_POINT('Ctrl Pts',(-0.325118024785957,56.3407799463547,
15.1777131839381));
#51805=CARTESIAN_POINT('Ctrl Pts',(-0.419898235242895,56.3527103237726,
15.1634078671292));
#51806=CARTESIAN_POINT('Ctrl Pts',(-0.513732117860426,56.364704380367,15.1420555001306));
#51807=CARTESIAN_POINT('Ctrl Pts',(-0.605457643405961,56.3768028412959,
15.1136862713413));
#51808=CARTESIAN_POINT('Ctrl Pts',(-0.637051603263352,56.380970037795,15.1039147680414));
#51809=CARTESIAN_POINT('Ctrl Pts',(-0.66839563189717,56.385149631178,15.0933111903414));
#51810=CARTESIAN_POINT('Ctrl Pts',(-0.699443003129483,56.3893433170818,
15.0818780096305));
#51811=CARTESIAN_POINT('Ctrl Pts',(-0.69947526575327,56.3893476749164,15.0818661289336));
#51812=CARTESIAN_POINT('Ctrl Pts',(-0.699507528056461,56.3893520327582,
15.0818542473376));
#51813=CARTESIAN_POINT('Ctrl Pts',(-0.699539790038952,56.389356390607,15.0818423648428));
#51814=CARTESIAN_POINT('Ctrl Pts',(-0.78224520260987,56.4005279820027,15.0513809187576));
#51815=CARTESIAN_POINT('Ctrl Pts',(-0.862845916453469,56.4117464350318,
15.0150127704698));
#51816=CARTESIAN_POINT('Ctrl Pts',(-0.940695421505603,56.422863422228,14.9731872027529));
#51817=CARTESIAN_POINT('Ctrl Pts',(-1.02619563775041,56.4350729386357,14.9272511999232));
#51818=CARTESIAN_POINT('Ctrl Pts',(-1.10840993016031,56.4471642416883,14.8747167149216));
#51819=CARTESIAN_POINT('Ctrl Pts',(-1.18649340540652,56.4592287353092,14.8162241243345));
#51820=CARTESIAN_POINT('Ctrl Pts',(-1.19648353546117,56.4607722867448,14.8087404847378));
#51821=CARTESIAN_POINT('Ctrl Pts',(-1.20640602416328,56.4623154026554,14.8011592507069));
#51822=CARTESIAN_POINT('Ctrl Pts',(-1.2162590773069,56.4638582773433,14.7934817067346));
#51823=CARTESIAN_POINT('Ctrl Pts',(-1.30651622245473,56.4779915071776,14.7231529273614));
#51824=CARTESIAN_POINT('Ctrl Pts',(-1.39094420748223,56.4921062989355,14.6447395298765));
#51825=CARTESIAN_POINT('Ctrl Pts',(-1.46799871801572,56.5063320712309,14.5593892863486));
#51826=CARTESIAN_POINT('Ctrl Pts',(-1.52148336091198,56.51620638418,14.5001464559861));
#51827=CARTESIAN_POINT('Ctrl Pts',(-1.57141296562096,56.5261347541126,14.4375617369057));
#51828=CARTESIAN_POINT('Ctrl Pts',(-1.61724853091761,56.5361453034843,14.372092803771));
#51829=CARTESIAN_POINT('Ctrl Pts',(-1.63329747805945,56.5396504152177,14.3491693939578));
#51830=CARTESIAN_POINT('Ctrl Pts',(-1.64884489548224,56.5431656067566,14.3258926168765));
#51831=CARTESIAN_POINT('Ctrl Pts',(-1.66386901373267,56.5466920994784,14.3022828030678));
#51832=CARTESIAN_POINT('Ctrl Pts',(-1.66775409226985,56.5476040133064,14.2961775542029));
#51833=CARTESIAN_POINT('Ctrl Pts',(-1.67160414596099,56.5485166645035,14.2900500889728));
#51834=CARTESIAN_POINT('Ctrl Pts',(-1.67541879375985,56.5494300660031,14.2839007854373));
#51835=CARTESIAN_POINT('Ctrl Pts',(-1.67542857316578,56.5494324076411,14.2838850208009));
#51836=CARTESIAN_POINT('Ctrl Pts',(-1.67543835234168,56.5494347492824,14.2838692560154));
#51837=CARTESIAN_POINT('Ctrl Pts',(-1.67544813128754,56.549437090927,14.2838534910808));
#51838=CARTESIAN_POINT('Ctrl Pts',(-1.73166717470118,56.5628991780055,14.1932210695618));
#51839=CARTESIAN_POINT('Ctrl Pts',(-1.7802821448428,56.5764719208028,14.0976574064469));
#51840=CARTESIAN_POINT('Ctrl Pts',(-1.82086816109241,56.5899673755073,13.9985909126802));
#51841=CARTESIAN_POINT('Ctrl Pts',(-1.83346210570417,56.594155049607,13.9678503263732));
#51842=CARTESIAN_POINT('Ctrl Pts',(-1.84528453972575,56.5983357505854,13.9367695762817));
#51843=CARTESIAN_POINT('Ctrl Pts',(-1.85632531934735,56.6025053100698,13.905383230766));
#51844=CARTESIAN_POINT('Ctrl Pts',(-1.89151540826478,56.6157948760269,13.8053460660597));
#51845=CARTESIAN_POINT('Ctrl Pts',(-1.91877554968822,56.6289730326751,13.7021842607744));
#51846=CARTESIAN_POINT('Ctrl Pts',(-1.93772504824362,56.6421593605133,13.5971903439077));
#51847=CARTESIAN_POINT('Ctrl Pts',(-1.95452879666546,56.6538525319685,13.5040854335222));
#51848=CARTESIAN_POINT('Ctrl Pts',(-1.96478960842525,56.6655532679108,13.4095385159904));
#51849=CARTESIAN_POINT('Ctrl Pts',(-1.96821851392384,56.6773260564793,13.3146094627546));
#51850=CARTESIAN_POINT('Ctrl Pts',(-1.96864668786567,56.6787961469468,13.3027554915867));
#51851=CARTESIAN_POINT('Ctrl Pts',(-1.96896839853184,56.6802673622679,13.2908955655712));
#51852=CARTESIAN_POINT('Ctrl Pts',(-1.96918314058438,56.6817398291142,13.2790317489242));
#51853=CARTESIAN_POINT('Ctrl Pts',(-1.9705243099076,56.6909361059507,13.2049364017167));
#51854=CARTESIAN_POINT('Ctrl Pts',(-1.96768877568565,56.700180753234,13.1306939107237));
#51855=CARTESIAN_POINT('Ctrl Pts',(-1.96057944937995,56.7094914055201,13.056870603467));
#51856=CARTESIAN_POINT('Ctrl Pts',(-1.95988008122185,56.7104073254624,13.0496083583258));
#51857=CARTESIAN_POINT('Ctrl Pts',(-1.95913939547865,56.7113238842644,13.0423501628215));
#51858=CARTESIAN_POINT('Ctrl Pts',(-1.95835732692828,56.7122410987799,13.0350965506566));
#51859=CARTESIAN_POINT('Ctrl Pts',(-1.9583549776439,56.7122438540342,13.0350747612652));
#51860=CARTESIAN_POINT('Ctrl Pts',(-1.95835262798405,56.712246609294,13.0350529719006));
#51861=CARTESIAN_POINT('Ctrl Pts',(-1.95835027794874,56.7122493645591,13.0350311825627));
#51862=CARTESIAN_POINT('Ctrl Pts',(-1.94942210937261,56.7227170675724,12.9522499239088));
#51863=CARTESIAN_POINT('Ctrl Pts',(-1.93507012850912,56.7332631872279,12.8698553643149));
#51864=CARTESIAN_POINT('Ctrl Pts',(-1.91555053220342,56.7438198278824,12.7885681907034));
#51865=CARTESIAN_POINT('Ctrl Pts',(-1.91187738352266,56.7458063500464,12.7732717742284));
#51866=CARTESIAN_POINT('Ctrl Pts',(-1.90802139393833,56.7477932422511,12.7580145634693));
#51867=CARTESIAN_POINT('Ctrl Pts',(-1.90398447376313,56.7497800486625,12.7428013385255));
#51868=CARTESIAN_POINT('Ctrl Pts',(-1.87969668306578,56.7617335023307,12.6512722502031));
#51869=CARTESIAN_POINT('Ctrl Pts',(-1.84886272379624,56.773683397275,12.5613300144799));
#51870=CARTESIAN_POINT('Ctrl Pts',(-1.81181807371057,56.7855656036989,12.4737890131985));
#51871=CARTESIAN_POINT('Ctrl Pts',(-1.77337490374494,56.7978963904674,12.3829431398149));
#51872=CARTESIAN_POINT('Ctrl Pts',(-1.72822716320002,56.8101594420461,12.2946479662481));
#51873=CARTESIAN_POINT('Ctrl Pts',(-1.67673317282235,56.8224286711405,12.2098773844661));
#51874=CARTESIAN_POINT('Ctrl Pts',(-1.63200254411193,56.833086426097,12.1362408029651));
#51875=CARTESIAN_POINT('Ctrl Pts',(-1.5824772617458,56.8437495532281,12.0652671014348));
#51876=CARTESIAN_POINT('Ctrl Pts',(-1.52848077798596,56.8544481068479,11.9977181194456));
#51877=CARTESIAN_POINT('Ctrl Pts',(-1.52027105502172,56.8560747342729,11.9874478501608));
#51878=CARTESIAN_POINT('Ctrl Pts',(-1.51195805342695,56.8577021810085,11.9772566934403));
#51879=CARTESIAN_POINT('Ctrl Pts',(-1.50354299493526,56.859330553044,11.9671472623586));
#51880=CARTESIAN_POINT('Ctrl Pts',(-1.47174310670255,56.8654840514161,11.928944464504));
#51881=CARTESIAN_POINT('Ctrl Pts',(-1.43848741615714,56.8716502280323,11.8919122782969));
#51882=CARTESIAN_POINT('Ctrl Pts',(-1.40386139808873,56.877831231114,11.8562029393545));
#51883=CARTESIAN_POINT('Ctrl Pts',(-1.40386046433392,56.8778313977962,11.8562019763859));
#51884=CARTESIAN_POINT('Ctrl Pts',(-1.40385953057813,56.8778315644784,11.8562010134183));
#51885=CARTESIAN_POINT('Ctrl Pts',(-1.40385859682132,56.8778317311607,11.8562000504517));
#51886=CARTESIAN_POINT('Ctrl Pts',(-1.34522097650263,56.888298963774,11.7957281242066));
#51887=CARTESIAN_POINT('Ctrl Pts',(-1.28249847102813,56.8988525226504,11.7388890411541));
#51888=CARTESIAN_POINT('Ctrl Pts',(-1.21634219263946,56.9094485475929,11.6861013943469));
#51889=CARTESIAN_POINT('Ctrl Pts',(-1.19953584886059,56.9121403622204,11.6726912183042));
#51890=CARTESIAN_POINT('Ctrl Pts',(-1.18250809592946,56.9148349151284,11.6595423287713));
#51891=CARTESIAN_POINT('Ctrl Pts',(-1.16526997419257,56.9175314826331,11.6466612036137));
#51892=CARTESIAN_POINT('Ctrl Pts',(-1.08024870125905,56.9308314004145,11.5831293598069));
#51893=CARTESIAN_POINT('Ctrl Pts',(-0.990110409353869,56.944179928467,11.5261072649819));
#51894=CARTESIAN_POINT('Ctrl Pts',(-0.895963198840052,56.9575258852969,
11.4762188380546));
#51895=CARTESIAN_POINT('Ctrl Pts',(-0.86252406533658,56.9622660919343,11.4584995051164));
#51896=CARTESIAN_POINT('Ctrl Pts',(-0.828577042689153,56.9670063253804,
11.4416791736747));
#51897=CARTESIAN_POINT('Ctrl Pts',(-0.794164262756547,56.9717454508399,
11.425784319842));
#51898=CARTESIAN_POINT('Ctrl Pts',(-0.698103620334191,56.984974356992,11.3814150514084));
#51899=CARTESIAN_POINT('Ctrl Pts',(-0.598389926248981,56.9981979151434,
11.3442478963313));
#51900=CARTESIAN_POINT('Ctrl Pts',(-0.496141424071205,57.0114391775981,
11.3149825420423));
#51901=CARTESIAN_POINT('Ctrl Pts',(-0.419989513947958,57.0213009106005,
11.2931865002219));
#51902=CARTESIAN_POINT('Ctrl Pts',(-0.342433433999361,57.0311722124074,
11.2757784038796));
#51903=CARTESIAN_POINT('Ctrl Pts',(-0.264046529588669,57.0410477488817,
11.2630516991051));
#51904=CARTESIAN_POINT('Ctrl Pts',(-0.249205642273958,57.0429174709366,
11.260642169186));
#51905=CARTESIAN_POINT('Ctrl Pts',(-0.234335003176676,57.0447873443258,
11.2584002982776));
#51906=CARTESIAN_POINT('Ctrl Pts',(-0.21943853560129,57.0466573321898,11.2563278666349));
#51907=CARTESIAN_POINT('Ctrl Pts',(-0.11879000273389,57.0592919741976,11.2423254057661));
#51908=CARTESIAN_POINT('Ctrl Pts',(-0.0167823939950706,57.0719792727903,
11.2360362300478));
#51909=CARTESIAN_POINT('Ctrl Pts',(0.0853667345546593,57.0847009503705,
11.2373113037582));
#51910=CARTESIAN_POINT('Ctrl Pts',(0.110531223645454,57.0878349420279,11.2376254188067));
#51911=CARTESIAN_POINT('Ctrl Pts',(0.13570428321117,57.0909710189366,11.2383983493524));
#51912=CARTESIAN_POINT('Ctrl Pts',(0.160867712219528,57.0941089055934,11.2396273856827));
#51913=CARTESIAN_POINT('Ctrl Pts',(0.17190683574445,57.0954854873939,11.240166560366));
#51914=CARTESIAN_POINT('Ctrl Pts',(0.182944465887215,57.0968624637778,11.240793529023));
#51915=CARTESIAN_POINT('Ctrl Pts',(0.193979268323433,57.0982398378226,11.241508084893));
#51916=CARTESIAN_POINT('Ctrl Pts',(0.310199306268968,57.1127465283301,11.2490338843623));
#51917=CARTESIAN_POINT('Ctrl Pts',(0.426117937433488,57.1272987039844,11.2662718750778));
#51918=CARTESIAN_POINT('Ctrl Pts',(0.540146549680601,57.1419037653696,11.2930139483905));
#51919=CARTESIAN_POINT('Ctrl Pts',(0.551276280104599,57.1433292882523,11.2956241008872));
#51920=CARTESIAN_POINT('Ctrl Pts',(0.562387996858273,57.1447553151042,11.298324835973));
#51921=CARTESIAN_POINT('Ctrl Pts',(0.573480216019194,57.1461818529016,11.3011159860358));
#51922=CARTESIAN_POINT('Ctrl Pts',(0.697527491616906,57.1621352094609,11.3323301692442));
#51923=CARTESIAN_POINT('Ctrl Pts',(0.819136344563904,57.1781526813702,11.3748562817526));
#51924=CARTESIAN_POINT('Ctrl Pts',(0.93606778237377,57.1942216481512,11.4283982508154));
#51925=CARTESIAN_POINT('Ctrl Pts',(0.99511780650718,57.2023364280084,11.4554367840321));
#51926=CARTESIAN_POINT('Ctrl Pts',(1.05297228500711,57.2104639569118,11.4852831934948));
#51927=CARTESIAN_POINT('Ctrl Pts',(1.10933041666177,57.2186004187615,11.5178839589184));
#51928=CARTESIAN_POINT('Ctrl Pts',(1.10933175267172,57.2186006116422,11.5178847317429));
#51929=CARTESIAN_POINT('Ctrl Pts',(1.10933308868084,57.2186008045229,11.517885504569));
#51930=CARTESIAN_POINT('Ctrl Pts',(1.10933442468911,57.2186009974035,11.5178862773967));
#51931=CARTESIAN_POINT('Ctrl Pts',(1.12852030193005,57.2213708791972,11.5289845440871));
#51932=CARTESIAN_POINT('Ctrl Pts',(1.14753692501207,57.2241416825675,11.5404042732587));
#51933=CARTESIAN_POINT('Ctrl Pts',(1.16637602644111,57.2269135946435,11.552137425452));
#51934=CARTESIAN_POINT('Ctrl Pts',(1.27525068865178,57.2429329887787,11.6199454887253));
#51935=CARTESIAN_POINT('Ctrl Pts',(1.37818710760162,57.258988265738,11.6982209598812));
#51936=CARTESIAN_POINT('Ctrl Pts',(1.47356521081465,57.2750817193222,11.7853567463418));
#51937=CARTESIAN_POINT('Ctrl Pts',(1.48314108575922,57.2766974874467,11.7941051001697));
#51938=CARTESIAN_POINT('Ctrl Pts',(1.49264079909951,57.2783136401906,11.8029427313062));
#51939=CARTESIAN_POINT('Ctrl Pts',(1.50206273000616,57.2799301797367,11.8118679915361));
#51940=CARTESIAN_POINT('Ctrl Pts',(1.60475210073033,57.2975488006307,11.9091441619562));
#51941=CARTESIAN_POINT('Ctrl Pts',(1.69820428117194,57.3152139186673,12.0168279148488));
#51942=CARTESIAN_POINT('Ctrl Pts',(1.78041366025471,57.3329448589268,12.1328930198129));
#51943=CARTESIAN_POINT('Ctrl Pts',(1.81839841676897,57.34113742109,12.1865207786046));
#51944=CARTESIAN_POINT('Ctrl Pts',(1.85398400347341,57.3493442200302,12.2419396266027));
#51945=CARTESIAN_POINT('Ctrl Pts',(1.88697436285143,57.3575676858942,12.2989601069398));
#51946=CARTESIAN_POINT('Ctrl Pts',(1.93596769315265,57.3697801924232,12.3836400946622));
#51947=CARTESIAN_POINT('Ctrl Pts',(1.97924341638224,57.3820318062515,12.4718732311336));
#51948=CARTESIAN_POINT('Ctrl Pts',(2.01610593080336,57.3942624585106,12.5629186579116));
#51949=CARTESIAN_POINT('Ctrl Pts',(2.01610697815278,57.3942628060118,12.5629212447231));
#51950=CARTESIAN_POINT('Ctrl Pts',(2.01610802549702,57.3942631535129,12.5629238315368));
#51951=CARTESIAN_POINT('Ctrl Pts',(2.01610907283609,57.3942635010141,12.5629264183528));
#51952=CARTESIAN_POINT('Ctrl Pts',(2.05154606796938,57.4060212937583,12.6504520235051));
#51953=CARTESIAN_POINT('Ctrl Pts',(2.08109335709301,57.4177969516692,12.74067767571));
#51954=CARTESIAN_POINT('Ctrl Pts',(2.10461089161464,57.4296087684235,12.8326815628148));
#51955=CARTESIAN_POINT('Ctrl Pts',(2.11116188035192,57.4328990401335,12.8583099477824));
#51956=CARTESIAN_POINT('Ctrl Pts',(2.11724527915549,57.4361921147007,12.8840761843313));
#51957=CARTESIAN_POINT('Ctrl Pts',(2.12285872882916,57.4394883806281,12.9099600987078));
#51958=CARTESIAN_POINT('Ctrl Pts',(2.14887168309908,57.4547634111023,13.0299072114719));
#51959=CARTESIAN_POINT('Ctrl Pts',(2.164793939548,57.4701168724529,13.1523804142498));
#51960=CARTESIAN_POINT('Ctrl Pts',(2.17046447447609,57.4855089821036,13.2756306015249));
#51961=CARTESIAN_POINT('Ctrl Pts',(2.17310856134027,57.4926860959836,13.3331003473805));
#51962=CARTESIAN_POINT('Ctrl Pts',(2.17352397983032,57.4998720476228,13.3907427526979));
#51963=CARTESIAN_POINT('Ctrl Pts',(2.17168907884137,57.507069560088,13.4483984305321));
#51964=CARTESIAN_POINT('Ctrl Pts',(2.16778234790218,57.5223939535036,13.5711544929962));
#51965=CARTESIAN_POINT('Ctrl Pts',(2.15365044376428,57.5378670458362,13.6940004938917));
#51966=CARTESIAN_POINT('Ctrl Pts',(2.12908713899266,57.5533516912026,13.8151280705915));
#51967=CARTESIAN_POINT('Ctrl Pts',(2.11820072091225,57.5602144616992,13.8688116222668));
#51968=CARTESIAN_POINT('Ctrl Pts',(2.10526733362143,57.5670735780649,13.9221527172546));
#51969=CARTESIAN_POINT('Ctrl Pts',(2.09028234147873,57.5739147073408,13.9749698748476));
#51970=CARTESIAN_POINT('Ctrl Pts',(2.09028139064532,57.5739151414267,13.9749732262219));
#51971=CARTESIAN_POINT('Ctrl Pts',(2.09028043980363,57.5739155755126,13.9749765775942));
#51972=CARTESIAN_POINT('Ctrl Pts',(2.09027948895371,57.5739160095984,13.9749799289644));
#51973=CARTESIAN_POINT('Ctrl Pts',(2.06838335284136,57.5839121206977,14.0521551533744));
#51974=CARTESIAN_POINT('Ctrl Pts',(2.04207605996703,57.5939491656667,14.128270426977));
#51975=CARTESIAN_POINT('Ctrl Pts',(2.01160877246451,57.6040107056676,14.2028291736451));
#51976=CARTESIAN_POINT('Ctrl Pts',(1.99599643373423,57.6091665361836,14.2410352793968));
#51977=CARTESIAN_POINT('Ctrl Pts',(1.97929160389414,57.6143288730566,14.2788335405652));
#51978=CARTESIAN_POINT('Ctrl Pts',(1.96152606695844,57.6194957795549,14.3161619667831));
#51979=CARTESIAN_POINT('Ctrl Pts',(1.96152459443129,57.6194962078229,14.316165060814));
#51980=CARTESIAN_POINT('Ctrl Pts',(1.96152312189686,57.6194966360909,14.3161681548417));
#51981=CARTESIAN_POINT('Ctrl Pts',(1.96152164935513,57.6194970643589,14.3161712488662));
#51982=CARTESIAN_POINT('Ctrl Pts',(1.92897574505878,57.628962582074,14.3845549307998));
#51983=CARTESIAN_POINT('Ctrl Pts',(1.89286971516756,57.6384435260741,14.4513607768799));
#51984=CARTESIAN_POINT('Ctrl Pts',(1.85339670738357,57.6479368122006,14.516286924724));
#51985=CARTESIAN_POINT('Ctrl Pts',(1.83670686721662,57.6519507304958,14.5437387732404));
#51986=CARTESIAN_POINT('Ctrl Pts',(1.81941486125606,57.6559669850194,14.5708551735042));
#51987=CARTESIAN_POINT('Ctrl Pts',(1.80153377049652,57.6599858781018,14.5976157278655));
#51988=CARTESIAN_POINT('Ctrl Pts',(1.793570187723,57.6617757458537,14.6095338984395));
#51989=CARTESIAN_POINT('Ctrl Pts',(1.78548973929216,57.663566141785,14.6213815115252));
#51990=CARTESIAN_POINT('Ctrl Pts',(1.77729365128469,57.6653567549875,14.6331567786028));
#51991=CARTESIAN_POINT('Ctrl Pts',(1.77729193427258,57.6653571301061,14.6331592454231));
#51992=CARTESIAN_POINT('Ctrl Pts',(1.77729021725538,57.6653575052246,14.6331617122403));
#51993=CARTESIAN_POINT('Ctrl Pts',(1.77728850023312,57.6653578803432,14.6331641790542));
#51994=CARTESIAN_POINT('Ctrl Pts',(1.73393580426888,57.6748291616104,14.6954481907934));
#51995=CARTESIAN_POINT('Ctrl Pts',(1.68737652870182,57.6843072213637,14.7556671002019));
#51996=CARTESIAN_POINT('Ctrl Pts',(1.63778729106415,57.6938025052366,14.8134821898953));
#51997=CARTESIAN_POINT('Ctrl Pts',(1.58822204723924,57.7032931948048,14.8712693056874));
#51998=CARTESIAN_POINT('Ctrl Pts',(1.53562822159541,57.7128009278753,14.9266541483628));
#51999=CARTESIAN_POINT('Ctrl Pts',(1.48020683297272,57.7223264388571,14.9792508401895));
#52000=CARTESIAN_POINT('Ctrl Pts',(1.42489588709152,57.7318329675727,15.0317427182794));
#52001=CARTESIAN_POINT('Ctrl Pts',(1.3667674610436,57.7413569461082,15.0814561529771));
#52002=CARTESIAN_POINT('Ctrl Pts',(1.30606647115989,57.7508925704664,15.1279763795914));
#52003=CARTESIAN_POINT('Ctrl Pts',(1.2915763606101,57.7531688472022,15.1390813587315));
#52004=CARTESIAN_POINT('Ctrl Pts',(1.27693989936916,57.7554457689097,15.1500042944493));
#52005=CARTESIAN_POINT('Ctrl Pts',(1.26216089829315,57.7577232302763,15.1607394370694));
#52006=CARTESIAN_POINT('Ctrl Pts',(1.26215807027415,57.7577236660773,15.1607414912804));
#52007=CARTESIAN_POINT('Ctrl Pts',(1.2621552422499,57.7577241018783,15.1607435454846));
#52008=CARTESIAN_POINT('Ctrl Pts',(1.26215241422026,57.7577245376793,15.1607455996821));
#52009=CARTESIAN_POINT('Ctrl Pts',(1.1821024916842,57.7700602766915,15.2188915071568));
#52010=CARTESIAN_POINT('Ctrl Pts',(1.09777583633315,57.7823787703683,15.2716098900839));
#52011=CARTESIAN_POINT('Ctrl Pts',(1.01010282620475,57.7947581127681,15.3185931659071));
#52012=CARTESIAN_POINT('Ctrl Pts',(0.98372483612274,57.7984826589035,15.3327289231016));
#52013=CARTESIAN_POINT('Ctrl Pts',(0.957044199268231,57.802212699256,15.3463457681613));
#52014=CARTESIAN_POINT('Ctrl Pts',(0.930086900172838,57.8059503238116,15.3594359711277));
#52015=CARTESIAN_POINT('Ctrl Pts',(0.850978071322352,57.8169187483645,15.3978504510958));
#52016=CARTESIAN_POINT('Ctrl Pts',(0.769463204092305,57.8279050259332,15.4317615894296));
#52017=CARTESIAN_POINT('Ctrl Pts',(0.686093571267212,57.8389144685452,15.461031010559));
#52018=CARTESIAN_POINT('Ctrl Pts',(0.598922955959961,57.8504258528964,15.491634881094));
#52019=CARTESIAN_POINT('Ctrl Pts',(0.509725733949969,57.8619623442583,15.5171631613577));
#52020=CARTESIAN_POINT('Ctrl Pts',(0.419141906685512,57.8735279509147,15.5374357709995));
#52021=CARTESIAN_POINT('Ctrl Pts',(0.316167620052189,57.8866755527648,15.5604813584857));
#52022=CARTESIAN_POINT('Ctrl Pts',(0.211405608724186,57.8998601824428,15.576733339609));
#52023=CARTESIAN_POINT('Ctrl Pts',(0.105826024951418,57.9130840446135,15.5859073055695));
#52024=CARTESIAN_POINT('Ctrl Pts',(-0.0197282419384677,57.9288097394967,
15.5968169012459));
#52025=CARTESIAN_POINT('Ctrl Pts',(-0.146439200881165,57.9445909373644,
15.5977142886005));
#52026=CARTESIAN_POINT('Ctrl Pts',(-0.27260456530094,57.9604427243888,15.5881099353691));
#52027=CARTESIAN_POINT('Ctrl Pts',(-0.307697137477017,57.9648518582492,
15.5854385091775));
#52028=CARTESIAN_POINT('Ctrl Pts',(-0.342741440753223,57.969310802562,15.5819373104183));
#52029=CARTESIAN_POINT('Ctrl Pts',(-0.377704756191395,57.9737727477083,
15.5776147022987));
#52030=CARTESIAN_POINT('Ctrl Pts',(-0.457793389572851,57.983993491494,15.5677131305339));
#52031=CARTESIAN_POINT('Ctrl Pts',(-0.537469825606877,57.9942304878195,
15.5534967718189));
#52032=CARTESIAN_POINT('Ctrl Pts',(-0.616216254675355,58.0043814023485,
15.5349138487034));
#52033=CARTESIAN_POINT('Ctrl Pts',(-0.63028710889917,58.006195224769,15.5315933476305));
#52034=CARTESIAN_POINT('Ctrl Pts',(-0.644328335635221,58.0080063032693,
15.528133545172));
#52035=CARTESIAN_POINT('Ctrl Pts',(-0.658337074143732,58.0098140600242,
15.5245342972585));
#52036=CARTESIAN_POINT('Ctrl Pts',(-0.658338275441633,58.0098142150456,
15.5245339886105));
#52037=CARTESIAN_POINT('Ctrl Pts',(-0.658339476739311,58.009814370067,15.5245336799615));
#52038=CARTESIAN_POINT('Ctrl Pts',(-0.658340678036733,58.0098145250883,
15.5245333713115));
#52039=CARTESIAN_POINT('Ctrl Pts',(-0.739222618996494,58.0202519307906,
15.5037523275969));
#52040=CARTESIAN_POINT('Ctrl Pts',(-0.819204934486232,58.0306008708064,
15.4782729641146));
#52041=CARTESIAN_POINT('Ctrl Pts',(-0.897738436735581,58.0410160411495,
15.4483462602352));
#52042=CARTESIAN_POINT('Ctrl Pts',(-0.92649322773712,58.0448295225032,15.4373886931999));
#52043=CARTESIAN_POINT('Ctrl Pts',(-0.9550535891957,58.0486518445508,15.4258353655298));
#52044=CARTESIAN_POINT('Ctrl Pts',(-0.983391973449421,58.052490464911,15.4137002333862));
#52045=CARTESIAN_POINT('Ctrl Pts',(-1.09169238759642,58.0671604676548,15.3673235654325));
#52046=CARTESIAN_POINT('Ctrl Pts',(-1.19679237425643,58.0819014253187,15.3125136141435));
#52047=CARTESIAN_POINT('Ctrl Pts',(-1.29755132669116,58.0966671351421,15.2501467519184));
#52048=CARTESIAN_POINT('Ctrl Pts',(-1.36875778954245,58.1071020785649,15.2060720215756));
#52049=CARTESIAN_POINT('Ctrl Pts',(-1.4378010898869,58.1175498179365,15.1582232951837));
#52050=CARTESIAN_POINT('Ctrl Pts',(-1.50433297279242,58.1280191132008,15.1068504820689));
#52051=CARTESIAN_POINT('Ctrl Pts',(-1.54974714864477,58.1351653774492,15.0717837761989));
#52052=CARTESIAN_POINT('Ctrl Pts',(-1.59399216625096,58.1423218737279,15.0350736355508));
#52053=CARTESIAN_POINT('Ctrl Pts',(-1.63695408575892,58.1494917037906,14.9967914350999));
#52054=CARTESIAN_POINT('Ctrl Pts',(-1.69734190352785,58.1595697076652,14.9429814896622));
#52055=CARTESIAN_POINT('Ctrl Pts',(-1.75518989077996,58.1696732263718,14.886069715756));
#52056=CARTESIAN_POINT('Ctrl Pts',(-1.81014253459797,58.1798063669947,14.8262699726838));
#52057=CARTESIAN_POINT('Ctrl Pts',(-1.87387451074958,58.1915583962265,14.7569165160608));
#52058=CARTESIAN_POINT('Ctrl Pts',(-1.93370658902649,58.2033612615372,14.6836703597443));
#52059=CARTESIAN_POINT('Ctrl Pts',(-1.98893194374559,58.2153383669724,14.6069358635697));
#52060=CARTESIAN_POINT('Ctrl Pts',(-2.00335825377246,58.2184671008142,14.5868908020721));
#52061=CARTESIAN_POINT('Ctrl Pts',(-2.01747019945016,58.221607701593,14.5666079736676));
#52062=CARTESIAN_POINT('Ctrl Pts',(-2.03125520687666,58.2247623194602,14.5460951747106));
#52063=CARTESIAN_POINT('Ctrl Pts',(-2.07642243173065,58.235098573198,14.4788840246394));
#52064=CARTESIAN_POINT('Ctrl Pts',(-2.11816673589426,58.2454008500489,14.4092448347116));
#52065=CARTESIAN_POINT('Ctrl Pts',(-2.15610926884306,58.255610553224,14.337534168832));
#52066=CARTESIAN_POINT('Ctrl Pts',(-2.17407630646753,58.260445183567,14.3035768093253));
#52067=CARTESIAN_POINT('Ctrl Pts',(-2.1911915558923,58.2652590716473,14.2691551915749));
#52068=CARTESIAN_POINT('Ctrl Pts',(-2.20741879394274,58.2700460825528,14.2343081529327));
#52069=CARTESIAN_POINT('Ctrl Pts',(-2.20742037612162,58.2700465492932,14.2343047552967));
#52070=CARTESIAN_POINT('Ctrl Pts',(-2.20742195829227,58.2700470160334,14.2343013576562));
#52071=CARTESIAN_POINT('Ctrl Pts',(-2.20742354045467,58.2700474827733,14.2342979600113));
#52072=CARTESIAN_POINT('Ctrl Pts',(-2.2423675324464,58.2803560050086,14.1592568166455));
#52073=CARTESIAN_POINT('Ctrl Pts',(-2.27329381777304,58.2905507441748,14.0820463417982));
#52074=CARTESIAN_POINT('Ctrl Pts',(-2.30006406188348,58.3007721133346,14.0031713102078));
#52075=CARTESIAN_POINT('Ctrl Pts',(-2.3323740168309,58.3131086454816,13.9079742433956));
#52076=CARTESIAN_POINT('Ctrl Pts',(-2.35852831113392,58.3256652461448,13.8103298458482));
#52077=CARTESIAN_POINT('Ctrl Pts',(-2.37856484609779,58.3382746346422,13.7111382426403));
#52078=CARTESIAN_POINT('Ctrl Pts',(-2.38226392232532,58.3406025366132,13.6928258297376));
#52079=CARTESIAN_POINT('Ctrl Pts',(-2.38575457854688,58.3429322532296,13.6744605754864));
#52080=CARTESIAN_POINT('Ctrl Pts',(-2.38903717202239,58.3452627531585,13.6560479890038));
#52081=CARTESIAN_POINT('Ctrl Pts',(-2.40987265671179,58.3600550495393,13.5391784568449));
#52082=CARTESIAN_POINT('Ctrl Pts',(-2.42232664060288,58.3748790286422,13.4204016788481));
#52083=CARTESIAN_POINT('Ctrl Pts',(-2.42634547880896,58.3897364539911,13.3010464102513));
#52084=CARTESIAN_POINT('Ctrl Pts',(-2.43027591694206,58.4042670690985,13.1843165308619));
#52085=CARTESIAN_POINT('Ctrl Pts',(-2.42614041294498,58.4188295468759,13.0670338935525));
#52086=CARTESIAN_POINT('Ctrl Pts',(-2.41387033313529,58.433431651294,12.9503879038096));
#52087=CARTESIAN_POINT('Ctrl Pts',(-2.40412122003183,58.4450336595717,12.8577075818632));
#52088=CARTESIAN_POINT('Ctrl Pts',(-2.38923682936086,58.4566606239254,12.765429212999));
#52089=CARTESIAN_POINT('Ctrl Pts',(-2.36916153037971,58.4683187763596,12.6741341540109));
#52090=CARTESIAN_POINT('Ctrl Pts',(-2.34908729832197,58.4799763092087,12.5828439469971));
#52091=CARTESIAN_POINT('Ctrl Pts',(-2.32369861772447,58.4918483155166,12.492561724561));
#52092=CARTESIAN_POINT('Ctrl Pts',(-2.29305561911638,58.5037818778372,12.4039662773282));
#52093=CARTESIAN_POINT('Ctrl Pts',(-2.28370438907306,58.507423606505,12.3769298760131));
#52094=CARTESIAN_POINT('Ctrl Pts',(-2.27386400194058,58.5110711045075,12.3500502322717));
#52095=CARTESIAN_POINT('Ctrl Pts',(-2.26353653476627,58.5147201244505,12.3233457404454));
#52096=CARTESIAN_POINT('Ctrl Pts',(-2.24107844936941,58.5226552744839,12.2652742164413));
#52097=CARTESIAN_POINT('Ctrl Pts',(-2.21634898676585,58.5305477092106,12.2080222560835));
#52098=CARTESIAN_POINT('Ctrl Pts',(-2.18939070437801,58.5383506903398,12.1518002682921));
#52099=CARTESIAN_POINT('Ctrl Pts',(-2.18938782706648,58.5383515231677,12.1517942676066));
#52100=CARTESIAN_POINT('Ctrl Pts',(-2.18938494972885,58.538352355995,12.1517882669321));
#52101=CARTESIAN_POINT('Ctrl Pts',(-2.18938207236512,58.538353188822,12.1517822662684));
#52102=CARTESIAN_POINT('Ctrl Pts',(-2.15380875524676,58.548649563825,12.077595083127));
#52103=CARTESIAN_POINT('Ctrl Pts',(-2.1142433990334,58.5588769501379,12.0050782113557));
#52104=CARTESIAN_POINT('Ctrl Pts',(-2.07099563869339,58.5690748660087,11.9346041460495));
#52105=CARTESIAN_POINT('Ctrl Pts',(-2.02764045632519,58.5792981122273,11.8639550319785));
#52106=CARTESIAN_POINT('Ctrl Pts',(-1.98058610030465,58.5894923299576,11.7953580761275));
#52107=CARTESIAN_POINT('Ctrl Pts',(-1.93012306899672,58.5997142606411,11.7291406106755));
#52108=CARTESIAN_POINT('Ctrl Pts',(-1.87972234867691,58.6099235694391,11.6630049095488));
#52109=CARTESIAN_POINT('Ctrl Pts',(-1.8258426072529,58.6203100199353,11.599323431948));
#52110=CARTESIAN_POINT('Ctrl Pts',(-1.76885646971354,58.6307171702467,11.5382756463943));
#52111=CARTESIAN_POINT('Ctrl Pts',(-1.75227196569756,58.6337459318646,11.5205090931868));
#52112=CARTESIAN_POINT('Ctrl Pts',(-1.73542377387291,58.6367765420156,11.5029650986599));
#52113=CARTESIAN_POINT('Ctrl Pts',(-1.71831766398917,58.6398093087261,11.4856494580447));
#52114=CARTESIAN_POINT('Ctrl Pts',(-0.211978292710951,66.0826669143831,
10.2439166213909));
#52115=CARTESIAN_POINT('Ctrl Pts',(0.380426698411577,66.1566886141943,10.2144267143116));
#52116=CARTESIAN_POINT('Ctrl Pts',(1.54604714045993,66.3004784630863,10.5056263688969));
#52117=CARTESIAN_POINT('Ctrl Pts',(2.75615769215105,66.5118442591118,11.7841923780606));
#52118=CARTESIAN_POINT('Ctrl Pts',(3.09938745941552,66.7171914208913,13.4595450858029));
#52119=CARTESIAN_POINT('Ctrl Pts',(2.51521498728355,66.919733558191,15.0420371329737));
#52120=CARTESIAN_POINT('Ctrl Pts',(1.20364263133209,67.1193482064331,16.0633151491819));
#52121=CARTESIAN_POINT('Ctrl Pts',(-0.425010768267335,67.3159276396824,
16.2362178374675));
#52122=CARTESIAN_POINT('Ctrl Pts',(-1.874476613348,67.5093778719358,15.5355630093087));
#52123=CARTESIAN_POINT('Ctrl Pts',(-2.82066310998034,67.7207586572874,14.0488554654566));
#52124=CARTESIAN_POINT('Ctrl Pts',(-2.65718161004858,67.9486110389564,12.101625506873));
#52125=CARTESIAN_POINT('Ctrl Pts',(-1.12386966785095,68.1912532325112,10.6893961684456));
#52126=CARTESIAN_POINT('Ctrl Pts',(0.90652387195178,68.4279099084122,10.683338398873));
#52127=CARTESIAN_POINT('Ctrl Pts',(2.37479267666757,68.6585764425755,12.0118831411098));
#52128=CARTESIAN_POINT('Ctrl Pts',(2.54915169405804,68.8832926157084,13.935283018162));
#52129=CARTESIAN_POINT('Ctrl Pts',(1.50934916221757,69.0839138557608,15.3042900857091));
#52130=CARTESIAN_POINT('Ctrl Pts',(0.0788806318954479,69.2621301783978,
15.7062194542042));
#52131=CARTESIAN_POINT('Ctrl Pts',(-1.1790274152294,69.4193887352863,15.3450857446561));
#52132=CARTESIAN_POINT('Ctrl Pts',(-2.04074624188028,69.5736038028972,14.3920281022972));
#52133=CARTESIAN_POINT('Ctrl Pts',(-2.26609286242154,69.7248824507778,13.1524725423401));
#52134=CARTESIAN_POINT('Ctrl Pts',(-1.81045081861987,69.8733436066605,12.0031498816977));
#52135=CARTESIAN_POINT('Ctrl Pts',(-0.836645778823911,70.0191227628882,
11.2782840667528));
#52136=CARTESIAN_POINT('Ctrl Pts',(0.352571010602829,70.1623683591737,11.1804871759654));
#52137=CARTESIAN_POINT('Ctrl Pts',(1.13590843302084,70.2680173733739,11.5801035007707));
#52138=CARTESIAN_POINT('Ctrl Pts',(1.51874801489704,70.3377610718551,11.9891882143963));
#52139=CARTESIAN_POINT('Ctrl Pts',(1.73313352509794,70.3840751496341,12.2931037723312));
#52140=CARTESIAN_POINT('Ctrl Pts',(1.99094615982158,70.464668067495,12.892271037609));
#52141=CARTESIAN_POINT('Ctrl Pts',(1.98017460809902,70.5785246349932,13.8401174532572));
#52142=CARTESIAN_POINT('Ctrl Pts',(1.37511235343592,70.7133250089865,14.7866139544086));
#52143=CARTESIAN_POINT('Ctrl Pts',(0.375128048534321,70.8464820657692,15.2661514257348));
#52144=CARTESIAN_POINT('Ctrl Pts',(-0.442862949154468,70.9452798994256,
15.1768702880818));
#52145=CARTESIAN_POINT('Ctrl Pts',(-1.07271986066901,71.0325888573339,14.8687929172157));
#52146=CARTESIAN_POINT('Ctrl Pts',(-1.60325302953884,71.1195156735062,14.3937214166867));
#52147=CARTESIAN_POINT('Ctrl Pts',(-1.94329386684104,71.238230764045,13.465985211871));
#52148=CARTESIAN_POINT('Ctrl Pts',(-1.70419247526824,71.3812704329662,12.297859121067));
#52149=CARTESIAN_POINT('Ctrl Pts',(-0.695068394539133,71.537828646783,11.4125559681135));
#52150=CARTESIAN_POINT('Ctrl Pts',(0.767455142864972,71.7081887803066,11.4411332113733));
#52151=CARTESIAN_POINT('Ctrl Pts',(1.82687444435982,71.8786768812991,12.451469255393));
#52152=CARTESIAN_POINT('Ctrl Pts',(1.93180306940232,72.0498248057693,13.9160723142885));
#52153=CARTESIAN_POINT('Ctrl Pts',(1.01274800143708,72.2221959240743,15.0763853677582));
#52154=CARTESIAN_POINT('Ctrl Pts',(-0.463802623258719,72.3962970524919,
15.3172652274182));
#52155=CARTESIAN_POINT('Ctrl Pts',(-1.41174851696204,72.5285808476124,14.6949935892069));
#52156=CARTESIAN_POINT('Ctrl Pts',(-1.77120197887337,72.6176272164111,14.0747773357718));
#52157=CARTESIAN_POINT('Ctrl Pts',(-1.89237232728703,72.6623344317626,13.7360097561691));
#52158=CARTESIAN_POINT('Ctrl Pts',(-1.94839182416811,72.7072228438111,13.3793116458357));
#52159=CARTESIAN_POINT('Ctrl Pts',(-1.93017702510986,72.7973993946095,12.6532690816778));
#52160=CARTESIAN_POINT('Ctrl Pts',(-1.50263901342807,72.9037786179062,11.8496624808967));
#52161=CARTESIAN_POINT('Ctrl Pts',(-0.630581690926918,73.0272027788306,
11.3457210074282));
#52162=CARTESIAN_POINT('Ctrl Pts',(0.205537810305626,73.1311361320603,11.2132845890605));
#52163=CARTESIAN_POINT('Ctrl Pts',(1.12633452278661,73.246925337271,11.4727990344487));
#52164=CARTESIAN_POINT('Ctrl Pts',(1.88802696495275,73.3751787428074,12.2092415047944));
#52165=CARTESIAN_POINT('Ctrl Pts',(2.16788213476735,73.4864771984917,13.0849137392193));
#52166=CARTESIAN_POINT('Ctrl Pts',(2.10875605441894,73.5799628212917,13.839064603789));
#52167=CARTESIAN_POINT('Ctrl Pts',(1.89824583651733,73.6548938780849,14.407528971708));
#52168=CARTESIAN_POINT('Ctrl Pts',(1.53626458253903,73.7305404812233,14.9009329211788));
#52169=CARTESIAN_POINT('Ctrl Pts',(0.886359411788144,73.8323674503564,15.4073073512682));
#52170=CARTESIAN_POINT('Ctrl Pts',(-0.155974258659698,73.9615073445991,
15.6703330193617));
#52171=CARTESIAN_POINT('Ctrl Pts',(-1.4103108874569,74.11954167518,15.2705985126791));
#52172=CARTESIAN_POINT('Ctrl Pts',(-2.28241883663609,74.2807336983208,14.250391442501));
#52173=CARTESIAN_POINT('Ctrl Pts',(-2.49025969304922,74.4451559691366,12.8970113274614));
#52174=CARTESIAN_POINT('Ctrl Pts',(-1.89750274873868,74.6266654271034,11.5063938234114));
#52175=CARTESIAN_POINT('Ctrl Pts',(-0.968179087375076,74.7550741614314,
10.9360195678874));
#52176=CARTESIAN_POINT('Ctrl Pts',(-0.399335820024005,74.8272038040824,
10.8269364066545));
#52177=CARTESIAN_POINT('Ctrl Pts',(-0.232712102076973,66.1500001422474,
10.4337952405977));
#52178=CARTESIAN_POINT('Ctrl Pts',(0.323505159358684,66.2195320956462,10.4019766084206));
#52179=CARTESIAN_POINT('Ctrl Pts',(1.41885650546918,66.3544304567715,10.6673707794366));
#52180=CARTESIAN_POINT('Ctrl Pts',(2.5601329833614,66.5522844135896,11.8558770664517));
#52181=CARTESIAN_POINT('Ctrl Pts',(2.89225673664195,66.7441284736519,13.4185171662456));
#52182=CARTESIAN_POINT('Ctrl Pts',(2.35854209488697,66.9330258398754,14.8982921253924));
#52183=CARTESIAN_POINT('Ctrl Pts',(1.14452779598673,67.1189188109853,15.858546537134));
#52184=CARTESIAN_POINT('Ctrl Pts',(-0.368886136917636,67.3017645672808,
16.0311146214169));
#52185=CARTESIAN_POINT('Ctrl Pts',(-1.7208292711234,67.4815341043535,15.3907835204228));
#52186=CARTESIAN_POINT('Ctrl Pts',(-2.61060558070679,67.6778450412109,14.0173879819278));
#52187=CARTESIAN_POINT('Ctrl Pts',(-2.47388624749099,67.8893805174368,12.2086454666814));
#52188=CARTESIAN_POINT('Ctrl Pts',(-1.06167646901042,68.1146940198439,10.8852381073462));
#52189=CARTESIAN_POINT('Ctrl Pts',(0.824939146135245,68.3346416449378,10.8626410058012));
#52190=CARTESIAN_POINT('Ctrl Pts',(2.20292293912136,68.5493585943811,12.0862717801252));
#52191=CARTESIAN_POINT('Ctrl Pts',(2.38312259731573,68.7590181212548,13.8788181919177));
#52192=CARTESIAN_POINT('Ctrl Pts',(1.42321675441193,68.9467723674098,15.1696260261314));
#52193=CARTESIAN_POINT('Ctrl Pts',(0.0841122076395244,69.114121213424,15.5607304375997));
#52194=CARTESIAN_POINT('Ctrl Pts',(-1.10435554946171,69.2622850508236,15.2329820656295));
#52195=CARTESIAN_POINT('Ctrl Pts',(-1.92886454480659,69.4081347580794,14.3406387637774));
#52196=CARTESIAN_POINT('Ctrl Pts',(-2.15589492821219,69.5518169497582,13.1659981100321));
#52197=CARTESIAN_POINT('Ctrl Pts',(-1.73368924628502,69.6934860371802,12.0645543898351));
#52198=CARTESIAN_POINT('Ctrl Pts',(-0.808056908338198,69.8333100483188,
11.3585939430159));
#52199=CARTESIAN_POINT('Ctrl Pts',(0.337496169984268,69.9714658525598,11.2505370053794));
#52200=CARTESIAN_POINT('Ctrl Pts',(1.10199168624709,70.0739639583279,11.6288124504944));
#52201=CARTESIAN_POINT('Ctrl Pts',(1.4794208139859,70.1418912017691,12.0228157110452));
#52202=CARTESIAN_POINT('Ctrl Pts',(1.69196418541103,70.1870702500522,12.31676674533));
#52203=CARTESIAN_POINT('Ctrl Pts',(1.95099988179501,70.265877979775,12.8994774417758));
#52204=CARTESIAN_POINT('Ctrl Pts',(1.95234057170264,70.3777613097285,13.8307171871858));
#52205=CARTESIAN_POINT('Ctrl Pts',(1.36616071463902,70.5111302178427,14.7747372260413));
#52206=CARTESIAN_POINT('Ctrl Pts',(0.376518429062347,70.6437980414608,15.2656471251188));
#52207=CARTESIAN_POINT('Ctrl Pts',(-0.445266890827574,70.7429376681528,
15.1871923622793));
#52208=CARTESIAN_POINT('Ctrl Pts',(-1.08393108388633,70.8309432285604,14.8848086793263));
#52209=CARTESIAN_POINT('Ctrl Pts',(-1.6268240779312,70.9188802310522,14.4115488637459));
#52210=CARTESIAN_POINT('Ctrl Pts',(-1.98597374383122,71.0397352815001,13.4721919911164));
#52211=CARTESIAN_POINT('Ctrl Pts',(-1.75776001616476,71.1863965767199,12.2715025036978));
#52212=CARTESIAN_POINT('Ctrl Pts',(-0.72856317221135,71.3482357693688,11.341204564793));
#52213=CARTESIAN_POINT('Ctrl Pts',(0.796736434165317,71.525926773327,11.3482292755109));
#52214=CARTESIAN_POINT('Ctrl Pts',(1.92658702317335,71.7052519183896,12.3940355331555));
#52215=CARTESIAN_POINT('Ctrl Pts',(2.06063201142701,71.8866716744668,13.9443662779092));
#52216=CARTESIAN_POINT('Ctrl Pts',(1.09800003567519,72.0706593400645,15.1968247724198));
#52217=CARTESIAN_POINT('Ctrl Pts',(-0.483584678898562,72.2576289765107,
15.4781733998579));
#52218=CARTESIAN_POINT('Ctrl Pts',(-1.51594107605642,72.400417605289,14.8209080799252));
#52219=CARTESIAN_POINT('Ctrl Pts',(-1.91364046970523,72.4967881402075,14.1549274787836));
#52220=CARTESIAN_POINT('Ctrl Pts',(-2.04964515460577,72.5452183807088,13.7897650560395));
#52221=CARTESIAN_POINT('Ctrl Pts',(-2.11538726758662,72.593891541241,13.403882027485));
#52222=CARTESIAN_POINT('Ctrl Pts',(-2.10583383941686,72.6917508546746,12.6159577385697));
#52223=CARTESIAN_POINT('Ctrl Pts',(-1.65259506466878,72.8074223333838,11.7362211740724));
#52224=CARTESIAN_POINT('Ctrl Pts',(-0.709990601959533,72.9418458825809,
11.1754511852134));
#52225=CARTESIAN_POINT('Ctrl Pts',(0.199383467279647,73.055138674421,11.0197089552784));
#52226=CARTESIAN_POINT('Ctrl Pts',(1.20709847264826,73.1814449840387,11.2902860435783));
#52227=CARTESIAN_POINT('Ctrl Pts',(2.04790744246493,73.3214054143136,12.0836804919538));
#52228=CARTESIAN_POINT('Ctrl Pts',(2.36463705500525,73.4428655296851,13.0354647113357));
#52229=CARTESIAN_POINT('Ctrl Pts',(2.30982205012451,73.5448575784662,13.8588149816474));
#52230=CARTESIAN_POINT('Ctrl Pts',(2.08749320339945,73.6265834298673,14.4813690786832));
#52231=CARTESIAN_POINT('Ctrl Pts',(1.69914608640829,73.7090528163163,15.0237069822103));
#52232=CARTESIAN_POINT('Ctrl Pts',(0.997414939924506,73.8200083024837,15.5834484621141));
#52233=CARTESIAN_POINT('Ctrl Pts',(-0.133920474939632,73.9605915715644,
15.8823022870827));
#52234=CARTESIAN_POINT('Ctrl Pts',(-1.50164951944074,74.1323493045711,15.4626328954726));
#52235=CARTESIAN_POINT('Ctrl Pts',(-2.45908764564237,74.3071896509351,14.3661585846542));
#52236=CARTESIAN_POINT('Ctrl Pts',(-2.6989717800723,74.4851213923391,12.9040951113791));
#52237=CARTESIAN_POINT('Ctrl Pts',(-2.07424714095716,74.681031593353,11.3969787136035));
#52238=CARTESIAN_POINT('Ctrl Pts',(-1.08029539867703,74.8191821549513,10.7738526892301));
#52239=CARTESIAN_POINT('Ctrl Pts',(-0.470844590569356,74.8966283641617,
10.6507068346715));
#52240=CARTESIAN_POINT('Ctrl Pts',(-0.253445911442996,66.2173333701116,
10.6236738598046));
#52241=CARTESIAN_POINT('Ctrl Pts',(0.266583620305798,66.2823755770983,10.5895265025299));
#52242=CARTESIAN_POINT('Ctrl Pts',(1.29166587047844,66.4083824504568,10.8291151899761));
#52243=CARTESIAN_POINT('Ctrl Pts',(2.36410827457176,66.5927245680674,11.9275617548428));
#52244=CARTESIAN_POINT('Ctrl Pts',(2.68512601386841,66.7710655264124,13.3774892466885));
#52245=CARTESIAN_POINT('Ctrl Pts',(2.2018692024904,66.9463181215596,14.7545471178109));
#52246=CARTESIAN_POINT('Ctrl Pts',(1.08541296064137,67.1184894155377,15.6537779250861));
#52247=CARTESIAN_POINT('Ctrl Pts',(-0.312761505567944,67.2876014948792,
15.8260114053663));
#52248=CARTESIAN_POINT('Ctrl Pts',(-1.56718192889881,67.4536903367711,15.246004031537));
#52249=CARTESIAN_POINT('Ctrl Pts',(-2.40054805143325,67.6349314251346,13.985920498399));
#52250=CARTESIAN_POINT('Ctrl Pts',(-2.2905908849334,67.8301499959172,12.31566542649));
#52251=CARTESIAN_POINT('Ctrl Pts',(-0.999483270169913,68.0381348071765,
11.0810800462465));
#52252=CARTESIAN_POINT('Ctrl Pts',(0.74335442031871,68.2413733814635,11.0419436127296));
#52253=CARTESIAN_POINT('Ctrl Pts',(2.03105320157515,68.4401407461865,12.1606604191405));
#52254=CARTESIAN_POINT('Ctrl Pts',(2.21709350057343,68.6347436268011,13.8223533656732));
#52255=CARTESIAN_POINT('Ctrl Pts',(1.3370843466063,68.8096308790588,15.0349619665538));
#52256=CARTESIAN_POINT('Ctrl Pts',(0.0893437833835981,68.9661122484503,
15.4152414209954));
#52257=CARTESIAN_POINT('Ctrl Pts',(-1.02968368369404,69.1051813663608,15.1208783866031));
#52258=CARTESIAN_POINT('Ctrl Pts',(-1.81698284773289,69.2426657132616,14.2892494252577));
#52259=CARTESIAN_POINT('Ctrl Pts',(-2.04569699400286,69.3787514487384,13.1795236777241));
#52260=CARTESIAN_POINT('Ctrl Pts',(-1.65692767395016,69.5136284676997,12.1259588979727));
#52261=CARTESIAN_POINT('Ctrl Pts',(-0.779468037852491,69.6474973337496,
11.4389038192792));
#52262=CARTESIAN_POINT('Ctrl Pts',(0.322421329365702,69.7805633459459,11.3205868347935));
#52263=CARTESIAN_POINT('Ctrl Pts',(1.06807493947333,69.8799105432819,11.677521400218));
#52264=CARTESIAN_POINT('Ctrl Pts',(1.44009361307476,69.9460213316832,12.0564432076942));
#52265=CARTESIAN_POINT('Ctrl Pts',(1.65079484572412,69.9900653504704,12.3404297183289));
#52266=CARTESIAN_POINT('Ctrl Pts',(1.91105360376844,70.0670878920549,12.9066838459426));
#52267=CARTESIAN_POINT('Ctrl Pts',(1.92450653530627,70.1769979844637,13.8213169211144));
#52268=CARTESIAN_POINT('Ctrl Pts',(1.35720907584211,70.3089354266989,14.7628604976741));
#52269=CARTESIAN_POINT('Ctrl Pts',(0.377908809590368,70.4411140171526,15.2651428245026));
#52270=CARTESIAN_POINT('Ctrl Pts',(-0.447670832500686,70.54059543688,15.1975144364766));
#52271=CARTESIAN_POINT('Ctrl Pts',(-1.09514230710363,70.6292975997868,14.9008244414368));
#52272=CARTESIAN_POINT('Ctrl Pts',(-1.65039512632356,70.7182447885983,14.4293763108051));
#52273=CARTESIAN_POINT('Ctrl Pts',(-2.0286536208214,70.8412397989554,13.4783987703618));
#52274=CARTESIAN_POINT('Ctrl Pts',(-1.81132755706128,70.9915227204736,12.2451458863287));
#52275=CARTESIAN_POINT('Ctrl Pts',(-0.762057949883573,71.1586428919545,
11.2698531614724));
#52276=CARTESIAN_POINT('Ctrl Pts',(0.826017725465654,71.3436647663474,11.2553253396486));
#52277=CARTESIAN_POINT('Ctrl Pts',(2.0262996019869,71.5318269554803,12.3366018109182));
#52278=CARTESIAN_POINT('Ctrl Pts',(2.1894609534517,71.7235185431642,13.9726602415297));
#52279=CARTESIAN_POINT('Ctrl Pts',(1.18325206991327,71.9191227560546,15.3172641770814));
#52280=CARTESIAN_POINT('Ctrl Pts',(-0.503366734538406,72.1189609005295,
15.6390815722975));
#52281=CARTESIAN_POINT('Ctrl Pts',(-1.6201336351508,72.2722543629655,14.9468225706433));
#52282=CARTESIAN_POINT('Ctrl Pts',(-2.0560789605371,72.3759490640039,14.2350776217954));
#52283=CARTESIAN_POINT('Ctrl Pts',(-2.20691798192451,72.4281023296549,13.84352035591));
#52284=CARTESIAN_POINT('Ctrl Pts',(-2.28238271100513,72.4805602386708,13.4284524091344));
#52285=CARTESIAN_POINT('Ctrl Pts',(-2.28149065372387,72.5861023147396,12.5786463954616));
#52286=CARTESIAN_POINT('Ctrl Pts',(-1.80255111590949,72.7110660488616,11.6227798672479));
#52287=CARTESIAN_POINT('Ctrl Pts',(-0.789399512992146,72.8564889863311,
11.0051813629984));
#52288=CARTESIAN_POINT('Ctrl Pts',(0.193229124253671,72.9791412167817,10.8261333214963));
#52289=CARTESIAN_POINT('Ctrl Pts',(1.28786242250991,73.1159646308063,11.1077730527079));
#52290=CARTESIAN_POINT('Ctrl Pts',(2.20778791997711,73.2676320858199,11.9581194791132));
#52291=CARTESIAN_POINT('Ctrl Pts',(2.56139197524314,73.3992538608785,12.9860156834522));
#52292=CARTESIAN_POINT('Ctrl Pts',(2.51088804583008,73.5097523356408,13.8785653595058));
#52293=CARTESIAN_POINT('Ctrl Pts',(2.27674057028156,73.5982729816497,14.5552091856582));
#52294=CARTESIAN_POINT('Ctrl Pts',(1.86202759027756,73.6875651514094,15.1464810432419));
#52295=CARTESIAN_POINT('Ctrl Pts',(1.10847046806087,73.8076491546109,15.7595895729601));
#52296=CARTESIAN_POINT('Ctrl Pts',(-0.111866691219567,73.9596757985298,
16.0942715548037));
#52297=CARTESIAN_POINT('Ctrl Pts',(-1.59298815142457,74.1451569339621,15.6546672782663));
#52298=CARTESIAN_POINT('Ctrl Pts',(-2.63575645464866,74.3336456035494,14.4819257268073));
#52299=CARTESIAN_POINT('Ctrl Pts',(-2.90768386709537,74.5250868155417,12.911178895297));
#52300=CARTESIAN_POINT('Ctrl Pts',(-2.25099153317564,74.7353977596027,11.2875636037955));
#52301=CARTESIAN_POINT('Ctrl Pts',(-1.19241170997896,74.8832901484711,10.6116858105728));
#52302=CARTESIAN_POINT('Ctrl Pts',(-0.542353361114717,74.9660529242413,
10.4744772626884));
#52303=CARTESIAN_POINT('Ctrl Pts',(-0.274179720809018,66.2846665979758,
10.8135524790114));
#52304=CARTESIAN_POINT('Ctrl Pts',(0.209662081252906,66.3452190585503,10.7770763966391));
#52305=CARTESIAN_POINT('Ctrl Pts',(1.1644752354877,66.462334444142,10.9908596005156));
#52306=CARTESIAN_POINT('Ctrl Pts',(2.1680835657821,66.6331647225451,11.9992464432339));
#52307=CARTESIAN_POINT('Ctrl Pts',(2.47799529109485,66.7980025791729,13.3364613271311));
#52308=CARTESIAN_POINT('Ctrl Pts',(2.04519631009381,66.9596104032439,14.6108021102295));
#52309=CARTESIAN_POINT('Ctrl Pts',(1.026298125296,67.11806002009,15.4490093130383));
#52310=CARTESIAN_POINT('Ctrl Pts',(-0.256636874218245,67.2734384224776,
15.6209081893157));
#52311=CARTESIAN_POINT('Ctrl Pts',(-1.41353458667422,67.4258465691887,15.101224542651));
#52312=CARTESIAN_POINT('Ctrl Pts',(-2.1904905221597,67.5920178090584,13.9544530148703));
#52313=CARTESIAN_POINT('Ctrl Pts',(-2.10729552237581,67.7709194743977,12.4226853862984));
#52314=CARTESIAN_POINT('Ctrl Pts',(-0.937290071329389,67.9615755945092,
11.276921985147));
#52315=CARTESIAN_POINT('Ctrl Pts',(0.661769694502177,68.1481051179891,11.2212462196578));
#52316=CARTESIAN_POINT('Ctrl Pts',(1.85918346402893,68.330922897992,12.2350490581559));
#52317=CARTESIAN_POINT('Ctrl Pts',(2.05106440383111,68.5104691323476,13.765888539429));
#52318=CARTESIAN_POINT('Ctrl Pts',(1.25095193880067,68.6724893907078,14.9002979069763));
#52319=CARTESIAN_POINT('Ctrl Pts',(0.094575359127677,68.8181032834765,15.2697524043909));
#52320=CARTESIAN_POINT('Ctrl Pts',(-0.95501181792635,68.9480776818981,15.0087747075765));
#52321=CARTESIAN_POINT('Ctrl Pts',(-1.70510115065919,69.0771966684437,14.237860086738));
#52322=CARTESIAN_POINT('Ctrl Pts',(-1.93549905979351,69.2056859477188,13.1930492454163));
#52323=CARTESIAN_POINT('Ctrl Pts',(-1.58016610161529,69.3337708982194,12.1873634061102));
#52324=CARTESIAN_POINT('Ctrl Pts',(-0.750879167366774,69.4616846191802,
11.5192136955424));
#52325=CARTESIAN_POINT('Ctrl Pts',(0.307346488747144,69.589660839332,11.3906366642075));
#52326=CARTESIAN_POINT('Ctrl Pts',(1.03415819269958,69.6858571282358,11.7262303499418));
#52327=CARTESIAN_POINT('Ctrl Pts',(1.40076641216363,69.7501514615973,12.0900707043431));
#52328=CARTESIAN_POINT('Ctrl Pts',(1.60962550603721,69.7930604508885,12.3640926913277));
#52329=CARTESIAN_POINT('Ctrl Pts',(1.87110732574187,69.8682978043347,12.9138902501093));
#52330=CARTESIAN_POINT('Ctrl Pts',(1.89667249890989,69.9762346591989,13.8119166550429));
#52331=CARTESIAN_POINT('Ctrl Pts',(1.34825743704521,70.1067406355551,14.7509837693068));
#52332=CARTESIAN_POINT('Ctrl Pts',(0.379299190118395,70.2384299928442,15.2646385238866));
#52333=CARTESIAN_POINT('Ctrl Pts',(-0.450074774173788,70.3382532056071,
15.2078365106741));
#52334=CARTESIAN_POINT('Ctrl Pts',(-1.10635353032094,70.4276519710131,14.9168402035474));
#52335=CARTESIAN_POINT('Ctrl Pts',(-1.67396617471592,70.5176093461441,14.4472037578643));
#52336=CARTESIAN_POINT('Ctrl Pts',(-2.07133349781158,70.6427443164105,13.4846055496071));
#52337=CARTESIAN_POINT('Ctrl Pts',(-1.8648950979578,70.7966488642273,12.2187892689594));
#52338=CARTESIAN_POINT('Ctrl Pts',(-0.79555272755579,70.9690500145402,11.1985017581518));
#52339=CARTESIAN_POINT('Ctrl Pts',(0.855299016765999,71.1614027593676,11.1624214037862));
#52340=CARTESIAN_POINT('Ctrl Pts',(2.12601218080043,71.3584019925708,12.2791680886806));
#52341=CARTESIAN_POINT('Ctrl Pts',(2.31828989547639,71.5603654118617,14.0009542051504));
#52342=CARTESIAN_POINT('Ctrl Pts',(1.26850410415137,71.7675861720447,15.4377035817429));
#52343=CARTESIAN_POINT('Ctrl Pts',(-0.523148790178248,71.9802928245481,
15.7999897447371));
#52344=CARTESIAN_POINT('Ctrl Pts',(-1.72432619424518,72.1440911206419,15.0727370613615));
#52345=CARTESIAN_POINT('Ctrl Pts',(-2.19851745136895,72.2551099878002,14.3152277648071));
#52346=CARTESIAN_POINT('Ctrl Pts',(-2.36419080924325,72.3109862786011,13.8972756557804));
#52347=CARTESIAN_POINT('Ctrl Pts',(-2.44937815442366,72.3672289361006,13.4530227907838));
#52348=CARTESIAN_POINT('Ctrl Pts',(-2.45714746803088,72.4804537748047,12.5413350523533));
#52349=CARTESIAN_POINT('Ctrl Pts',(-1.9525071671502,72.6147097643392,11.5093385604234));
#52350=CARTESIAN_POINT('Ctrl Pts',(-0.868808424024757,72.7711320900814,
10.8349115407836));
#52351=CARTESIAN_POINT('Ctrl Pts',(0.187074781227695,72.9031437591424,10.6325576877142));
#52352=CARTESIAN_POINT('Ctrl Pts',(1.36862637237156,73.0504842775738,10.9252600618375));
#52353=CARTESIAN_POINT('Ctrl Pts',(2.36766839748931,73.2138587573261,11.8325584662726));
#52354=CARTESIAN_POINT('Ctrl Pts',(2.75814689548104,73.355642192072,12.9365666555686));
#52355=CARTESIAN_POINT('Ctrl Pts',(2.71195404153565,73.4746470928152,13.8983157373642));
#52356=CARTESIAN_POINT('Ctrl Pts',(2.46598793716368,73.5699625334321,14.6290492926334));
#52357=CARTESIAN_POINT('Ctrl Pts',(2.02490909414682,73.6660774865024,15.2692551042736));
#52358=CARTESIAN_POINT('Ctrl Pts',(1.21952599619723,73.795290006738,15.935730683806));
#52359=CARTESIAN_POINT('Ctrl Pts',(-0.0898129074995017,73.9587600254952,
16.3062408225249));
#52360=CARTESIAN_POINT('Ctrl Pts',(-1.68432678340842,74.1579645633531,15.8467016610598));
#52361=CARTESIAN_POINT('Ctrl Pts',(-2.81242526365495,74.3601015561637,14.5976928689606));
#52362=CARTESIAN_POINT('Ctrl Pts',(-3.11639595411845,74.5650522387442,12.9182626792148));
#52363=CARTESIAN_POINT('Ctrl Pts',(-2.42773592539411,74.7897639258524,11.1781484939875));
#52364=CARTESIAN_POINT('Ctrl Pts',(-1.30452802128091,74.947398141991,10.4495189319157));
#52365=CARTESIAN_POINT('Ctrl Pts',(-0.613862131660059,75.0354774843205,
10.2982476907052));
#52366=CARTESIAN_POINT('Ctrl Pts',(-0.20632980674377,66.2927243572952,10.8082436938974));
#52367=CARTESIAN_POINT('Ctrl Pts',(-0.128574527433418,66.3024089395535,
10.8044812541815));
#52368=CARTESIAN_POINT('Ctrl Pts',(-0.0506754578630011,66.3120240875613,
10.804265682262));
#52369=CARTESIAN_POINT('Ctrl Pts',(0.0269800873958463,66.3216036971303,
10.8076269268464));
#52370=CARTESIAN_POINT('Ctrl Pts',(0.0605881294274984,66.3257495945027,
10.8090816181875));
#52371=CARTESIAN_POINT('Ctrl Pts',(0.0941500065403234,66.329888771884,10.811205889199));
#52372=CARTESIAN_POINT('Ctrl Pts',(0.127631933618099,66.3340236840922,10.8140003326875));
#52373=CARTESIAN_POINT('Ctrl Pts',(0.207592087260993,66.3438985104337,10.8206739070658));
#52374=CARTESIAN_POINT('Ctrl Pts',(0.28709887183089,66.353750182809,10.8311726784691));
#52375=CARTESIAN_POINT('Ctrl Pts',(0.365733082267086,66.3636214504582,10.8455067276754));
#52376=CARTESIAN_POINT('Ctrl Pts',(0.395837834971989,66.3674006207432,10.8509944537456));
#52377=CARTESIAN_POINT('Ctrl Pts',(0.425814190594611,66.371182595206,10.8570441252314));
#52378=CARTESIAN_POINT('Ctrl Pts',(0.455636808229107,66.3749695193208,10.8636554465057));
#52379=CARTESIAN_POINT('Ctrl Pts',(0.517293924456777,66.3827988394413,10.8773240992452));
#52380=CARTESIAN_POINT('Ctrl Pts',(0.578298801727241,66.3906500383086,10.8933946452472));
#52381=CARTESIAN_POINT('Ctrl Pts',(0.63844465679772,66.3985429049582,10.9118645401074));
#52382=CARTESIAN_POINT('Ctrl Pts',(0.708879361742415,66.4077859647333,10.9334939872791));
#52383=CARTESIAN_POINT('Ctrl Pts',(0.778141127474599,66.4170876831115,10.9584175255254));
#52384=CARTESIAN_POINT('Ctrl Pts',(0.845994629726718,66.4264002712149,10.9864050187958));
#52385=CARTESIAN_POINT('Ctrl Pts',(0.880948989604227,66.4311975999475,11.0008226225948));
#52386=CARTESIAN_POINT('Ctrl Pts',(0.91553040598333,66.4359979173664,11.0160536611649));
#52387=CARTESIAN_POINT('Ctrl Pts',(0.949711354512664,66.4407953576399,11.0320693502863));
#52388=CARTESIAN_POINT('Ctrl Pts',(1.00559245745332,66.4486385060986,11.0582527773404));
#52389=CARTESIAN_POINT('Ctrl Pts',(1.0603979421282,66.4564726611815,11.0865296427796));
#52390=CARTESIAN_POINT('Ctrl Pts',(1.11399609828178,66.4642684761698,11.1167611542193));
#52391=CARTESIAN_POINT('Ctrl Pts',(1.11400306933225,66.4642694901043,11.1167650861716));
#52392=CARTESIAN_POINT('Ctrl Pts',(1.11401004036335,66.4642705040378,11.1167690181557));
#52393=CARTESIAN_POINT('Ctrl Pts',(1.11401701137518,66.4642715179701,11.1167729501718));
#52394=CARTESIAN_POINT('Ctrl Pts',(1.17827799662113,66.4736182663468,11.1530195143464));
#52395=CARTESIAN_POINT('Ctrl Pts',(1.24090219464405,66.4828754714546,11.1919803961549));
#52396=CARTESIAN_POINT('Ctrl Pts',(1.30162376134801,66.492087325675,11.2335589286607));
#52397=CARTESIAN_POINT('Ctrl Pts',(1.33696003876224,66.4974480673998,11.2577551185624));
#52398=CARTESIAN_POINT('Ctrl Pts',(1.37165114866207,66.5027933319895,11.2828372815448));
#52399=CARTESIAN_POINT('Ctrl Pts',(1.40563841799055,66.5081308304738,11.3087812985492));
#52400=CARTESIAN_POINT('Ctrl Pts',(1.49914029805756,66.5228147445684,11.3801555046663));
#52401=CARTESIAN_POINT('Ctrl Pts',(1.58726120625653,66.5374568742704,11.4580964528296));
#52402=CARTESIAN_POINT('Ctrl Pts',(1.6691858726033,66.552055734798,11.5416423539517));
#52403=CARTESIAN_POINT('Ctrl Pts',(1.72792555617097,66.5625230639442,11.6015444568728));
#52404=CARTESIAN_POINT('Ctrl Pts',(1.783478182354,66.5729676196947,11.6643239448273));
#52405=CARTESIAN_POINT('Ctrl Pts',(1.83566700012392,66.5833648758533,11.7295897058178));
#52406=CARTESIAN_POINT('Ctrl Pts',(1.85446199222063,66.5871092861634,11.7530941558977));
#52407=CARTESIAN_POINT('Ctrl Pts',(1.87282091500671,66.5908476195423,11.776921509298));
#52408=CARTESIAN_POINT('Ctrl Pts',(1.89073609827162,66.5945789255838,11.8010550384089));
#52409=CARTESIAN_POINT('Ctrl Pts',(1.94243923882681,66.6053474585016,11.8707042978814));
#52410=CARTESIAN_POINT('Ctrl Pts',(1.99041327308698,66.6160671105291,11.9429260565201));
#52411=CARTESIAN_POINT('Ctrl Pts',(2.03423646585349,66.6267693105913,12.01742935282));
#52412=CARTESIAN_POINT('Ctrl Pts',(2.04177936952561,66.6286113868768,12.0302529549304));
#52413=CARTESIAN_POINT('Ctrl Pts',(2.04919921354728,66.6304529315439,12.0431440616382));
#52414=CARTESIAN_POINT('Ctrl Pts',(2.05649374231333,66.6322940866312,12.0561010755627));
#52415=CARTESIAN_POINT('Ctrl Pts',(2.05651131612243,66.6322985222993,12.0561322912994));
#52416=CARTESIAN_POINT('Ctrl Pts',(2.0565288892047,66.6323029579623,12.0561635074063));
#52417=CARTESIAN_POINT('Ctrl Pts',(2.05654646156012,66.6323073936202,12.0561947238834));
#52418=CARTESIAN_POINT('Ctrl Pts',(2.08973882214424,66.640685892394,12.1151594180502));
#52419=CARTESIAN_POINT('Ctrl Pts',(2.12033951567111,66.6490469766174,12.1754488244082));
#52420=CARTESIAN_POINT('Ctrl Pts',(2.14816376735373,66.6574225110525,12.2368725263844));
#52421=CARTESIAN_POINT('Ctrl Pts',(2.1588245023618,66.6606315588351,12.2604067373832));
#52422=CARTESIAN_POINT('Ctrl Pts',(2.16907744849476,66.6638426595896,12.2841069643975));
#52423=CARTESIAN_POINT('Ctrl Pts',(2.17891157135012,66.6670573505497,12.3079605868637));
#52424=CARTESIAN_POINT('Ctrl Pts',(2.21103541485258,66.6775583612481,12.3858800969552));
#52425=CARTESIAN_POINT('Ctrl Pts',(2.23869378441463,66.6881003976164,12.4654516961015));
#52426=CARTESIAN_POINT('Ctrl Pts',(2.26192857755125,66.6986571054894,12.5461589481352));
#52427=CARTESIAN_POINT('Ctrl Pts',(2.26945233491085,66.7020755180436,12.5722931072771));
#52428=CARTESIAN_POINT('Ctrl Pts',(2.2765122979034,66.7054955185458,12.5985467504864));
#52429=CARTESIAN_POINT('Ctrl Pts',(2.28310993093245,66.708916354768,12.6249035025459));
#52430=CARTESIAN_POINT('Ctrl Pts',(2.29772380927258,66.7164935698316,12.6832841924605));
#52431=CARTESIAN_POINT('Ctrl Pts',(2.31006995575646,66.7240742115067,12.7421670091656));
#52432=CARTESIAN_POINT('Ctrl Pts',(2.32029033489198,66.7316277682419,12.8013610671194));
#52433=CARTESIAN_POINT('Ctrl Pts',(2.32913573241391,66.7381651198549,12.8525915514874));
#52434=CARTESIAN_POINT('Ctrl Pts',(2.33638929861048,66.7446822853669,12.9040559349618));
#52435=CARTESIAN_POINT('Ctrl Pts',(2.34214460101437,66.7511634606035,12.9556617412829));
#52436=CARTESIAN_POINT('Ctrl Pts',(2.35154000132738,66.7617438318113,13.0399070467136));
#52437=CARTESIAN_POINT('Ctrl Pts',(2.35643489871645,66.7723064011337,13.1245139713782));
#52438=CARTESIAN_POINT('Ctrl Pts',(2.35674260359262,66.7828379873103,13.2088734477217));
#52439=CARTESIAN_POINT('Ctrl Pts',(2.35683598286597,66.7860340103197,13.234474038453));
#52440=CARTESIAN_POINT('Ctrl Pts',(2.35650726928768,66.7892271781399,13.2600518228344));
#52441=CARTESIAN_POINT('Ctrl Pts',(2.35575499732339,66.7924171175958,13.2855897940599));
#52442=CARTESIAN_POINT('Ctrl Pts',(2.3553580237854,66.7941004470457,13.299066168658));
#52443=CARTESIAN_POINT('Ctrl Pts',(2.35484311653384,66.7957828491342,13.312531230463));
#52444=CARTESIAN_POINT('Ctrl Pts',(2.35421017337586,66.7974642404135,13.3259823103315));
#52445=CARTESIAN_POINT('Ctrl Pts',(2.35420420852186,66.7974800858387,13.3261090732589));
#52446=CARTESIAN_POINT('Ctrl Pts',(2.35419823318525,66.7974959311742,13.3262358349446));
#52447=CARTESIAN_POINT('Ctrl Pts',(2.35419224736687,66.7975117764198,13.3263625953865));
#52448=CARTESIAN_POINT('Ctrl Pts',(2.3498557505447,66.8089910517747,13.4181956947107));
#52449=CARTESIAN_POINT('Ctrl Pts',(2.34000021559603,66.8204583206326,13.5096570933105));
#52450=CARTESIAN_POINT('Ctrl Pts',(2.32488075766611,66.8318982230755,13.6000526938134));
#52451=CARTESIAN_POINT('Ctrl Pts',(2.31622785363271,66.8384453081924,13.6517863247291));
#52452=CARTESIAN_POINT('Ctrl Pts',(2.30585184672865,66.8449834475544,13.7031710052325));
#52453=CARTESIAN_POINT('Ctrl Pts',(2.29380786495925,66.8515099027997,13.7540788498824));
#52454=CARTESIAN_POINT('Ctrl Pts',(2.27850022461253,66.859804886265,13.818781619419));
#52455=CARTESIAN_POINT('Ctrl Pts',(2.26070184706353,66.8680569366806,13.8827974598016));
#52456=CARTESIAN_POINT('Ctrl Pts',(2.240352918434,66.8762889633602,13.9458858798222));
#52457=CARTESIAN_POINT('Ctrl Pts',(2.21999116305402,66.8845261790181,14.0090140670184));
#52458=CARTESIAN_POINT('Ctrl Pts',(2.19707493853215,66.8927433465053,14.0712134292098));
#52459=CARTESIAN_POINT('Ctrl Pts',(2.171560354261,66.9009568640359,14.1321939171343));
#52460=CARTESIAN_POINT('Ctrl Pts',(2.162848206583,66.9037614316872,14.1530161657208));
#52461=CARTESIAN_POINT('Ctrl Pts',(2.15383329251866,66.906565517488,14.1736958976251));
#52462=CARTESIAN_POINT('Ctrl Pts',(2.14451451176516,66.9093695990993,14.1942203440636));
#52463=CARTESIAN_POINT('Ctrl Pts',(2.12491521274497,66.9152671553818,14.2373874464574));
#52464=CARTESIAN_POINT('Ctrl Pts',(2.10396974110037,66.9211653741846,14.2798728753076));
#52465=CARTESIAN_POINT('Ctrl Pts',(2.08168992125604,66.9270668759013,14.3215809602485));
#52466=CARTESIAN_POINT('Ctrl Pts',(2.05028777690612,66.9353847083651,14.3803661440168));
#52467=CARTESIAN_POINT('Ctrl Pts',(2.01623275577107,66.9437095392524,14.4376089298039));
#52468=CARTESIAN_POINT('Ctrl Pts',(1.97974060707564,66.9520291918567,14.4931656805495));
#52469=CARTESIAN_POINT('Ctrl Pts',(1.96959382145095,66.9543425040201,14.5086134538369));
#52470=CARTESIAN_POINT('Ctrl Pts',(1.95925840028277,66.9566554544955,14.5239310965515));
#52471=CARTESIAN_POINT('Ctrl Pts',(1.94873846627286,66.9589678709832,14.5391160110685));
#52472=CARTESIAN_POINT('Ctrl Pts',(1.94872104198101,66.9589717010661,14.5391411620231));
#52473=CARTESIAN_POINT('Ctrl Pts',(1.94870361719158,66.9589755311455,14.5391663125967));
#52474=CARTESIAN_POINT('Ctrl Pts',(1.94868619190455,66.9589793612212,14.5391914627893));
#52475=CARTESIAN_POINT('Ctrl Pts',(1.89403693194997,66.970991261193,14.6180676049373));
#52476=CARTESIAN_POINT('Ctrl Pts',(1.83449757953572,66.9829673125227,14.6931949198015));
#52477=CARTESIAN_POINT('Ctrl Pts',(1.77072151982188,66.9949079017398,14.7642457570623));
#52478=CARTESIAN_POINT('Ctrl Pts',(1.75846157446336,66.9972032923928,14.7779041640947));
#52479=CARTESIAN_POINT('Ctrl Pts',(1.74604492160895,66.9994973882052,14.7914119831457));
#52480=CARTESIAN_POINT('Ctrl Pts',(1.73347599386595,67.0017902142481,14.8047669541893));
#52481=CARTESIAN_POINT('Ctrl Pts',(1.67720405971062,67.0120553505235,14.8645580570246));
#52482=CARTESIAN_POINT('Ctrl Pts',(1.61794709446245,67.0222902773526,14.9213753155833));
#52483=CARTESIAN_POINT('Ctrl Pts',(1.5559915757977,67.0325046651358,14.9748663003062));
#52484=CARTESIAN_POINT('Ctrl Pts',(1.52958317353144,67.0368585252485,14.9976667137742));
#52485=CARTESIAN_POINT('Ctrl Pts',(1.50268493007333,67.0412085746359,15.0198623253546));
#52486=CARTESIAN_POINT('Ctrl Pts',(1.47532121336855,67.0455552096023,15.0414239960638));
#52487=CARTESIAN_POINT('Ctrl Pts',(1.40606940945473,67.0565556272586,15.0959920435303));
#52488=CARTESIAN_POINT('Ctrl Pts',(1.33384075616785,67.0675334930611,15.1464966187475));
#52489=CARTESIAN_POINT('Ctrl Pts',(1.25917508646185,67.078486108812,15.19268924909));
#52490=CARTESIAN_POINT('Ctrl Pts',(1.23426236182438,67.0821405259134,15.2081017443443));
#52491=CARTESIAN_POINT('Ctrl Pts',(1.20907797401137,67.0857921854888,15.2230344376171));
#52492=CARTESIAN_POINT('Ctrl Pts',(1.18364085068563,67.089441147962,15.2374787195179));
#52493=CARTESIAN_POINT('Ctrl Pts',(1.11822926315564,67.0988244585334,15.2746222045638));
#52494=CARTESIAN_POINT('Ctrl Pts',(1.05119792189493,67.1081888260333,15.3086733309431));
#52495=CARTESIAN_POINT('Ctrl Pts',(0.982784239981919,67.1175391347301,15.339316920084));
#52496=CARTESIAN_POINT('Ctrl Pts',(0.982754689870178,67.117543173435,15.3393301560546));
#52497=CARTESIAN_POINT('Ctrl Pts',(0.982725139490667,67.1175472121386,15.3393433913963));
#52498=CARTESIAN_POINT('Ctrl Pts',(0.982695588843454,67.117551250841,15.3393566261091));
#52499=CARTESIAN_POINT('Ctrl Pts',(0.922109324786144,67.1258316073113,15.3664911182148));
#52500=CARTESIAN_POINT('Ctrl Pts',(0.860393446777788,67.1341074761172,15.3909823791377));
#52501=CARTESIAN_POINT('Ctrl Pts',(0.797780896354277,67.1423763150738,15.4126612129705));
#52502=CARTESIAN_POINT('Ctrl Pts',(0.766596055873062,67.1464946974442,15.4234585845888));
#52503=CARTESIAN_POINT('Ctrl Pts',(0.735189585599855,67.1506112410446,15.4335581944996));
#52504=CARTESIAN_POINT('Ctrl Pts',(0.703595057907955,67.1547250667235,15.4429389996781));
#52505=CARTESIAN_POINT('Ctrl Pts',(0.641949281710978,67.1627517724741,15.4612423913991));
#52506=CARTESIAN_POINT('Ctrl Pts',(0.579580168885443,67.1707690573066,15.4768103078731));
#52507=CARTESIAN_POINT('Ctrl Pts',(0.516718838837556,67.1787729109142,15.4894972302361));
#52508=CARTESIAN_POINT('Ctrl Pts',(0.441872852807582,67.1883027174716,15.5046029432908));
#52509=CARTESIAN_POINT('Ctrl Pts',(0.366326326676958,67.1978137420768,15.5156230006873));
#52510=CARTESIAN_POINT('Ctrl Pts',(0.290532214727299,67.2073042918928,15.522654148052));
#52511=CARTESIAN_POINT('Ctrl Pts',(0.269175928660516,67.2099784164598,15.5246352939568));
#52512=CARTESIAN_POINT('Ctrl Pts',(0.247799672064465,67.212650955634,15.5262997854447));
#52513=CARTESIAN_POINT('Ctrl Pts',(0.226412839104641,67.2153219660869,15.5276498267794));
#52514=CARTESIAN_POINT('Ctrl Pts',(0.153760445636115,67.2243955536886,15.5322360006383));
#52515=CARTESIAN_POINT('Ctrl Pts',(0.0809892877114056,67.2334511436151,
15.5331939577042));
#52516=CARTESIAN_POINT('Ctrl Pts',(0.0084977608233186,67.2424878466249,
15.5306280363472));
#52517=CARTESIAN_POINT('Ctrl Pts',(-0.0171323136797231,67.2456828596333,
15.529720830245));
#52518=CARTESIAN_POINT('Ctrl Pts',(-0.0427278879719226,67.2488755695627,
15.528373252418));
#52519=CARTESIAN_POINT('Ctrl Pts',(-0.0682728697896764,67.2520661270457,
15.5265902350381));
#52520=CARTESIAN_POINT('Ctrl Pts',(-0.124540879855816,67.2590939778326,
15.522662777168));
#52521=CARTESIAN_POINT('Ctrl Pts',(-0.18055920935557,67.2661108894267,15.5166226061125));
#52522=CARTESIAN_POINT('Ctrl Pts',(-0.236146700513096,67.2731171545432,
15.50852728233));
#52523=CARTESIAN_POINT('Ctrl Pts',(-0.236233284555977,67.2731280676236,
15.5085146729129));
#52524=CARTESIAN_POINT('Ctrl Pts',(-0.236319867735188,67.2731389807008,
15.5085020584813));
#52525=CARTESIAN_POINT('Ctrl Pts',(-0.236406450050159,67.273149893775,15.5084894390349));
#52526=CARTESIAN_POINT('Ctrl Pts',(-0.316070580862892,67.2831909808522,
15.4968783239268));
#52527=CARTESIAN_POINT('Ctrl Pts',(-0.395006978126522,67.2932299245716,
15.4810193120499));
#52528=CARTESIAN_POINT('Ctrl Pts',(-0.472747734688077,67.3032562003277,
15.4610162228001));
#52529=CARTESIAN_POINT('Ctrl Pts',(-0.550488491249631,67.3132824760838,
15.4410131335504));
#52530=CARTESIAN_POINT('Ctrl Pts',(-0.627032943894451,67.3232960838948,
15.4168652821069));
#52531=CARTESIAN_POINT('Ctrl Pts',(-0.701871333130362,67.333280333127,15.3887132297439));
#52532=CARTESIAN_POINT('Ctrl Pts',(-0.774821849382517,67.3430127197179,
15.3612713409699));
#52533=CARTESIAN_POINT('Ctrl Pts',(-0.846161267725897,67.3527182757035,
15.3300166603921));
#52534=CARTESIAN_POINT('Ctrl Pts',(-0.915438489116591,67.3623829279607,
15.2950659221268));
#52535=CARTESIAN_POINT('Ctrl Pts',(-0.980872828743778,67.3715114715928,
15.2620539387943));
#52536=CARTESIAN_POINT('Ctrl Pts',(-1.0444799377276,67.3806050676091,15.2257336576489));
#52537=CARTESIAN_POINT('Ctrl Pts',(-1.10599348298211,67.3896757278653,15.1864015641231));
#52538=CARTESIAN_POINT('Ctrl Pts',(-1.16757719813956,67.3987567352304,15.1470246035818));
#52539=CARTESIAN_POINT('Ctrl Pts',(-1.22706311989344,67.4078147542586,15.1046296196428));
#52540=CARTESIAN_POINT('Ctrl Pts',(-1.28422412356873,67.4168682564532,15.0594815636921));
#52541=CARTESIAN_POINT('Ctrl Pts',(-1.2955747325846,67.4186660339069,15.050516396918));
#52542=CARTESIAN_POINT('Ctrl Pts',(-1.30683377813668,67.420463653499,15.0414425531802));
#52543=CARTESIAN_POINT('Ctrl Pts',(-1.31799963780015,67.4222612899385,15.0322619206413));
#52544=CARTESIAN_POINT('Ctrl Pts',(-1.32453057563323,67.4233127317609,15.0268921468678));
#52545=CARTESIAN_POINT('Ctrl Pts',(-1.33102942544951,67.4243641463121,15.0214860540425));
#52546=CARTESIAN_POINT('Ctrl Pts',(-1.33749952549552,67.4254162679058,15.0160475134865));
#52547=CARTESIAN_POINT('Ctrl Pts',(-1.33751806149286,67.4254192820977,15.0160319327733));
#52548=CARTESIAN_POINT('Ctrl Pts',(-1.33753659725431,67.4254222962954,15.0160163517937));
#52549=CARTESIAN_POINT('Ctrl Pts',(-1.33755513278003,67.425425310499,15.0160007705477));
#52550=CARTESIAN_POINT('Ctrl Pts',(-1.40298136426129,67.4360647702156,14.9610024812003));
#52551=CARTESIAN_POINT('Ctrl Pts',(-1.46511058522356,67.4467073549907,14.9022625456091));
#52552=CARTESIAN_POINT('Ctrl Pts',(-1.52353124202221,67.4573366947174,14.8402373390394));
#52553=CARTESIAN_POINT('Ctrl Pts',(-1.54897547923987,67.4619661435509,14.8132231944557));
#52554=CARTESIAN_POINT('Ctrl Pts',(-1.57371600557726,67.4665930088666,14.785586495174));
#52555=CARTESIAN_POINT('Ctrl Pts',(-1.59771806237704,67.4712156094635,14.7573679195037));
#52556=CARTESIAN_POINT('Ctrl Pts',(-1.65325135088431,67.4819108684051,14.692078918772));
#52557=CARTESIAN_POINT('Ctrl Pts',(-1.70487583412141,67.4925918169658,14.6237000370156));
#52558=CARTESIAN_POINT('Ctrl Pts',(-1.75218278013087,67.5032409785434,14.552690583972));
#52559=CARTESIAN_POINT('Ctrl Pts',(-1.77189075024948,67.5076773959379,14.5231082013248));
#52560=CARTESIAN_POINT('Ctrl Pts',(-1.79084902985319,67.512108215328,14.4930697761375));
#52561=CARTESIAN_POINT('Ctrl Pts',(-1.8090267429479,67.5165318258867,14.4626108117319));
#52562=CARTESIAN_POINT('Ctrl Pts',(-1.84335536439334,67.5248858169252,14.4050890402497));
#52563=CARTESIAN_POINT('Ctrl Pts',(-1.87490195828364,67.5332142608485,14.346067564168));
#52564=CARTESIAN_POINT('Ctrl Pts',(-1.9035877123574,67.5415337881176,14.2858085576063));
#52565=CARTESIAN_POINT('Ctrl Pts',(-1.94202078541709,67.5526802616784,14.2050737512026));
#52566=CARTESIAN_POINT('Ctrl Pts',(-1.97537637401675,67.5638241508068,14.1221106450092));
#52567=CARTESIAN_POINT('Ctrl Pts',(-2.00317650316492,67.5749463956344,14.0375344464522));
#52568=CARTESIAN_POINT('Ctrl Pts',(-2.00320023983893,67.5749558921765,14.0374622324835));
#52569=CARTESIAN_POINT('Ctrl Pts',(-2.00322397246332,67.5749653887027,14.0373900173417));
#52570=CARTESIAN_POINT('Ctrl Pts',(-2.00324770103807,67.5749748852127,14.0373178010271));
#52571=CARTESIAN_POINT('Ctrl Pts',(-2.03196544584963,67.5864681314573,13.9499172843105));
#52572=CARTESIAN_POINT('Ctrl Pts',(-2.0547759415268,67.5979492797131,13.8607102695829));
#52573=CARTESIAN_POINT('Ctrl Pts',(-2.07171504811789,67.6094062229046,13.7705530614861));
#52574=CARTESIAN_POINT('Ctrl Pts',(-2.08118435698114,67.6158108897106,13.7201533284704));
#52575=CARTESIAN_POINT('Ctrl Pts',(-2.08881975601745,67.6222079961578,13.6694570053028));
#52576=CARTESIAN_POINT('Ctrl Pts',(-2.09463440220168,67.6285954557751,13.6186151067743));
#52577=CARTESIAN_POINT('Ctrl Pts',(-2.11079879530123,67.6463522383703,13.4772774556597));
#52578=CARTESIAN_POINT('Ctrl Pts',(-2.11295458015199,67.6640480070286,13.3348199791513));
#52579=CARTESIAN_POINT('Ctrl Pts',(-2.10146517596219,67.6816853824547,13.1940825068232));
#52580=CARTESIAN_POINT('Ctrl Pts',(-2.09503340637605,67.6915587869386,13.1152976560862));
#52581=CARTESIAN_POINT('Ctrl Pts',(-2.08420569210718,67.7013817774878,13.0370725157586));
#52582=CARTESIAN_POINT('Ctrl Pts',(-2.06913454676473,67.7111860523834,12.959848535269));
#52583=CARTESIAN_POINT('Ctrl Pts',(-2.06599239843656,67.7132301230411,12.9437482857076));
#52584=CARTESIAN_POINT('Ctrl Pts',(-2.0626656890284,67.7152733992467,12.9276914124349));
#52585=CARTESIAN_POINT('Ctrl Pts',(-2.05915561342543,67.7173161983369,12.9116817033688));
#52586=CARTESIAN_POINT('Ctrl Pts',(-2.03713566130002,67.7301314032656,12.8112471067808));
#52587=CARTESIAN_POINT('Ctrl Pts',(-2.00790429751469,67.7429423660994,12.7125993664872));
#52588=CARTESIAN_POINT('Ctrl Pts',(-1.97153595331814,67.755730975715,12.6169478106865));
#52589=CARTESIAN_POINT('Ctrl Pts',(-1.95784057497515,67.7605468355249,12.5809279072587));
#52590=CARTESIAN_POINT('Ctrl Pts',(-1.94313362391793,67.7653595013681,12.5453330264051));
#52591=CARTESIAN_POINT('Ctrl Pts',(-1.92742097746522,67.7701679189001,12.5102280246347));
#52592=CARTESIAN_POINT('Ctrl Pts',(-1.9273624926875,67.7701858165363,12.5100973586625));
#52593=CARTESIAN_POINT('Ctrl Pts',(-1.92730399397775,67.7702037141136,12.5099666994772));
#52594=CARTESIAN_POINT('Ctrl Pts',(-1.92724548133832,67.770221611632,12.5098360470811));
#52595=CARTESIAN_POINT('Ctrl Pts',(-1.89388268805193,67.78042643594,12.4353405376545));
#52596=CARTESIAN_POINT('Ctrl Pts',(-1.85594606712321,67.7906246373749,12.3629623359507));
#52597=CARTESIAN_POINT('Ctrl Pts',(-1.81390514066782,67.8008029960214,12.2931814052689));
#52598=CARTESIAN_POINT('Ctrl Pts',(-1.78587564941085,67.8075891027689,12.2466571216396));
#52599=CARTESIAN_POINT('Ctrl Pts',(-1.75602455769745,67.8143660326299,12.2012893012407));
#52600=CARTESIAN_POINT('Ctrl Pts',(-1.72449539874654,67.8211312655222,12.15720489228));
#52601=CARTESIAN_POINT('Ctrl Pts',(-1.67186591855563,67.8324240085683,12.0836177873484));
#52602=CARTESIAN_POINT('Ctrl Pts',(-1.61455546875788,67.8436855174882,12.0135978166629));
#52603=CARTESIAN_POINT('Ctrl Pts',(-1.55319430343768,67.854913951671,11.9476584511344));
#52604=CARTESIAN_POINT('Ctrl Pts',(-1.490176702463,67.866445495787,11.8799390621086));
#52605=CARTESIAN_POINT('Ctrl Pts',(-1.42290462552336,67.8779542420573,11.8164900235485));
#52606=CARTESIAN_POINT('Ctrl Pts',(-1.3519086775529,67.8894258700583,11.7578511951201));
#52607=CARTESIAN_POINT('Ctrl Pts',(-1.26422403677566,67.9035940811907,11.6854284054634));
#52608=CARTESIAN_POINT('Ctrl Pts',(-1.17086690995426,67.9177431912997,11.6202438185883));
#52609=CARTESIAN_POINT('Ctrl Pts',(-1.07297991040925,67.9318726891546,11.5633852818377));
#52610=CARTESIAN_POINT('Ctrl Pts',(-1.00587196812349,67.9415593843335,11.5244050350178));
#52611=CARTESIAN_POINT('Ctrl Pts',(-0.936641483811394,67.9512356360637,
11.4893481233654));
#52612=CARTESIAN_POINT('Ctrl Pts',(-0.865781018865037,67.960887828404,11.4586032577573));
#52613=CARTESIAN_POINT('Ctrl Pts',(-0.847384567092266,67.9633936839755,
11.450621424194));
#52614=CARTESIAN_POINT('Ctrl Pts',(-0.828869449365365,67.9658991326647,
11.4429260972646));
#52615=CARTESIAN_POINT('Ctrl Pts',(-0.810245547536746,67.9684040062905,
11.4355179994328));
#52616=CARTESIAN_POINT('Ctrl Pts',(-0.736597453735771,67.9783095120996,
11.4062227266687));
#52617=CARTESIAN_POINT('Ctrl Pts',(-0.661248837710498,67.9882057440261,
11.38142390213));
#52618=CARTESIAN_POINT('Ctrl Pts',(-0.584846569699776,67.998079249931,11.3611449005179));
#52619=CARTESIAN_POINT('Ctrl Pts',(-0.573442856976445,67.9995529578175,
11.3581180805724));
#52620=CARTESIAN_POINT('Ctrl Pts',(-0.562015697016959,68.001026159749,11.3551918633376));
#52621=CARTESIAN_POINT('Ctrl Pts',(-0.550567263942966,68.0024988113496,
11.3523662310898));
#52622=CARTESIAN_POINT('Ctrl Pts',(-0.472904306267075,68.0124888665996,
11.3331979347609));
#52623=CARTESIAN_POINT('Ctrl Pts',(-0.39428703663205,68.0225320115889,11.3184783768812));
#52624=CARTESIAN_POINT('Ctrl Pts',(-0.315215629184613,68.0325840335563,
11.3082877865524));
#52625=CARTESIAN_POINT('Ctrl Pts',(-0.282660584676796,68.0367226221196,
11.3040921470358));
#52626=CARTESIAN_POINT('Ctrl Pts',(-0.25002913617594,68.0408626348629,11.3006644275602));
#52627=CARTESIAN_POINT('Ctrl Pts',(-0.217358653533609,68.0450006500746,
11.298010839096));
#52628=CARTESIAN_POINT('Ctrl Pts',(-0.181681488236276,68.0495194891235,
11.2951130394122));
#52629=CARTESIAN_POINT('Ctrl Pts',(-0.145955374805118,68.0540179908222,
11.2931782964597));
#52630=CARTESIAN_POINT('Ctrl Pts',(-0.110230287715655,68.0584894806757,
11.2922190932064));
#52631=CARTESIAN_POINT('Ctrl Pts',(-0.0423475323296861,68.0669859484711,
11.2903964703632));
#52632=CARTESIAN_POINT('Ctrl Pts',(0.0255381246184789,68.0753844205154,
11.2920980014165));
#52633=CARTESIAN_POINT('Ctrl Pts',(0.0930775806306368,68.0837449761361,
11.2971864971469));
#52634=CARTESIAN_POINT('Ctrl Pts',(0.137346259163022,68.0892248951491,11.3005217473102));
#52635=CARTESIAN_POINT('Ctrl Pts',(0.181467291853591,68.0946886578296,11.3053121976461));
#52636=CARTESIAN_POINT('Ctrl Pts',(0.225353864231717,68.1001546860651,11.3115228668994));
#52637=CARTESIAN_POINT('Ctrl Pts',(0.297516569778419,68.1091424781092,11.3217350724168));
#52638=CARTESIAN_POINT('Ctrl Pts',(0.369075997083405,68.1181922182479,11.335681354184));
#52639=CARTESIAN_POINT('Ctrl Pts',(0.439522592928712,68.127252151519,11.3534441897224));
#52640=CARTESIAN_POINT('Ctrl Pts',(0.476542392403333,68.1320131610317,11.3627785883806));
#52641=CARTESIAN_POINT('Ctrl Pts',(0.513254263083907,68.1367769028364,11.3731663224128));
#52642=CARTESIAN_POINT('Ctrl Pts',(0.549580840090984,68.1415353209377,11.3846147330983));
#52643=CARTESIAN_POINT('Ctrl Pts',(0.564733045808992,68.1435201082725,11.389389988246));
#52644=CARTESIAN_POINT('Ctrl Pts',(0.579817609193851,68.1455038884702,11.3943495590984));
#52645=CARTESIAN_POINT('Ctrl Pts',(0.594828695117815,68.1474864940762,11.3994926536556));
#52646=CARTESIAN_POINT('Ctrl Pts',(0.594906076925064,68.1474967143631,11.3995191661913));
#52647=CARTESIAN_POINT('Ctrl Pts',(0.594983456779897,68.1475069346188,11.3995456836037));
#52648=CARTESIAN_POINT('Ctrl Pts',(0.595060834681638,68.1475171548433,11.3995722058921));
#52649=CARTESIAN_POINT('Ctrl Pts',(0.665877287827978,68.1568707303468,11.423845471988));
#52650=CARTESIAN_POINT('Ctrl Pts',(0.73518618280262,68.1662151610773,11.4522488590251));
#52651=CARTESIAN_POINT('Ctrl Pts',(0.802629491157741,68.1756010542221,11.4843469818994));
#52652=CARTESIAN_POINT('Ctrl Pts',(0.835024812134113,68.1801094187803,11.4997648049364));
#52653=CARTESIAN_POINT('Ctrl Pts',(0.866990480367676,68.1846274397819,11.5160350135853));
#52654=CARTESIAN_POINT('Ctrl Pts',(0.898491049337421,68.189161220833,11.533109553695));
#52655=CARTESIAN_POINT('Ctrl Pts',(0.954629245752853,68.1972410206422,11.563538651255));
#52656=CARTESIAN_POINT('Ctrl Pts',(1.00926548907983,68.2053397654749,11.596575708451));
#52657=CARTESIAN_POINT('Ctrl Pts',(1.06211801029435,68.2133825614083,11.6321386704489));
#52658=CARTESIAN_POINT('Ctrl Pts',(1.0856187251249,68.2169587664658,11.6479516346981));
#52659=CARTESIAN_POINT('Ctrl Pts',(1.1087661791076,68.2205238214085,11.6642636601206));
#52660=CARTESIAN_POINT('Ctrl Pts',(1.13153290330004,68.2240707202695,11.6810656650742));
#52661=CARTESIAN_POINT('Ctrl Pts',(1.19303899423634,68.233652945716,11.7264575991906));
#52662=CARTESIAN_POINT('Ctrl Pts',(1.2517793554944,68.243103398153,11.7754365697995));
#52663=CARTESIAN_POINT('Ctrl Pts',(1.30743930758822,68.2524853875863,11.8275669677571));
#52664=CARTESIAN_POINT('Ctrl Pts',(1.33212184564187,68.2566458531005,11.8506843166397));
#52665=CARTESIAN_POINT('Ctrl Pts',(1.35619901603249,68.2607929394217,11.8744219613097));
#52666=CARTESIAN_POINT('Ctrl Pts',(1.37964491300665,68.2649325665086,11.898744776689));
#52667=CARTESIAN_POINT('Ctrl Pts',(1.43951542026191,68.2755033531079,11.9608545478032));
#52668=CARTESIAN_POINT('Ctrl Pts',(1.49544913426984,68.2861632631523,12.0266391247986));
#52669=CARTESIAN_POINT('Ctrl Pts',(1.54679585661343,68.2968697758467,12.0956172984592));
#52670=CARTESIAN_POINT('Ctrl Pts',(1.56054512482113,68.2997366913553,12.114087794079));
#52671=CARTESIAN_POINT('Ctrl Pts',(1.57396550254669,68.3026069255889,12.1327869891534));
#52672=CARTESIAN_POINT('Ctrl Pts',(1.58704457420983,68.3054796122426,12.1517050167623));
#52673=CARTESIAN_POINT('Ctrl Pts',(1.62490231172075,68.3137946838385,12.2064637750206));
#52674=CARTESIAN_POINT('Ctrl Pts',(1.6598499050247,68.3220977869915,12.2630779089639));
#52675=CARTESIAN_POINT('Ctrl Pts',(1.69159465907481,68.3303776403841,12.3212218319517));
#52676=CARTESIAN_POINT('Ctrl Pts',(1.69162866258708,68.3303865093801,12.3212841130327));
#52677=CARTESIAN_POINT('Ctrl Pts',(1.69166266242805,68.3303953783495,12.3213463958674));
#52678=CARTESIAN_POINT('Ctrl Pts',(1.69169665859768,68.3304042472921,12.3214086804553));
#52679=CARTESIAN_POINT('Ctrl Pts',(1.73837666322693,68.3425821569951,12.4069313990927));
#52680=CARTESIAN_POINT('Ctrl Pts',(1.7784439712871,68.354873351144,12.4959070786658));
#52681=CARTESIAN_POINT('Ctrl Pts',(1.81184444214334,68.3673094571146,12.5871853379815));
#52682=CARTESIAN_POINT('Ctrl Pts',(1.81511395909518,68.3685268069975,12.5961204160962));
#52683=CARTESIAN_POINT('Ctrl Pts',(1.81831963390605,68.3697455484385,12.6050775647659));
#52684=CARTESIAN_POINT('Ctrl Pts',(1.82146144150065,68.3709657130339,12.6140557110386));
#52685=CARTESIAN_POINT('Ctrl Pts',(1.83518482791304,68.3762953806616,12.6532721706269));
#52686=CARTESIAN_POINT('Ctrl Pts',(1.84763132521184,68.3816113175297,12.6929107899243));
#52687=CARTESIAN_POINT('Ctrl Pts',(1.85876621911123,68.3868926362954,12.7328949381302));
#52688=CARTESIAN_POINT('Ctrl Pts',(1.88213228354135,68.3979752416324,12.8167998402876));
#52689=CARTESIAN_POINT('Ctrl Pts',(1.89972274998347,68.4089036487107,12.9022325279816));
#52690=CARTESIAN_POINT('Ctrl Pts',(1.91156292015285,68.4197387381173,12.9883869853891));
#52691=CARTESIAN_POINT('Ctrl Pts',(1.91418807307555,68.4221410487443,13.0074887907206));
#52692=CARTESIAN_POINT('Ctrl Pts',(1.91653048657638,68.4245387945221,13.0266262679722));
#52693=CARTESIAN_POINT('Ctrl Pts',(1.91859030038067,68.4269326771513,13.0457909463844));
#52694=CARTESIAN_POINT('Ctrl Pts',(1.92780694550799,68.4376441145752,13.1315433767914));
#52695=CARTESIAN_POINT('Ctrl Pts',(1.93136651984106,68.4482792579377,13.2178383265643));
#52696=CARTESIAN_POINT('Ctrl Pts',(1.92929849046949,68.4589098962436,13.303852590471));
#52697=CARTESIAN_POINT('Ctrl Pts',(1.92865281765568,68.4622289565248,13.3307076596339));
#52698=CARTESIAN_POINT('Ctrl Pts',(1.92745865079619,68.465547629321,13.3575357406677));
#52699=CARTESIAN_POINT('Ctrl Pts',(1.9257170153009,68.4688682392933,13.3843128006366));
#52700=CARTESIAN_POINT('Ctrl Pts',(1.92063311035048,68.4785612350564,13.4624761293595));
#52701=CARTESIAN_POINT('Ctrl Pts',(1.91088369555087,68.4882716339163,13.540200727461));
#52702=CARTESIAN_POINT('Ctrl Pts',(1.89651268966639,68.4980493886105,13.6168404080137));
#52703=CARTESIAN_POINT('Ctrl Pts',(1.89163960444516,68.5013649416261,13.6428282684088));
#52704=CARTESIAN_POINT('Ctrl Pts',(1.88623536412119,68.5046882787922,13.6686917434138));
#52705=CARTESIAN_POINT('Ctrl Pts',(1.88030238419093,68.5080214676176,13.6944068048617));
#52706=CARTESIAN_POINT('Ctrl Pts',(1.87853989043799,68.5090116486988,13.7020459062393));
#52707=CARTESIAN_POINT('Ctrl Pts',(1.8767307406184,68.5100026769951,13.7096718313121));
#52708=CARTESIAN_POINT('Ctrl Pts',(1.87487500718747,68.5109945955062,13.7172839207466));
#52709=CARTESIAN_POINT('Ctrl Pts',(1.87486545951162,68.5109996988882,13.7173230846487));
#52710=CARTESIAN_POINT('Ctrl Pts',(1.87485591059547,68.5110048022975,13.7173622482144));
#52711=CARTESIAN_POINT('Ctrl Pts',(1.87484636043896,68.5110099057344,13.7174014114436));
#52712=CARTESIAN_POINT('Ctrl Pts',(1.85917391303867,68.5193849879302,13.781670897485));
#52713=CARTESIAN_POINT('Ctrl Pts',(1.84015899201398,68.5278345730983,13.8450380564246));
#52714=CARTESIAN_POINT('Ctrl Pts',(1.81789758862606,68.5362602246994,13.9071800405893));
#52715=CARTESIAN_POINT('Ctrl Pts',(1.80795815696797,68.5400221702877,13.9349256410774));
#52716=CARTESIAN_POINT('Ctrl Pts',(1.79737187952954,68.5437792600655,13.9624263961141));
#52717=CARTESIAN_POINT('Ctrl Pts',(1.78614921560244,68.5475223268054,13.9896508523836));
#52718=CARTESIAN_POINT('Ctrl Pts',(1.74796944304481,68.5602563298663,14.0822691072939));
#52719=CARTESIAN_POINT('Ctrl Pts',(1.70240793878841,68.5728284818333,14.1717234680048));
#52720=CARTESIAN_POINT('Ctrl Pts',(1.65027068966862,68.5852971810842,14.2570857062341));
#52721=CARTESIAN_POINT('Ctrl Pts',(1.6353432564385,68.5888670985363,14.2815257972065));
#52722=CARTESIAN_POINT('Ctrl Pts',(1.61987649583512,68.5924285700032,14.3056305968578));
#52723=CARTESIAN_POINT('Ctrl Pts',(1.60388860643214,68.5959830481571,14.3293786131698));
#52724=CARTESIAN_POINT('Ctrl Pts',(1.54680696873879,68.6086736184419,14.4141662689318));
#52725=CARTESIAN_POINT('Ctrl Pts',(1.48308517939347,68.621276833383,14.4944038412733));
#52726=CARTESIAN_POINT('Ctrl Pts',(1.41360953097037,68.6338621081308,14.5690594159253));
#52727=CARTESIAN_POINT('Ctrl Pts',(1.39411697807346,68.6373931170428,14.5900052835924));
#52728=CARTESIAN_POINT('Ctrl Pts',(1.3741713902224,68.6409227560878,14.6105120462728));
#52729=CARTESIAN_POINT('Ctrl Pts',(1.35379203710025,68.6444526565273,14.6305575735054));
#52730=CARTESIAN_POINT('Ctrl Pts',(1.29005185512864,68.6554930705682,14.6932536534969));
#52731=CARTESIAN_POINT('Ctrl Pts',(1.222070258675,68.6665368844859,14.7514333519707));
#52732=CARTESIAN_POINT('Ctrl Pts',(1.15048022755247,68.6776191296774,14.8043943858278));
#52733=CARTESIAN_POINT('Ctrl Pts',(1.12769732473153,68.6811459575231,14.8212487727968));
#52734=CARTESIAN_POINT('Ctrl Pts',(1.10454900298406,68.6846767030892,14.8375750169322));
#52735=CARTESIAN_POINT('Ctrl Pts',(1.08105568853527,68.688212565933,14.8533515989667));
#52736=CARTESIAN_POINT('Ctrl Pts',(1.08100793061116,68.6882197537425,14.8533836700825));
#52737=CARTESIAN_POINT('Ctrl Pts',(1.08096017123722,68.6882269415754,14.8534157389415));
#52738=CARTESIAN_POINT('Ctrl Pts',(1.08091241041353,68.6882341294314,14.8534478055435));
#52739=CARTESIAN_POINT('Ctrl Pts',(1.04397323247013,68.6937933613285,14.8782487579797));
#52740=CARTESIAN_POINT('Ctrl Pts',(1.00616614155911,68.6993665948157,14.9016999595785));
#52741=CARTESIAN_POINT('Ctrl Pts',(0.967582305246923,68.7049215413284,14.9237450951548));
#52742=CARTESIAN_POINT('Ctrl Pts',(0.876599878534621,68.7180203558135,14.9757285193976));
#52743=CARTESIAN_POINT('Ctrl Pts',(0.781288567449834,68.7310154485496,15.0198988992346));
#52744=CARTESIAN_POINT('Ctrl Pts',(0.68307542716729,68.7439719937914,15.0559590573212));
#52745=CARTESIAN_POINT('Ctrl Pts',(0.6597944733637,68.7470432806921,15.0645069448253));
#52746=CARTESIAN_POINT('Ctrl Pts',(0.636350240894378,68.750112424547,15.0725990593959));
#52747=CARTESIAN_POINT('Ctrl Pts',(0.612761336926078,68.7531803358453,15.080231302944));
#52748=CARTESIAN_POINT('Ctrl Pts',(0.514135265683734,68.7660073853207,15.1121419926873));
#52749=CARTESIAN_POINT('Ctrl Pts',(0.412982668221154,68.7788149252882,15.1360130738438));
#52750=CARTESIAN_POINT('Ctrl Pts',(0.310748511205798,68.791674532808,15.1515415805569));
#52751=CARTESIAN_POINT('Ctrl Pts',(0.284690919064263,68.7949522084659,15.1554995091622));
#52752=CARTESIAN_POINT('Ctrl Pts',(0.258562866953896,68.7982332972666,15.158915640518));
#52753=CARTESIAN_POINT('Ctrl Pts',(0.23238785137156,68.8015190464572,15.1617852813338));
#52754=CARTESIAN_POINT('Ctrl Pts',(0.186079891383616,68.8073320837625,15.1668621536536));
#52755=CARTESIAN_POINT('Ctrl Pts',(0.139627173158232,68.8131594362542,15.1702280817056));
#52756=CARTESIAN_POINT('Ctrl Pts',(0.0931656021664205,68.819006769892,15.1718581172147));
#52757=CARTESIAN_POINT('Ctrl Pts',(0.0931363051828622,68.8190104570087,
15.1718591450561));
#52758=CARTESIAN_POINT('Ctrl Pts',(0.0931070081897869,68.8190141441331,
15.1718601722065));
#52759=CARTESIAN_POINT('Ctrl Pts',(0.0930777111871997,68.819017831265,15.171861198666));
#52760=CARTESIAN_POINT('Ctrl Pts',(0.0168424844714795,68.8286123056233,
15.1745322012442));
#52761=CARTESIAN_POINT('Ctrl Pts',(-0.0594613922952572,68.8382587090525,
15.172524000833));
#52762=CARTESIAN_POINT('Ctrl Pts',(-0.135291198925329,68.8478383066952,
15.1658754378252));
#52763=CARTESIAN_POINT('Ctrl Pts',(-0.169829887171067,68.8522015874578,
15.1628471742015));
#52764=CARTESIAN_POINT('Ctrl Pts',(-0.20426951442597,68.8565509183454,15.1588563460492));
#52765=CARTESIAN_POINT('Ctrl Pts',(-0.238555396103396,68.8608746332391,
15.1539076293075));
#52766=CARTESIAN_POINT('Ctrl Pts',(-0.324231610074392,68.8716790665585,
15.1415413930115));
#52767=CARTESIAN_POINT('Ctrl Pts',(-0.408985156019361,68.8823265393815,
15.1231883931297));
#52768=CARTESIAN_POINT('Ctrl Pts',(-0.492035858729042,68.8929252685954,
15.0991508658813));
#52769=CARTESIAN_POINT('Ctrl Pts',(-0.522655954429459,68.8968329309299,
15.0902884317209));
#52770=CARTESIAN_POINT('Ctrl Pts',(-0.553045033027673,68.9007340325433,
15.0806530445927));
#52771=CARTESIAN_POINT('Ctrl Pts',(-0.58316546096429,68.9046342223475,15.0702588694412));
#52772=CARTESIAN_POINT('Ctrl Pts',(-0.657939331423372,68.9143164316374,
15.044455361339));
#52773=CARTESIAN_POINT('Ctrl Pts',(-0.731054767225249,68.923995341976,15.0139754646491));
#52774=CARTESIAN_POINT('Ctrl Pts',(-0.801855521623986,68.9337441827855,
14.9790783821898));
#52775=CARTESIAN_POINT('Ctrl Pts',(-0.836912412580603,68.9385713071871,
14.9617991423728));
#52776=CARTESIAN_POINT('Ctrl Pts',(-0.871402523768628,68.9434156445553,
14.9434372900059));
#52777=CARTESIAN_POINT('Ctrl Pts',(-0.905250619902248,68.9482864747851,
14.9240259389021));
#52778=CARTESIAN_POINT('Ctrl Pts',(-0.905266930137861,68.948288821871,14.9240165852383));
#52779=CARTESIAN_POINT('Ctrl Pts',(-0.905283240224452,68.948291168963,14.9240072313309));
#52780=CARTESIAN_POINT('Ctrl Pts',(-0.905299550162034,68.9482935160612,
14.9239978771798));
#52781=CARTESIAN_POINT('Ctrl Pts',(-0.970253699103387,68.9576408090992,
14.886745072231));
#52782=CARTESIAN_POINT('Ctrl Pts',(-1.03295147104993,68.9670915532174,14.8455528180476));
#52783=CARTESIAN_POINT('Ctrl Pts',(-1.09292850686405,68.9765452662854,14.8007804210796));
#52784=CARTESIAN_POINT('Ctrl Pts',(-1.11214782069943,68.9795746570497,14.7864333507917));
#52785=CARTESIAN_POINT('Ctrl Pts',(-1.13108766917462,68.9826043180204,14.7717190471577));
#52786=CARTESIAN_POINT('Ctrl Pts',(-1.14973261369638,68.9856308458847,14.7566504437348));
#52787=CARTESIAN_POINT('Ctrl Pts',(-1.21031410155768,68.9954646944571,14.7076892674604));
#52788=CARTESIAN_POINT('Ctrl Pts',(-1.26778845896674,69.0052650179686,14.6549820159269));
#52789=CARTESIAN_POINT('Ctrl Pts',(-1.32169867323303,69.0149270081729,14.5989165098566));
#52790=CARTESIAN_POINT('Ctrl Pts',(-1.37953165188915,69.0252920508809,14.5387714100822));
#52791=CARTESIAN_POINT('Ctrl Pts',(-1.43327523568867,69.0354990150761,14.4747485045646));
#52792=CARTESIAN_POINT('Ctrl Pts',(-1.48247885284466,69.0456765259749,14.4074637756967));
#52793=CARTESIAN_POINT('Ctrl Pts',(-1.49158732613464,69.0475605660422,14.395008163871));
#52794=CARTESIAN_POINT('Ctrl Pts',(-1.50054027425752,69.0494436145655,14.3824406410803));
#52795=CARTESIAN_POINT('Ctrl Pts',(-1.50933489930898,69.0513265115291,14.3697649315476));
#52796=CARTESIAN_POINT('Ctrl Pts',(-1.5489866824539,69.0598158128522,14.3126147423519));
#52797=CARTESIAN_POINT('Ctrl Pts',(-1.58549035758771,69.0684227163165,14.2533140301097));
#52798=CARTESIAN_POINT('Ctrl Pts',(-1.61848591346177,69.0770917173401,14.1922107166905));
#52799=CARTESIAN_POINT('Ctrl Pts',(-1.61850931052721,69.0770978645069,14.1921673884851));
#52800=CARTESIAN_POINT('Ctrl Pts',(-1.6185327058295,69.0771040117048,14.1921240593746));
#52801=CARTESIAN_POINT('Ctrl Pts',(-1.61855609936858,69.0771101589338,14.192080729359));
#52802=CARTESIAN_POINT('Ctrl Pts',(-1.66070022745041,69.0881845673918,14.1140204701822));
#52803=CARTESIAN_POINT('Ctrl Pts',(-1.69710444854914,69.099259015454,14.0328720507928));
#52804=CARTESIAN_POINT('Ctrl Pts',(-1.7275382889765,69.1103228311945,13.9496120546416));
#52805=CARTESIAN_POINT('Ctrl Pts',(-1.73599710152014,69.1133979193875,13.9264706866795));
#52806=CARTESIAN_POINT('Ctrl Pts',(-1.74399497917996,69.1164721865456,13.9031663243045));
#52807=CARTESIAN_POINT('Ctrl Pts',(-1.75152764174066,69.1195454042379,13.8797201735005));
#52808=CARTESIAN_POINT('Ctrl Pts',(-1.78195104824263,69.131957715339,13.7850243377229));
#52809=CARTESIAN_POINT('Ctrl Pts',(-1.80484100416277,69.1444324335709,13.6880260368187));
#52810=CARTESIAN_POINT('Ctrl Pts',(-1.81988876386058,69.1568625540882,13.5899141816979));
#52811=CARTESIAN_POINT('Ctrl Pts',(-1.82183488333921,69.1584701355585,13.577225422961));
#52812=CARTESIAN_POINT('Ctrl Pts',(-1.82364978265495,69.1600769627076,13.5645180883504));
#52813=CARTESIAN_POINT('Ctrl Pts',(-1.82533275185528,69.1616827966858,13.5517947958796));
#52814=CARTESIAN_POINT('Ctrl Pts',(-1.82750250595369,69.1637531048381,13.5353913964719));
#52815=CARTESIAN_POINT('Ctrl Pts',(-1.82945186819067,69.1658199909594,13.5189609076884));
#52816=CARTESIAN_POINT('Ctrl Pts',(-1.83117927532594,69.1678829316276,13.5025085813656));
#52817=CARTESIAN_POINT('Ctrl Pts',(-1.84019634134475,69.1786514828382,13.4166274306009));
#52818=CARTESIAN_POINT('Ctrl Pts',(-1.84317880715676,69.1893342220889,13.3301344567272));
#52819=CARTESIAN_POINT('Ctrl Pts',(-1.84003546593005,69.2000820374621,13.2439078475955));
#52820=CARTESIAN_POINT('Ctrl Pts',(-1.83949636341294,69.2019253544624,13.2291194493048));
#52821=CARTESIAN_POINT('Ctrl Pts',(-1.838777102145,69.2037706015976,13.2143387659784));
#52822=CARTESIAN_POINT('Ctrl Pts',(-1.83787724861594,69.2056185596576,13.1995700790813));
#52823=CARTESIAN_POINT('Ctrl Pts',(-1.83787470789756,69.2056237773301,13.1995283799904));
#52824=CARTESIAN_POINT('Ctrl Pts',(-1.8378721657395,69.2056289950242,13.199486680995));
#52825=CARTESIAN_POINT('Ctrl Pts',(-1.8378696221418,69.2056342127399,13.1994449820954));
#52826=CARTESIAN_POINT('Ctrl Pts',(-1.83209449120491,69.2174808154877,13.1047693951828));
#52827=CARTESIAN_POINT('Ctrl Pts',(-1.81881982165952,69.2293288211434,13.0105424621769));
#52828=CARTESIAN_POINT('Ctrl Pts',(-1.79847145921251,69.2412080594862,12.9179033354241));
#52829=CARTESIAN_POINT('Ctrl Pts',(-1.79176339780701,69.245124181015,12.8873638287473));
#52830=CARTESIAN_POINT('Ctrl Pts',(-1.78428698650568,69.2490437111564,12.8569967182915));
#52831=CARTESIAN_POINT('Ctrl Pts',(-1.77605856810413,69.2529677599195,12.8268422391248));
#52832=CARTESIAN_POINT('Ctrl Pts',(-1.76412320153114,69.2586596144353,12.7831029996854));
#52833=CARTESIAN_POINT('Ctrl Pts',(-1.75060234828232,69.264357284898,12.7398079525592));
#52834=CARTESIAN_POINT('Ctrl Pts',(-1.73552925179681,69.2700398628983,12.6970738834494));
#52835=CARTESIAN_POINT('Ctrl Pts',(-1.72421277786779,69.2743061890544,12.6649902980078));
#52836=CARTESIAN_POINT('Ctrl Pts',(-1.7120214176308,69.2785639695877,12.6332225871527));
#52837=CARTESIAN_POINT('Ctrl Pts',(-1.69897118040291,69.2828169025217,12.6018098352524));
#52838=CARTESIAN_POINT('Ctrl Pts',(-1.68592135101795,69.2870697025441,12.5703980650559));
#52839=CARTESIAN_POINT('Ctrl Pts',(-1.67201256779544,69.2913177462213,12.5393414325066));
#52840=CARTESIAN_POINT('Ctrl Pts',(-1.65726440129855,69.2955608417011,12.5086925894493));
#52841=CARTESIAN_POINT('Ctrl Pts',(-1.62776592614726,69.3040476489664,12.4473904516187));
#52842=CARTESIAN_POINT('Ctrl Pts',(-1.59490854670523,69.3125146766274,12.3877174264648));
#52843=CARTESIAN_POINT('Ctrl Pts',(-1.55885295601687,69.3209949076823,12.3300602016484));
#52844=CARTESIAN_POINT('Ctrl Pts',(-1.54048039462877,69.3253161117638,12.3006802668815));
#52845=CARTESIAN_POINT('Ctrl Pts',(-1.52127756550842,69.3296407416996,12.2718241534475));
#52846=CARTESIAN_POINT('Ctrl Pts',(-1.501269486861,69.3339738588297,12.243546551302));
#52847=CARTESIAN_POINT('Ctrl Pts',(-1.50125417910618,69.3339771740053,12.2435249167109));
#52848=CARTESIAN_POINT('Ctrl Pts',(-1.50123887088004,69.3339804891859,12.2435032824584));
#52849=CARTESIAN_POINT('Ctrl Pts',(-1.5012235621826,69.3339838043714,12.2434816485444));
#52850=CARTESIAN_POINT('Ctrl Pts',(-1.44270312331132,69.3466567385215,12.1607818535739));
#52851=CARTESIAN_POINT('Ctrl Pts',(-1.37727059666993,69.3594023695588,12.0830028973156));
#52852=CARTESIAN_POINT('Ctrl Pts',(-1.30595300121857,69.3720704918851,12.0110840954185));
#52853=CARTESIAN_POINT('Ctrl Pts',(-1.22373895563992,69.3866741472626,11.9281769864546));
#52854=CARTESIAN_POINT('Ctrl Pts',(-1.13368135921862,69.4011774147825,11.8530272603493));
#52855=CARTESIAN_POINT('Ctrl Pts',(-1.03741168707502,69.4156969169235,11.7869269111661));
#52856=CARTESIAN_POINT('Ctrl Pts',(-1.02836624472683,69.4170611608917,11.7807161608393));
#52857=CARTESIAN_POINT('Ctrl Pts',(-1.01926592256557,69.4184255518865,11.774585308269));
#52858=CARTESIAN_POINT('Ctrl Pts',(-1.01011205113707,69.4197901889151,11.7685354310156));
#52859=CARTESIAN_POINT('Ctrl Pts',(-0.927728839566411,69.4320716789841,
11.714087613867));
#52860=CARTESIAN_POINT('Ctrl Pts',(-0.841010321457216,69.4443741814331,
11.666203708608));
#52861=CARTESIAN_POINT('Ctrl Pts',(-0.751025060748099,69.4567556143385,
11.6257067166657));
#52862=CARTESIAN_POINT('Ctrl Pts',(-0.738337487655072,69.4585013484036,
11.6199967977161));
#52863=CARTESIAN_POINT('Ctrl Pts',(-0.725584981363605,69.4602486552138,
11.6144336457452));
#52864=CARTESIAN_POINT('Ctrl Pts',(-0.712770542514273,69.4619977006017,
11.6090194833255));
#52865=CARTESIAN_POINT('Ctrl Pts',(-0.712748839065249,69.4620006629099,
11.6090103135133));
#52866=CARTESIAN_POINT('Ctrl Pts',(-0.712727135438581,69.4620036252231,
11.6090011441285));
#52867=CARTESIAN_POINT('Ctrl Pts',(-0.712705431634265,69.4620065875413,
11.608991975171));
#52868=CARTESIAN_POINT('Ctrl Pts',(-0.68373789530444,69.4659603211094,11.5967543920721));
#52869=CARTESIAN_POINT('Ctrl Pts',(-0.654446042270547,69.4699210624971,
11.5852762013665));
#52870=CARTESIAN_POINT('Ctrl Pts',(-0.624871340462196,69.4738815372614,
11.5745657079349));
#52871=CARTESIAN_POINT('Ctrl Pts',(-0.5038218893111,69.4900917868059,11.5307275871027));
#52872=CARTESIAN_POINT('Ctrl Pts',(-0.378032318714275,69.5062965304003,
11.4997508387732));
#52873=CARTESIAN_POINT('Ctrl Pts',(-0.250354183834203,69.5224717181252,
11.4819724632507));
#52874=CARTESIAN_POINT('Ctrl Pts',(-0.12071941207351,69.5388947867334,11.4639216383754));
#52875=CARTESIAN_POINT('Ctrl Pts',(0.0108627437138111,69.5552872739215,
11.459474420351));
#52876=CARTESIAN_POINT('Ctrl Pts',(0.141436553988745,69.5716444458873,11.4689754951994));
#52877=CARTESIAN_POINT('Ctrl Pts',(0.153514045885899,69.573157410941,11.4698543020157));
#52878=CARTESIAN_POINT('Ctrl Pts',(0.165582926188795,69.5746700887724,11.4708524507153));
#52879=CARTESIAN_POINT('Ctrl Pts',(0.177640863840469,69.5761824848123,11.4719702206754));
#52880=CARTESIAN_POINT('Ctrl Pts',(0.216070703669195,69.581002640568,11.4755326640861));
#52881=CARTESIAN_POINT('Ctrl Pts',(0.254389918738245,69.5858200152393,11.4803103128853));
#52882=CARTESIAN_POINT('Ctrl Pts',(0.29251715287334,69.5906438953241,11.4863076060511));
#52883=CARTESIAN_POINT('Ctrl Pts',(0.292527528266156,69.590645208025,11.4863092380675));
#52884=CARTESIAN_POINT('Ctrl Pts',(0.292537903645354,69.5906465207263,11.4863108701744));
#52885=CARTESIAN_POINT('Ctrl Pts',(0.292548279010891,69.5906478334283,11.4863125023716));
#52886=CARTESIAN_POINT('Ctrl Pts',(0.388751094272645,69.6028195128875,11.5014466165791));
#52887=CARTESIAN_POINT('Ctrl Pts',(0.483781469591908,69.6150409052945,11.5243562069561));
#52888=CARTESIAN_POINT('Ctrl Pts',(0.576463822122927,69.6272495061805,11.5545531893843));
#52889=CARTESIAN_POINT('Ctrl Pts',(0.682512323524433,69.6412187656222,11.5891050177087));
#52890=CARTESIAN_POINT('Ctrl Pts',(0.785493577277762,69.6551694244689,11.633191059219));
#52891=CARTESIAN_POINT('Ctrl Pts',(0.883813285938799,69.6690842139963,11.6861095460118));
#52892=CARTESIAN_POINT('Ctrl Pts',(0.905440101635131,69.6721449694914,11.6977497184287));
#52893=CARTESIAN_POINT('Ctrl Pts',(0.926841273950825,69.6752039869934,11.7098174162052));
#52894=CARTESIAN_POINT('Ctrl Pts',(0.947999644255617,69.6782610787044,11.7223054517188));
#52895=CARTESIAN_POINT('Ctrl Pts',(0.977334911426482,69.6824996188573,11.7396196329603));
#52896=CARTESIAN_POINT('Ctrl Pts',(1.0062044211962,69.6867347405138,11.7577423413469));
#52897=CARTESIAN_POINT('Ctrl Pts',(1.03456180279423,69.690973810479,11.776651724978));
#52898=CARTESIAN_POINT('Ctrl Pts',(1.06292010858455,69.6952130185992,11.7955617248828));
#52899=CARTESIAN_POINT('Ctrl Pts',(1.09076538640764,69.6994561467566,11.8152581911504));
#52900=CARTESIAN_POINT('Ctrl Pts',(1.11803848669445,69.7036964996888,11.8357132175244));
#52901=CARTESIAN_POINT('Ctrl Pts',(1.15077513339974,69.7087863110557,11.8602659440098));
#52902=CARTESIAN_POINT('Ctrl Pts',(1.18269098424645,69.7138745411377,11.8859129245652));
#52903=CARTESIAN_POINT('Ctrl Pts',(1.21371105698516,69.7189734331952,11.912617539152));
#52904=CARTESIAN_POINT('Ctrl Pts',(1.23438455871875,69.7223716184503,11.9304149795578));
#52905=CARTESIAN_POINT('Ctrl Pts',(1.2546601880194,69.7257745416328,11.9486822204782));
#52906=CARTESIAN_POINT('Ctrl Pts',(1.27452332141809,69.7291858428091,11.967395862835));
#52907=CARTESIAN_POINT('Ctrl Pts',(1.31715055371471,69.7365066579474,12.007556232493));
#52908=CARTESIAN_POINT('Ctrl Pts',(1.35787582192742,69.7438593168303,12.0497730907761));
#52909=CARTESIAN_POINT('Ctrl Pts',(1.39653348139712,69.7512108225702,12.0938224692718));
#52910=CARTESIAN_POINT('Ctrl Pts',(1.40333686633492,69.7525046185244,12.1015747461113));
#52911=CARTESIAN_POINT('Ctrl Pts',(1.41007620558189,69.7537983776909,12.1093837751367));
#52912=CARTESIAN_POINT('Ctrl Pts',(1.41675059216139,69.7550919204249,12.1172485883696));
#52913=CARTESIAN_POINT('Ctrl Pts',(1.46052910805424,69.7635765025607,12.1688353292648));
#52914=CARTESIAN_POINT('Ctrl Pts',(1.50151284102932,69.7720536819369,12.2228206859292));
#52915=CARTESIAN_POINT('Ctrl Pts',(1.53944830035807,69.7804859331021,12.2789293798705));
#52916=CARTESIAN_POINT('Ctrl Pts',(1.54389162139629,69.7814735894971,12.2855013034646));
#52917=CARTESIAN_POINT('Ctrl Pts',(1.54829317003369,69.7824606371911,12.2921024302378));
#52918=CARTESIAN_POINT('Ctrl Pts',(1.55265261989843,69.7834471680316,12.298732390422));
#52919=CARTESIAN_POINT('Ctrl Pts',(1.55266401720386,69.7834497472087,12.2987497237287));
#52920=CARTESIAN_POINT('Ctrl Pts',(1.55267541421877,69.7834523263782,12.2987670572298));
#52921=CARTESIAN_POINT('Ctrl Pts',(1.55268681094315,69.7834549055402,12.2987843909253));
#52922=CARTESIAN_POINT('Ctrl Pts',(1.59993576317875,69.794147688385,12.3706470530331));
#52923=CARTESIAN_POINT('Ctrl Pts',(1.64219334337782,69.8047098714146,12.4458491507882));
#52924=CARTESIAN_POINT('Ctrl Pts',(1.67908667743357,69.8152487412729,12.5236951541159));
#52925=CARTESIAN_POINT('Ctrl Pts',(1.71597474371204,69.8257861063493,12.601530042281));
#52926=CARTESIAN_POINT('Ctrl Pts',(1.74749420336776,69.8363010435062,12.682011004518));
#52927=CARTESIAN_POINT('Ctrl Pts',(1.77322308422684,69.8469495522407,12.7643046379956));
#52928=CARTESIAN_POINT('Ctrl Pts',(1.77323296526681,69.8469536417439,12.7643362424282));
#52929=CARTESIAN_POINT('Ctrl Pts',(1.7732428454533,69.8469577312668,12.7643678471283));
#52930=CARTESIAN_POINT('Ctrl Pts',(1.77325272478628,69.8469618208095,12.7643994520956));
#52931=CARTESIAN_POINT('Ctrl Pts',(1.79992357399828,69.8580021993299,12.8497221475336));
#52932=CARTESIAN_POINT('Ctrl Pts',(1.82039847299613,69.8691749690202,12.937104973935));
#52933=CARTESIAN_POINT('Ctrl Pts',(1.83456353934237,69.880353384387,13.0255553584996));
#52934=CARTESIAN_POINT('Ctrl Pts',(1.84872059399211,69.8915254772934,13.1139557159326));
#52935=CARTESIAN_POINT('Ctrl Pts',(1.85658086837671,69.9027139196788,13.2034183259347));
#52936=CARTESIAN_POINT('Ctrl Pts',(1.85811281102288,69.914042475166,13.2930013745112));
#52937=CARTESIAN_POINT('Ctrl Pts',(1.85961737215055,69.9251685471905,13.3809832404928));
#52938=CARTESIAN_POINT('Ctrl Pts',(1.85500143945498,69.9363253476092,13.4690832168717));
#52939=CARTESIAN_POINT('Ctrl Pts',(1.84420378027491,69.9474653598375,13.5564675180094));
#52940=CARTESIAN_POINT('Ctrl Pts',(1.8345395353106,69.95743602156,13.6346792190963));
#52941=CARTESIAN_POINT('Ctrl Pts',(1.81992454299468,69.9673932662656,13.7123189970479));
#52942=CARTESIAN_POINT('Ctrl Pts',(1.80028811406486,69.9773093570152,13.7888228408032));
#52943=CARTESIAN_POINT('Ctrl Pts',(1.80028560513862,69.9773106239838,13.7888326156203));
#52944=CARTESIAN_POINT('Ctrl Pts',(1.80028309613099,69.9773118909515,13.7888423904164));
#52945=CARTESIAN_POINT('Ctrl Pts',(1.80028058704198,69.9773131579182,13.7888521651914));
#52946=CARTESIAN_POINT('Ctrl Pts',(1.79446016413059,69.9802521855423,13.8115270580995));
#52947=CARTESIAN_POINT('Ctrl Pts',(1.78820186104656,69.9831858509615,13.8340887284314));
#52948=CARTESIAN_POINT('Ctrl Pts',(1.78151353793073,69.9861135095289,13.8565259325416));
#52949=CARTESIAN_POINT('Ctrl Pts',(1.75782960471734,69.9964806028617,13.935978021569));
#52950=CARTESIAN_POINT('Ctrl Pts',(1.7287544737392,70.0067732359488,14.0138794677029));
#52951=CARTESIAN_POINT('Ctrl Pts',(1.69462535931963,70.0170483962411,14.0896684836126));
#52952=CARTESIAN_POINT('Ctrl Pts',(1.69183469961894,70.0178885726193,14.0958655782648));
#52953=CARTESIAN_POINT('Ctrl Pts',(1.68901022154927,70.0187286324704,14.1020485413191));
#52954=CARTESIAN_POINT('Ctrl Pts',(1.68615209497705,70.0195686071028,14.1082170607523));
#52955=CARTESIAN_POINT('Ctrl Pts',(1.64842455736105,70.030656350678,14.1896420932248));
#52956=CARTESIAN_POINT('Ctrl Pts',(1.60483464544317,70.0417295703943,14.2685507960509));
#52957=CARTESIAN_POINT('Ctrl Pts',(1.55581371265823,70.0528476944124,14.3441219594759));
#52958=CARTESIAN_POINT('Ctrl Pts',(1.50732926037688,70.0638441427212,14.4188660791564));
#52959=CARTESIAN_POINT('Ctrl Pts',(1.45352846295804,70.0748846241759,14.4903420632944));
#52960=CARTESIAN_POINT('Ctrl Pts',(1.39490150108386,70.0860110902979,14.557678414196));
#52961=CARTESIAN_POINT('Ctrl Pts',(1.35786942450768,70.0930391902076,14.6002118292534));
#52962=CARTESIAN_POINT('Ctrl Pts',(1.3189135161113,70.1001012649247,14.6410920456838));
#52963=CARTESIAN_POINT('Ctrl Pts',(1.27818060303822,70.1072045904037,14.6800943415359));
#52964=CARTESIAN_POINT('Ctrl Pts',(1.27816250885692,70.1072077458092,14.6801116669507));
#52965=CARTESIAN_POINT('Ctrl Pts',(1.27814441432512,70.1072109012229,14.680128991995));
#52966=CARTESIAN_POINT('Ctrl Pts',(1.27812631944288,70.1072140566447,14.680146316669));
#52967=CARTESIAN_POINT('Ctrl Pts',(1.22493024275396,70.116490495039,14.7310781035215));
#52968=CARTESIAN_POINT('Ctrl Pts',(1.16856508890574,70.1257915775979,14.7789302298088));
#52969=CARTESIAN_POINT('Ctrl Pts',(1.10954585560057,70.1350925529722,14.8233679525907));
#52970=CARTESIAN_POINT('Ctrl Pts',(1.09646681096988,70.137153709399,14.8332156399801));
#52971=CARTESIAN_POINT('Ctrl Pts',(1.08325756611831,70.1392148600082,14.8428957953405));
#52972=CARTESIAN_POINT('Ctrl Pts',(1.06992394830663,70.1412757345038,14.8524050373711));
#52973=CARTESIAN_POINT('Ctrl Pts',(0.996965772678296,70.1525523171633,14.904437198482));
#52974=CARTESIAN_POINT('Ctrl Pts',(0.920283437593562,70.1638204440748,14.951352796264));
#52975=CARTESIAN_POINT('Ctrl Pts',(0.840676818107517,70.175061902439,14.9927205550713));
#52976=CARTESIAN_POINT('Ctrl Pts',(0.795391524750961,70.181456756825,15.0162531595856));
#52977=CARTESIAN_POINT('Ctrl Pts',(0.749157050823362,70.1878434907123,15.0379927628673));
#52978=CARTESIAN_POINT('Ctrl Pts',(0.702094673609501,70.1942225345618,15.0578681942149));
#52979=CARTESIAN_POINT('Ctrl Pts',(0.618921025038079,70.2054962606836,15.0929941746686));
#52980=CARTESIAN_POINT('Ctrl Pts',(0.533133877493328,70.2167497624942,15.1223069293621));
#52981=CARTESIAN_POINT('Ctrl Pts',(0.445527765571953,70.2279938296179,15.1453246978411));
#52982=CARTESIAN_POINT('Ctrl Pts',(0.41604327251346,70.2317781046164,15.1530715002052));
#52983=CARTESIAN_POINT('Ctrl Pts',(0.386355096314788,70.235560989632,15.1601045217764));
#52984=CARTESIAN_POINT('Ctrl Pts',(0.356501118187787,70.2393419128353,15.1664045404908));
#52985=CARTESIAN_POINT('Ctrl Pts',(0.356497694570308,70.2393423464269,15.1664052629692));
#52986=CARTESIAN_POINT('Ctrl Pts',(0.356494270950439,70.2393427800186,15.166405985438));
#52987=CARTESIAN_POINT('Ctrl Pts',(0.356490847328433,70.2393432136104,15.1664067078971));
#52988=CARTESIAN_POINT('Ctrl Pts',(0.26518298974908,70.2509070882866,15.185674663696));
#52989=CARTESIAN_POINT('Ctrl Pts',(0.172264435215834,70.2625249530684,15.198098086844));
#52990=CARTESIAN_POINT('Ctrl Pts',(0.0787817346057373,70.2741829872538,
15.2037064118793));
#52991=CARTESIAN_POINT('Ctrl Pts',(-0.0156222507291631,70.2859559129512,
15.2093700077205));
#52992=CARTESIAN_POINT('Ctrl Pts',(-0.110600567102631,70.2977695714574,
15.2080845097316));
#52993=CARTESIAN_POINT('Ctrl Pts',(-0.205096011477666,70.3096120876114,
15.1998951032177));
#52994=CARTESIAN_POINT('Ctrl Pts',(-0.297223970214025,70.3211579017698,
15.191910873815));
#52995=CARTESIAN_POINT('Ctrl Pts',(-0.388892914324814,70.3327309933088,
15.177365559377));
#52996=CARTESIAN_POINT('Ctrl Pts',(-0.479149317467216,70.3443253752098,
15.1562983448823));
#52997=CARTESIAN_POINT('Ctrl Pts',(-0.551891956122537,70.3536699303183,
15.1393191088603));
#52998=CARTESIAN_POINT('Ctrl Pts',(-0.62371763751532,70.3630283842836,15.118103776966));
#52999=CARTESIAN_POINT('Ctrl Pts',(-0.694139123852421,70.3724009765456,
15.0926628341088));
#53000=CARTESIAN_POINT('Ctrl Pts',(-0.764864088097802,70.3818139595299,
15.0671122547682));
#53001=CARTESIAN_POINT('Ctrl Pts',(-0.834160445598943,70.391216549276,15.0373047095698));
#53002=CARTESIAN_POINT('Ctrl Pts',(-0.901575673922172,70.4006539779655,
15.0034955940613));
#53003=CARTESIAN_POINT('Ctrl Pts',(-0.913682702578334,70.4023488356768,
14.997423851215));
#53004=CARTESIAN_POINT('Ctrl Pts',(-0.92572935864844,70.4040448559331,14.9912229041927));
#53005=CARTESIAN_POINT('Ctrl Pts',(-0.937713386497447,70.4057423488503,
14.9848940070625));
#53006=CARTESIAN_POINT('Ctrl Pts',(-0.938294742236985,70.4058246957259,
14.9845869866918));
#53007=CARTESIAN_POINT('Ctrl Pts',(-0.938875950619259,70.4059070460711,
14.9842796651939));
#53008=CARTESIAN_POINT('Ctrl Pts',(-0.939457011373071,70.4059893998935,
14.9839720427189));
#53009=CARTESIAN_POINT('Ctrl Pts',(-0.939465540023992,70.4059906086604,
14.9839675275203));
#53010=CARTESIAN_POINT('Ctrl Pts',(-0.939474068641808,70.4059918174268,
14.9839630122576));
#53011=CARTESIAN_POINT('Ctrl Pts',(-0.939482597226596,70.4059930261928,
14.9839584969309));
#53012=CARTESIAN_POINT('Ctrl Pts',(-1.00939412915963,70.4159016668488,14.9469449221697));
#53013=CARTESIAN_POINT('Ctrl Pts',(-1.07708576410025,70.4257798249436,14.9056298077126));
#53014=CARTESIAN_POINT('Ctrl Pts',(-1.14215186022346,70.4356567711562,14.8602973421181));
#53015=CARTESIAN_POINT('Ctrl Pts',(-1.20733991421339,70.4455522304097,14.8148799067602));
#53016=CARTESIAN_POINT('Ctrl Pts',(-1.26989112231966,70.4554464180391,14.7654263960899));
#53017=CARTESIAN_POINT('Ctrl Pts',(-1.32930124400838,70.4653537079032,14.7122515857891));
#53018=CARTESIAN_POINT('Ctrl Pts',(-1.38859276529357,70.4752412198483,14.659182928342));
#53019=CARTESIAN_POINT('Ctrl Pts',(-1.44475293254124,70.4851415401354,14.6024050340269));
#53020=CARTESIAN_POINT('Ctrl Pts',(-1.49721656075818,70.4950561567261,14.5423079518511));
#53021=CARTESIAN_POINT('Ctrl Pts',(-1.51814295636831,70.4990108429754,14.518336767254));
#53022=CARTESIAN_POINT('Ctrl Pts',(-1.53848075620142,70.5029676821934,14.4938385830972));
#53023=CARTESIAN_POINT('Ctrl Pts',(-1.55819304826531,70.5069263743563,14.4688428834298));
#53024=CARTESIAN_POINT('Ctrl Pts',(-1.55820491784598,70.5069287580475,14.4688278324924));
#53025=CARTESIAN_POINT('Ctrl Pts',(-1.55821678719993,70.5069311417393,14.4688127813746));
#53026=CARTESIAN_POINT('Ctrl Pts',(-1.5582286563271,70.5069335254318,14.4687977300765));
#53027=CARTESIAN_POINT('Ctrl Pts',(-1.60608790998573,70.5165451625486,14.4081071769877));
#53028=CARTESIAN_POINT('Ctrl Pts',(-1.65037144160631,70.5261963929361,14.3443353252483));
#53029=CARTESIAN_POINT('Ctrl Pts',(-1.69077538048006,70.5358717255455,14.2780585430121));
#53030=CARTESIAN_POINT('Ctrl Pts',(-1.69503801462446,70.5368924775882,14.2710663119867));
#53031=CARTESIAN_POINT('Ctrl Pts',(-1.69925750474247,70.5379134977626,14.2640462300519));
#53032=CARTESIAN_POINT('Ctrl Pts',(-1.7034335209034,70.5389347677829,14.2569989939056));
#53033=CARTESIAN_POINT('Ctrl Pts',(-1.74721911509653,70.5496427997798,14.1831086136498));
#53034=CARTESIAN_POINT('Ctrl Pts',(-1.78622351033457,70.5603785454426,14.1062323600374));
#53035=CARTESIAN_POINT('Ctrl Pts',(-1.82013061855966,70.5711368687535,14.027094074813));
#53036=CARTESIAN_POINT('Ctrl Pts',(-1.85399094680987,70.5818803493332,13.9480649728009));
#53037=CARTESIAN_POINT('Ctrl Pts',(-1.88277186781581,70.592646729472,13.8667814792335));
#53038=CARTESIAN_POINT('Ctrl Pts',(-1.90619754185183,70.6034421128268,13.7838715555113));
#53039=CARTESIAN_POINT('Ctrl Pts',(-1.91915314766995,70.6094125165465,13.7380180919779));
#53040=CARTESIAN_POINT('Ctrl Pts',(-1.93047113420154,70.6153919626634,13.6916653440043));
#53041=CARTESIAN_POINT('Ctrl Pts',(-1.94010317057641,70.6213821810444,13.6449060603244));
#53042=CARTESIAN_POINT('Ctrl Pts',(-1.95201614892721,70.6287909302551,13.5870738104761));
#53043=CARTESIAN_POINT('Ctrl Pts',(-1.9613503006164,70.6362166060507,13.5286148927615));
#53044=CARTESIAN_POINT('Ctrl Pts',(-1.96800620138842,70.6436261756634,13.4697421946718));
#53045=CARTESIAN_POINT('Ctrl Pts',(-1.98416216515208,70.661611530654,13.3268396470551));
#53046=CARTESIAN_POINT('Ctrl Pts',(-1.98448596022075,70.6796484252118,13.1816590285085));
#53047=CARTESIAN_POINT('Ctrl Pts',(-1.96926429907825,70.6977348846467,13.0377052164726));
#53048=CARTESIAN_POINT('Ctrl Pts',(-1.9532151699708,70.7168045459569,12.8859259005856));
#53049=CARTESIAN_POINT('Ctrl Pts',(-1.91988458772862,70.7359289508103,12.7355123366635));
#53050=CARTESIAN_POINT('Ctrl Pts',(-1.8696091510795,70.7551146490957,12.590575892318));
#53051=CARTESIAN_POINT('Ctrl Pts',(-1.8581578190305,70.7594846121691,12.5575634420874));
#53052=CARTESIAN_POINT('Ctrl Pts',(-1.84582736992532,70.7638578024727,12.5248350970751));
#53053=CARTESIAN_POINT('Ctrl Pts',(-1.83262171414446,70.7682343868168,12.4924393355125));
#53054=CARTESIAN_POINT('Ctrl Pts',(-1.81839550540839,70.7729492001864,12.4575399807359));
#53055=CARTESIAN_POINT('Ctrl Pts',(-1.80315332895003,70.777668016289,12.4230260852078));
#53056=CARTESIAN_POINT('Ctrl Pts',(-1.78690283692899,70.7823825107768,12.3889586203893));
#53057=CARTESIAN_POINT('Ctrl Pts',(-1.78690182115909,70.7823828054659,12.3889564909334));
#53058=CARTESIAN_POINT('Ctrl Pts',(-1.78690080538529,70.7823831001548,12.3889543614794));
#53059=CARTESIAN_POINT('Ctrl Pts',(-1.78689978960751,70.7823833948438,12.388952232027));
#53060=CARTESIAN_POINT('Ctrl Pts',(-1.74550545441033,70.7943923745589,12.3021741327641));
#53061=CARTESIAN_POINT('Ctrl Pts',(-1.6975318256225,70.8063799624736,12.218222764267));
#53062=CARTESIAN_POINT('Ctrl Pts',(-1.64368964950784,70.8183742497046,12.1379277482001));
#53063=CARTESIAN_POINT('Ctrl Pts',(-1.63290887041808,70.8207758569633,12.1218503365371));
#53064=CARTESIAN_POINT('Ctrl Pts',(-1.62189296865058,70.8231777298505,12.1059194580783));
#53065=CARTESIAN_POINT('Ctrl Pts',(-1.61064787764368,70.8255800893088,12.0901416761132));
#53066=CARTESIAN_POINT('Ctrl Pts',(-1.54009393665742,70.8406529710973,11.9911487291488));
#53067=CARTESIAN_POINT('Ctrl Pts',(-1.4605174170031,70.8557465159916,11.8981815621156));
#53068=CARTESIAN_POINT('Ctrl Pts',(-1.37328510870703,70.8709351750474,11.8127095566969));
#53069=CARTESIAN_POINT('Ctrl Pts',(-1.30099894827056,70.883521450325,11.7418820936019));
#53070=CARTESIAN_POINT('Ctrl Pts',(-1.22345672961429,70.8961742533405,11.6761972236881));
#53071=CARTESIAN_POINT('Ctrl Pts',(-1.14135866360981,70.9089326401881,11.6164470701242));
#53072=CARTESIAN_POINT('Ctrl Pts',(-1.12973467647591,70.9107390569746,11.6079872482298));
#53073=CARTESIAN_POINT('Ctrl Pts',(-1.11801931508906,70.9125475893433,11.5996464713191));
#53074=CARTESIAN_POINT('Ctrl Pts',(-1.10621452707645,70.9143583471047,11.5914270632553));
#53075=CARTESIAN_POINT('Ctrl Pts',(-1.10078039265814,70.9151918988011,11.5876433978298));
#53076=CARTESIAN_POINT('Ctrl Pts',(-1.09532728269988,70.9160259169017,11.5838854298758));
#53077=CARTESIAN_POINT('Ctrl Pts',(-1.08985537693032,70.9168604098746,11.5801533805886));
#53078=CARTESIAN_POINT('Ctrl Pts',(-1.01625744140572,70.9280844628101,11.5299567700513));
#53079=CARTESIAN_POINT('Ctrl Pts',(-0.93923646562749,70.9393967051461,11.4844380068382));
#53080=CARTESIAN_POINT('Ctrl Pts',(-0.859395350069275,70.9506694405085,
11.4441790152186));
#53081=CARTESIAN_POINT('Ctrl Pts',(-0.835028922366022,70.9541097267483,
11.4318925159401));
#53082=CARTESIAN_POINT('Ctrl Pts',(-0.810399897410274,70.9575463516296,
11.4200955467953));
#53083=CARTESIAN_POINT('Ctrl Pts',(-0.785525510500858,70.9609757349325,
11.4088036780356));
#53084=CARTESIAN_POINT('Ctrl Pts',(-0.762132153311586,70.9642009315509,
11.3981841311021));
#53085=CARTESIAN_POINT('Ctrl Pts',(-0.738523661806519,70.967419583261,11.3880122786022));
#53086=CARTESIAN_POINT('Ctrl Pts',(-0.714717770134932,70.9706286150032,
11.3783018029276));
#53087=CARTESIAN_POINT('Ctrl Pts',(-0.714716722865029,70.970628756175,11.3783013757439));
#53088=CARTESIAN_POINT('Ctrl Pts',(-0.714715675594629,70.9706288973469,
11.3783009485611));
#53089=CARTESIAN_POINT('Ctrl Pts',(-0.714714628323901,70.9706290385188,
11.3783005213791));
#53090=CARTESIAN_POINT('Ctrl Pts',(-0.637105405154823,70.9810907434083,
11.3466437036312));
#53091=CARTESIAN_POINT('Ctrl Pts',(-0.557226499885859,70.9914732155707,
11.3198241702613));
#53092=CARTESIAN_POINT('Ctrl Pts',(-0.475813234330459,71.0018390425587,
11.2979662624588));
#53093=CARTESIAN_POINT('Ctrl Pts',(-0.451818659763821,71.0048941172681,
11.291524177191));
#53094=CARTESIAN_POINT('Ctrl Pts',(-0.427691015240452,71.0079477337291,
11.285512798002));
#53095=CARTESIAN_POINT('Ctrl Pts',(-0.403449600131215,71.0110014624199,
11.2799345969682));
#53096=CARTESIAN_POINT('Ctrl Pts',(-0.295355884253575,71.0246181956008,
11.2550611118629));
#53097=CARTESIAN_POINT('Ctrl Pts',(-0.184991029156832,71.0383072748101,
11.2388246119196));
#53098=CARTESIAN_POINT('Ctrl Pts',(-0.07382045547731,71.0521996774235,11.2313724643906));
#53099=CARTESIAN_POINT('Ctrl Pts',(-0.0310994279747684,71.0575382998168,
11.2285087263617));
#53100=CARTESIAN_POINT('Ctrl Pts',(0.0117424070116354,71.0628810203524,
11.226930962945));
#53101=CARTESIAN_POINT('Ctrl Pts',(0.0546335509162594,71.0682293716919,
11.2266456339177));
#53102=CARTESIAN_POINT('Ctrl Pts',(0.165674313258151,71.082075703497,11.2259069463981));
#53103=CARTESIAN_POINT('Ctrl Pts',(0.277077544205819,71.0960740139967,11.2338758835229));
#53104=CARTESIAN_POINT('Ctrl Pts',(0.387446675908198,71.1102697790105,11.2507520614417));
#53105=CARTESIAN_POINT('Ctrl Pts',(0.469551691496286,71.1208301910547,11.2633064670959));
#53106=CARTESIAN_POINT('Ctrl Pts',(0.551086850323243,71.1314192058162,11.2807598778748));
#53107=CARTESIAN_POINT('Ctrl Pts',(0.631369457466356,71.1419445439166,11.3031163186117));
#53108=CARTESIAN_POINT('Ctrl Pts',(0.657909466524091,71.1454240344122,11.3105069622488));
#53109=CARTESIAN_POINT('Ctrl Pts',(0.684312800191152,71.1488965830908,11.3184330683517));
#53110=CARTESIAN_POINT('Ctrl Pts',(0.710555509033363,71.1523589076908,11.3268937387277));
#53111=CARTESIAN_POINT('Ctrl Pts',(0.737811912617902,71.1559549738288,11.3356812251017));
#53112=CARTESIAN_POINT('Ctrl Pts',(0.764893414727017,71.1595399798575,11.3450449920988));
#53113=CARTESIAN_POINT('Ctrl Pts',(0.791770462418447,71.1631103669693,11.3549821775479));
#53114=CARTESIAN_POINT('Ctrl Pts',(0.791775501359393,71.1631110363497,11.3549840405833));
#53115=CARTESIAN_POINT('Ctrl Pts',(0.791780540293847,71.1631117057296,11.3549859036391));
#53116=CARTESIAN_POINT('Ctrl Pts',(0.791785579221842,71.163112375109,11.3549877667152));
#53117=CARTESIAN_POINT('Ctrl Pts',(0.872396842029561,71.1738209065673,11.3847927009848));
#53118=CARTESIAN_POINT('Ctrl Pts',(0.951351908195907,71.1843979836468,11.419813974218));
#53119=CARTESIAN_POINT('Ctrl Pts',(1.02801671639817,71.194959265503,11.4596562735348));
#53120=CARTESIAN_POINT('Ctrl Pts',(1.05011940307327,71.1980041137095,11.4711429240445));
#53121=CARTESIAN_POINT('Ctrl Pts',(1.07203165928233,71.2010476242585,11.4830299669435));
#53122=CARTESIAN_POINT('Ctrl Pts',(1.09373817003166,71.2040925074142,11.4953071389792));
#53123=CARTESIAN_POINT('Ctrl Pts',(1.17076089443873,71.2148968784554,11.5388710838769));
#53124=CARTESIAN_POINT('Ctrl Pts',(1.24514461388718,71.2259201288154,11.5874360518204));
#53125=CARTESIAN_POINT('Ctrl Pts',(1.31641777296803,71.2369917159873,11.6404960142158));
#53126=CARTESIAN_POINT('Ctrl Pts',(1.32787419490414,71.2387713589242,11.6490248534725));
#53127=CARTESIAN_POINT('Ctrl Pts',(1.33925031396308,71.2405522626534,11.6576699179167));
#53128=CARTESIAN_POINT('Ctrl Pts',(1.3505442430379,71.2423337327342,11.6664292093449));
#53129=CARTESIAN_POINT('Ctrl Pts',(1.42865171810356,71.2546541686949,11.7270074308202));
#53130=CARTESIAN_POINT('Ctrl Pts',(1.50285916325863,71.2670061407611,11.7930685481099));
#53131=CARTESIAN_POINT('Ctrl Pts',(1.57240659892121,71.2794577260796,11.8640979704692));
#53132=CARTESIAN_POINT('Ctrl Pts',(1.5811968343051,71.2810315061163,11.8730755170282));
#53133=CARTESIAN_POINT('Ctrl Pts',(1.58991256127224,71.2826068747412,11.8821324528914));
#53134=CARTESIAN_POINT('Ctrl Pts',(1.59855218723446,71.2841839670128,11.8912677546883));
#53135=CARTESIAN_POINT('Ctrl Pts',(1.65899979691212,71.2952181782716,11.9551833871148));
#53136=CARTESIAN_POINT('Ctrl Pts',(1.71568819992305,71.3064094743598,12.0229634916327));
#53137=CARTESIAN_POINT('Ctrl Pts',(1.76808256701075,71.3176009568167,12.0940940114363));
#53138=CARTESIAN_POINT('Ctrl Pts',(1.78201294070464,71.3205764967741,12.1130058673663));
#53139=CARTESIAN_POINT('Ctrl Pts',(1.79564005369749,71.3235520771964,12.1321545766696));
#53140=CARTESIAN_POINT('Ctrl Pts',(1.80895447139048,71.3265248094507,12.1515305530256));
#53141=CARTESIAN_POINT('Ctrl Pts',(1.85328472667293,71.3364224995154,12.2160427230665));
#53142=CARTESIAN_POINT('Ctrl Pts',(1.89414300930226,71.346287426131,12.2830723463133));
#53143=CARTESIAN_POINT('Ctrl Pts',(1.93114510948473,71.3560608208897,12.3522197824008));
#53144=CARTESIAN_POINT('Ctrl Pts',(1.93611964086167,71.3573747479005,12.3615159058305));
#53145=CARTESIAN_POINT('Ctrl Pts',(1.94102455125582,71.35868702262,12.3708502887935));
#53146=CARTESIAN_POINT('Ctrl Pts',(1.94585897866666,71.3599975041675,12.3802219460974));
#53147=CARTESIAN_POINT('Ctrl Pts',(1.94585962985694,71.3599976806874,12.3802232084459));
#53148=CARTESIAN_POINT('Ctrl Pts',(1.94586028104596,71.3599978572073,12.3802244707951));
#53149=CARTESIAN_POINT('Ctrl Pts',(1.94586093223373,71.3599980337272,12.380225733145));
#53150=CARTESIAN_POINT('Ctrl Pts',(1.98619576175937,71.370931744641,12.4584161888338));
#53151=CARTESIAN_POINT('Ctrl Pts',(2.0217086491527,71.3817242349857,12.539322072039));
#53152=CARTESIAN_POINT('Ctrl Pts',(2.05217280790861,71.3925449886504,12.6222710572936));
#53153=CARTESIAN_POINT('Ctrl Pts',(2.06038003658161,71.3954601651518,12.6446180157517));
#53154=CARTESIAN_POINT('Ctrl Pts',(2.06822080311025,71.3983773562506,12.6671129733622));
#53155=CARTESIAN_POINT('Ctrl Pts',(2.07569065099517,71.4012997935818,12.6897421371436));
#53156=CARTESIAN_POINT('Ctrl Pts',(2.09153592110757,71.4074989571544,12.7377438124197));
#53157=CARTESIAN_POINT('Ctrl Pts',(2.10565957213874,71.4138124411617,12.7863718679594));
#53158=CARTESIAN_POINT('Ctrl Pts',(2.11810832935687,71.4201325350876,12.8354888385054));
#53159=CARTESIAN_POINT('Ctrl Pts',(2.14267259448761,71.4326035360179,12.9324079337828));
#53160=CARTESIAN_POINT('Ctrl Pts',(2.16072569386879,71.4451031594844,13.0312526015205));
#53161=CARTESIAN_POINT('Ctrl Pts',(2.17208083446691,71.4576591703852,13.1311612395562));
#53162=CARTESIAN_POINT('Ctrl Pts',(2.17359503021924,71.4593335008972,13.1444839486876));
#53163=CARTESIAN_POINT('Ctrl Pts',(2.17499004738872,71.4610088333506,13.1578255752569));
#53164=CARTESIAN_POINT('Ctrl Pts',(2.17626537266087,71.462685232893,13.1711840706296));
#53165=CARTESIAN_POINT('Ctrl Pts',(2.18527813737428,71.474532402373,13.2655889870447));
#53166=CARTESIAN_POINT('Ctrl Pts',(2.18821857238941,71.4865700961145,13.3608429088672));
#53167=CARTESIAN_POINT('Ctrl Pts',(2.18501020941626,71.4986391581974,13.4560936714542));
#53168=CARTESIAN_POINT('Ctrl Pts',(2.18434840391752,71.5011287055828,13.4757415351674));
#53169=CARTESIAN_POINT('Ctrl Pts',(2.18342506209214,71.5036196100868,13.4953894145309));
#53170=CARTESIAN_POINT('Ctrl Pts',(2.18223963969097,71.5061105101725,13.5150300748985));
#53171=CARTESIAN_POINT('Ctrl Pts',(2.17691261588212,71.5173040594499,13.6032908208534));
#53172=CARTESIAN_POINT('Ctrl Pts',(2.16629030045941,71.5284959395751,13.6914037443961));
#53173=CARTESIAN_POINT('Ctrl Pts',(2.15030415455817,71.5396240769922,13.7786439086661));
#53174=CARTESIAN_POINT('Ctrl Pts',(2.14578077443653,71.5427728531822,13.8033290596278));
#53175=CARTESIAN_POINT('Ctrl Pts',(2.1408282253218,71.545916538471,13.8279444804834));
#53176=CARTESIAN_POINT('Ctrl Pts',(2.13544561019691,71.549053756753,13.8524741441037));
#53177=CARTESIAN_POINT('Ctrl Pts',(2.12803121764441,71.5533751818086,13.8862630275815));
#53178=CARTESIAN_POINT('Ctrl Pts',(2.11980078157287,71.5576844542003,13.9198879844507));
#53179=CARTESIAN_POINT('Ctrl Pts',(2.11075327030379,71.5619785174693,13.953304851992));
#53180=CARTESIAN_POINT('Ctrl Pts',(2.11075235061384,71.5619789539657,13.9533082488551));
#53181=CARTESIAN_POINT('Ctrl Pts',(2.11075143091544,71.561979390462,13.9533116457163));
#53182=CARTESIAN_POINT('Ctrl Pts',(2.11075051120861,71.5619798269581,13.9533150425754));
#53183=CARTESIAN_POINT('Ctrl Pts',(2.08957577910432,71.5720294291065,14.0315221186651));
#53184=CARTESIAN_POINT('Ctrl Pts',(2.06392338841043,71.5819768958523,14.1086902093775));
#53185=CARTESIAN_POINT('Ctrl Pts',(2.03396025847612,71.5919861059351,14.1843500081339));
#53186=CARTESIAN_POINT('Ctrl Pts',(2.02376865458318,71.5953906202388,14.2100847928923));
#53187=CARTESIAN_POINT('Ctrl Pts',(2.0130784186635,71.5988022211228,14.2356446483217));
#53188=CARTESIAN_POINT('Ctrl Pts',(2.00189651879196,71.6022271799728,14.261009792523));
#53189=CARTESIAN_POINT('Ctrl Pts',(1.95863636229423,71.6154775450764,14.3591416055727));
#53190=CARTESIAN_POINT('Ctrl Pts',(1.90804853165839,71.6288708767552,14.4544124267342));
#53191=CARTESIAN_POINT('Ctrl Pts',(1.85078153392663,71.6423234260279,14.5459243130061));
#53192=CARTESIAN_POINT('Ctrl Pts',(1.83853215476964,71.6452009188806,14.5654986548908));
#53193=CARTESIAN_POINT('Ctrl Pts',(1.82597700665506,71.6480811400064,14.5849010797434));
#53194=CARTESIAN_POINT('Ctrl Pts',(1.81312214043868,71.6509633009607,14.6041228878331));
#53195=CARTESIAN_POINT('Ctrl Pts',(1.74555966945489,71.666111332264,14.7051486651113));
#53196=CARTESIAN_POINT('Ctrl Pts',(1.66963839935241,71.6814304867716,14.801130603571));
#53197=CARTESIAN_POINT('Ctrl Pts',(1.58630743542294,71.6968001766533,14.8906800925929));
#53198=CARTESIAN_POINT('Ctrl Pts',(1.57847428137015,71.6982449355149,14.8990977912463));
#53199=CARTESIAN_POINT('Ctrl Pts',(1.57057564463731,71.6996901464177,14.9074586885919));
#53200=CARTESIAN_POINT('Ctrl Pts',(1.56261230585935,71.7011357126583,14.9157616535523));
#53201=CARTESIAN_POINT('Ctrl Pts',(1.49019630791816,71.7142812191883,14.991266100901));
#53202=CARTESIAN_POINT('Ctrl Pts',(1.41243396089567,71.7274470391968,15.0619806279928));
#53203=CARTESIAN_POINT('Ctrl Pts',(1.3299595783442,71.7405764813823,15.1270113030264));
#53204=CARTESIAN_POINT('Ctrl Pts',(1.307680840418,71.7441231269287,15.1445779864185));
#53205=CARTESIAN_POINT('Ctrl Pts',(1.28505835030234,71.747667133117,15.1617302002453));
#53206=CARTESIAN_POINT('Ctrl Pts',(1.26210475420861,71.7512074164063,15.1784509681943));
#53207=CARTESIAN_POINT('Ctrl Pts',(1.2238596562881,71.7571062080603,15.2063109777939));
#53208=CARTESIAN_POINT('Ctrl Pts',(1.18469629591523,71.7629947807052,15.232971940542));
#53209=CARTESIAN_POINT('Ctrl Pts',(1.14467692932067,71.768868991772,15.2583540662385));
#53210=CARTESIAN_POINT('Ctrl Pts',(1.14467076444827,71.7688698966779,15.2583579762845));
#53211=CARTESIAN_POINT('Ctrl Pts',(1.14466459955562,71.7688708015835,15.2583618863002));
#53212=CARTESIAN_POINT('Ctrl Pts',(1.1446584346426,71.7688717064887,15.2583657962856));
#53213=CARTESIAN_POINT('Ctrl Pts',(1.10071341999499,71.7753220933381,15.2862371325845));
#53214=CARTESIAN_POINT('Ctrl Pts',(1.05571839411559,71.7817545254206,15.3125819795612));
#53215=CARTESIAN_POINT('Ctrl Pts',(1.00978071557335,71.7882093696722,15.3373356118852));
#53216=CARTESIAN_POINT('Ctrl Pts',(0.880191475056821,71.8064183517271,15.4071650964105));
#53217=CARTESIAN_POINT('Ctrl Pts',(0.743087453138814,71.8248188944842,15.4643302827042));
#53218=CARTESIAN_POINT('Ctrl Pts',(0.601240848352391,71.843353052873,15.5081262725566));
#53219=CARTESIAN_POINT('Ctrl Pts',(0.459347343337411,71.8618933394046,15.5519367431357));
#53220=CARTESIAN_POINT('Ctrl Pts',(0.312700705102145,71.8805844082547,15.5823503811493));
#53221=CARTESIAN_POINT('Ctrl Pts',(0.1641159504501,71.899352922242,15.5986382270688));
#53222=CARTESIAN_POINT('Ctrl Pts',(0.0321111188423181,71.916027139824,15.6131085834852));
#53223=CARTESIAN_POINT('Ctrl Pts',(-0.101423215562088,71.932761667862,15.6164281715104));
#53224=CARTESIAN_POINT('Ctrl Pts',(-0.234482419868063,71.9494967982338,
15.6081083003707));
#53225=CARTESIAN_POINT('Ctrl Pts',(-0.243288383689666,71.9506043424535,
15.6075576846907));
#53226=CARTESIAN_POINT('Ctrl Pts',(-0.252092280033786,71.9517118910096,
15.6069561026561));
#53227=CARTESIAN_POINT('Ctrl Pts',(-0.260893533916475,71.9528194273214,
15.6063034180066));
#53228=CARTESIAN_POINT('Ctrl Pts',(-0.330418216456274,71.9615683069137,
15.6011475966137));
#53229=CARTESIAN_POINT('Ctrl Pts',(-0.399776517792103,71.9703161707563,
15.5928027171852));
#53230=CARTESIAN_POINT('Ctrl Pts',(-0.468680029306107,71.9790543660095,
15.5812047536984));
#53231=CARTESIAN_POINT('Ctrl Pts',(-0.476242589928811,71.9800134336953,
15.5799318098376));
#53232=CARTESIAN_POINT('Ctrl Pts',(-0.483799671584185,71.9809723852518,
15.5786196828546));
#53233=CARTESIAN_POINT('Ctrl Pts',(-0.491350900777853,71.9819310858116,
15.5772684232766));
#53234=CARTESIAN_POINT('Ctrl Pts',(-0.491355026516865,71.9819316096135,
15.5772676849936));
#53235=CARTESIAN_POINT('Ctrl Pts',(-0.491359152254362,71.9819321334154,
15.5772669466988));
#53236=CARTESIAN_POINT('Ctrl Pts',(-0.491363277990312,71.9819326572172,
15.5772662083924));
#53237=CARTESIAN_POINT('Ctrl Pts',(-0.599984076087746,71.9957231110571,
15.5578283581625));
#53238=CARTESIAN_POINT('Ctrl Pts',(-0.707545851576862,72.0094797114707,
15.5302639013997));
#53239=CARTESIAN_POINT('Ctrl Pts',(-0.812963944553361,72.0232380427708,
15.4950649743857));
#53240=CARTESIAN_POINT('Ctrl Pts',(-0.855848862106878,72.0288350412254,
15.480745771293));
#53241=CARTESIAN_POINT('Ctrl Pts',(-0.898378762592077,72.0344322873196,
15.4651636734896));
#53242=CARTESIAN_POINT('Ctrl Pts',(-0.940479812768093,72.0400320146097,
15.4483541203874));
#53243=CARTESIAN_POINT('Ctrl Pts',(-1.05991870548102,72.0559182032971,15.400666131581));
#53244=CARTESIAN_POINT('Ctrl Pts',(-1.17585534434287,72.0719457058116,15.342970078193));
#53245=CARTESIAN_POINT('Ctrl Pts',(-1.286696153303,72.0880627897628,15.2761931399249));
#53246=CARTESIAN_POINT('Ctrl Pts',(-1.31543473728105,72.0922415951591,15.2588793484953));
#53247=CARTESIAN_POINT('Ctrl Pts',(-1.34383101040018,72.0964264420064,15.240955182115));
#53248=CARTESIAN_POINT('Ctrl Pts',(-1.37185775388227,72.1006164696211,15.2224369452993));
#53249=CARTESIAN_POINT('Ctrl Pts',(-1.48286036129561,72.117211476125,15.1490936911122));
#53250=CARTESIAN_POINT('Ctrl Pts',(-1.58809465719197,72.1338459986869,15.066477464604));
#53251=CARTESIAN_POINT('Ctrl Pts',(-1.68595660883222,72.1505301337724,14.9754582562636));
#53252=CARTESIAN_POINT('Ctrl Pts',(-1.70681201011313,72.1540856967506,14.9560611148578));
#53253=CARTESIAN_POINT('Ctrl Pts',(-1.72733249353319,72.1576435137915,14.9362821807924));
#53254=CARTESIAN_POINT('Ctrl Pts',(-1.74750235772902,72.1612036840118,14.9161296223245));
#53255=CARTESIAN_POINT('Ctrl Pts',(-1.77049418539539,72.1652619572543,14.8931575216287));
#53256=CARTESIAN_POINT('Ctrl Pts',(-1.79303100671763,72.1693233872736,14.8696993952342));
#53257=CARTESIAN_POINT('Ctrl Pts',(-1.81508151286912,72.1733973014865,14.8457586729703));
#53258=CARTESIAN_POINT('Ctrl Pts',(-1.85712541155155,72.181165070409,14.8001106822016));
#53259=CARTESIAN_POINT('Ctrl Pts',(-1.89732243389114,72.1890650989457,14.752631215339));
#53260=CARTESIAN_POINT('Ctrl Pts',(-1.93561044495043,72.1969626246315,14.7035378686259));
#53261=CARTESIAN_POINT('Ctrl Pts',(-1.94050771329313,72.1979727659644,14.6972585324566));
#53262=CARTESIAN_POINT('Ctrl Pts',(-1.94537380547937,72.1989828749059,14.6909527511329));
#53263=CARTESIAN_POINT('Ctrl Pts',(-1.95020863905481,72.1999926770107,14.6846209413863));
#53264=CARTESIAN_POINT('Ctrl Pts',(-1.95021287859332,72.1999935624797,14.6846153891888));
#53265=CARTESIAN_POINT('Ctrl Pts',(-1.95021711810784,72.1999944479484,14.6846098369711));
#53266=CARTESIAN_POINT('Ctrl Pts',(-1.95022135759829,72.1999953334168,14.6846042847335));
#53267=CARTESIAN_POINT('Ctrl Pts',(-2.02012671004489,72.2145959052262,14.5930529221521));
#53268=CARTESIAN_POINT('Ctrl Pts',(-2.08350271444183,72.2291185208218,14.4960806229705));
#53269=CARTESIAN_POINT('Ctrl Pts',(-2.13981592348098,72.2436382301198,14.3948233216095));
#53270=CARTESIAN_POINT('Ctrl Pts',(-2.15568285604744,72.247729335071,14.3662928435925));
#53271=CARTESIAN_POINT('Ctrl Pts',(-2.17098883835595,72.2518201700969,14.3374223900523));
#53272=CARTESIAN_POINT('Ctrl Pts',(-2.18572142668799,72.2559123209899,14.3082379124049));
#53273=CARTESIAN_POINT('Ctrl Pts',(-2.18572719673364,72.2559139236885,14.3082264822498));
#53274=CARTESIAN_POINT('Ctrl Pts',(-2.18573296669124,72.2559155263873,14.3082150520466));
#53275=CARTESIAN_POINT('Ctrl Pts',(-2.18573873656072,72.2559171290863,14.3082036217953));
#53276=CARTESIAN_POINT('Ctrl Pts',(-2.23476047601701,72.2695339182556,14.2110903674256));
#53277=CARTESIAN_POINT('Ctrl Pts',(-2.27742353843653,72.2831703516847,14.1105036799087));
#53278=CARTESIAN_POINT('Ctrl Pts',(-2.31321095092577,72.296784221078,14.0072753291497));
#53279=CARTESIAN_POINT('Ctrl Pts',(-2.32634447211919,72.3017803364651,13.9693918489494));
#53280=CARTESIAN_POINT('Ctrl Pts',(-2.33855163565415,72.3067734455887,13.9311528495216));
#53281=CARTESIAN_POINT('Ctrl Pts',(-2.34980584038207,72.3117616912306,13.8926004503245));
#53282=CARTESIAN_POINT('Ctrl Pts',(-2.34980928625165,72.311763218557,13.892588646155));
#53283=CARTESIAN_POINT('Ctrl Pts',(-2.34981273203262,72.3117647458824,13.8925768419563));
#53284=CARTESIAN_POINT('Ctrl Pts',(-2.34981617772495,72.3117662732069,13.8925650377283));
#53285=CARTESIAN_POINT('Ctrl Pts',(-2.37274164238379,72.3219281275906,13.8140271459381));
#53286=CARTESIAN_POINT('Ctrl Pts',(-2.39174539427942,72.332048545218,13.7341892736926));
#53287=CARTESIAN_POINT('Ctrl Pts',(-2.4066798856095,72.3422167273012,13.6534209894091));
#53288=CARTESIAN_POINT('Ctrl Pts',(-2.41905169904031,72.3506401043606,13.5865121056583));
#53289=CARTESIAN_POINT('Ctrl Pts',(-2.4286303555641,72.3590961491279,13.5189655055544));
#53290=CARTESIAN_POINT('Ctrl Pts',(-2.43532692904267,72.367632225426,13.4510177600665));
#53291=CARTESIAN_POINT('Ctrl Pts',(-2.43532751033381,72.3676329663938,13.4510118619124));
#53292=CARTESIAN_POINT('Ctrl Pts',(-2.43532809160323,72.3676337073623,13.4510059637553));
#53293=CARTESIAN_POINT('Ctrl Pts',(-2.43532867285094,72.3676344483313,13.4510000655951));
#53294=CARTESIAN_POINT('Ctrl Pts',(-2.43685242895941,72.3695769180901,13.4355378840728));
#53295=CARTESIAN_POINT('Ctrl Pts',(-2.43822752235068,72.3715229059429,13.4200562506372));
#53296=CARTESIAN_POINT('Ctrl Pts',(-2.43945255372853,72.373472621177,13.4045578859649));
#53297=CARTESIAN_POINT('Ctrl Pts',(-2.4455198139933,72.3831290511928,13.3277985360858));
#53298=CARTESIAN_POINT('Ctrl Pts',(-2.44790520255198,72.3928785634079,13.2506233464808));
#53299=CARTESIAN_POINT('Ctrl Pts',(-2.44659781380402,72.4026310200357,13.1734055148817));
#53300=CARTESIAN_POINT('Ctrl Pts',(-2.44633392768895,72.4045994765455,13.1578197041377));
#53301=CARTESIAN_POINT('Ctrl Pts',(-2.44591959423343,72.4065680740621,13.1422319876076));
#53302=CARTESIAN_POINT('Ctrl Pts',(-2.44535470772765,72.408536103423,13.1266451784564));
#53303=CARTESIAN_POINT('Ctrl Pts',(-2.44380192716608,72.4139458940714,13.0837995908572));
#53304=CARTESIAN_POINT('Ctrl Pts',(-2.44111186504103,72.4193508130069,13.0409635853769));
#53305=CARTESIAN_POINT('Ctrl Pts',(-2.43728466864259,72.4247344546358,12.9982043293178));
#53306=CARTESIAN_POINT('Ctrl Pts',(-2.43728253046173,72.4247374623726,12.9981804405456));
#53307=CARTESIAN_POINT('Ctrl Pts',(-2.43728039192522,72.4247404701038,12.9981565517893));
#53308=CARTESIAN_POINT('Ctrl Pts',(-2.43727825303304,72.4247434778295,12.9981326630488));
#53309=CARTESIAN_POINT('Ctrl Pts',(-2.42898557216907,72.43640470559,12.9055138282334));
#53310=CARTESIAN_POINT('Ctrl Pts',(-2.41534357920754,72.4479824797458,12.8131291710771));
#53311=CARTESIAN_POINT('Ctrl Pts',(-2.3964964848232,72.4595253844034,12.7215935711713));
#53312=CARTESIAN_POINT('Ctrl Pts',(-2.38767962564182,72.4649252706052,12.6787723023861));
#53313=CARTESIAN_POINT('Ctrl Pts',(-2.3777241637851,72.4703174560377,12.6361373888414));
#53314=CARTESIAN_POINT('Ctrl Pts',(-2.36664778503021,72.4757065424221,12.5937543546988));
#53315=CARTESIAN_POINT('Ctrl Pts',(-2.33923788833977,72.4890425165993,12.4888721894186));
#53316=CARTESIAN_POINT('Ctrl Pts',(-2.30482530756836,72.5024462168457,12.3855591051039));
#53317=CARTESIAN_POINT('Ctrl Pts',(-2.26370876476586,72.5159725324142,12.2847530831423));
#53318=CARTESIAN_POINT('Ctrl Pts',(-2.25166244364125,72.5199354711699,12.2552189436191));
#53319=CARTESIAN_POINT('Ctrl Pts',(-2.23904084444868,72.5239088908104,12.2259002943049));
#53320=CARTESIAN_POINT('Ctrl Pts',(-2.22585196595221,72.5278940616467,12.1968214169595));
#53321=CARTESIAN_POINT('Ctrl Pts',(-2.18333437932186,72.5407412378729,12.1030785193374));
#53322=CARTESIAN_POINT('Ctrl Pts',(-2.13508628031869,72.5536090363629,12.0117609457507));
#53323=CARTESIAN_POINT('Ctrl Pts',(-2.08136896746144,72.5665109076533,11.9234977558));
#53324=CARTESIAN_POINT('Ctrl Pts',(-2.06607621375076,72.570183934645,11.8983701544022));
#53325=CARTESIAN_POINT('Ctrl Pts',(-2.05033990200067,72.5738597246151,11.8734902495142));
#53326=CARTESIAN_POINT('Ctrl Pts',(-2.03416539392586,72.5775385913636,11.8488729526678));
#53327=CARTESIAN_POINT('Ctrl Pts',(1.35925139903161,68.5015684297319,11.2018017462371));
#53328=CARTESIAN_POINT('Ctrl Pts',(1.81201504569449,68.5705202281901,11.5183578934431));
#53329=CARTESIAN_POINT('Ctrl Pts',(2.4871255928394,68.7068329045687,12.4537467086246));
#53330=CARTESIAN_POINT('Ctrl Pts',(2.42336085847789,68.9065763946622,14.1441642030493));
#53331=CARTESIAN_POINT('Ctrl Pts',(1.35774589260468,69.1016690675509,15.4062116397971));
#53332=CARTESIAN_POINT('Ctrl Pts',(-0.221166469575229,69.2922152826969,
15.7370705160361));
#53333=CARTESIAN_POINT('Ctrl Pts',(-1.63549669696357,69.4783571664629,15.0420008198722));
#53334=CARTESIAN_POINT('Ctrl Pts',(-2.3066978913788,69.6602591510739,13.6560348131309));
#53335=CARTESIAN_POINT('Ctrl Pts',(-1.98918266931016,69.8381154442101,12.1835559119558));
#53336=CARTESIAN_POINT('Ctrl Pts',(-0.900255468145694,70.0057067926906,
11.274956447888));
#53337=CARTESIAN_POINT('Ctrl Pts',(0.420880950868389,70.1637298446908,11.183392327644));
#53338=CARTESIAN_POINT('Ctrl Pts',(1.50237204011775,70.3127965825961,11.8007288591049));
#53339=CARTESIAN_POINT('Ctrl Pts',(2.14764777535062,70.483880181877,13.0834385708106));
#53340=CARTESIAN_POINT('Ctrl Pts',(1.68418285768135,70.6757162506824,14.7103694985184));
#53341=CARTESIAN_POINT('Ctrl Pts',(-0.0330782420554639,70.8873605170864,
15.4592990478547));
#53342=CARTESIAN_POINT('Ctrl Pts',(-1.6707310055211,71.0956282386167,14.6202665191846));
#53343=CARTESIAN_POINT('Ctrl Pts',(-2.06050794163202,71.3014160745871,12.8448001592972));
#53344=CARTESIAN_POINT('Ctrl Pts',(-0.939643177328641,71.5056429104108,
11.4241772577033));
#53345=CARTESIAN_POINT('Ctrl Pts',(0.405518300920993,71.658307121143,11.3989157803725));
#53346=CARTESIAN_POINT('Ctrl Pts',(1.112140023751,71.7601738993637,11.8201165612096));
#53347=CARTESIAN_POINT('Ctrl Pts',(1.41249129287616,71.8111398715806,12.0998255829605));
#53348=CARTESIAN_POINT('Ctrl Pts',(1.64338713283149,71.8621472327744,12.4403692775591));
#53349=CARTESIAN_POINT('Ctrl Pts',(1.89705351737498,71.9472687575764,13.0780800622876));
#53350=CARTESIAN_POINT('Ctrl Pts',(1.83265904354054,72.0667825484646,14.0874300328648));
#53351=CARTESIAN_POINT('Ctrl Pts',(0.96215776514328,72.2215130192343,15.0670008052881));
#53352=CARTESIAN_POINT('Ctrl Pts',(-0.337956441766793,72.3776743394961,
15.3063172669432));
#53353=CARTESIAN_POINT('Ctrl Pts',(-1.52424768912109,72.5356499306958,14.6886989506691));
#53354=CARTESIAN_POINT('Ctrl Pts',(-2.08756836957837,72.6957944328977,13.4555231657513));
#53355=CARTESIAN_POINT('Ctrl Pts',(-1.76878172405223,72.8584427198578,12.1159502014204));
#53356=CARTESIAN_POINT('Ctrl Pts',(-0.674972234182401,73.0239265058316,
11.2404721033924));
#53357=CARTESIAN_POINT('Ctrl Pts',(0.752502222318795,73.192553636038,11.222102813825));
#53358=CARTESIAN_POINT('Ctrl Pts',(1.9128224007105,73.3646026686541,12.1029513221996));
#53359=CARTESIAN_POINT('Ctrl Pts',(2.29555630198192,73.5403436305485,13.5401202935886));
#53360=CARTESIAN_POINT('Ctrl Pts',(1.69942781075577,73.7200063918782,14.9399925255078));
#53361=CARTESIAN_POINT('Ctrl Pts',(0.33633086029822,73.9038061569606,15.6934571496578));
#53362=CARTESIAN_POINT('Ctrl Pts',(-1.23229046294891,74.0919248239957,15.4456602078211));
#53363=CARTESIAN_POINT('Ctrl Pts',(-2.48091999765483,74.3059137887571,14.1213831739387));
#53364=CARTESIAN_POINT('Ctrl Pts',(-2.44805375166388,74.5038696724368,12.3829147385172));
#53365=CARTESIAN_POINT('Ctrl Pts',(-1.56312085739856,74.6726204857052,11.3087811705623));
#53366=CARTESIAN_POINT('Ctrl Pts',(-0.992890126921472,74.7523693988593,
11.0014174397873));
#53367=CARTESIAN_POINT('Ctrl Pts',(-0.733503873481175,74.78666297405,10.9114679132036));
#53368=CARTESIAN_POINT('Ctrl Pts',(1.19498081016287,82.2340164369994,10.482675015848));
#53369=CARTESIAN_POINT('Ctrl Pts',(1.72598823950189,82.3066323787876,10.7204975998541));
#53370=CARTESIAN_POINT('Ctrl Pts',(2.62667932021033,82.4489632634736,11.4943972620624));
#53371=CARTESIAN_POINT('Ctrl Pts',(3.13961817930498,82.6588420064339,13.1654943300609));
#53372=CARTESIAN_POINT('Ctrl Pts',(2.70364992086808,82.8640080375243,14.8177084226806));
#53373=CARTESIAN_POINT('Ctrl Pts',(1.47859444808645,83.0663675786054,15.9753243882897));
#53374=CARTESIAN_POINT('Ctrl Pts',(-0.148581296960598,83.265798455397,16.3080276235447));
#53375=CARTESIAN_POINT('Ctrl Pts',(-1.68357605211574,83.4621940706116,15.7402832040705));
#53376=CARTESIAN_POINT('Ctrl Pts',(-2.67007897214778,83.655461159339,14.4707656858787));
#53377=CARTESIAN_POINT('Ctrl Pts',(-2.85891941300041,83.8666402933621,12.7190213299314));
#53378=CARTESIAN_POINT('Ctrl Pts',(-1.84603430281946,84.0942739879358,11.0522678886856));
#53379=CARTESIAN_POINT('Ctrl Pts',(0.151482086621562,84.336683926515,10.4633967604406));
#53380=CARTESIAN_POINT('Ctrl Pts',(1.97167797911635,84.5731173043586,11.3592888645195));
#53381=CARTESIAN_POINT('Ctrl Pts',(2.69573223495876,84.8035699798368,13.2004961804263));
#53382=CARTESIAN_POINT('Ctrl Pts',(1.99918277764129,85.0280847473626,14.9997242915337));
#53383=CARTESIAN_POINT('Ctrl Pts',(0.460113177574641,85.2285334817215,15.7643099300201));
#53384=CARTESIAN_POINT('Ctrl Pts',(-0.997754222001919,85.406604631475,15.4897739817101));
#53385=CARTESIAN_POINT('Ctrl Pts',(-2.04757701996071,85.5768355775209,14.5349258191164));
#53386=CARTESIAN_POINT('Ctrl Pts',(-2.30990438101913,85.7305593231813,13.2552846444736));
#53387=CARTESIAN_POINT('Ctrl Pts',(-1.88543687624611,85.8813849837293,12.0945359749286));
#53388=CARTESIAN_POINT('Ctrl Pts',(-1.04530190918308,86.017391015636,11.3343139025098));
#53389=CARTESIAN_POINT('Ctrl Pts',(-0.0516858839223906,86.1388075906432,
11.1567759640611));
#53390=CARTESIAN_POINT('Ctrl Pts',(1.0831281897424,86.2826143370863,11.4262298525765));
#53391=CARTESIAN_POINT('Ctrl Pts',(1.94436773624321,86.4239758161431,12.3037970364228));
#53392=CARTESIAN_POINT('Ctrl Pts',(2.05173254243784,86.5856935562115,13.6502755336076));
#53393=CARTESIAN_POINT('Ctrl Pts',(1.53497337091036,86.7222956550306,14.6619025754067));
#53394=CARTESIAN_POINT('Ctrl Pts',(0.572769711474274,86.8570741630587,15.241996329925));
#53395=CARTESIAN_POINT('Ctrl Pts',(-0.443480299089395,86.9791287379262,
15.2286754209456));
#53396=CARTESIAN_POINT('Ctrl Pts',(-1.0756340334284,87.067071681156,14.8834129767296));
#53397=CARTESIAN_POINT('Ctrl Pts',(-1.57789463619398,87.1545918000081,14.391654854311));
#53398=CARTESIAN_POINT('Ctrl Pts',(-1.93160007404001,87.2524891088848,13.6570681730652));
#53399=CARTESIAN_POINT('Ctrl Pts',(-1.8143716581144,87.3820297380612,12.5849378774665));
#53400=CARTESIAN_POINT('Ctrl Pts',(-1.08170690016791,87.5251166129853,11.6442906211455));
#53401=CARTESIAN_POINT('Ctrl Pts',(0.215983600329857,87.6817468300896,11.298789702101));
#53402=CARTESIAN_POINT('Ctrl Pts',(1.51453851662001,87.8522043046485,11.9740541069845));
#53403=CARTESIAN_POINT('Ctrl Pts',(2.01541164598604,88.022810735053,13.3507388599802));
#53404=CARTESIAN_POINT('Ctrl Pts',(1.45918555813443,88.19409616606,14.7109522605905));
#53405=CARTESIAN_POINT('Ctrl Pts',(0.118244489973287,88.366622968629,15.3433638174458));
#53406=CARTESIAN_POINT('Ctrl Pts',(-1.31110040792424,88.5408973526556,14.9039500226772));
#53407=CARTESIAN_POINT('Ctrl Pts',(-2.08169099810388,88.7174617667036,13.5973159668313));
#53408=CARTESIAN_POINT('Ctrl Pts',(-1.81686385850973,88.8669016282602,12.3443338848999));
#53409=CARTESIAN_POINT('Ctrl Pts',(-1.13020678008131,88.9880846501656,11.6322033391202));
#53410=CARTESIAN_POINT('Ctrl Pts',(-0.566646546821027,89.0645455077854,
11.369180962554));
#53411=CARTESIAN_POINT('Ctrl Pts',(0.169750362747802,89.1569914263112,11.2509573070016));
#53412=CARTESIAN_POINT('Ctrl Pts',(1.00960082538348,89.2607654928535,11.4321878451837));
#53413=CARTESIAN_POINT('Ctrl Pts',(2.08830318520032,89.4346617692564,12.3934859611261));
#53414=CARTESIAN_POINT('Ctrl Pts',(2.24388338663252,89.600432357722,13.8708609404721));
#53415=CARTESIAN_POINT('Ctrl Pts',(1.58763714078365,89.7383934335917,14.8013457360256));
#53416=CARTESIAN_POINT('Ctrl Pts',(0.967463015391611,89.8386609176866,15.3110237752385));
#53417=CARTESIAN_POINT('Ctrl Pts',(0.0702839024881292,89.952800674869,15.6303519455016));
#53418=CARTESIAN_POINT('Ctrl Pts',(-1.19203032177318,90.1079507396483,15.356422665022));
#53419=CARTESIAN_POINT('Ctrl Pts',(-2.14007301474896,90.266169579479,14.4410255702375));
#53420=CARTESIAN_POINT('Ctrl Pts',(-2.46919738320312,90.4275439920485,13.1380722770788));
#53421=CARTESIAN_POINT('Ctrl Pts',(-2.05448680883129,90.5921473637104,11.8318607370155));
#53422=CARTESIAN_POINT('Ctrl Pts',(-0.992366573357415,90.7600372906474,
10.9226765107351));
#53423=CARTESIAN_POINT('Ctrl Pts',(-0.0534675979651628,90.8741828745936,
10.7780340477837));
#53424=CARTESIAN_POINT('Ctrl Pts',(0.404552238010835,90.9318150127178,10.8366690372188));
#53425=CARTESIAN_POINT('Ctrl Pts',(1.09092693438828,82.3007689497503,10.6418050319898));
#53426=CARTESIAN_POINT('Ctrl Pts',(1.59144193186989,82.3689958494283,10.8615507258058));
#53427=CARTESIAN_POINT('Ctrl Pts',(2.44170527637221,82.5025601160605,11.5817113845902));
#53428=CARTESIAN_POINT('Ctrl Pts',(2.93320795887768,82.6990780757878,13.1427952373425));
#53429=CARTESIAN_POINT('Ctrl Pts',(2.53714311960989,82.8908092014927,14.6896184836951));
#53430=CARTESIAN_POINT('Ctrl Pts',(1.40246086876332,83.0795927252857,15.7779590132722));
#53431=CARTESIAN_POINT('Ctrl Pts',(-0.110779940039283,83.265371108554,16.0993529543373));
#53432=CARTESIAN_POINT('Ctrl Pts',(-1.54287138803243,83.4481022462018,15.5822415579395));
#53433=CARTESIAN_POINT('Ctrl Pts',(-2.46910424843797,83.6277575655426,14.4095457148995));
#53434=CARTESIAN_POINT('Ctrl Pts',(-2.65763851847854,83.8239427479212,12.783843019403));
#53435=CARTESIAN_POINT('Ctrl Pts',(-1.72998411638569,84.0353418599503,11.2284215222705));
#53436=CARTESIAN_POINT('Ctrl Pts',(0.120398789033176,84.2605110232883,10.6655946771609));
#53437=CARTESIAN_POINT('Ctrl Pts',(1.81973633994219,84.4803193348133,11.4831765154348));
#53438=CARTESIAN_POINT('Ctrl Pts',(2.50974551050697,84.6949030131653,13.1909391184697));
#53439=CARTESIAN_POINT('Ctrl Pts',(1.8761801922996,84.9044369388084,14.876091597299));
#53440=CARTESIAN_POINT('Ctrl Pts',(0.442943858324112,85.0920834801847,15.6062822964452));
#53441=CARTESIAN_POINT('Ctrl Pts',(-0.928757782177521,85.2593421026985,
15.3624189358734));
#53442=CARTESIAN_POINT('Ctrl Pts',(-1.9273104586054,85.4197698003848,14.4731596758825));
#53443=CARTESIAN_POINT('Ctrl Pts',(-2.18893445549896,85.5652612914026,13.2650373897583));
#53444=CARTESIAN_POINT('Ctrl Pts',(-1.79750693525794,85.708628960392,12.1575362726721));
#53445=CARTESIAN_POINT('Ctrl Pts',(-1.00407430876644,85.8384401934296,11.4230188211684));
#53446=CARTESIAN_POINT('Ctrl Pts',(-0.0530396829851482,85.9549193837048,
11.241705895162));
#53447=CARTESIAN_POINT('Ctrl Pts',(1.04269874870432,86.0934463163342,11.4887610721776));
#53448=CARTESIAN_POINT('Ctrl Pts',(1.88784008915594,86.2304017149048,12.3278656793438));
#53449=CARTESIAN_POINT('Ctrl Pts',(2.00925658113287,86.388298190667,13.6408958019134));
#53450=CARTESIAN_POINT('Ctrl Pts',(1.5141869042575,86.5225448053115,14.6412674792069));
#53451=CARTESIAN_POINT('Ctrl Pts',(0.569943927398302,86.6558988636545,15.2274692057216));
#53452=CARTESIAN_POINT('Ctrl Pts',(-0.442474907701717,86.7775073163584,
15.2276295219295));
#53453=CARTESIAN_POINT('Ctrl Pts',(-1.08059670664969,86.865674160951,14.8898130646209));
#53454=CARTESIAN_POINT('Ctrl Pts',(-1.59202319075267,86.953731069283,14.4015536673542));
#53455=CARTESIAN_POINT('Ctrl Pts',(-1.959495328548,87.0526718366557,13.6642829173165));
#53456=CARTESIAN_POINT('Ctrl Pts',(-1.85526539888215,87.184535161682,12.5716123493504));
#53457=CARTESIAN_POINT('Ctrl Pts',(-1.11790566111324,87.3312254586828,11.5971429409853));
#53458=CARTESIAN_POINT('Ctrl Pts',(0.217555757790785,87.4931099341109,11.220397012999));
#53459=CARTESIAN_POINT('Ctrl Pts',(1.58160777082197,87.6708613923171,11.9041881844393));
#53460=CARTESIAN_POINT('Ctrl Pts',(2.1295848131522,87.8502603315557,13.343619575246));
#53461=CARTESIAN_POINT('Ctrl Pts',(1.56147398870172,88.0317657967935,14.7931214983046));
#53462=CARTESIAN_POINT('Ctrl Pts',(0.140883975998077,88.2158505766912,15.488448435748));
#53463=CARTESIAN_POINT('Ctrl Pts',(-1.39976173027164,88.4029283983156,15.0386864184388));
#53464=CARTESIAN_POINT('Ctrl Pts',(-2.25057505170216,88.5934288956208,13.6408160242912));
#53465=CARTESIAN_POINT('Ctrl Pts',(-1.98209790536562,88.7553327392467,12.2797577791271));
#53466=CARTESIAN_POINT('Ctrl Pts',(-1.24650932068784,88.8869313391437,11.4969890384965));
#53467=CARTESIAN_POINT('Ctrl Pts',(-0.637504828814648,88.9700746021111,
11.2032694363274));
#53468=CARTESIAN_POINT('Ctrl Pts',(0.162096212239786,89.070681500301,11.0645677160771));
#53469=CARTESIAN_POINT('Ctrl Pts',(1.07919346721318,89.1837246869346,11.2504526561831));
#53470=CARTESIAN_POINT('Ctrl Pts',(2.26799185493347,89.3733161811301,12.2838066555285));
#53471=CARTESIAN_POINT('Ctrl Pts',(2.45699812867301,89.5541602756378,13.8931639381941));
#53472=CARTESIAN_POINT('Ctrl Pts',(1.75330953186089,89.7045894476644,14.9158667687635));
#53473=CARTESIAN_POINT('Ctrl Pts',(1.08391027807925,89.8138804379689,15.4791011190795));
#53474=CARTESIAN_POINT('Ctrl Pts',(0.110595832794049,89.938226094315,15.8379510560887));
#53475=CARTESIAN_POINT('Ctrl Pts',(-1.26592796379711,90.1070398976702,15.5550459780666));
#53476=CARTESIAN_POINT('Ctrl Pts',(-2.30627773892431,90.2789125402582,14.5718470411942));
#53477=CARTESIAN_POINT('Ctrl Pts',(-2.6777912572662,90.4538666744987,13.1631880283135));
#53478=CARTESIAN_POINT('Ctrl Pts',(-2.24365046799695,90.6319112907103,11.7459518731515));
#53479=CARTESIAN_POINT('Ctrl Pts',(-1.10765396453851,90.8130402539771,10.7538573219242));
#53480=CARTESIAN_POINT('Ctrl Pts',(-0.0992408494391709,90.9358356281587,
10.5885159276331));
#53481=CARTESIAN_POINT('Ctrl Pts',(0.393261874122084,90.9977379954965,10.6465837081081));
#53482=CARTESIAN_POINT('Ctrl Pts',(0.986873058613682,82.3675214625011,10.8009350481316));
#53483=CARTESIAN_POINT('Ctrl Pts',(1.45689562423789,82.4313593200691,11.0026038517577));
#53484=CARTESIAN_POINT('Ctrl Pts',(2.25673123253409,82.5561569686474,11.6690255071179));
#53485=CARTESIAN_POINT('Ctrl Pts',(2.72679773845037,82.7393141451417,13.120096144624));
#53486=CARTESIAN_POINT('Ctrl Pts',(2.37063631835171,82.9176103654609,14.5615285447094));
#53487=CARTESIAN_POINT('Ctrl Pts',(1.32632728944021,83.0928178719662,15.5805936382548));
#53488=CARTESIAN_POINT('Ctrl Pts',(-0.0729785831179774,83.264943761711,
15.8906782851302));
#53489=CARTESIAN_POINT('Ctrl Pts',(-1.40216672394912,83.4340104217921,15.4241999118085));
#53490=CARTESIAN_POINT('Ctrl Pts',(-2.26812952472817,83.6000539717464,14.3483257439206));
#53491=CARTESIAN_POINT('Ctrl Pts',(-2.45635762395667,83.7812452024802,12.8486647088747));
#53492=CARTESIAN_POINT('Ctrl Pts',(-1.61393392995191,83.9764097319649,11.4045751558552));
#53493=CARTESIAN_POINT('Ctrl Pts',(0.0893154914447954,84.1843381200616,
10.8677925938811));
#53494=CARTESIAN_POINT('Ctrl Pts',(1.66779470076804,84.3875213652679,11.6070641663502));
#53495=CARTESIAN_POINT('Ctrl Pts',(2.3237587860552,84.5862360464939,13.1813820565129));
#53496=CARTESIAN_POINT('Ctrl Pts',(1.75317760695792,84.780789130254,14.7524589030643));
#53497=CARTESIAN_POINT('Ctrl Pts',(0.425774539073593,84.9556334786481,15.4482546628703));
#53498=CARTESIAN_POINT('Ctrl Pts',(-0.859761342353121,85.112079573922,15.2350638900366));
#53499=CARTESIAN_POINT('Ctrl Pts',(-1.80704389725007,85.2627040232489,14.4113935326486));
#53500=CARTESIAN_POINT('Ctrl Pts',(-2.06796452997879,85.3999632596242,13.2747901350428));
#53501=CARTESIAN_POINT('Ctrl Pts',(-1.70957699426978,85.5358729370547,12.2205365704158));
#53502=CARTESIAN_POINT('Ctrl Pts',(-0.962846708349784,85.6594893712233,
11.511723739827));
#53503=CARTESIAN_POINT('Ctrl Pts',(-0.0543934820478983,85.7710311767666,
11.3266358262627));
#53504=CARTESIAN_POINT('Ctrl Pts',(1.00226930766624,85.904278295582,11.5512922917787));
#53505=CARTESIAN_POINT('Ctrl Pts',(1.83131244206865,86.0368276136668,12.3519343222649));
#53506=CARTESIAN_POINT('Ctrl Pts',(1.96678061982792,86.1909028251225,13.6315160702192));
#53507=CARTESIAN_POINT('Ctrl Pts',(1.49340043760464,86.3227939555925,14.6206323830071));
#53508=CARTESIAN_POINT('Ctrl Pts',(0.56711814332234,86.4547235642503,15.2129420815183));
#53509=CARTESIAN_POINT('Ctrl Pts',(-0.441469516314034,86.5758858947906,
15.2265836229135));
#53510=CARTESIAN_POINT('Ctrl Pts',(-1.08555937987099,86.6642766407459,14.896213152512));
#53511=CARTESIAN_POINT('Ctrl Pts',(-1.60615174531136,86.7528703385578,14.4114524803976));
#53512=CARTESIAN_POINT('Ctrl Pts',(-1.98739058305599,86.8528545644265,13.6714976615677));
#53513=CARTESIAN_POINT('Ctrl Pts',(-1.8961591396499,86.9870405853029,12.5582868212341));
#53514=CARTESIAN_POINT('Ctrl Pts',(-1.15410442205856,87.1373343043804,11.5499952608252));
#53515=CARTESIAN_POINT('Ctrl Pts',(0.219127915251716,87.3044730381322,11.1420043238971));
#53516=CARTESIAN_POINT('Ctrl Pts',(1.64867702502392,87.4895184799861,11.8343222618939));
#53517=CARTESIAN_POINT('Ctrl Pts',(2.24375798031837,87.6777099280584,13.3365002905118));
#53518=CARTESIAN_POINT('Ctrl Pts',(1.66376241926902,87.869435427527,14.8752907360187));
#53519=CARTESIAN_POINT('Ctrl Pts',(0.16352346202287,88.0650781847536,15.63353305405));
#53520=CARTESIAN_POINT('Ctrl Pts',(-1.48842305261904,88.2649594439756,15.1734228142003));
#53521=CARTESIAN_POINT('Ctrl Pts',(-2.41945910530045,88.4693960245382,13.684316081751));
#53522=CARTESIAN_POINT('Ctrl Pts',(-2.14733195222152,88.6437638502332,12.2151816733544));
#53523=CARTESIAN_POINT('Ctrl Pts',(-1.36281186129439,88.7857780281219,11.3617747378727));
#53524=CARTESIAN_POINT('Ctrl Pts',(-0.708363110808276,88.875603696437,11.0373579101007));
#53525=CARTESIAN_POINT('Ctrl Pts',(0.154442061731767,88.9843715742907,10.8781781251525));
#53526=CARTESIAN_POINT('Ctrl Pts',(1.14878610904288,89.1066838810156,11.0687174671823));
#53527=CARTESIAN_POINT('Ctrl Pts',(2.44768052466662,89.3119705930039,12.1741273499311));
#53528=CARTESIAN_POINT('Ctrl Pts',(2.6701128707135,89.5078881935536,13.9154669359159));
#53529=CARTESIAN_POINT('Ctrl Pts',(1.91898192293812,89.6707854617373,15.0303878015014));
#53530=CARTESIAN_POINT('Ctrl Pts',(1.20035754076689,89.7890999582511,15.6471784629207));
#53531=CARTESIAN_POINT('Ctrl Pts',(0.150907763099969,89.9236515137611,16.0455501666756));
#53532=CARTESIAN_POINT('Ctrl Pts',(-1.33982560582105,90.1061290556921,15.7536692911111));
#53533=CARTESIAN_POINT('Ctrl Pts',(-2.47248246309965,90.2916555010373,14.7026685121508));
#53534=CARTESIAN_POINT('Ctrl Pts',(-2.88638513132925,90.4801893569489,13.188303779548));
#53535=CARTESIAN_POINT('Ctrl Pts',(-2.43281412716261,90.6716752177104,11.6600430092875));
#53536=CARTESIAN_POINT('Ctrl Pts',(-1.22294135571961,90.8660432173068,10.5850381331131));
#53537=CARTESIAN_POINT('Ctrl Pts',(-0.145014100913177,90.9974883817239,
10.3989978074825));
#53538=CARTESIAN_POINT('Ctrl Pts',(0.381971510233331,91.0636609782751,10.4564983789973));
#53539=CARTESIAN_POINT('Ctrl Pts',(0.882819182839093,82.434273975252,10.9600650642734));
#53540=CARTESIAN_POINT('Ctrl Pts',(1.32234931660589,82.49372279071,11.1436569777094));
#53541=CARTESIAN_POINT('Ctrl Pts',(2.07175718869597,82.6097538212342,11.7563396296457));
#53542=CARTESIAN_POINT('Ctrl Pts',(2.52038751802309,82.7795502144957,13.0973970519055));
#53543=CARTESIAN_POINT('Ctrl Pts',(2.20412951709352,82.9444115294294,14.4334386057238));
#53544=CARTESIAN_POINT('Ctrl Pts',(1.2501937101171,83.1060430186465,15.3832282632374));
#53545=CARTESIAN_POINT('Ctrl Pts',(-0.0351772261966642,83.2645164148681,
15.6820036159229));
#53546=CARTESIAN_POINT('Ctrl Pts',(-1.26146205986579,83.4199185973822,15.2661582656774));
#53547=CARTESIAN_POINT('Ctrl Pts',(-2.06715480101835,83.5723503779501,14.2871057729414));
#53548=CARTESIAN_POINT('Ctrl Pts',(-2.2550767294348,83.7385476570392,12.9134863983464));
#53549=CARTESIAN_POINT('Ctrl Pts',(-1.49788374351813,83.9174776039795,11.5807287894401));
#53550=CARTESIAN_POINT('Ctrl Pts',(0.0582321938564075,84.1081652168351,
11.0699905106014));
#53551=CARTESIAN_POINT('Ctrl Pts',(1.51585306159387,84.2947233957224,11.7309518172656));
#53552=CARTESIAN_POINT('Ctrl Pts',(2.13777206160342,84.4775690798224,13.1718249945562));
#53553=CARTESIAN_POINT('Ctrl Pts',(1.63017502161623,84.6571413216995,14.6288262088296));
#53554=CARTESIAN_POINT('Ctrl Pts',(0.408605219823062,84.8191834771113,15.2902270292953));
#53555=CARTESIAN_POINT('Ctrl Pts',(-0.790764902528728,84.9648170451454,
15.1077088441999));
#53556=CARTESIAN_POINT('Ctrl Pts',(-1.68677733589476,85.105638246113,14.3496273894146));
#53557=CARTESIAN_POINT('Ctrl Pts',(-1.94699460445861,85.2346652278456,13.2845428803274));
#53558=CARTESIAN_POINT('Ctrl Pts',(-1.6216470532816,85.3631169137173,12.2835368681594));
#53559=CARTESIAN_POINT('Ctrl Pts',(-0.92161910793314,85.4805385490169,11.6004286584856));
#53560=CARTESIAN_POINT('Ctrl Pts',(-0.0557472811106569,85.5871429698282,
11.4115657573635));
#53561=CARTESIAN_POINT('Ctrl Pts',(0.961839866628155,85.7151102748299,11.6138235113798));
#53562=CARTESIAN_POINT('Ctrl Pts',(1.77478479498137,85.8432535124287,12.3760029651859));
#53563=CARTESIAN_POINT('Ctrl Pts',(1.92430465852295,85.993507459578,13.622136338525));
#53564=CARTESIAN_POINT('Ctrl Pts',(1.47261397095176,86.1230431058733,14.5999972868073));
#53565=CARTESIAN_POINT('Ctrl Pts',(0.564292359246367,86.2535482648462,15.1984149573149));
#53566=CARTESIAN_POINT('Ctrl Pts',(-0.440464124926358,86.3742644732228,
15.2255377238975));
#53567=CARTESIAN_POINT('Ctrl Pts',(-1.0905220530923,86.4628791205409,14.9026132404033));
#53568=CARTESIAN_POINT('Ctrl Pts',(-1.62028029987006,86.5520096078327,14.4213512934408));
#53569=CARTESIAN_POINT('Ctrl Pts',(-2.01528583756397,86.6530372921974,13.678712405819));
#53570=CARTESIAN_POINT('Ctrl Pts',(-1.93705288041765,86.7895460089237,12.5449612931179));
#53571=CARTESIAN_POINT('Ctrl Pts',(-1.19030318300388,86.943443150078,11.502847580665));
#53572=CARTESIAN_POINT('Ctrl Pts',(0.220700072712643,87.1158361421535,11.0636116347951));
#53573=CARTESIAN_POINT('Ctrl Pts',(1.71574627922587,87.3081755676547,11.7644563393486));
#53574=CARTESIAN_POINT('Ctrl Pts',(2.35793114748454,87.5051595245611,13.3293810057776));
#53575=CARTESIAN_POINT('Ctrl Pts',(1.76605084983632,87.7071050582604,14.9574599737328));
#53576=CARTESIAN_POINT('Ctrl Pts',(0.186162948047658,87.9143057928158,15.778617672352));
#53577=CARTESIAN_POINT('Ctrl Pts',(-1.57708437496644,88.1269904896355,15.3081592099618));
#53578=CARTESIAN_POINT('Ctrl Pts',(-2.58834315889874,88.3453631534556,13.7278161392108));
#53579=CARTESIAN_POINT('Ctrl Pts',(-2.31256599907742,88.5321949612197,12.1506055675816));
#53580=CARTESIAN_POINT('Ctrl Pts',(-1.47911440190093,88.6846247171001,11.226560437249));
#53581=CARTESIAN_POINT('Ctrl Pts',(-0.779221392801904,88.7811327907629,
10.871446383874));
#53582=CARTESIAN_POINT('Ctrl Pts',(0.146787911223744,88.8980616482805,10.691788534228));
#53583=CARTESIAN_POINT('Ctrl Pts',(1.21837875087259,89.0296430750967,10.8869822781816));
#53584=CARTESIAN_POINT('Ctrl Pts',(2.62736919439976,89.2506250048775,12.0644480443334));
#53585=CARTESIAN_POINT('Ctrl Pts',(2.88322761275398,89.4616161114694,13.9377699336378));
#53586=CARTESIAN_POINT('Ctrl Pts',(2.08465431401534,89.63698147581,15.1449088342394));
#53587=CARTESIAN_POINT('Ctrl Pts',(1.31680480345452,89.7643194785334,15.8152558067619));
#53588=CARTESIAN_POINT('Ctrl Pts',(0.191219693405885,89.9090769332071,16.2531492772627));
#53589=CARTESIAN_POINT('Ctrl Pts',(-1.41372324784499,90.1052182137141,15.9522926041556));
#53590=CARTESIAN_POINT('Ctrl Pts',(-2.638687187275,90.3043984618164,14.8334899831074));
#53591=CARTESIAN_POINT('Ctrl Pts',(-3.09497900539232,90.5065120393991,13.2134195307825));
#53592=CARTESIAN_POINT('Ctrl Pts',(-2.62197778632827,90.7114391447102,11.5741341454235));
#53593=CARTESIAN_POINT('Ctrl Pts',(-1.33822874690071,90.9190461806365,10.416218944302));
#53594=CARTESIAN_POINT('Ctrl Pts',(-0.190787352387184,91.0591411352891,
10.2094796873319));
#53595=CARTESIAN_POINT('Ctrl Pts',(0.37068114634458,91.1295839610538,10.2664130498865));
#53596=CARTESIAN_POINT('Ctrl Pts',(0.920533865651003,82.4393565600724,10.9761000835092));
#53597=CARTESIAN_POINT('Ctrl Pts',(0.930994513306672,82.4407797944805,10.9806730010019));
#53598=CARTESIAN_POINT('Ctrl Pts',(0.941423665733055,82.4422018898699,10.9853165122668));
#53599=CARTESIAN_POINT('Ctrl Pts',(0.951820353857793,82.4436229114634,10.9900301168068));
#53600=CARTESIAN_POINT('Ctrl Pts',(1.02615204531446,82.453782583214,11.0237302907574));
#53601=CARTESIAN_POINT('Ctrl Pts',(1.09881834405504,82.4638831712601,11.0610046463177));
#53602=CARTESIAN_POINT('Ctrl Pts',(1.1694201192702,82.4739548102459,11.1016609610774));
#53603=CARTESIAN_POINT('Ctrl Pts',(1.23335157916184,82.4830749008089,11.1384761480679));
#53604=CARTESIAN_POINT('Ctrl Pts',(1.29558946004411,82.4921711969464,11.178064012004));
#53605=CARTESIAN_POINT('Ctrl Pts',(1.35582412660719,82.5012626039083,11.2202475575312));
#53606=CARTESIAN_POINT('Ctrl Pts',(1.42322871684646,82.5114361899167,11.2674523444644));
#53607=CARTESIAN_POINT('Ctrl Pts',(1.48812697663125,82.5216063052533,11.3179140070938));
#53608=CARTESIAN_POINT('Ctrl Pts',(1.55011210052986,82.5318142072745,11.3714148650172));
#53609=CARTESIAN_POINT('Ctrl Pts',(1.57821000765237,82.5364414575704,11.3956668474664));
#53610=CARTESIAN_POINT('Ctrl Pts',(1.60570885058393,82.5410763797476,11.4205428057615));
#53611=CARTESIAN_POINT('Ctrl Pts',(1.63256866727547,82.5457223547656,11.4460196295166));
#53612=CARTESIAN_POINT('Ctrl Pts',(1.68097537945571,82.5540953223878,11.4919339143734));
#53613=CARTESIAN_POINT('Ctrl Pts',(1.72731518937305,82.5625081638741,11.5398143925773));
#53614=CARTESIAN_POINT('Ctrl Pts',(1.7715643694936,82.5709132106333,11.5894150810159));
#53615=CARTESIAN_POINT('Ctrl Pts',(1.81569939097242,82.5792965731778,11.6388878044345));
#53616=CARTESIAN_POINT('Ctrl Pts',(1.85775518464244,82.5876721800752,11.6900715580635));
#53617=CARTESIAN_POINT('Ctrl Pts',(1.89773094642547,82.5959989594274,11.7427682864444));
#53618=CARTESIAN_POINT('Ctrl Pts',(1.91033667158171,82.5986246777945,11.7593853675198));
#53619=CARTESIAN_POINT('Ctrl Pts',(1.92273569868281,82.6012455876238,11.7761532549623));
#53620=CARTESIAN_POINT('Ctrl Pts',(1.93492831235468,82.6038605304053,11.7930667633059));
#53621=CARTESIAN_POINT('Ctrl Pts',(1.94582122437246,82.606196726927,11.8081773346121));
#53622=CARTESIAN_POINT('Ctrl Pts',(1.95656549789998,82.6085228755565,11.8233952376663));
#53623=CARTESIAN_POINT('Ctrl Pts',(1.96712724119019,82.610848366971,11.8387322038599));
#53624=CARTESIAN_POINT('Ctrl Pts',(1.96715436113799,82.6108543382585,11.8387715854005));
#53625=CARTESIAN_POINT('Ctrl Pts',(1.96718147988153,82.6108603095415,11.8388109677247));
#53626=CARTESIAN_POINT('Ctrl Pts',(1.96720859742029,82.61086628082,11.8388503508325));
#53627=CARTESIAN_POINT('Ctrl Pts',(2.04383660407255,82.6277397581419,11.9501380705541));
#53628=CARTESIAN_POINT('Ctrl Pts',(2.11078017326571,82.6445646537931,12.0675952760296));
#53629=CARTESIAN_POINT('Ctrl Pts',(2.16755235526014,82.661334864107,12.1893717483931));
#53630=CARTESIAN_POINT('Ctrl Pts',(2.22793839858296,82.6791725904542,12.3188999623443));
#53631=CARTESIAN_POINT('Ctrl Pts',(2.27681893361483,82.6969483090552,12.4533119179796));
#53632=CARTESIAN_POINT('Ctrl Pts',(2.31365407565392,82.7146619567084,12.5904314693233));
#53633=CARTESIAN_POINT('Ctrl Pts',(2.34880641410517,82.7315663611178,12.7212867507283));
#53634=CARTESIAN_POINT('Ctrl Pts',(2.37299160473249,82.7484143374262,12.8546084560198));
#53635=CARTESIAN_POINT('Ctrl Pts',(2.38574068823176,82.7652115237532,12.9885594457077));
#53636=CARTESIAN_POINT('Ctrl Pts',(2.38923264560951,82.7698122512269,13.0252484474484));
#53637=CARTESIAN_POINT('Ctrl Pts',(2.39186681884341,82.7744087884096,13.0619816538601));
#53638=CARTESIAN_POINT('Ctrl Pts',(2.39385078342915,82.7789577812924,13.0987563954806));
#53639=CARTESIAN_POINT('Ctrl Pts',(2.39385087309786,82.7789579868921,13.0987580575786));
#53640=CARTESIAN_POINT('Ctrl Pts',(2.39385096276524,82.7789581924915,13.0987597196767));
#53641=CARTESIAN_POINT('Ctrl Pts',(2.3938510524313,82.7789583980909,13.098761381775));
#53642=CARTESIAN_POINT('Ctrl Pts',(2.39752709562371,82.7873873662675,13.166902497685));
#53643=CARTESIAN_POINT('Ctrl Pts',(2.39828854108446,82.7957891942172,13.2350848776881));
#53644=CARTESIAN_POINT('Ctrl Pts',(2.39605616560726,82.8041987158248,13.3030783290674));
#53645=CARTESIAN_POINT('Ctrl Pts',(2.39521945688256,82.8073506587535,13.3285627131114));
#53646=CARTESIAN_POINT('Ctrl Pts',(2.39396213470044,82.8105036170795,13.3540200372025));
#53647=CARTESIAN_POINT('Ctrl Pts',(2.39228000488214,82.8136591892446,13.3794363069799));
#53648=CARTESIAN_POINT('Ctrl Pts',(2.38582315035503,82.8257718515364,13.4769966467281));
#53649=CARTESIAN_POINT('Ctrl Pts',(2.37310613543231,82.8379259190769,13.5739780393391));
#53650=CARTESIAN_POINT('Ctrl Pts',(2.35445818219782,82.8500908714037,13.6696283756344));
#53651=CARTESIAN_POINT('Ctrl Pts',(2.33923615030137,82.8600209312879,13.7477062457193));
#53652=CARTESIAN_POINT('Ctrl Pts',(2.32006269363205,82.8699583679949,13.8248982501427));
#53653=CARTESIAN_POINT('Ctrl Pts',(2.29711475887482,82.8798899526932,13.9008207825145));
#53654=CARTESIAN_POINT('Ctrl Pts',(2.26972748757379,82.8917428277976,13.9914307225341));
#53655=CARTESIAN_POINT('Ctrl Pts',(2.23696730721706,82.9035860950502,14.0802302740837));
#53656=CARTESIAN_POINT('Ctrl Pts',(2.19914064222399,82.9153963320166,14.1665197842907));
#53657=CARTESIAN_POINT('Ctrl Pts',(2.16873815448171,82.924888593221,14.2358733944184));
#53658=CARTESIAN_POINT('Ctrl Pts',(2.13506345482034,82.9343596099332,14.3036063662027));
#53659=CARTESIAN_POINT('Ctrl Pts',(2.09828154655871,82.9437995142575,14.3693790747516));
#53660=CARTESIAN_POINT('Ctrl Pts',(2.09827926593422,82.9438000995691,14.369383152921));
#53661=CARTESIAN_POINT('Ctrl Pts',(2.09827698529767,82.9438006848806,14.3693872310829));
#53662=CARTESIAN_POINT('Ctrl Pts',(2.09827470464909,82.943801270192,14.3693913092375));
#53663=CARTESIAN_POINT('Ctrl Pts',(2.09693217075603,82.9441458214716,14.3717919687587));
#53664=CARTESIAN_POINT('Ctrl Pts',(2.09558546479307,82.9444903396463,14.374190068563));
#53665=CARTESIAN_POINT('Ctrl Pts',(2.09423459446982,82.9448348255343,14.3765855912899));
#53666=CARTESIAN_POINT('Ctrl Pts',(2.04022528568224,82.9586077572339,14.4723612734103));
#53667=CARTESIAN_POINT('Ctrl Pts',(1.97962952520666,82.9723175346397,14.5640780526061));
#53668=CARTESIAN_POINT('Ctrl Pts',(1.91316752949104,82.9859834432265,14.6510156889316));
#53669=CARTESIAN_POINT('Ctrl Pts',(1.87270278139702,82.9943038004846,14.7039468342565));
#53670=CARTESIAN_POINT('Ctrl Pts',(1.83006374203318,83.0026077717938,14.7551053957788));
#53671=CARTESIAN_POINT('Ctrl Pts',(1.78541721884374,83.0108985437968,14.8043204535108));
#53672=CARTESIAN_POINT('Ctrl Pts',(1.65763162308314,83.0346280789104,14.9451819366323));
#53673=CARTESIAN_POINT('Ctrl Pts',(1.51336634790013,83.0582549027632,15.0700837180756));
#53674=CARTESIAN_POINT('Ctrl Pts',(1.35699330054957,83.0817754177794,15.1752608586358));
#53675=CARTESIAN_POINT('Ctrl Pts',(1.30429717907158,83.0897015913593,15.2107044818789));
#53676=CARTESIAN_POINT('Ctrl Pts',(1.25028177908284,83.0976059460742,15.2440258520453));
#53677=CARTESIAN_POINT('Ctrl Pts',(1.19506856748379,83.1054958017013,15.2750223457027));
#53678=CARTESIAN_POINT('Ctrl Pts',(1.19506406440212,83.1054964451826,15.2750248737162));
#53679=CARTESIAN_POINT('Ctrl Pts',(1.19505956131248,83.1054970886637,15.2750274017142));
#53680=CARTESIAN_POINT('Ctrl Pts',(1.1950550582149,83.1054977321447,15.2750299296967));
#53681=CARTESIAN_POINT('Ctrl Pts',(1.1347180566568,83.1141197338409,15.3089023658992));
#53682=CARTESIAN_POINT('Ctrl Pts',(1.07295896734627,83.1227234186035,15.3399797628626));
#53683=CARTESIAN_POINT('Ctrl Pts',(1.00999286229148,83.1313199199441,15.3680862300822));
#53684=CARTESIAN_POINT('Ctrl Pts',(0.995778869549489,83.1332604974588,15.3744309947888));
#53685=CARTESIAN_POINT('Ctrl Pts',(0.981503556850033,83.1352006824813,15.3806242744179));
#53686=CARTESIAN_POINT('Ctrl Pts',(0.967169734092123,83.1371405568294,15.3866639028358));
#53687=CARTESIAN_POINT('Ctrl Pts',(0.883478264771382,83.1484669794617,15.4219277249845));
#53688=CARTESIAN_POINT('Ctrl Pts',(0.797774212518988,83.1597853120529,15.4519580355328));
#53689=CARTESIAN_POINT('Ctrl Pts',(0.710743099405598,83.171086254001,15.4767512079966));
#53690=CARTESIAN_POINT('Ctrl Pts',(0.652124685216517,83.1786978226935,15.4934502527469));
#53691=CARTESIAN_POINT('Ctrl Pts',(0.59290321784703,83.1863016382014,15.5077739015619));
#53692=CARTESIAN_POINT('Ctrl Pts',(0.533275044503793,83.1938965479578,15.51972279897));
#53693=CARTESIAN_POINT('Ctrl Pts',(0.436752412107777,83.2061907478537,15.5390649818242));
#53694=CARTESIAN_POINT('Ctrl Pts',(0.33917125756754,83.2184569160692,15.5523664089726));
#53695=CARTESIAN_POINT('Ctrl Pts',(0.241390583592281,83.2306917323916,15.559404755261));
#53696=CARTESIAN_POINT('Ctrl Pts',(0.195580195304286,83.2364237616728,15.5627022307566));
#53697=CARTESIAN_POINT('Ctrl Pts',(0.149726630899953,83.2421488480259,15.5646254222749));
#53698=CARTESIAN_POINT('Ctrl Pts',(0.103921117916872,83.247866324241,15.5651541213653));
#53699=CARTESIAN_POINT('Ctrl Pts',(0.0607635922639142,83.2532532768228,
15.5656522567002));
#53700=CARTESIAN_POINT('Ctrl Pts',(0.0176523014704029,83.2586332082964,
15.5649035786488));
#53701=CARTESIAN_POINT('Ctrl Pts',(-0.0253295424226451,83.2640045459169,
15.5629001654344));
#53702=CARTESIAN_POINT('Ctrl Pts',(-0.0253674153657417,83.2640092788074,
15.5628984001505));
#53703=CARTESIAN_POINT('Ctrl Pts',(-0.0254052882083584,83.2640140116914,
15.5628966338927));
#53704=CARTESIAN_POINT('Ctrl Pts',(-0.025443160950471,83.2640187445686,
15.5628948666609));
#53705=CARTESIAN_POINT('Ctrl Pts',(-0.102628557979231,83.273664441926,15.5592932133354));
#53706=CARTESIAN_POINT('Ctrl Pts',(-0.17953270492342,83.2832960245341,15.5518071478355));
#53707=CARTESIAN_POINT('Ctrl Pts',(-0.255746825396155,83.292912320685,15.5404684889302));
#53708=CARTESIAN_POINT('Ctrl Pts',(-0.294626486742618,83.2978179514977,
15.5346842167294));
#53709=CARTESIAN_POINT('Ctrl Pts',(-0.333325787768408,83.3027195064199,
15.5278976329917));
#53710=CARTESIAN_POINT('Ctrl Pts',(-0.371785817460665,83.3076162188687,
15.5201152844023));
#53711=CARTESIAN_POINT('Ctrl Pts',(-0.417916676564152,83.313489577622,15.5107807511441));
#53712=CARTESIAN_POINT('Ctrl Pts',(-0.463697662900614,83.3193558862578,
15.499983461912));
#53713=CARTESIAN_POINT('Ctrl Pts',(-0.509026553977117,83.325213952138,15.4877233112308));
#53714=CARTESIAN_POINT('Ctrl Pts',(-0.580017665418723,83.3343884675045,
15.4685222740415));
#53715=CARTESIAN_POINT('Ctrl Pts',(-0.649902559680175,83.3435431400438,
15.4457301312203));
#53716=CARTESIAN_POINT('Ctrl Pts',(-0.718388236301924,83.3526802822629,
15.4196147550527));
#53717=CARTESIAN_POINT('Ctrl Pts',(-0.757687564455145,83.3579234742436,
15.4046288954032));
#53718=CARTESIAN_POINT('Ctrl Pts',(-0.796527047443576,83.3631610125617,
15.3885483859335));
#53719=CARTESIAN_POINT('Ctrl Pts',(-0.834857972488083,83.3683942942767,
15.3714199738278));
#53720=CARTESIAN_POINT('Ctrl Pts',(-0.900204612771983,83.3773160037669,
15.3422194214485));
#53721=CARTESIAN_POINT('Ctrl Pts',(-0.964154981785965,83.386233016291,15.3101017265351));
#53722=CARTESIAN_POINT('Ctrl Pts',(-1.02631379660646,83.3951374072177,15.2750876881961));
#53723=CARTESIAN_POINT('Ctrl Pts',(-1.04641301710453,83.398016666051,15.2637658044193));
#53724=CARTESIAN_POINT('Ctrl Pts',(-1.06632462917669,83.4008945582043,15.2521413717555));
#53725=CARTESIAN_POINT('Ctrl Pts',(-1.08603449675238,83.403770680953,15.2402159565468));
#53726=CARTESIAN_POINT('Ctrl Pts',(-1.1165315839713,83.4082209070127,15.221763756077));
#53727=CARTESIAN_POINT('Ctrl Pts',(-1.14654451282116,83.4126667380911,15.2025915369825));
#53728=CARTESIAN_POINT('Ctrl Pts',(-1.17602742366442,83.4171070602856,15.1827217267305));
#53729=CARTESIAN_POINT('Ctrl Pts',(-1.18115537816718,83.4178793642929,15.1792657761464));
#53730=CARTESIAN_POINT('Ctrl Pts',(-1.18626732394777,83.4186515049187,15.1757887122118));
#53731=CARTESIAN_POINT('Ctrl Pts',(-1.19136337777988,83.4194235303912,15.1722904085955));
#53732=CARTESIAN_POINT('Ctrl Pts',(-1.20370360741183,83.4212930105666,15.1638191735244));
#53733=CARTESIAN_POINT('Ctrl Pts',(-1.21595052391483,83.4231617944611,15.1552235063429));
#53734=CARTESIAN_POINT('Ctrl Pts',(-1.22810567416795,83.4250303944022,15.1465034350886));
#53735=CARTESIAN_POINT('Ctrl Pts',(-1.3048196415846,83.4368235612503,15.0914690465254));
#53736=CARTESIAN_POINT('Ctrl Pts',(-1.3778034004921,83.4485983575214,15.0315266355163));
#53737=CARTESIAN_POINT('Ctrl Pts',(-1.44655635735356,83.4603445874994,14.9673737889971));
#53738=CARTESIAN_POINT('Ctrl Pts',(-1.46682813418681,83.4638079578563,14.948458352524));
#53739=CARTESIAN_POINT('Ctrl Pts',(-1.48673238395627,83.4672688566375,14.9291770775887));
#53740=CARTESIAN_POINT('Ctrl Pts',(-1.50625700994449,83.4707270522028,14.9095482865858));
#53741=CARTESIAN_POINT('Ctrl Pts',(-1.55111765444156,83.4786727553343,14.8644483079424));
#53742=CARTESIAN_POINT('Ctrl Pts',(-1.59404661937215,83.4866129941764,14.8175620406124));
#53743=CARTESIAN_POINT('Ctrl Pts',(-1.63479702237727,83.4945348551692,14.768981806382));
#53744=CARTESIAN_POINT('Ctrl Pts',(-1.65962609684212,83.499361616673,14.7393820438207));
#53745=CARTESIAN_POINT('Ctrl Pts',(-1.68364569267376,83.5041814271582,14.7091541429046));
#53746=CARTESIAN_POINT('Ctrl Pts',(-1.70679447914964,83.5089901673716,14.678326641304));
#53747=CARTESIAN_POINT('Ctrl Pts',(-1.75589190588166,83.5191892666008,14.612943041056));
#53748=CARTESIAN_POINT('Ctrl Pts',(-1.80124541987183,83.5293612597565,14.5449417134995));
#53749=CARTESIAN_POINT('Ctrl Pts',(-1.8426741934976,83.5395229198191,14.4747652361496));
#53750=CARTESIAN_POINT('Ctrl Pts',(-1.86260765044563,83.5444122031759,14.4409998198075));
#53751=CARTESIAN_POINT('Ctrl Pts',(-1.88163269427647,83.5492991862322,14.4067300963384));
#53752=CARTESIAN_POINT('Ctrl Pts',(-1.8997296875192,83.5541862481475,14.3720011160247));
#53753=CARTESIAN_POINT('Ctrl Pts',(-1.92158429925602,83.5600880484774,14.3300610892704));
#53754=CARTESIAN_POINT('Ctrl Pts',(-1.94204849094845,83.5659844261093,14.287444637675));
#53755=CARTESIAN_POINT('Ctrl Pts',(-1.96106096675531,83.5718746730521,14.2442382822083));
#53756=CARTESIAN_POINT('Ctrl Pts',(-1.99815646377279,83.5833672130095,14.1599377814934));
#53757=CARTESIAN_POINT('Ctrl Pts',(-2.02972387459205,83.5948362906809,14.073392176862));
#53758=CARTESIAN_POINT('Ctrl Pts',(-2.05567441802314,83.6062770112547,13.9853995832281));
#53759=CARTESIAN_POINT('Ctrl Pts',(-2.082910325879,83.6182844057117,13.8930486011156));
#53760=CARTESIAN_POINT('Ctrl Pts',(-2.10396279000991,83.6302614193266,13.7990979105521));
#53761=CARTESIAN_POINT('Ctrl Pts',(-2.11875188980933,83.6422080216074,13.7044276981067));
#53762=CARTESIAN_POINT('Ctrl Pts',(-2.13568049761226,83.6558829137463,13.5960617448815));
#53763=CARTESIAN_POINT('Ctrl Pts',(-2.14440607927575,83.6695174237031,13.4867574548221));
#53764=CARTESIAN_POINT('Ctrl Pts',(-2.14480094308811,83.6831222411339,13.3777440851263));
#53765=CARTESIAN_POINT('Ctrl Pts',(-2.1449848087353,83.68945723179,13.3269827513613));
#53766=CARTESIAN_POINT('Ctrl Pts',(-2.14336126039987,83.6957863688328,13.2762797618052));
#53767=CARTESIAN_POINT('Ctrl Pts',(-2.13991520788354,83.7021084497047,13.2257776338899));
#53768=CARTESIAN_POINT('Ctrl Pts',(-2.13735460109351,83.7068061039427,13.1882517717509));
#53769=CARTESIAN_POINT('Ctrl Pts',(-2.13378782571262,83.711499651679,13.1508385175056));
#53770=CARTESIAN_POINT('Ctrl Pts',(-2.12921075693525,83.7161880527221,13.1136005849409));
#53771=CARTESIAN_POINT('Ctrl Pts',(-2.12749003241444,83.7179506320126,13.0996011834057));
#53772=CARTESIAN_POINT('Ctrl Pts',(-2.12562663483203,83.7197124004024,13.0856272189981));
#53773=CARTESIAN_POINT('Ctrl Pts',(-2.12362006952077,83.7214735974353,13.0716796777322));
#53774=CARTESIAN_POINT('Ctrl Pts',(-2.12170821201978,83.7231516677871,13.0583904460088));
#53775=CARTESIAN_POINT('Ctrl Pts',(-2.11966627769195,83.7248293207514,13.0451243973671));
#53776=CARTESIAN_POINT('Ctrl Pts',(-2.11749488714512,83.7265069918328,13.0318801072292));
#53777=CARTESIAN_POINT('Ctrl Pts',(-2.10743796819187,83.7342772209703,12.9705384233463));
#53778=CARTESIAN_POINT('Ctrl Pts',(-2.09483566207979,83.7420931254287,12.9096366888758));
#53779=CARTESIAN_POINT('Ctrl Pts',(-2.07967270917475,83.7499239804326,12.8494260098162));
#53780=CARTESIAN_POINT('Ctrl Pts',(-2.06847733416977,83.7557057934427,12.8049702144578));
#53781=CARTESIAN_POINT('Ctrl Pts',(-2.05588647717042,83.7614956354928,12.7608921651894));
#53782=CARTESIAN_POINT('Ctrl Pts',(-2.04190468002499,83.7672790925443,12.7173075817562));
#53783=CARTESIAN_POINT('Ctrl Pts',(-2.02043797771301,83.7761586199448,12.6503907706897));
#53784=CARTESIAN_POINT('Ctrl Pts',(-1.99565768808357,83.7850145658778,12.5846513691579));
#53785=CARTESIAN_POINT('Ctrl Pts',(-1.9676515739853,83.7938109299173,12.5204627342433));
#53786=CARTESIAN_POINT('Ctrl Pts',(-1.9538485678395,83.7981462784942,12.4888269236089));
#53787=CARTESIAN_POINT('Ctrl Pts',(-1.93926241902684,83.8024670525039,12.4575684725663));
#53788=CARTESIAN_POINT('Ctrl Pts',(-1.92390657318214,83.8067683519166,12.4267356533827));
#53789=CARTESIAN_POINT('Ctrl Pts',(-1.89166098374728,83.8158006081858,12.3619901200809));
#53790=CARTESIAN_POINT('Ctrl Pts',(-1.85601110579874,83.8247473695038,12.2991102096693));
#53791=CARTESIAN_POINT('Ctrl Pts',(-1.81727422075553,83.8336388418575,12.238344897837));
#53792=CARTESIAN_POINT('Ctrl Pts',(-1.79796068687771,83.8380719745767,12.2080483753531));
#53793=CARTESIAN_POINT('Ctrl Pts',(-1.77787917342235,83.8424914562996,12.1782769483276));
#53794=CARTESIAN_POINT('Ctrl Pts',(-1.75706515116445,83.8469015828313,12.1490586139349));
#53795=CARTESIAN_POINT('Ctrl Pts',(-1.71277251746687,83.856286415643,12.08688144479));
#53796=CARTESIAN_POINT('Ctrl Pts',(-1.66531380074296,83.8656823428975,12.0270797276552));
#53797=CARTESIAN_POINT('Ctrl Pts',(-1.61500751869232,83.8751276643025,11.969942402271));
#53798=CARTESIAN_POINT('Ctrl Pts',(-1.59336574893447,83.8791910429265,11.9453619166908));
#53799=CARTESIAN_POINT('Ctrl Pts',(-1.57119653894742,83.8832636510564,11.9212740518963));
#53800=CARTESIAN_POINT('Ctrl Pts',(-1.54852306630582,83.8873489352535,11.8976998295399));
#53801=CARTESIAN_POINT('Ctrl Pts',(-1.49732767543146,83.8965732708729,11.8444705978659));
#53802=CARTESIAN_POINT('Ctrl Pts',(-1.44338996086774,83.9057839105178,11.7940717731439));
#53803=CARTESIAN_POINT('Ctrl Pts',(-1.38703478780361,83.914966322146,11.7469233471102));
#53804=CARTESIAN_POINT('Ctrl Pts',(-1.38343386813591,83.9155530495897,11.7439107098424));
#53805=CARTESIAN_POINT('Ctrl Pts',(-1.37982308897923,83.9161396618501,11.7409113290383));
#53806=CARTESIAN_POINT('Ctrl Pts',(-1.37620253927408,83.9167261551632,11.7379253082228));
#53807=CARTESIAN_POINT('Ctrl Pts',(-1.37612089191015,83.9167393812302,11.7378579701808));
#53808=CARTESIAN_POINT('Ctrl Pts',(-1.37603923957738,83.9167526072368,11.737790638933));
#53809=CARTESIAN_POINT('Ctrl Pts',(-1.37595758227736,83.9167658331827,11.7377233144798));
#53810=CARTESIAN_POINT('Ctrl Pts',(-1.31802902337669,83.9261484602153,11.6899626299106));
#53811=CARTESIAN_POINT('Ctrl Pts',(-1.25743212616101,83.9355275036484,11.6454873917573));
#53812=CARTESIAN_POINT('Ctrl Pts',(-1.19470546146937,83.9449119543165,11.604431264857));
#53813=CARTESIAN_POINT('Ctrl Pts',(-1.17671609789645,83.947603318441,11.5926567890844));
#53814=CARTESIAN_POINT('Ctrl Pts',(-1.15855158918339,83.9502951516034,11.5811632006949));
#53815=CARTESIAN_POINT('Ctrl Pts',(-1.14022464344702,83.9529877242921,11.5699528728668));
#53816=CARTESIAN_POINT('Ctrl Pts',(-1.09406051506142,83.9597701021678,11.5417149427421));
#53817=CARTESIAN_POINT('Ctrl Pts',(-1.04695490462354,83.9666268406677,11.5150804142541));
#53818=CARTESIAN_POINT('Ctrl Pts',(-0.998974241279411,83.9735062868492,
11.4902348779045));
#53819=CARTESIAN_POINT('Ctrl Pts',(-0.960745749746977,83.9789874709714,
11.4704392496292));
#53820=CARTESIAN_POINT('Ctrl Pts',(-0.921962617620407,83.9844829431642,
11.4517799302311));
#53821=CARTESIAN_POINT('Ctrl Pts',(-0.88268051519462,83.9899636398392,11.434358889804));
#53822=CARTESIAN_POINT('Ctrl Pts',(-0.816695114645877,83.9991700199222,
11.4050953254942));
#53823=CARTESIAN_POINT('Ctrl Pts',(-0.749301312910663,84.0083340447604,
11.3793265531328));
#53824=CARTESIAN_POINT('Ctrl Pts',(-0.680845101544926,84.01741093097,11.3572724133502));
#53825=CARTESIAN_POINT('Ctrl Pts',(-0.658885316737399,84.0203226677417,
11.350197757098));
#53826=CARTESIAN_POINT('Ctrl Pts',(-0.63681656120727,84.0232253855314,11.3435055292045));
#53827=CARTESIAN_POINT('Ctrl Pts',(-0.61465129680208,84.0261174586991,11.337203426556));
#53828=CARTESIAN_POINT('Ctrl Pts',(-0.586163091571372,84.0298345347708,
11.3291035640706));
#53829=CARTESIAN_POINT('Ctrl Pts',(-0.557514326792003,84.0335343414654,
11.3216473411737));
#53830=CARTESIAN_POINT('Ctrl Pts',(-0.528729632709615,84.0372142064508,
11.3148495329407));
#53831=CARTESIAN_POINT('Ctrl Pts',(-0.465587636856985,84.0452863443369,
11.2999378865628));
#53832=CARTESIAN_POINT('Ctrl Pts',(-0.40178544084305,84.0532626606676,11.2881948406741));
#53833=CARTESIAN_POINT('Ctrl Pts',(-0.337666692143502,84.0611911519319,
11.2795709196196));
#53834=CARTESIAN_POINT('Ctrl Pts',(-0.306667368869647,84.06502431881,11.2754015351248));
#53835=CARTESIAN_POINT('Ctrl Pts',(-0.275593292892654,84.0688464065403,
11.2719610487364));
#53836=CARTESIAN_POINT('Ctrl Pts',(-0.244478997263503,84.072663396452,11.2692433684568));
#53837=CARTESIAN_POINT('Ctrl Pts',(-0.181914129491077,84.080338629469,11.2637786358023));
#53838=CARTESIAN_POINT('Ctrl Pts',(-0.119189614352646,84.0879938376136,
11.2612358390966));
#53839=CARTESIAN_POINT('Ctrl Pts',(-0.0566277683661131,84.0956727428236,
11.2615605645425));
#53840=CARTESIAN_POINT('Ctrl Pts',(-0.0237304160100429,84.0997105976282,
11.2617313172952));
#53841=CARTESIAN_POINT('Ctrl Pts',(0.00912273728367127,84.1037551056446,
11.2626945690433));
#53842=CARTESIAN_POINT('Ctrl Pts',(0.0418902000078147,84.1078132896965,
11.2644403680562));
#53843=CARTESIAN_POINT('Ctrl Pts',(0.0419056063519559,84.107815197741,11.264441188882));
#53844=CARTESIAN_POINT('Ctrl Pts',(0.0419210126854209,84.1078171057897,
11.2644420098812));
#53845=CARTESIAN_POINT('Ctrl Pts',(0.0419364190082416,84.1078190138425,
11.2644428310537));
#53846=CARTESIAN_POINT('Ctrl Pts',(0.11244951656894,84.1165519679687,11.2682012500287));
#53847=CARTESIAN_POINT('Ctrl Pts',(0.182742589941573,84.1253708535697,11.2755933293198));
#53848=CARTESIAN_POINT('Ctrl Pts',(0.252423154216101,84.1342327116647,11.2865505888385));
#53849=CARTESIAN_POINT('Ctrl Pts',(0.311066974026106,84.1416909349831,11.2957723217495));
#53850=CARTESIAN_POINT('Ctrl Pts',(0.36927598288803,84.1491795139062,11.307518873596));
#53851=CARTESIAN_POINT('Ctrl Pts',(0.426797171757144,84.1566702369035,11.3217282112539));
#53852=CARTESIAN_POINT('Ctrl Pts',(0.497941490212501,84.1659350381507,11.3393028418074));
#53853=CARTESIAN_POINT('Ctrl Pts',(0.568033257380841,84.175201088505,11.3606482678425));
#53854=CARTESIAN_POINT('Ctrl Pts',(0.6366482686779,84.1844109178024,11.3856681260411));
#53855=CARTESIAN_POINT('Ctrl Pts',(0.689440677073762,84.1914969629744,11.4049184117593));
#53856=CARTESIAN_POINT('Ctrl Pts',(0.741357765843272,84.1985495835019,11.4263437266034));
#53857=CARTESIAN_POINT('Ctrl Pts',(0.792188040999814,84.2055398094129,11.4498901643867));
#53858=CARTESIAN_POINT('Ctrl Pts',(0.858837515049693,84.2147055060184,11.480764632195));
#53859=CARTESIAN_POINT('Ctrl Pts',(0.923639760751696,84.2237643972766,11.5153000606163));
#53860=CARTESIAN_POINT('Ctrl Pts',(0.986267076755456,84.2327703292168,11.5531856368514));
#53861=CARTESIAN_POINT('Ctrl Pts',(1.03580120012658,84.2398934341535,11.5831506573403));
#53862=CARTESIAN_POINT('Ctrl Pts',(1.08397572511079,84.2469835299394,11.6152120160499));
#53863=CARTESIAN_POINT('Ctrl Pts',(1.13064244971601,84.2540699419949,11.6492341550756));
#53864=CARTESIAN_POINT('Ctrl Pts',(1.18898779521535,84.2629297701321,11.6917705334665));
#53865=CARTESIAN_POINT('Ctrl Pts',(1.24497295725207,84.2717853438818,11.7373664374954));
#53866=CARTESIAN_POINT('Ctrl Pts',(1.29826907067271,84.2806930341029,11.7857151232982));
#53867=CARTESIAN_POINT('Ctrl Pts',(1.32510955955017,84.2851790415237,11.8100640350713));
#53868=CARTESIAN_POINT('Ctrl Pts',(1.35126880282397,84.2896783694891,11.8351114349608));
#53869=CARTESIAN_POINT('Ctrl Pts',(1.37670914154942,84.2941988365226,11.8608205516891));
#53870=CARTESIAN_POINT('Ctrl Pts',(1.37671939860801,84.2942006590885,11.8608309171139));
#53871=CARTESIAN_POINT('Ctrl Pts',(1.37672965554978,84.2942024816579,11.8608412826462));
#53872=CARTESIAN_POINT('Ctrl Pts',(1.37673991237473,84.2942043042308,11.8608516482861));
#53873=CARTESIAN_POINT('Ctrl Pts',(1.42519115891715,84.3028137839123,11.9098169156571));
#53874=CARTESIAN_POINT('Ctrl Pts',(1.47107438780239,84.3115059336939,11.961229336335));
#53875=CARTESIAN_POINT('Ctrl Pts',(1.51414983245555,84.3202183653974,12.0148077257121));
#53876=CARTESIAN_POINT('Ctrl Pts',(1.54021921899898,84.3254911548401,12.0472335254756));
#53877=CARTESIAN_POINT('Ctrl Pts',(1.56525978374168,84.3307712580808,12.0804517127647));
#53878=CARTESIAN_POINT('Ctrl Pts',(1.58921607951863,84.336043799453,12.114391041236));
#53879=CARTESIAN_POINT('Ctrl Pts',(1.63014859721911,84.3450526376745,12.1723808981122));
#53880=CARTESIAN_POINT('Ctrl Pts',(1.66791850612996,84.3540388540006,12.2324828660429));
#53881=CARTESIAN_POINT('Ctrl Pts',(1.70228293889561,84.3629343762338,12.2943846515697));
#53882=CARTESIAN_POINT('Ctrl Pts',(1.71235776328242,84.365542329199,12.3125327648432));
#53883=CARTESIAN_POINT('Ctrl Pts',(1.72213967286767,84.368142442784,12.3308353075211));
#53884=CARTESIAN_POINT('Ctrl Pts',(1.73162207870361,84.3707328924981,12.349283710003));
#53885=CARTESIAN_POINT('Ctrl Pts',(1.76665572128149,84.3803035532534,12.4174430727075));
#53886=CARTESIAN_POINT('Ctrl Pts',(1.79760864253359,84.3897436393863,12.4876088936978));
#53887=CARTESIAN_POINT('Ctrl Pts',(1.8243893325239,84.3991173094973,12.5592399400937));
#53888=CARTESIAN_POINT('Ctrl Pts',(1.83613596899814,84.4032288202636,12.5906589910064));
#53889=CARTESIAN_POINT('Ctrl Pts',(1.84708005500493,84.4073276386148,12.6223606004483));
#53890=CARTESIAN_POINT('Ctrl Pts',(1.85721419484448,84.4114195764118,12.6543022099861));
#53891=CARTESIAN_POINT('Ctrl Pts',(1.87914681723638,84.4202754761696,12.7234312403403));
#53892=CARTESIAN_POINT('Ctrl Pts',(1.89733714776918,84.429131228048,12.7936688366494));
#53893=CARTESIAN_POINT('Ctrl Pts',(1.91172596705363,84.4380582798587,12.8645489414833));
#53894=CARTESIAN_POINT('Ctrl Pts',(1.91879856644955,84.4424462327543,12.899388950015));
#53895=CARTESIAN_POINT('Ctrl Pts',(1.92495305738059,84.4468515157404,12.9343849044072));
#53896=CARTESIAN_POINT('Ctrl Pts',(1.93018399265379,84.4512832086093,12.9694857532766));
#53897=CARTESIAN_POINT('Ctrl Pts',(1.94033215932514,84.4598808217552,13.0375824216598));
#53898=CARTESIAN_POINT('Ctrl Pts',(1.94681973089025,84.4684651833917,13.1060811090079));
#53899=CARTESIAN_POINT('Ctrl Pts',(1.94951938827062,84.4770235061186,13.1745130007201));
#53900=CARTESIAN_POINT('Ctrl Pts',(1.94952148319877,84.4770301473581,13.1745661037166));
#53901=CARTESIAN_POINT('Ctrl Pts',(1.94952357584832,84.4770367885819,13.1746192066731));
#53902=CARTESIAN_POINT('Ctrl Pts',(1.94952566621936,84.4770434297901,13.1746723095892));
#53903=CARTESIAN_POINT('Ctrl Pts',(1.95321377855843,84.4887607380318,13.2683635813158));
#53904=CARTESIAN_POINT('Ctrl Pts',(1.94997710535719,84.5005654525547,13.3622008441398));
#53905=CARTESIAN_POINT('Ctrl Pts',(1.94023064075133,84.5124864410356,13.4552283662948));
#53906=CARTESIAN_POINT('Ctrl Pts',(1.93889149641256,84.5141243605153,13.4680101579169));
#53907=CARTESIAN_POINT('Ctrl Pts',(1.93742952483265,84.5157644806227,13.4807767086174));
#53908=CARTESIAN_POINT('Ctrl Pts',(1.93584586179906,84.5174068815216,13.4935255863242));
#53909=CARTESIAN_POINT('Ctrl Pts',(1.93078145231806,84.5226591293216,13.5342953307461));
#53910=CARTESIAN_POINT('Ctrl Pts',(1.92441474003774,84.5278965434236,13.5748785418289));
#53911=CARTESIAN_POINT('Ctrl Pts',(1.91674824229219,84.5330985451104,13.6151934729252));
#53912=CARTESIAN_POINT('Ctrl Pts',(1.90072584242437,84.5439703347992,13.6994486267263));
#53913=CARTESIAN_POINT('Ctrl Pts',(1.8790235834995,84.5546856545393,13.78253754425));
#53914=CARTESIAN_POINT('Ctrl Pts',(1.85200845167572,84.5653055336086,13.86378565604));
#53915=CARTESIAN_POINT('Ctrl Pts',(1.84567881643702,84.5677937672854,13.8828220581135));
#53916=CARTESIAN_POINT('Ctrl Pts',(1.83905736303953,84.5702767861689,13.9017575639899));
#53917=CARTESIAN_POINT('Ctrl Pts',(1.83214849970748,84.5727554200334,13.9205837604938));
#53918=CARTESIAN_POINT('Ctrl Pts',(1.80276168665853,84.583298275854,14.0006608861357));
#53919=CARTESIAN_POINT('Ctrl Pts',(1.76817737507296,84.5937627800115,14.0787579868579));
#53920=CARTESIAN_POINT('Ctrl Pts',(1.72877618720114,84.6042221585337,14.1541803414388));
#53921=CARTESIAN_POINT('Ctrl Pts',(1.71877371941299,84.6068773981953,14.1733272177882));
#53922=CARTESIAN_POINT('Ctrl Pts',(1.70846074517972,84.6095323429264,14.192301966208));
#53923=CARTESIAN_POINT('Ctrl Pts',(1.69784329734153,84.6121882626014,14.2110937120938));
#53924=CARTESIAN_POINT('Ctrl Pts',(1.6593259326395,84.6218232547671,14.2792653236433));
#53925=CARTESIAN_POINT('Ctrl Pts',(1.61680242456352,84.6314719811794,14.3450252545571));
#53926=CARTESIAN_POINT('Ctrl Pts',(1.57059790327892,84.6411879864025,14.4078184499548));
#53927=CARTESIAN_POINT('Ctrl Pts',(1.55518597834373,84.6444288455004,14.4287636732144));
#53928=CARTESIAN_POINT('Ctrl Pts',(1.5393645425185,84.6476772306958,14.4493792380232));
#53929=CARTESIAN_POINT('Ctrl Pts',(1.52314571628208,84.650935249667,14.4696458332225));
#53930=CARTESIAN_POINT('Ctrl Pts',(1.51321437916295,84.6529302451291,14.482055756496));
#53931=CARTESIAN_POINT('Ctrl Pts',(1.50313420107118,84.6549287667643,14.4943345436136));
#53932=CARTESIAN_POINT('Ctrl Pts',(1.49290815883134,84.6569312013671,14.506477572868));
#53933=CARTESIAN_POINT('Ctrl Pts',(1.49290573429091,84.6569316761337,14.5064804519159));
#53934=CARTESIAN_POINT('Ctrl Pts',(1.49290330974226,84.6569321509006,14.5064833309562));
#53935=CARTESIAN_POINT('Ctrl Pts',(1.49290088518542,84.6569326256676,14.5064862099888));
#53936=CARTESIAN_POINT('Ctrl Pts',(1.45024439600519,84.6652854497019,14.5571385283166));
#53937=CARTESIAN_POINT('Ctrl Pts',(1.40498648153156,84.6737130343868,14.6054928961033));
#53938=CARTESIAN_POINT('Ctrl Pts',(1.35736068401196,84.6821171446992,14.6513015909629));
#53939=CARTESIAN_POINT('Ctrl Pts',(1.33661729455568,84.6857775502425,14.6712535423726));
#53940=CARTESIAN_POINT('Ctrl Pts',(1.31542527026016,84.6894334213537,14.6907222036987));
#53941=CARTESIAN_POINT('Ctrl Pts',(1.29380661699577,84.6930762686412,14.7096856787528));
#53942=CARTESIAN_POINT('Ctrl Pts',(1.21819377269838,84.7058173973959,14.7760118401961));
#53943=CARTESIAN_POINT('Ctrl Pts',(1.13733310798374,84.7183994754612,14.8361805171429));
#53944=CARTESIAN_POINT('Ctrl Pts',(1.05237565193126,84.7308790234823,14.8897122344806));
#53945=CARTESIAN_POINT('Ctrl Pts',(1.03074457149719,84.7340564503919,14.9033419844438));
#53946=CARTESIAN_POINT('Ctrl Pts',(1.00884764583026,84.737227257367,14.9165414830533));
#53947=CARTESIAN_POINT('Ctrl Pts',(0.986703343889802,84.7403924316647,14.929302767917));
#53948=CARTESIAN_POINT('Ctrl Pts',(0.897700508179527,84.7531139655734,14.9805931876028));
#53949=CARTESIAN_POINT('Ctrl Pts',(0.804705082511613,84.7657460769024,15.0248040056999));
#53950=CARTESIAN_POINT('Ctrl Pts',(0.708987808209041,84.778359764823,15.0613999764066));
#53951=CARTESIAN_POINT('Ctrl Pts',(0.686393878910136,84.7813372082902,15.0700384043268));
#53952=CARTESIAN_POINT('Ctrl Pts',(0.663648114616261,84.784313656368,15.0782526849068));
#53953=CARTESIAN_POINT('Ctrl Pts',(0.640766884118675,84.7872901001448,15.0860360142635));
#53954=CARTESIAN_POINT('Ctrl Pts',(0.555343153654182,84.7984022180423,15.1150939370509));
#53955=CARTESIAN_POINT('Ctrl Pts',(0.46803366463815,84.8095155007575,15.1381429345199));
#53956=CARTESIAN_POINT('Ctrl Pts',(0.379741860209001,84.8206689781605,15.1548254304413));
#53957=CARTESIAN_POINT('Ctrl Pts',(0.345706641857807,84.8249684829814,15.1612562922296));
#53958=CARTESIAN_POINT('Ctrl Pts',(0.311525238234077,84.8292739996287,15.1667415968204));
#53959=CARTESIAN_POINT('Ctrl Pts',(0.277248428798174,84.8335879080472,15.171262700616));
#53960=CARTESIAN_POINT('Ctrl Pts',(0.277228626528439,84.8335904002622,15.1712653125312));
#53961=CARTESIAN_POINT('Ctrl Pts',(0.277208824226786,84.83359289248,15.1712679241245));
#53962=CARTESIAN_POINT('Ctrl Pts',(0.277189021893341,84.8335953847006,15.1712705353961));
#53963=CARTESIAN_POINT('Ctrl Pts',(0.233350133862176,84.8391127233394,15.1770514319758));
#53964=CARTESIAN_POINT('Ctrl Pts',(0.189338665706105,84.8446426258861,15.1812538886977));
#53965=CARTESIAN_POINT('Ctrl Pts',(0.145258156107619,84.8501541848413,15.1838692224844));
#53966=CARTESIAN_POINT('Ctrl Pts',(0.0304069274952764,84.8645144842874,
15.1906834426777));
#53967=CARTESIAN_POINT('Ctrl Pts',(-0.0849308408675299,84.8788334517048,
15.1868143314595));
#53968=CARTESIAN_POINT('Ctrl Pts',(-0.198933758964356,84.8931556939499,
15.1726946107426));
#53969=CARTESIAN_POINT('Ctrl Pts',(-0.223228356926069,84.8962078361499,
15.1696856269036));
#53970=CARTESIAN_POINT('Ctrl Pts',(-0.247462405555277,84.8992601386906,
15.1662109498615));
#53971=CARTESIAN_POINT('Ctrl Pts',(-0.271618367075097,84.9023130519731,
15.1622744760133));
#53972=CARTESIAN_POINT('Ctrl Pts',(-0.364907236343795,84.9141032192932,
15.147072050976));
#53973=CARTESIAN_POINT('Ctrl Pts',(-0.457026917293188,84.9258838533372,
15.1249613059293));
#53974=CARTESIAN_POINT('Ctrl Pts',(-0.546873661499603,84.9376491320311,
15.0961755835741));
#53975=CARTESIAN_POINT('Ctrl Pts',(-0.615648390383315,84.9466550660754,
15.0741410594721));
#53976=CARTESIAN_POINT('Ctrl Pts',(-0.683094787328754,84.9556525017402,
15.0481942569581));
#53977=CARTESIAN_POINT('Ctrl Pts',(-0.748707450847617,84.9646368100891,
15.0184586558434));
#53978=CARTESIAN_POINT('Ctrl Pts',(-0.791487566201658,84.9704946693335,
14.9990707453764));
#53979=CARTESIAN_POINT('Ctrl Pts',(-0.833497079961818,84.9763481286158,
14.9780688999819));
#53980=CARTESIAN_POINT('Ctrl Pts',(-0.874636646032348,84.982197574172,14.9555393532476));
#53981=CARTESIAN_POINT('Ctrl Pts',(-0.924245481152777,84.9892512261149,
14.9283717217912));
#53982=CARTESIAN_POINT('Ctrl Pts',(-0.97258930392851,84.9962990375357,14.8989826808508));
#53983=CARTESIAN_POINT('Ctrl Pts',(-1.01949348913406,85.0033416679318,14.8675220679944));
#53984=CARTESIAN_POINT('Ctrl Pts',(-1.05768897855176,85.0090766937848,14.8419027442567));
#53985=CARTESIAN_POINT('Ctrl Pts',(-1.09493703556075,85.0148093498287,14.8149050405272));
#53986=CARTESIAN_POINT('Ctrl Pts',(-1.13114809258377,85.0205410247945,14.7866021628256));
#53987=CARTESIAN_POINT('Ctrl Pts',(-1.18079463350689,85.0283993382252,14.7477979938349));
#53988=CARTESIAN_POINT('Ctrl Pts',(-1.22848950474429,85.0362554172582,14.7065422562557));
#53989=CARTESIAN_POINT('Ctrl Pts',(-1.27398630056078,85.0441110927398,14.6630287743675));
#53990=CARTESIAN_POINT('Ctrl Pts',(-1.32466816608288,85.0528620450036,14.6145562523386));
#53991=CARTESIAN_POINT('Ctrl Pts',(-1.37262196931536,85.0616127845679,14.5632784958926));
#53992=CARTESIAN_POINT('Ctrl Pts',(-1.41745419185327,85.0703558398986,14.5095270121629));
#53993=CARTESIAN_POINT('Ctrl Pts',(-1.45012075667082,85.0767263825015,14.470361514048));
#53994=CARTESIAN_POINT('Ctrl Pts',(-1.48113202213731,85.0830932242741,14.4298806369453));
#53995=CARTESIAN_POINT('Ctrl Pts',(-1.51033674457732,85.0894520383892,14.3882280783937));
#53996=CARTESIAN_POINT('Ctrl Pts',(-1.5183179595479,85.0911898074269,14.376845055509));
#53997=CARTESIAN_POINT('Ctrl Pts',(-1.5261641850647,85.0929269493669,14.3653747431672));
#53998=CARTESIAN_POINT('Ctrl Pts',(-1.53387239419349,85.0946633543111,14.3538203086066));
#53999=CARTESIAN_POINT('Ctrl Pts',(-1.54397549056108,85.0969392482562,14.3386759911796));
#54000=CARTESIAN_POINT('Ctrl Pts',(-1.55384693578398,85.099215102824,14.3233789956478));
#54001=CARTESIAN_POINT('Ctrl Pts',(-1.56348446782898,85.1014908120453,14.3079375425852));
#54002=CARTESIAN_POINT('Ctrl Pts',(-1.60584304572334,85.111492937679,14.2400697534772));
#54003=CARTESIAN_POINT('Ctrl Pts',(-1.64367824027177,85.1214920067102,14.1694110929465));
#54004=CARTESIAN_POINT('Ctrl Pts',(-1.67681194118092,85.1314758558772,14.096697829742));
#54005=CARTESIAN_POINT('Ctrl Pts',(-1.67977505246016,85.1323687007833,14.0901951607241));
#54006=CARTESIAN_POINT('Ctrl Pts',(-1.68270059459859,85.1332614240155,14.0836760742639));
#54007=CARTESIAN_POINT('Ctrl Pts',(-1.68558845876882,85.1341540169019,14.0771411045514));
#54008=CARTESIAN_POINT('Ctrl Pts',(-1.71053382662586,85.1418642333748,14.020692042614));
#54009=CARTESIAN_POINT('Ctrl Pts',(-1.73277695401505,85.1497096690635,13.9630881628073));
#54010=CARTESIAN_POINT('Ctrl Pts',(-1.7521451336866,85.1575209055195,13.9045489350716));
#54011=CARTESIAN_POINT('Ctrl Pts',(-1.75531802257158,85.1588005397314,13.8949590578519));
#54012=CARTESIAN_POINT('Ctrl Pts',(-1.75841371544478,85.1600792417608,13.8853441835167));
#54013=CARTESIAN_POINT('Ctrl Pts',(-1.76143140981071,85.1613562499825,13.8757054010843));
#54014=CARTESIAN_POINT('Ctrl Pts',(-1.78711647398328,85.172225487932,13.7936650367198));
#54015=CARTESIAN_POINT('Ctrl Pts',(-1.80710976981629,85.1829063505651,13.7098598581591));
#54016=CARTESIAN_POINT('Ctrl Pts',(-1.82131724798675,85.1935080294538,13.6250864076034));
#54017=CARTESIAN_POINT('Ctrl Pts',(-1.82442537749334,85.1958273285284,13.6065407614384));
#54018=CARTESIAN_POINT('Ctrl Pts',(-1.82725652043322,85.1981428589666,13.5879485953943));
#54019=CARTESIAN_POINT('Ctrl Pts',(-1.82980953101542,85.2004557989677,13.5693179618627));
#54020=CARTESIAN_POINT('Ctrl Pts',(-1.8409357181689,85.2105357428215,13.4881244419824));
#54021=CARTESIAN_POINT('Ctrl Pts',(-1.84689003772633,85.2207240542008,13.4062065620465));
#54022=CARTESIAN_POINT('Ctrl Pts',(-1.84744767118077,85.2309365956636,13.3243157245479));
#54023=CARTESIAN_POINT('Ctrl Pts',(-1.8476067617552,85.2338501925342,13.3009525990486));
#54024=CARTESIAN_POINT('Ctrl Pts',(-1.8473268300071,85.2367657388299,13.2775918996761));
#54025=CARTESIAN_POINT('Ctrl Pts',(-1.84660325967835,85.2396812268938,13.254251562075));
#54026=CARTESIAN_POINT('Ctrl Pts',(-1.84525068982847,85.2451311480641,13.210621474341));
#54027=CARTESIAN_POINT('Ctrl Pts',(-1.8423460763394,85.2505783880291,13.1670660463023));
#54028=CARTESIAN_POINT('Ctrl Pts',(-1.83787331074505,85.2560199081706,13.1237159040522));
#54029=CARTESIAN_POINT('Ctrl Pts',(-1.8378683536336,85.2560259389409,13.1236678596192));
#54030=CARTESIAN_POINT('Ctrl Pts',(-1.83786339459672,85.2560319697041,13.1236198154383));
#54031=CARTESIAN_POINT('Ctrl Pts',(-1.8378584336345,85.2560380004604,13.1235717715096));
#54032=CARTESIAN_POINT('Ctrl Pts',(-1.82797948276968,85.2680472724092,13.0279000872513));
#54033=CARTESIAN_POINT('Ctrl Pts',(-1.81044219892233,85.28005266257,12.9330379411312));
#54034=CARTESIAN_POINT('Ctrl Pts',(-1.78571394556554,85.2921023437014,12.8401665668285));
#54035=CARTESIAN_POINT('Ctrl Pts',(-1.78409750453677,85.2928900094812,12.8340957336947));
#54036=CARTESIAN_POINT('Ctrl Pts',(-1.78245035058582,85.293677865537,12.8280333953093));
#54037=CARTESIAN_POINT('Ctrl Pts',(-1.78077261990269,85.2944659257482,12.8219798764064));
#54038=CARTESIAN_POINT('Ctrl Pts',(-1.76631134890319,85.3012586442652,12.7698013126855));
#54039=CARTESIAN_POINT('Ctrl Pts',(-1.74961557956881,85.3081305891139,12.7182583022491));
#54040=CARTESIAN_POINT('Ctrl Pts',(-1.73067981586692,85.3149635245604,12.6675575414924));
#54041=CARTESIAN_POINT('Ctrl Pts',(-1.69540238770607,85.3276933195207,12.5731017554225));
#54042=CARTESIAN_POINT('Ctrl Pts',(-1.65234437070366,85.3402888608063,12.4815558298799));
#54043=CARTESIAN_POINT('Ctrl Pts',(-1.60208024214139,85.3529049691793,12.3942033494227));
#54044=CARTESIAN_POINT('Ctrl Pts',(-1.60207728341293,85.3529057118091,12.3941982075396));
#54045=CARTESIAN_POINT('Ctrl Pts',(-1.6020743246595,85.3529064544391,12.394193065671));
#54046=CARTESIAN_POINT('Ctrl Pts',(-1.6020713658811,85.3529071970693,12.3941879238167));
#54047=CARTESIAN_POINT('Ctrl Pts',(-1.55393748472671,85.3649884238915,12.3105394146255));
#54048=CARTESIAN_POINT('Ctrl Pts',(-1.49919060049532,85.3771228765528,12.2306974760314));
#54049=CARTESIAN_POINT('Ctrl Pts',(-1.43866195428871,85.3892315961811,12.1555799556733));
#54050=CARTESIAN_POINT('Ctrl Pts',(-1.42326560832809,85.3923116260219,12.1364727163144));
#54051=CARTESIAN_POINT('Ctrl Pts',(-1.40749543808891,85.395389974111,12.1176711391185));
#54052=CARTESIAN_POINT('Ctrl Pts',(-1.39136565169905,85.3984653071638,12.099190255997));
#54053=CARTESIAN_POINT('Ctrl Pts',(-1.35810659243762,85.4048065370958,12.0610833169411));
#54054=CARTESIAN_POINT('Ctrl Pts',(-1.32331641102166,85.4111350656515,12.0243374978035));
#54055=CARTESIAN_POINT('Ctrl Pts',(-1.28711150508702,85.4174404648073,11.9890756728186));
#54056=CARTESIAN_POINT('Ctrl Pts',(-1.21026713566218,85.430823579874,11.9142329785544));
#54057=CARTESIAN_POINT('Ctrl Pts',(-1.12703675666197,85.4441024937404,11.8460620040289));
#54058=CARTESIAN_POINT('Ctrl Pts',(-1.03860274557366,85.4574053086368,11.7856639216873));
#54059=CARTESIAN_POINT('Ctrl Pts',(-1.02851505306579,85.458922764472,11.7787742954538));
#54060=CARTESIAN_POINT('Ctrl Pts',(-1.01835959564601,85.4604405376539,11.7719858043035));
#54061=CARTESIAN_POINT('Ctrl Pts',(-1.00813808582199,85.46195882316,11.7653000811902));
#54062=CARTESIAN_POINT('Ctrl Pts',(-0.994262190381637,85.4640199248264,
11.7562240839588));
#54063=CARTESIAN_POINT('Ctrl Pts',(-0.980264984472829,85.466081951658,11.7473377229105));
#54064=CARTESIAN_POINT('Ctrl Pts',(-0.966151166278289,85.4681453614856,
11.7386452804256));
#54065=CARTESIAN_POINT('Ctrl Pts',(-0.940392368458494,85.4719112422581,
11.7227809079757));
#54066=CARTESIAN_POINT('Ctrl Pts',(-0.914245017282329,85.4756817621344,
11.7075624545021));
#54067=CARTESIAN_POINT('Ctrl Pts',(-0.887741119288026,85.479461189823,11.6930162484083));
#54068=CARTESIAN_POINT('Ctrl Pts',(-0.883792159728891,85.4800243072597,
11.6908489302419));
#54069=CARTESIAN_POINT('Ctrl Pts',(-0.879835197767357,85.4805876560108,
11.6886964736288));
#54070=CARTESIAN_POINT('Ctrl Pts',(-0.875870294913486,85.4811512272568,
11.6865589593512));
#54071=CARTESIAN_POINT('Ctrl Pts',(-0.856700558214391,85.4838760134103,
11.6762243843558));
#54072=CARTESIAN_POINT('Ctrl Pts',(-0.837345201296476,85.4866060015936,
11.6662390695374));
#54073=CARTESIAN_POINT('Ctrl Pts',(-0.817814529132744,85.4893401868611,
11.6566048832587));
#54074=CARTESIAN_POINT('Ctrl Pts',(-0.746638371608368,85.4993044522829,
11.621494757276));
#54075=CARTESIAN_POINT('Ctrl Pts',(-0.673158530375076,85.5093202081103,
11.5910629328178));
#54076=CARTESIAN_POINT('Ctrl Pts',(-0.598021337714578,85.5192973541955,
11.5654695330317));
#54077=CARTESIAN_POINT('Ctrl Pts',(-0.471464483992447,85.5361022969004,
11.5223614524889));
#54078=CARTESIAN_POINT('Ctrl Pts',(-0.340174224350369,85.5527999218405,
11.4929617275192));
#54079=CARTESIAN_POINT('Ctrl Pts',(-0.207167320122267,85.5694565224654,
11.4777640481892));
#54080=CARTESIAN_POINT('Ctrl Pts',(-0.181477797397712,85.5726736495969,
11.4748287033605));
#54081=CARTESIAN_POINT('Ctrl Pts',(-0.155724129085211,85.5758892563297,
11.4724232758611));
#54082=CARTESIAN_POINT('Ctrl Pts',(-0.129927918261811,85.5791038343749,
11.470551501836));
#54083=CARTESIAN_POINT('Ctrl Pts',(-0.0492570413694765,85.5891565832656,
11.4646980199824));
#54084=CARTESIAN_POINT('Ctrl Pts',(0.031825063993792,85.5991988281697,11.4640642794784));
#54085=CARTESIAN_POINT('Ctrl Pts',(0.112634651844854,85.6092404307314,11.4687636308537));
#54086=CARTESIAN_POINT('Ctrl Pts',(0.112652623295684,85.609242663909,11.4687646759545));
#54087=CARTESIAN_POINT('Ctrl Pts',(0.112670594731866,85.6092448970854,11.4687657213194));
#54088=CARTESIAN_POINT('Ctrl Pts',(0.112688566153371,85.6092471302604,11.4687667669486));
#54089=CARTESIAN_POINT('Ctrl Pts',(0.143724140611242,85.6131036904697,11.4705725061627));
#54090=CARTESIAN_POINT('Ctrl Pts',(0.174715989893316,85.6169562827353,11.4731660658191));
#54091=CARTESIAN_POINT('Ctrl Pts',(0.205623145273929,85.6208032910311,11.4765451390782));
#54092=CARTESIAN_POINT('Ctrl Pts',(0.29075584452018,85.6313997434127,11.4858526804534));
#54093=CARTESIAN_POINT('Ctrl Pts',(0.375255485367746,85.6419536962468,11.501120936313));
#54094=CARTESIAN_POINT('Ctrl Pts',(0.458217992881756,85.6525722944883,11.5222495823753));
#54095=CARTESIAN_POINT('Ctrl Pts',(0.510912467054124,85.6593168043585,11.5356696552202));
#54096=CARTESIAN_POINT('Ctrl Pts',(0.56298461294796,85.6660876117512,11.5514542628319));
#54097=CARTESIAN_POINT('Ctrl Pts',(0.61418084935393,85.6729114254548,11.5695679816851));
#54098=CARTESIAN_POINT('Ctrl Pts',(0.614181367021844,85.6729114944534,11.569568164841));
#54099=CARTESIAN_POINT('Ctrl Pts',(0.614181884689718,85.672911563452,11.5695683479971));
#54100=CARTESIAN_POINT('Ctrl Pts',(0.614182402357452,85.6729116324507,11.5695685311534));
#54101=CARTESIAN_POINT('Ctrl Pts',(0.693738687769726,85.6835154889403,11.5977163899175));
#54102=CARTESIAN_POINT('Ctrl Pts',(0.771285993621759,85.6942295421365,11.6315422815696));
#54103=CARTESIAN_POINT('Ctrl Pts',(0.84616769083285,85.7049409977878,11.670540646632));
#54104=CARTESIAN_POINT('Ctrl Pts',(0.888237717285468,85.710958906561,11.6924507035736));
#54105=CARTESIAN_POINT('Ctrl Pts',(0.929466225656976,85.7169759433611,11.7159924317119));
#54106=CARTESIAN_POINT('Ctrl Pts',(0.969737048758562,85.7229717276922,11.741069015838));
#54107=CARTESIAN_POINT('Ctrl Pts',(1.08513929120223,85.7401535706178,11.812929827664));
#54108=CARTESIAN_POINT('Ctrl Pts',(1.19276131724192,85.7571688119804,11.8974403571697));
#54109=CARTESIAN_POINT('Ctrl Pts',(1.2902550715294,85.7740559112678,11.9923977871438));
#54110=CARTESIAN_POINT('Ctrl Pts',(1.38122592859114,85.7898131657369,12.0810020146891));
#54111=CARTESIAN_POINT('Ctrl Pts',(1.46337607084306,85.8054590702191,12.178701700058));
#54112=CARTESIAN_POINT('Ctrl Pts',(1.53476837406012,85.8210220936813,12.2837180051361));
#54113=CARTESIAN_POINT('Ctrl Pts',(1.53988742725632,85.822138011524,12.2912480052613));
#54114=CARTESIAN_POINT('Ctrl Pts',(1.54495116389373,85.8232535018488,12.2988156298782));
#54115=CARTESIAN_POINT('Ctrl Pts',(1.54995886674597,85.8243685745973,12.3064202269441));
#54116=CARTESIAN_POINT('Ctrl Pts',(1.59851553354426,85.835180760843,12.3801574067962));
#54117=CARTESIAN_POINT('Ctrl Pts',(1.64183205644228,85.8460018353106,12.4573960826899));
#54118=CARTESIAN_POINT('Ctrl Pts',(1.67924132530039,85.8569743091173,12.5374343967329));
#54119=CARTESIAN_POINT('Ctrl Pts',(1.68810875094259,85.8595752045254,12.5564065343867));
#54120=CARTESIAN_POINT('Ctrl Pts',(1.69664449412662,85.8621846198134,12.5755359644325));
#54121=CARTESIAN_POINT('Ctrl Pts',(1.70484010279699,85.8648044767534,12.594813334006));
#54122=CARTESIAN_POINT('Ctrl Pts',(1.70485234315749,85.8648083895798,12.5948421252725));
#54123=CARTESIAN_POINT('Ctrl Pts',(1.70486458275931,85.8648123024294,12.5948709168689));
#54124=CARTESIAN_POINT('Ctrl Pts',(1.70487682160245,85.8648162153023,12.5948997087954));
#54125=CARTESIAN_POINT('Ctrl Pts',(1.72779095621515,85.8721420790203,12.6488053002183));
#54126=CARTESIAN_POINT('Ctrl Pts',(1.74805965311354,85.8794788974896,12.7039665537236));
#54127=CARTESIAN_POINT('Ctrl Pts',(1.76562216590808,85.8868175658139,12.7600372081266));
#54128=CARTESIAN_POINT('Ctrl Pts',(1.78291244949569,85.8940424804925,12.8152387346342));
#54129=CARTESIAN_POINT('Ctrl Pts',(1.7975816587997,85.901269699012,12.8713249993773));
#54130=CARTESIAN_POINT('Ctrl Pts',(1.80959903861607,85.908493030258,12.9279776106178));
#54131=CARTESIAN_POINT('Ctrl Pts',(1.81942218280065,85.9143974641202,12.974286105244));
#54132=CARTESIAN_POINT('Ctrl Pts',(1.82747933074973,85.9203133829409,13.0209777274232));
#54133=CARTESIAN_POINT('Ctrl Pts',(1.8337621508321,85.9262359622378,13.0679168192808));
#54134=CARTESIAN_POINT('Ctrl Pts',(1.84424409691159,85.9361169004198,13.146227677052));
#54135=CARTESIAN_POINT('Ctrl Pts',(1.84976760624578,85.9459140879283,13.2252480455859));
#54136=CARTESIAN_POINT('Ctrl Pts',(1.85030224302454,85.9557598786602,13.3043850444585));
#54137=CARTESIAN_POINT('Ctrl Pts',(1.85037689590171,85.9571346748497,13.3154351721182));
#54138=CARTESIAN_POINT('Ctrl Pts',(1.85035420036891,85.9585104216572,13.3264876003774));
#54139=CARTESIAN_POINT('Ctrl Pts',(1.85023399555252,85.9598874822514,13.3375407366125));
#54140=CARTESIAN_POINT('Ctrl Pts',(1.84925342482349,85.9711208533536,13.4277066898715));
#54141=CARTESIAN_POINT('Ctrl Pts',(1.84176383598627,85.9823729208819,13.517921232015));
#54142=CARTESIAN_POINT('Ctrl Pts',(1.82766289675517,85.9936318843678,13.6070941099045));
#54143=CARTESIAN_POINT('Ctrl Pts',(1.82765574538415,85.9936375944147,13.6071393344334));
#54144=CARTESIAN_POINT('Ctrl Pts',(1.82764859231378,85.9936433044635,13.6071845586945));
#54145=CARTESIAN_POINT('Ctrl Pts',(1.82764143754412,85.993649014514,13.6072297826876));
#54146=CARTESIAN_POINT('Ctrl Pts',(1.81401739509538,86.0045220368684,13.6933448682657));
#54147=CARTESIAN_POINT('Ctrl Pts',(1.79421743148949,86.0154099384373,13.7785545676331));
#54148=CARTESIAN_POINT('Ctrl Pts',(1.76858430112525,86.0263033140579,13.8620023507837));
#54149=CARTESIAN_POINT('Ctrl Pts',(1.74374594861024,86.0368589309451,13.9428627617065));
#54150=CARTESIAN_POINT('Ctrl Pts',(1.71343311483025,86.0474197062229,14.0220691362845));
#54151=CARTESIAN_POINT('Ctrl Pts',(1.67796781209554,86.0579833269728,14.0988988079675));
#54152=CARTESIAN_POINT('Ctrl Pts',(1.64152004434362,86.0688395826938,14.1778568264822));
#54153=CARTESIAN_POINT('Ctrl Pts',(1.59963401777733,86.0796986852896,14.2543051112353));
#54154=CARTESIAN_POINT('Ctrl Pts',(1.55264416598259,86.0906938445333,14.327527131553));
#54155=CARTESIAN_POINT('Ctrl Pts',(1.50804735545421,86.1011290558565,14.3970201910518));
#54156=CARTESIAN_POINT('Ctrl Pts',(1.45883989384623,86.1115889042444,14.4636015287737));
#54157=CARTESIAN_POINT('Ctrl Pts',(1.4052349504777,86.1219992676407,14.5266672531493));
#54158=CARTESIAN_POINT('Ctrl Pts',(1.40235853756719,86.1225578822347,14.5300513265651));
#54159=CARTESIAN_POINT('Ctrl Pts',(1.39946944913583,86.1231163561666,14.5334252793147));
#54160=CARTESIAN_POINT('Ctrl Pts',(1.39656771389387,86.1236746845869,14.5367890190033));
#54161=CARTESIAN_POINT('Ctrl Pts',(1.39656494206585,86.1236752179196,14.5367922321524));
#54162=CARTESIAN_POINT('Ctrl Pts',(1.39656217022662,86.1236757512522,14.5367954452917));
#54163=CARTESIAN_POINT('Ctrl Pts',(1.39655939837615,86.1236762845845,14.5367986584214));
#54164=CARTESIAN_POINT('Ctrl Pts',(1.38123047217407,86.1266257264846,14.55456795324));
#54165=CARTESIAN_POINT('Ctrl Pts',(1.36555833065369,86.1295691303106,14.5720410264516));
#54166=CARTESIAN_POINT('Ctrl Pts',(1.34955505731457,86.1325059203192,14.5892111711369));
#54167=CARTESIAN_POINT('Ctrl Pts',(1.29375609819163,86.1427456895323,14.6490786858092));
#54168=CARTESIAN_POINT('Ctrl Pts',(1.23392824442023,86.1529058263795,14.7052724636152));
#54169=CARTESIAN_POINT('Ctrl Pts',(1.17059813120406,86.163044554318,14.7574500355268));
#54170=CARTESIAN_POINT('Ctrl Pts',(1.16667592349548,86.163672473563,14.7606815357465));
#54171=CARTESIAN_POINT('Ctrl Pts',(1.16274027004173,86.164300310863,14.7638976200291));
#54172=CARTESIAN_POINT('Ctrl Pts',(1.15879129130522,86.1649280801157,14.7670982024371));
#54173=CARTESIAN_POINT('Ctrl Pts',(1.09127884774159,86.1756605350288,14.8218159291218));
#54174=CARTESIAN_POINT('Ctrl Pts',(1.01987269787036,86.1863733647325,14.8720037640754));
#54175=CARTESIAN_POINT('Ctrl Pts',(0.945251604395908,86.1972037988522,14.9171692115491));
#54176=CARTESIAN_POINT('Ctrl Pts',(0.871359207707871,86.2079284706173,14.9618936052283));
#54177=CARTESIAN_POINT('Ctrl Pts',(0.794308857734811,86.2187200572444,15.0016847114781));
#54178=CARTESIAN_POINT('Ctrl Pts',(0.714843889454336,86.2295214956863,15.0360130145325));
#54179=CARTESIAN_POINT('Ctrl Pts',(0.655457380330701,86.237593728476,15.0616675655461));
#54180=CARTESIAN_POINT('Ctrl Pts',(0.594724679377242,86.2456711957035,15.0842699273015));
#54181=CARTESIAN_POINT('Ctrl Pts',(0.532996297408288,86.2537458065404,15.1036100910029));
#54182=CARTESIAN_POINT('Ctrl Pts',(0.532966724735384,86.253749674904,15.1036193564383));
#54183=CARTESIAN_POINT('Ctrl Pts',(0.53293715183407,86.253753543267,15.1036286211255));
#54184=CARTESIAN_POINT('Ctrl Pts',(0.532907578704435,86.2537574116292,15.1036378850645));
#54185=CARTESIAN_POINT('Ctrl Pts',(0.461793619796277,86.2630595909761,15.1259147081811));
#54186=CARTESIAN_POINT('Ctrl Pts',(0.38917133601737,86.2723823597116,15.1439193552667));
#54187=CARTESIAN_POINT('Ctrl Pts',(0.315674590734811,86.2817671702878,15.1575840066373));
#54188=CARTESIAN_POINT('Ctrl Pts',(0.300082603228587,86.2837581135424,15.1604828979097));
#54189=CARTESIAN_POINT('Ctrl Pts',(0.284451311816776,86.2857518491895,15.1631866447373));
#54190=CARTESIAN_POINT('Ctrl Pts',(0.268786836554964,86.2877487731267,15.1656948904237));
#54191=CARTESIAN_POINT('Ctrl Pts',(0.179942946359099,86.2990746865736,15.1799208571813));
#54192=CARTESIAN_POINT('Ctrl Pts',(0.0900295736881363,86.3104029506445,
15.1878531222001));
#54193=CARTESIAN_POINT('Ctrl Pts',(-3.5632935687461E-5,86.3217050596061,
15.1894668163097));
#54194=CARTESIAN_POINT('Ctrl Pts',(-0.0504520453204218,86.3280317178972,
15.1903701248208));
#54195=CARTESIAN_POINT('Ctrl Pts',(-0.100919683814972,86.3343506980785,
15.1892943044232));
#54196=CARTESIAN_POINT('Ctrl Pts',(-0.151304027318804,86.3406620734973,
15.1862310563657));
#54197=CARTESIAN_POINT('Ctrl Pts',(-0.241739297716183,86.351990412876,15.180732807364));
#54198=CARTESIAN_POINT('Ctrl Pts',(-0.331935073873759,86.3632980542052,
15.1688279446061));
#54199=CARTESIAN_POINT('Ctrl Pts',(-0.420963465396249,86.374594132703,15.1504427296073));
#54200=CARTESIAN_POINT('Ctrl Pts',(-0.450369245384569,86.3783251896541,
15.1443701545776));
#54201=CARTESIAN_POINT('Ctrl Pts',(-0.479645316965722,86.3820546740564,
15.1375909503703));
#54202=CARTESIAN_POINT('Ctrl Pts',(-0.508751498098799,86.3857819891471,
15.1301048276641));
#54203=CARTESIAN_POINT('Ctrl Pts',(-0.508752376006733,86.3857821015713,
15.1301046018658));
#54204=CARTESIAN_POINT('Ctrl Pts',(-0.50875325391444,86.3857822139955,15.1301043760669));
#54205=CARTESIAN_POINT('Ctrl Pts',(-0.508754131822008,86.3857823264197,
15.1301041502673));
#54206=CARTESIAN_POINT('Ctrl Pts',(-0.598882470889278,86.3973240964749,
15.1069229612656));
#54207=CARTESIAN_POINT('Ctrl Pts',(-0.687411283745175,86.4088929854641,
15.076956900895));
#54208=CARTESIAN_POINT('Ctrl Pts',(-0.773434460536162,86.4205016940216,
15.0406636234198));
#54209=CARTESIAN_POINT('Ctrl Pts',(-0.859773546252864,86.432153034051,15.0042370636046));
#54210=CARTESIAN_POINT('Ctrl Pts',(-0.94358831382734,86.4438442774286,14.9614369579727));
#54211=CARTESIAN_POINT('Ctrl Pts',(-1.02396527228439,86.4555881931186,14.9127258073221));
#54212=CARTESIAN_POINT('Ctrl Pts',(-1.09166140359485,86.4654793071133,14.8716996660742));
#54213=CARTESIAN_POINT('Ctrl Pts',(-1.15691892419963,86.4754077168827,14.8264806556248));
#54214=CARTESIAN_POINT('Ctrl Pts',(-1.21919476591611,86.485382666733,14.7773424303357));
#54215=CARTESIAN_POINT('Ctrl Pts',(-1.21920363688529,86.4853840876287,14.7773354307727));
#54216=CARTESIAN_POINT('Ctrl Pts',(-1.21921250779405,86.4853855085253,14.77732843113));
#54217=CARTESIAN_POINT('Ctrl Pts',(-1.21922137864223,86.4853869294228,14.7773214314079));
#54218=CARTESIAN_POINT('Ctrl Pts',(-1.26750307732052,86.4931205018568,14.7392237807633));
#54219=CARTESIAN_POINT('Ctrl Pts',(-1.31399705510086,86.500806458136,14.6987715625188));
#54220=CARTESIAN_POINT('Ctrl Pts',(-1.3584675226408,86.5084867176979,14.6561233562593));
#54221=CARTESIAN_POINT('Ctrl Pts',(-1.37843910964283,86.5119359050018,14.6369701427018));
#54222=CARTESIAN_POINT('Ctrl Pts',(-1.39800273845863,86.5153839815182,14.617373883547));
#54223=CARTESIAN_POINT('Ctrl Pts',(-1.41713772518216,86.5188349302985,14.5973480917732));
#54224=CARTESIAN_POINT('Ctrl Pts',(-1.41713928566028,86.518835211727,14.597346458649));
#54225=CARTESIAN_POINT('Ctrl Pts',(-1.41714084613556,86.5188354931555,14.5973448255219));
#54226=CARTESIAN_POINT('Ctrl Pts',(-1.41714240660789,86.5188357745839,14.5973431923921));
#54227=CARTESIAN_POINT('Ctrl Pts',(-1.47850189589284,86.5299018509344,14.5331267307454));
#54228=CARTESIAN_POINT('Ctrl Pts',(-1.5353902446252,86.540951619425,14.4645682733434));
#54229=CARTESIAN_POINT('Ctrl Pts',(-1.58741924090239,86.5520416805986,14.3923558074855));
#54230=CARTESIAN_POINT('Ctrl Pts',(-1.64111607342621,86.5634872436525,14.3178285061199));
#54231=CARTESIAN_POINT('Ctrl Pts',(-1.68966094579571,86.5749808199838,14.2393778432421));
#54232=CARTESIAN_POINT('Ctrl Pts',(-1.73259464990787,86.5865149313903,14.1576980759503));
#54233=CARTESIAN_POINT('Ctrl Pts',(-1.77573685917616,86.59810505757,14.0756216353925));
#54234=CARTESIAN_POINT('Ctrl Pts',(-1.81320580051726,86.609735890265,13.9902799352213));
#54235=CARTESIAN_POINT('Ctrl Pts',(-1.84443755951744,86.6213704244995,13.9025484558282));
#54236=CARTESIAN_POINT('Ctrl Pts',(-1.86808029660624,86.6301778770051,13.8361348957822));
#54237=CARTESIAN_POINT('Ctrl Pts',(-1.88814605498083,86.6389868820435,13.7683531610034));
#54238=CARTESIAN_POINT('Ctrl Pts',(-1.90439634024991,86.6477722337329,13.6996719007873));
#54239=CARTESIAN_POINT('Ctrl Pts',(-1.90792712384656,86.64968107257,13.6847491678658));
#54240=CARTESIAN_POINT('Ctrl Pts',(-1.9112779747624,86.6515887945627,13.6697840129319));
#54241=CARTESIAN_POINT('Ctrl Pts',(-1.91444677126181,86.6534951408393,13.6547813008456));
#54242=CARTESIAN_POINT('Ctrl Pts',(-1.91444982625446,86.6534969787212,13.6547668369395));
#54243=CARTESIAN_POINT('Ctrl Pts',(-1.91445288107791,86.6534988166019,13.6547523729984));
#54244=CARTESIAN_POINT('Ctrl Pts',(-1.91445593573215,86.6535006544812,13.6547379090224));
#54245=CARTESIAN_POINT('Ctrl Pts',(-1.93029411741999,86.6630299384141,13.5797431434025));
#54246=CARTESIAN_POINT('Ctrl Pts',(-1.94162247145959,86.6725943602713,13.503577754203));
#54247=CARTESIAN_POINT('Ctrl Pts',(-1.9484268665014,86.6821810365732,13.426884617186));
#54248=CARTESIAN_POINT('Ctrl Pts',(-1.94934130353894,86.6834693820945,13.4165778897573));
#54249=CARTESIAN_POINT('Ctrl Pts',(-1.95017411083732,86.6847581292951,13.4062616480156));
#54250=CARTESIAN_POINT('Ctrl Pts',(-1.95092532388645,86.6860472466744,13.3959374650937));
#54251=CARTESIAN_POINT('Ctrl Pts',(-1.95727090017054,86.6969365578737,13.3087279971827));
#54252=CARTESIAN_POINT('Ctrl Pts',(-1.95779056419137,86.7078640774532,13.2209521335627));
#54253=CARTESIAN_POINT('Ctrl Pts',(-1.95253420314447,86.7188045509795,13.1334461240541));
#54254=CARTESIAN_POINT('Ctrl Pts',(-1.94728560633413,86.7297288641956,13.0460693707653));
#54255=CARTESIAN_POINT('Ctrl Pts',(-1.93628233798267,86.7406691970177,12.9589607298055));
#54256=CARTESIAN_POINT('Ctrl Pts',(-1.91955696237647,86.7516552330178,12.8728427032526));
#54257=CARTESIAN_POINT('Ctrl Pts',(-1.91139040986356,86.7570194198688,12.8307935796508));
#54258=CARTESIAN_POINT('Ctrl Pts',(-1.90185949099508,86.7623922177723,12.7889789405383));
#54259=CARTESIAN_POINT('Ctrl Pts',(-1.89096277940852,86.7677752089414,12.7474747208012));
#54260=CARTESIAN_POINT('Ctrl Pts',(-1.87592358955661,86.7752045903213,12.6901923163507));
#54261=CARTESIAN_POINT('Ctrl Pts',(-1.85828093715202,86.782653842073,12.6334969487871));
#54262=CARTESIAN_POINT('Ctrl Pts',(-1.83804155738532,86.7900899697769,12.5776275467205));
#54263=CARTESIAN_POINT('Ctrl Pts',(-1.83804050637181,86.7900903559285,12.5776246454708));
#54264=CARTESIAN_POINT('Ctrl Pts',(-1.83803945535132,86.7900907420803,12.5776217442233));
#54265=CARTESIAN_POINT('Ctrl Pts',(-1.83803840432384,86.790091128232,12.5776188429781));
#54266=CARTESIAN_POINT('Ctrl Pts',(-1.79449266735854,86.8060900075022,12.4574156503374));
#54267=CARTESIAN_POINT('Ctrl Pts',(-1.73895084814189,86.8221283598989,12.3411716114307));
#54268=CARTESIAN_POINT('Ctrl Pts',(-1.67268003308299,86.8382021014664,12.2309915644402));
#54269=CARTESIAN_POINT('Ctrl Pts',(-1.60364918014691,86.8549452800329,12.1162227538629));
#54270=CARTESIAN_POINT('Ctrl Pts',(-1.52297725085347,86.8717265116971,12.0080350920145));
#54271=CARTESIAN_POINT('Ctrl Pts',(-1.43210104189571,86.8885485525361,11.9088177404275));
#54272=CARTESIAN_POINT('Ctrl Pts',(-1.3850676727566,86.8972548714454,11.8574673773818));
#54273=CARTESIAN_POINT('Ctrl Pts',(-1.33530102994277,86.9059722716785,11.8085198265075));
#54274=CARTESIAN_POINT('Ctrl Pts',(-1.28299987689475,86.9147023588632,11.7623058938006));
#54275=CARTESIAN_POINT('Ctrl Pts',(-1.25472676418535,86.919421695332,11.7373234287492));
#54276=CARTESIAN_POINT('Ctrl Pts',(-1.22571252189455,86.9241448233599,11.7131394463543));
#54277=CARTESIAN_POINT('Ctrl Pts',(-1.19599069435505,86.9288635364696,11.6898049290109));
#54278=CARTESIAN_POINT('Ctrl Pts',(-1.19598921671075,86.9288637710642,11.6898037689168));
#54279=CARTESIAN_POINT('Ctrl Pts',(-1.19598773906459,86.9288640056588,11.6898026088248));
#54280=CARTESIAN_POINT('Ctrl Pts',(-1.1959862614168,86.9288642402533,11.6898014487349));
#54281=CARTESIAN_POINT('Ctrl Pts',(-1.12041920220244,86.9408614297019,11.6304743331618));
#54282=CARTESIAN_POINT('Ctrl Pts',(-1.04021649755475,86.9528377927844,11.5765944927885));
#54283=CARTESIAN_POINT('Ctrl Pts',(-0.956382458435333,86.9648219511491,
11.5285893231278));
#54284=CARTESIAN_POINT('Ctrl Pts',(-0.94174133505533,86.9669149141397,11.5202055017199));
#54285=CARTESIAN_POINT('Ctrl Pts',(-0.926989542819542,86.9690081125826,
11.5120007684551));
#54286=CARTESIAN_POINT('Ctrl Pts',(-0.912132536345169,86.9711016959369,
11.5039772782886));
#54287=CARTESIAN_POINT('Ctrl Pts',(-0.810786332434802,86.9853829527905,
11.4492455076661));
#54288=CARTESIAN_POINT('Ctrl Pts',(-0.70454250358182,86.9996834798607,11.402946387786));
#54289=CARTESIAN_POINT('Ctrl Pts',(-0.595002221820435,87.014080947552,11.3656916042025));
#54290=CARTESIAN_POINT('Ctrl Pts',(-0.498075757091853,87.0268205135081,
11.3327267951943));
#54291=CARTESIAN_POINT('Ctrl Pts',(-0.39857100478865,87.0396097075564,11.3068307766587));
#54292=CARTESIAN_POINT('Ctrl Pts',(-0.297506797444648,87.0524921020393,
11.2884158931856));
#54293=CARTESIAN_POINT('Ctrl Pts',(-0.286596111482307,87.0538828591069,
11.286427859876));
#54294=CARTESIAN_POINT('Ctrl Pts',(-0.275667245422533,87.0552747017216,
11.2845270685171));
#54295=CARTESIAN_POINT('Ctrl Pts',(-0.264721479711684,87.0566676841916,
11.2827140745979));
#54296=CARTESIAN_POINT('Ctrl Pts',(-0.247350619328251,87.0588783384885,
11.2798368648093));
#54297=CARTESIAN_POINT('Ctrl Pts',(-0.229936804679973,87.0610953683484,
11.2771819347456));
#54298=CARTESIAN_POINT('Ctrl Pts',(-0.212485123333405,87.0633157544152,
11.2747504305229));
#54299=CARTESIAN_POINT('Ctrl Pts',(-0.124714877192573,87.0744828063306,
11.262521595955));
#54300=CARTESIAN_POINT('Ctrl Pts',(-0.0359624166409045,87.08573690229,11.2559445350597));
#54301=CARTESIAN_POINT('Ctrl Pts',(0.0529835866622808,87.0969516821591,
11.2552698032056));
#54302=CARTESIAN_POINT('Ctrl Pts',(0.0784856186886829,87.1001671124738,
11.2550763483823));
#54303=CARTESIAN_POINT('Ctrl Pts',(0.104003647599614,87.1033793268467,11.2553677784251));
#54304=CARTESIAN_POINT('Ctrl Pts',(0.129519357546692,87.1065853867447,11.2561492489883));
#54305=CARTESIAN_POINT('Ctrl Pts',(0.157463490542975,87.1100965790404,11.2570050949512));
#54306=CARTESIAN_POINT('Ctrl Pts',(0.185402461192954,87.1136002283852,11.2584487481659));
#54307=CARTESIAN_POINT('Ctrl Pts',(0.213307864462586,87.1170923527583,11.2604858640906));
#54308=CARTESIAN_POINT('Ctrl Pts',(0.213309293345847,87.1170925315709,11.2604859684001));
#54309=CARTESIAN_POINT('Ctrl Pts',(0.21331072222907,87.1170927103835,11.2604860727113));
#54310=CARTESIAN_POINT('Ctrl Pts',(0.213312151112264,87.1170928891961,11.260486177024));
#54311=CARTESIAN_POINT('Ctrl Pts',(0.296036961065724,87.1274451948233,11.2665253327291));
#54312=CARTESIAN_POINT('Ctrl Pts',(0.378652570307991,87.1377197497415,11.2777966697319));
#54313=CARTESIAN_POINT('Ctrl Pts',(0.460461010227518,87.1480100039539,11.2941051753275));
#54314=CARTESIAN_POINT('Ctrl Pts',(0.485688943100611,87.1511832931985,11.2991343616173));
#54315=CARTESIAN_POINT('Ctrl Pts',(0.510839999722393,87.1543580568021,11.3046422105368));
#54316=CARTESIAN_POINT('Ctrl Pts',(0.535893458079764,87.157536984341,11.3106220448498));
#54317=CARTESIAN_POINT('Ctrl Pts',(0.643826829621318,87.1712321940907,11.3363839045286));
#54318=CARTESIAN_POINT('Ctrl Pts',(0.749936585598241,87.185105181435,11.3709434084497));
#54319=CARTESIAN_POINT('Ctrl Pts',(0.852883685134752,87.1990028563483,11.4136672463958));
#54320=CARTESIAN_POINT('Ctrl Pts',(0.892380207461054,87.2043348164518,11.4300586068799));
#54321=CARTESIAN_POINT('Ctrl Pts',(0.931414528729908,87.2096708258374,11.4476528139777));
#54322=CARTESIAN_POINT('Ctrl Pts',(0.969919890804015,87.2150124051974,11.4664239213957));
#54323=CARTESIAN_POINT('Ctrl Pts',(1.0577844924855,87.2272012463752,11.5092573292008));
#54324=CARTESIAN_POINT('Ctrl Pts',(1.14291873269584,87.2394221753485,11.558228356988));
#54325=CARTESIAN_POINT('Ctrl Pts',(1.22440430680299,87.2517810800493,11.6130665127217));
#54326=CARTESIAN_POINT('Ctrl Pts',(1.2355027562513,87.2534643801986,11.6205355464238));
#54327=CARTESIAN_POINT('Ctrl Pts',(1.24653344464948,87.2551502353235,11.6281134447766));
#54328=CARTESIAN_POINT('Ctrl Pts',(1.25749397836516,87.2568389085591,11.6357995444945));
#54329=CARTESIAN_POINT('Ctrl Pts',(1.32334447416327,87.266984397154,11.6819773575743));
#54330=CARTESIAN_POINT('Ctrl Pts',(1.38666333379533,87.2772155382505,11.7320570775736));
#54331=CARTESIAN_POINT('Ctrl Pts',(1.44689953367254,87.2874052651517,11.7857499483419));
#54332=CARTESIAN_POINT('Ctrl Pts',(1.46948304521282,87.2912255561981,11.805880261494));
#54333=CARTESIAN_POINT('Ctrl Pts',(1.4916337159685,87.2950400554505,11.8265182121352));
#54334=CARTESIAN_POINT('Ctrl Pts',(1.51332427436683,87.2988421751302,11.8476478780693));
#54335=CARTESIAN_POINT('Ctrl Pts',(1.53376060318231,87.3024244419645,11.8675557473303));
#54336=CARTESIAN_POINT('Ctrl Pts',(1.55378722881955,87.3059956890905,11.8878990493415));
#54337=CARTESIAN_POINT('Ctrl Pts',(1.57337921717829,87.3095523818425,11.9086622815454));
#54338=CARTESIAN_POINT('Ctrl Pts',(1.57338250129789,87.3095529780354,11.9086657619955));
#54339=CARTESIAN_POINT('Ctrl Pts',(1.57338578540575,87.3095535742279,11.9086692424579));
#54340=CARTESIAN_POINT('Ctrl Pts',(1.57338906950178,87.30955417042,11.9086727229324));
#54341=CARTESIAN_POINT('Ctrl Pts',(1.62920314855619,87.3196866123056,11.9678243058351));
#54342=CARTESIAN_POINT('Ctrl Pts',(1.6816140911376,87.329701740186,12.0305038231267));
#54343=CARTESIAN_POINT('Ctrl Pts',(1.7302587584328,87.3397655313493,12.0961918407241));
#54344=CARTESIAN_POINT('Ctrl Pts',(1.7482039264464,87.3434780949935,12.1204243533058));
#54345=CARTESIAN_POINT('Ctrl Pts',(1.76563652037205,87.3471972312119,12.145065783603));
#54346=CARTESIAN_POINT('Ctrl Pts',(1.78253833906196,87.3509310937594,12.1700882671692));
#54347=CARTESIAN_POINT('Ctrl Pts',(1.83968116910642,87.3635547928344,12.2546859990433));
#54348=CARTESIAN_POINT('Ctrl Pts',(1.8907778241375,87.3763114616047,12.3436289523395));
#54349=CARTESIAN_POINT('Ctrl Pts',(1.93547034572799,87.3890968990374,12.4359588687816));
#54350=CARTESIAN_POINT('Ctrl Pts',(1.98052972878572,87.4019872865638,12.5290466813417));
#54351=CARTESIAN_POINT('Ctrl Pts',(2.01909805218481,87.4149119224749,12.6256147479312));
#54352=CARTESIAN_POINT('Ctrl Pts',(2.0506955219477,87.4278824573006,12.7247403476088));
#54353=CARTESIAN_POINT('Ctrl Pts',(2.05330000026777,87.4289515769803,12.7329109535865));
#54354=CARTESIAN_POINT('Ctrl Pts',(2.0558570884594,87.4300210086279,12.7410989415673));
#54355=CARTESIAN_POINT('Ctrl Pts',(2.05836650191244,87.4310907588341,12.7493037971863));
#54356=CARTESIAN_POINT('Ctrl Pts',(2.08765426114887,87.4435759818033,12.8450639580521));
#54357=CARTESIAN_POINT('Ctrl Pts',(2.11039846001263,87.4561894719074,12.9431372367724));
#54358=CARTESIAN_POINT('Ctrl Pts',(2.12612571186193,87.4688913063265,13.0425177242568));
#54359=CARTESIAN_POINT('Ctrl Pts',(2.12798518732701,87.4703930785172,13.0542677477165));
#54360=CARTESIAN_POINT('Ctrl Pts',(2.12974663119914,87.4718960865658,13.0660360299565));
#54361=CARTESIAN_POINT('Ctrl Pts',(2.13140930857862,87.4734002652213,13.0778208990135));
#54362=CARTESIAN_POINT('Ctrl Pts',(2.14235788618078,87.4833051433054,13.1554231777202));
#54363=CARTESIAN_POINT('Ctrl Pts',(2.14906760410476,87.4931764870455,13.233732958017));
#54364=CARTESIAN_POINT('Ctrl Pts',(2.15137219723108,87.5029556838565,13.3122203737897));
#54365=CARTESIAN_POINT('Ctrl Pts',(2.15164317447582,87.5041055353325,13.3214490326062));
#54366=CARTESIAN_POINT('Ctrl Pts',(2.15185330697249,87.5052541144115,13.3306801610893));
#54367=CARTESIAN_POINT('Ctrl Pts',(2.1520023708274,87.5064013270745,13.3399129105828));
#54368=CARTESIAN_POINT('Ctrl Pts',(2.15325866661982,87.5160699247523,13.4177256328426));
#54369=CARTESIAN_POINT('Ctrl Pts',(2.15019300464485,87.5256315510694,13.4957652625546));
#54370=CARTESIAN_POINT('Ctrl Pts',(2.14282132818636,87.5352799618495,13.5735395986408));
#54371=CARTESIAN_POINT('Ctrl Pts',(2.13954913455313,87.5395627689563,13.6080626394718));
#54372=CARTESIAN_POINT('Ctrl Pts',(2.13542859535056,87.5438625896556,13.6425327388421));
#54373=CARTESIAN_POINT('Ctrl Pts',(2.13046187476708,87.5481959501403,13.6769036507229));
#54374=CARTESIAN_POINT('Ctrl Pts',(2.11855989613429,87.5585801791359,13.7592682315196));
#54375=CARTESIAN_POINT('Ctrl Pts',(2.10191380634633,87.5689773604948,13.8410909731399));
#54376=CARTESIAN_POINT('Ctrl Pts',(2.08066693163373,87.5793978013831,13.9219092546352));
#54377=CARTESIAN_POINT('Ctrl Pts',(2.0601672445737,87.5894517872105,13.9998854041534));
#54378=CARTESIAN_POINT('Ctrl Pts',(2.03538435874549,87.5995270017667,14.0769234410713));
#54379=CARTESIAN_POINT('Ctrl Pts',(2.00642797456428,87.6096297977829,14.1525778250149));
#54380=CARTESIAN_POINT('Ctrl Pts',(1.97126548028827,87.6218978870882,14.2444469211605));
#54381=CARTESIAN_POINT('Ctrl Pts',(1.92993666546603,87.6342186032873,14.33427543214));
#54382=CARTESIAN_POINT('Ctrl Pts',(1.88260852340114,87.6466944811642,14.421097995489));
#54383=CARTESIAN_POINT('Ctrl Pts',(1.87457850659219,87.6488112240721,14.4358289063735));
#54384=CARTESIAN_POINT('Ctrl Pts',(1.86637586239482,87.6509324217059,14.4504731900229));
#54385=CARTESIAN_POINT('Ctrl Pts',(1.85800150360941,87.653058560142,14.465026018273));
#54386=CARTESIAN_POINT('Ctrl Pts',(1.81415844388124,87.6641897305197,14.5412157940559));
#54387=CARTESIAN_POINT('Ctrl Pts',(1.7656914553528,87.6753170692972,14.6149425619963));
#54388=CARTESIAN_POINT('Ctrl Pts',(1.7128562404809,87.6863794436326,14.6855371206224));
#54389=CARTESIAN_POINT('Ctrl Pts',(1.69708168377139,87.6896822418084,14.7066139321983));
#54390=CARTESIAN_POINT('Ctrl Pts',(1.68091795671351,87.692979262648,14.7274118231789));
#54391=CARTESIAN_POINT('Ctrl Pts',(1.66437235769046,87.6962689140814,14.7479137494339));
#54392=CARTESIAN_POINT('Ctrl Pts',(1.64386945753701,87.7003453693843,14.7733192331745));
#54393=CARTESIAN_POINT('Ctrl Pts',(1.62278064909653,87.7044106310044,14.7982692560839));
#54394=CARTESIAN_POINT('Ctrl Pts',(1.60112164566226,87.708462148479,14.8227301643944));
#54395=CARTESIAN_POINT('Ctrl Pts',(1.60111834920994,87.708462765111,14.8227338872905));
#54396=CARTESIAN_POINT('Ctrl Pts',(1.60111505274426,87.7084633817426,14.8227376101755));
#54397=CARTESIAN_POINT('Ctrl Pts',(1.60111175626517,87.7084639983738,14.8227413330495));
#54398=CARTESIAN_POINT('Ctrl Pts',(1.55102800237049,87.7178325411397,14.8793033503187));
#54399=CARTESIAN_POINT('Ctrl Pts',(1.49785170670597,87.7271117866214,14.9333308644897));
#54400=CARTESIAN_POINT('Ctrl Pts',(1.44185651869029,87.7364740387544,14.9845187815763));
#54401=CARTESIAN_POINT('Ctrl Pts',(1.41746833175872,87.7405516811949,15.0068132060579));
#54402=CARTESIAN_POINT('Ctrl Pts',(1.39254582061987,87.7446449859022,15.0285684545397));
#54403=CARTESIAN_POINT('Ctrl Pts',(1.36711373179781,87.7487677953584,15.0497570945603));
#54404=CARTESIAN_POINT('Ctrl Pts',(1.28170789454909,87.7626129810955,15.1209126159878));
#54405=CARTESIAN_POINT('Ctrl Pts',(1.19066969954911,87.7765114730761,15.1858723448039));
#54406=CARTESIAN_POINT('Ctrl Pts',(1.09504508815827,87.7904557390402,15.2440257369143));
#54407=CARTESIAN_POINT('Ctrl Pts',(1.08168541959868,87.7924038857451,15.2521503194136));
#54408=CARTESIAN_POINT('Ctrl Pts',(1.06823617222237,87.7943529279763,15.2601419909981));
#54409=CARTESIAN_POINT('Ctrl Pts',(1.05470014565361,87.7963028472321,15.2679990255087));
#54410=CARTESIAN_POINT('Ctrl Pts',(0.953908641202112,87.8108222702217,15.3265038108556));
#54411=CARTESIAN_POINT('Ctrl Pts',(0.848301459582856,87.8253907966777,15.37754590955));
#54412=CARTESIAN_POINT('Ctrl Pts',(0.739103056852967,87.8400855357775,15.4202742295696));
#54413=CARTESIAN_POINT('Ctrl Pts',(0.72723775368231,87.8416822398507,15.4249170124156));
#54414=CARTESIAN_POINT('Ctrl Pts',(0.715330095557562,87.8432804291626,15.429461614958));
#54415=CARTESIAN_POINT('Ctrl Pts',(0.703381687256164,87.8448801990184,15.4339069300187));
#54416=CARTESIAN_POINT('Ctrl Pts',(0.607605843093734,87.8577036065003,15.4695396094328));
#54417=CARTESIAN_POINT('Ctrl Pts',(0.509227792878079,87.8705804910181,15.4988256786442));
#54418=CARTESIAN_POINT('Ctrl Pts',(0.409159293207726,87.8834337315559,15.5212967277769));
#54419=CARTESIAN_POINT('Ctrl Pts',(0.383995983096763,87.8866658183629,15.5269473169205));
#54420=CARTESIAN_POINT('Ctrl Pts',(0.358725697059983,87.8898964288577,15.5321672167157));
#54421=CARTESIAN_POINT('Ctrl Pts',(0.333362726689558,87.8931243749597,15.5369494596605));
#54422=CARTESIAN_POINT('Ctrl Pts',(0.274532216139257,87.9006117360391,15.5480420797249));
#54423=CARTESIAN_POINT('Ctrl Pts',(0.215205024517501,87.9080847462132,15.5567788167315));
#54424=CARTESIAN_POINT('Ctrl Pts',(0.15556690485264,87.9155339187731,15.5630710699745));
#54425=CARTESIAN_POINT('Ctrl Pts',(0.104027553548264,87.9219715047273,15.5685088445422));
#54426=CARTESIAN_POINT('Ctrl Pts',(0.0522328186884648,87.9283902497721,
15.5721275529634));
#54427=CARTESIAN_POINT('Ctrl Pts',(0.000304409078912486,87.9348303106135,
15.5739164701182));
#54428=CARTESIAN_POINT('Ctrl Pts',(-0.148983585838682,87.9533447187647,
15.5790593939458));
#54429=CARTESIAN_POINT('Ctrl Pts',(-0.299391094048801,87.9720339484778,
15.5690851092438));
#54430=CARTESIAN_POINT('Ctrl Pts',(-0.448022467706194,87.9908509514967,
15.5446043392803));
#54431=CARTESIAN_POINT('Ctrl Pts',(-0.479347198187735,87.9948167195141,
15.539444906906));
#54432=CARTESIAN_POINT('Ctrl Pts',(-0.510593150090845,87.9987881792857,
15.5336409876383));
#54433=CARTESIAN_POINT('Ctrl Pts',(-0.541733374692063,88.0027649169591,
15.5271980525233));
#54434=CARTESIAN_POINT('Ctrl Pts',(-0.696464452009511,88.0225247264113,
15.4951840801066));
#54435=CARTESIAN_POINT('Ctrl Pts',(-0.8485795645406,88.0424219689274,15.4473842006064));
#54436=CARTESIAN_POINT('Ctrl Pts',(-0.994687792787653,88.0623859643358,
15.3845062365982));
#54437=CARTESIAN_POINT('Ctrl Pts',(-1.01503446511505,88.0651661012097,15.3757500060585));
#54438=CARTESIAN_POINT('Ctrl Pts',(-1.03526472751729,88.0679475429864,15.3667013922551));
#54439=CARTESIAN_POINT('Ctrl Pts',(-1.05536950139901,88.0707301089724,15.3573623201597));
#54440=CARTESIAN_POINT('Ctrl Pts',(-1.17551588968003,88.0873587592295,15.301551904745));
#54441=CARTESIAN_POINT('Ctrl Pts',(-1.29117517789633,88.1040261432729,15.2353679457917));
#54442=CARTESIAN_POINT('Ctrl Pts',(-1.4003793554562,88.120696826086,15.1592530954929));
#54443=CARTESIAN_POINT('Ctrl Pts',(-1.41130445319503,88.1223646087952,15.1516383485348));
#54444=CARTESIAN_POINT('Ctrl Pts',(-1.42216498158317,88.1240324265296,15.1439242297858));
#54445=CARTESIAN_POINT('Ctrl Pts',(-1.43295899592136,88.1257002451571,15.136111196351));
#54446=CARTESIAN_POINT('Ctrl Pts',(-1.43911012786573,88.1266506767681,15.1316588213552));
#54447=CARTESIAN_POINT('Ctrl Pts',(-1.44523964616295,88.1276011111596,15.1271743283995));
#54448=CARTESIAN_POINT('Ctrl Pts',(-1.45134725134598,88.1285514229008,15.1226579149591));
#54449=CARTESIAN_POINT('Ctrl Pts',(-1.45135770520861,88.1285530494677,15.1226501846026));
#54450=CARTESIAN_POINT('Ctrl Pts',(-1.45136815900826,88.1285546760345,15.1226424541515));
#54451=CARTESIAN_POINT('Ctrl Pts',(-1.45137861274486,88.1285563026012,15.1226347236059));
#54452=CARTESIAN_POINT('Ctrl Pts',(-1.54677226478709,88.1433992384115,15.0520910509509));
#54453=CARTESIAN_POINT('Ctrl Pts',(-1.6369183130347,88.1582358741482,14.9736734098144));
#54454=CARTESIAN_POINT('Ctrl Pts',(-1.72086861026843,88.1730991471263,14.8885464037324));
#54455=CARTESIAN_POINT('Ctrl Pts',(-1.73266016938776,88.1751868248094,14.8765895654847));
#54456=CARTESIAN_POINT('Ctrl Pts',(-1.74432950094035,88.1772750224463,14.8645004438381));
#54457=CARTESIAN_POINT('Ctrl Pts',(-1.75587398753047,88.179363825816,14.8522823465881));
#54458=CARTESIAN_POINT('Ctrl Pts',(-1.85064134368983,88.1965105712642,14.7519853983751));
#54459=CARTESIAN_POINT('Ctrl Pts',(-1.93699614621711,88.2136998169039,14.642992568439));
#54460=CARTESIAN_POINT('Ctrl Pts',(-2.01354772692068,88.2309824128667,14.5271011040686));
#54461=CARTESIAN_POINT('Ctrl Pts',(-2.08816594384959,88.2478285247666,14.414136559782));
#54462=CARTESIAN_POINT('Ctrl Pts',(-2.15347112698357,88.2647642414885,14.2946185688211));
#54463=CARTESIAN_POINT('Ctrl Pts',(-2.20821667601837,88.2818222288054,14.1701914439778));
#54464=CARTESIAN_POINT('Ctrl Pts',(-2.24970388707577,88.2947490937744,14.0758982186718));
#54465=CARTESIAN_POINT('Ctrl Pts',(-2.28512774333354,88.3077460182186,13.9787852163484));
#54466=CARTESIAN_POINT('Ctrl Pts',(-2.31395576790492,88.3208164870905,13.8795564772651));
#54467=CARTESIAN_POINT('Ctrl Pts',(-2.33345309418025,88.3296564683225,13.8124448686634));
#54468=CARTESIAN_POINT('Ctrl Pts',(-2.34993357542916,88.3385295904087,13.7443630982527));
#54469=CARTESIAN_POINT('Ctrl Pts',(-2.36333624981357,88.3473466042889,13.6755779354622));
#54470=CARTESIAN_POINT('Ctrl Pts',(-2.36334412537992,88.3473517852681,13.6755375165057));
#54471=CARTESIAN_POINT('Ctrl Pts',(-2.36335199988244,88.3473569662362,13.6754970972799));
#54472=CARTESIAN_POINT('Ctrl Pts',(-2.36335987332104,88.3473621471933,13.675456677785));
#54473=CARTESIAN_POINT('Ctrl Pts',(-2.38166744939442,88.3594090772867,13.58147195083));
#54474=CARTESIAN_POINT('Ctrl Pts',(-2.39421984738105,88.3713961678827,13.4860287760251));
#54475=CARTESIAN_POINT('Ctrl Pts',(-2.40101479196471,88.383357134674,13.3898891010969));
#54476=CARTESIAN_POINT('Ctrl Pts',(-2.40326525750871,88.38731857149,13.3580479251796));
#54477=CARTESIAN_POINT('Ctrl Pts',(-2.40488448099111,88.3912771153413,13.3261306518563));
#54478=CARTESIAN_POINT('Ctrl Pts',(-2.40587331290976,88.3952339088243,13.2941657917042));
#54479=CARTESIAN_POINT('Ctrl Pts',(-2.40920889778045,88.4085811928567,13.1863400814845));
#54480=CARTESIAN_POINT('Ctrl Pts',(-2.40536807839736,88.421910403757,13.0779700159226));
#54481=CARTESIAN_POINT('Ctrl Pts',(-2.39438836203394,88.4352856038816,12.9700894145612));
#54482=CARTESIAN_POINT('Ctrl Pts',(-2.39209862184288,88.4380749048321,12.9475916978081));
#54483=CARTESIAN_POINT('Ctrl Pts',(-2.38949849321608,88.4408661835501,12.9251154272601));
#54484=CARTESIAN_POINT('Ctrl Pts',(-2.38658846293994,88.4436599856111,12.9026702230902));
#54485=CARTESIAN_POINT('Ctrl Pts',(-2.37149981622855,88.4581459834459,12.7862907617282));
#54486=CARTESIAN_POINT('Ctrl Pts',(-2.34807116697853,88.4727071846531,12.6707431350032));
#54487=CARTESIAN_POINT('Ctrl Pts',(-2.31637745037266,88.4874116194763,12.55728259153));
#54488=CARTESIAN_POINT('Ctrl Pts',(-2.31250278139908,88.4892092886513,12.5434116387166));
#54489=CARTESIAN_POINT('Ctrl Pts',(-2.30850457460238,88.4910090900563,12.5295719422792));
#54490=CARTESIAN_POINT('Ctrl Pts',(-2.30438296280211,88.492811140838,12.5157658491687));
#54491=CARTESIAN_POINT('Ctrl Pts',(-2.28365152169375,88.5018753398616,12.4463220926658));
#54492=CARTESIAN_POINT('Ctrl Pts',(-2.25979030090262,88.5110019937939,12.3777268029861));
#54493=CARTESIAN_POINT('Ctrl Pts',(-2.23281244892046,88.520204065096,12.3102647269031));
#54494=CARTESIAN_POINT('Ctrl Pts',(-2.20408902789713,88.5300015452095,12.2384375993868));
#54495=CARTESIAN_POINT('Ctrl Pts',(-2.17182714020991,88.5398852265671,12.1678819029796));
#54496=CARTESIAN_POINT('Ctrl Pts',(-2.13619996140862,88.5497612773889,12.0989198439989));
#54497=CARTESIAN_POINT('Ctrl Pts',(-2.10985953763744,88.5570629884023,12.0479337732854));
#54498=CARTESIAN_POINT('Ctrl Pts',(-2.08167962138334,88.5643606575904,11.9978177248025));
#54499=CARTESIAN_POINT('Ctrl Pts',(-2.0517256356387,88.5716186150092,11.9486842696441));
#54500=CARTESIAN_POINT('Ctrl Pts',(-2.05169777747856,88.5716253651406,11.948638573967));
#54501=CARTESIAN_POINT('Ctrl Pts',(-2.05166991775728,88.5716321152547,11.948592879143));
#54502=CARTESIAN_POINT('Ctrl Pts',(-2.0516420564749,88.5716388653515,11.9485471851723));
#54503=CARTESIAN_POINT('Ctrl Pts',(-1.99058740264741,88.5864308918092,11.848414336839));
#54504=CARTESIAN_POINT('Ctrl Pts',(-1.92203241919673,88.6011404162034,11.7523767411012));
#54505=CARTESIAN_POINT('Ctrl Pts',(-1.84679973993252,88.6158179381924,11.6614367274794));
#54506=CARTESIAN_POINT('Ctrl Pts',(-1.77012497813778,88.6307768033194,11.5687535484372));
#54507=CARTESIAN_POINT('Ctrl Pts',(-1.68651548947329,88.6457033916041,11.4813644561497));
#54508=CARTESIAN_POINT('Ctrl Pts',(-1.59682250097743,88.6606501759218,11.4002908092098));
#54509=CARTESIAN_POINT('Ctrl Pts',(-1.54726366564214,88.6689088507103,11.3554944925066));
#54510=CARTESIAN_POINT('Ctrl Pts',(-1.49584705316933,88.6771735858944,11.312625635855));
#54511=CARTESIAN_POINT('Ctrl Pts',(-1.44271181452407,88.6854515692555,11.2718531617868));
#54512=CARTESIAN_POINT('Ctrl Pts',(-1.44269427247012,88.6854543021468,11.2718397011727));
#54513=CARTESIAN_POINT('Ctrl Pts',(-1.44267673022984,88.6854570350394,11.2718262407881));
#54514=CARTESIAN_POINT('Ctrl Pts',(-1.4426591878032,88.6854597679333,11.2718127806328));
#54515=CARTESIAN_POINT('Ctrl Pts',(-1.36786877183948,88.6971111932671,11.2144267283396));
#54516=CARTESIAN_POINT('Ctrl Pts',(-1.2896871105259,88.7087872796394,11.161207841561));
#54517=CARTESIAN_POINT('Ctrl Pts',(-1.20855202025243,88.7205536779918,11.1125764916225));
#54518=CARTESIAN_POINT('Ctrl Pts',(-1.19943449935656,88.7218759219491,11.1071115645759));
#54519=CARTESIAN_POINT('Ctrl Pts',(-1.19027965083921,88.7231993090832,11.1017045379434));
#54520=CARTESIAN_POINT('Ctrl Pts',(-1.18108807079193,88.7245239333106,11.0963559860755));
#54521=CARTESIAN_POINT('Ctrl Pts',(2.14925682029349,84.6483054938945,12.0236057114313));
#54522=CARTESIAN_POINT('Ctrl Pts',(2.19287098933027,84.6596480578688,12.1033343061839));
#54523=CARTESIAN_POINT('Ctrl Pts',(2.231937200779,84.6709868370664,12.1854677976133));
#54524=CARTESIAN_POINT('Ctrl Pts',(2.26636389384606,84.6822750513171,12.2693676919591));
#54525=CARTESIAN_POINT('Ctrl Pts',(2.28133677449313,84.6871845290983,12.3058574907874));
#54526=CARTESIAN_POINT('Ctrl Pts',(2.29543272638349,84.6920844693855,12.3426812535786));
#54527=CARTESIAN_POINT('Ctrl Pts',(2.30864723184453,84.6969711503224,12.3797860363184));
#54528=CARTESIAN_POINT('Ctrl Pts',(2.33932749547344,84.7083166115547,12.4659326211987));
#54529=CARTESIAN_POINT('Ctrl Pts',(2.36533388486355,84.719520070483,12.553580991922));
#54530=CARTESIAN_POINT('Ctrl Pts',(2.38649618898333,84.7306901567562,12.6421726883889));
#54531=CARTESIAN_POINT('Ctrl Pts',(2.39561515887648,84.735503417158,12.6803474073746));
#54532=CARTESIAN_POINT('Ctrl Pts',(2.40383466156047,84.7403103987368,12.7186966317093));
#54533=CARTESIAN_POINT('Ctrl Pts',(2.41114129373365,84.7451194157271,12.7571727164414));
#54534=CARTESIAN_POINT('Ctrl Pts',(2.43050120968639,84.7578615604718,12.8591203373082));
#54535=CARTESIAN_POINT('Ctrl Pts',(2.44345244131896,84.7706202824875,12.9619613477901));
#54536=CARTESIAN_POINT('Ctrl Pts',(2.44983626164971,84.7834913703342,13.0648855278049));
#54537=CARTESIAN_POINT('Ctrl Pts',(2.45140607708422,84.7866564394172,13.0901951320858));
#54538=CARTESIAN_POINT('Ctrl Pts',(2.45257865729089,84.7898282702867,13.1155095460192));
#54539=CARTESIAN_POINT('Ctrl Pts',(2.45335146297043,84.793008222476,13.1408162738566));
#54540=CARTESIAN_POINT('Ctrl Pts',(2.45388624577805,84.7952087546472,13.1583285713498));
#54541=CARTESIAN_POINT('Ctrl Pts',(2.45422965394671,84.7974131765683,13.1758375459544));
#54542=CARTESIAN_POINT('Ctrl Pts',(2.45438086824742,84.7996219230911,13.1933393515316));
#54543=CARTESIAN_POINT('Ctrl Pts',(2.45507531434162,84.8097655099656,13.273715747599));
#54544=CARTESIAN_POINT('Ctrl Pts',(2.45171514020669,84.8200035295251,13.3539544503281));
#54545=CARTESIAN_POINT('Ctrl Pts',(2.44439434627238,84.8302222778438,13.4336888791006));
#54546=CARTESIAN_POINT('Ctrl Pts',(2.43991491833263,84.8364748984118,13.4824765695079));
#54547=CARTESIAN_POINT('Ctrl Pts',(2.43395257145794,84.8427204305586,13.5310764656673));
#54548=CARTESIAN_POINT('Ctrl Pts',(2.42652634875635,84.8489340469272,13.5794138375531));
#54549=CARTESIAN_POINT('Ctrl Pts',(2.42500943331347,84.8502032696537,13.5892874582116));
#54550=CARTESIAN_POINT('Ctrl Pts',(2.42343150243139,84.8514711047787,13.5991497927408));
#54551=CARTESIAN_POINT('Ctrl Pts',(2.42181229469839,84.8527210817197,13.609006013937));
#54552=CARTESIAN_POINT('Ctrl Pts',(2.42180681093135,84.8527253150137,13.6090393939782));
#54553=CARTESIAN_POINT('Ctrl Pts',(2.42180132644769,84.8527295483047,13.6090727738877));
#54554=CARTESIAN_POINT('Ctrl Pts',(2.42179584124735,84.8527337815928,13.6091061536658));
#54555=CARTESIAN_POINT('Ctrl Pts',(2.40512791559537,84.8655975105884,13.7105375735987));
#54556=CARTESIAN_POINT('Ctrl Pts',(2.3818380810386,84.8784339362426,13.810753609036));
#54557=CARTESIAN_POINT('Ctrl Pts',(2.3523566788582,84.8912395537273,13.9089464545139));
#54558=CARTESIAN_POINT('Ctrl Pts',(2.336004608446,84.8983422809823,13.9634098180066));
#54559=CARTESIAN_POINT('Ctrl Pts',(2.31774871045274,84.9054355227729,14.0172507522878));
#54560=CARTESIAN_POINT('Ctrl Pts',(2.29766920602148,84.9125186231545,14.0703323703706));
#54561=CARTESIAN_POINT('Ctrl Pts',(2.25006071059923,84.9293126507782,14.1961888615083));
#54562=CARTESIAN_POINT('Ctrl Pts',(2.19229863809479,84.9459664925921,14.3178270217157));
#54563=CARTESIAN_POINT('Ctrl Pts',(2.12535334232426,84.962551052568,14.43359904628));
#54564=CARTESIAN_POINT('Ctrl Pts',(2.11089565313255,84.9661326995046,14.458601489379));
#54565=CARTESIAN_POINT('Ctrl Pts',(2.09600980491567,84.9697110866686,14.4833302121407));
#54566=CARTESIAN_POINT('Ctrl Pts',(2.08070583222711,84.9732868808465,14.507768434203));
#54567=CARTESIAN_POINT('Ctrl Pts',(2.02343999421288,84.9866671223257,14.5992136618216));
#54568=CARTESIAN_POINT('Ctrl Pts',(1.96027162876379,85.0000545294258,14.6865616750671));
#54569=CARTESIAN_POINT('Ctrl Pts',(1.89166144165137,85.013514996597,14.7689479802724));
#54570=CARTESIAN_POINT('Ctrl Pts',(1.87257221339513,85.0172600662591,14.7918701008997));
#54571=CARTESIAN_POINT('Ctrl Pts',(1.85306176095778,85.021010755739,14.8144078274359));
#54572=CARTESIAN_POINT('Ctrl Pts',(1.83314013504474,85.0247684008789,14.8365418326155));
#54573=CARTESIAN_POINT('Ctrl Pts',(1.78384715231707,85.0340661127114,14.8913090057256));
#54574=CARTESIAN_POINT('Ctrl Pts',(1.73213235121993,85.0433032183397,14.9437255234051));
#54575=CARTESIAN_POINT('Ctrl Pts',(1.67812973885351,85.0524810305914,14.9935538779059));
#54576=CARTESIAN_POINT('Ctrl Pts',(1.67810460485974,85.0524853021454,14.993577069109));
#54577=CARTESIAN_POINT('Ctrl Pts',(1.67807947036516,85.0524895736968,14.9936002597336));
#54578=CARTESIAN_POINT('Ctrl Pts',(1.67805433536979,85.0524938452456,14.9936234497798));
#54579=CARTESIAN_POINT('Ctrl Pts',(1.58086365874157,85.0690108451512,15.08329349929));
#54580=CARTESIAN_POINT('Ctrl Pts',(1.47618206021756,85.0854886548041,15.1643111625791));
#54581=CARTESIAN_POINT('Ctrl Pts',(1.36580274476862,85.1019180544506,15.2359968338182));
#54582=CARTESIAN_POINT('Ctrl Pts',(1.28658124915673,85.1137097711025,15.2874471084136));
#54583=CARTESIAN_POINT('Ctrl Pts',(1.20442853410608,85.125476173868,15.3340897167976));
#54584=CARTESIAN_POINT('Ctrl Pts',(1.12000583506295,85.1372153841286,15.3756916061252));
#54585=CARTESIAN_POINT('Ctrl Pts',(0.996577261945724,85.1543784692754,15.4365148432035));
#54586=CARTESIAN_POINT('Ctrl Pts',(0.868290307002927,85.1714844210568,15.4865678900596));
#54587=CARTESIAN_POINT('Ctrl Pts',(0.737167175096835,85.1885334620103,15.5251526957638));
#54588=CARTESIAN_POINT('Ctrl Pts',(0.625148580642901,85.2030984710719,15.5581157255469));
#54589=CARTESIAN_POINT('Ctrl Pts',(0.511071003745848,85.2175733420559,15.5827947611205));
#54590=CARTESIAN_POINT('Ctrl Pts',(0.39611249836126,85.2320031511263,15.5986955767301));
#54591=CARTESIAN_POINT('Ctrl Pts',(0.366333917902216,85.2357410148796,15.6028144865525));
#54592=CARTESIAN_POINT('Ctrl Pts',(0.336496385881311,85.239475831078,15.6063441544405));
#54593=CARTESIAN_POINT('Ctrl Pts',(0.306620746534905,85.2432083328465,15.6092755516791));
#54594=CARTESIAN_POINT('Ctrl Pts',(0.29544148056242,85.2446050102373,15.6103724610714));
#54595=CARTESIAN_POINT('Ctrl Pts',(0.284256833063029,85.246001651423,15.6113851010353));
#54596=CARTESIAN_POINT('Ctrl Pts',(0.273067872309848,85.2473979471003,15.6123136170645));
#54597=CARTESIAN_POINT('Ctrl Pts',(0.273057256352567,85.2473992718896,15.6123144980298));
#54598=CARTESIAN_POINT('Ctrl Pts',(0.273046640391623,85.2474005966785,15.6123153789195));
#54599=CARTESIAN_POINT('Ctrl Pts',(0.273036024426925,85.247401921467,15.6123162597336));
#54600=CARTESIAN_POINT('Ctrl Pts',(0.142388609612776,85.2637056863887,15.6231561674791));
#54601=CARTESIAN_POINT('Ctrl Pts',(0.011176502177052,85.2799507951204,15.6225366570752));
#54602=CARTESIAN_POINT('Ctrl Pts',(-0.11875750278832,85.2961599142673,15.6109905900159));
#54603=CARTESIAN_POINT('Ctrl Pts',(-0.153269989257969,85.3004653076506,
15.6079237755722));
#54604=CARTESIAN_POINT('Ctrl Pts',(-0.187692105702657,85.3047681392327,
15.6040862809233));
#54605=CARTESIAN_POINT('Ctrl Pts',(-0.221988927493997,85.3090687842354,
15.5994885635788));
#54606=CARTESIAN_POINT('Ctrl Pts',(-0.363094838903275,85.3267627395658,
15.5805723765269));
#54607=CARTESIAN_POINT('Ctrl Pts',(-0.502082635392263,85.3444214525854,
15.5487840486862));
#54608=CARTESIAN_POINT('Ctrl Pts',(-0.636562216114298,85.362078928714,15.5048537957376));
#54609=CARTESIAN_POINT('Ctrl Pts',(-0.656308226545274,85.3646716249876,
15.4984033946559));
#54610=CARTESIAN_POINT('Ctrl Pts',(-0.675956961236127,85.3672642824483,
15.4916912604578));
#54611=CARTESIAN_POINT('Ctrl Pts',(-0.69550077484739,85.3698569961539,15.4847197579916));
#54612=CARTESIAN_POINT('Ctrl Pts',(-0.778857614981396,85.3809152484562,
15.4549854170833));
#54613=CARTESIAN_POINT('Ctrl Pts',(-0.860308282720603,85.3919747902219,
15.4205322578276));
#54614=CARTESIAN_POINT('Ctrl Pts',(-0.939270356083257,85.4030420703751,
15.3815429803886));
#54615=CARTESIAN_POINT('Ctrl Pts',(-1.00540509097031,85.4123114779233,15.348887486212));
#54616=CARTESIAN_POINT('Ctrl Pts',(-1.06979766462332,85.4215867848494,15.3130479343755));
#54617=CARTESIAN_POINT('Ctrl Pts',(-1.13217977256314,85.4308033614711,15.274253321012));
#54618=CARTESIAN_POINT('Ctrl Pts',(-1.14839640811455,85.4331992706355,15.2641684084137));
#54619=CARTESIAN_POINT('Ctrl Pts',(-1.16447742505608,85.4355912449487,15.2538836798832));
#54620=CARTESIAN_POINT('Ctrl Pts',(-1.18041861045527,85.4379782209009,15.2434028764948));
#54621=CARTESIAN_POINT('Ctrl Pts',(-1.18042501130412,85.4379791793411,15.2433986681479));
#54622=CARTESIAN_POINT('Ctrl Pts',(-1.18043141213124,85.4379801377805,15.2433944597689));
#54623=CARTESIAN_POINT('Ctrl Pts',(-1.18043781293661,85.4379810962193,15.2433902513577));
#54624=CARTESIAN_POINT('Ctrl Pts',(-1.24921416677233,85.4482794760413,15.198171070387));
#54625=CARTESIAN_POINT('Ctrl Pts',(-1.31548179104275,85.4584987891364,15.1492373230104));
#54626=CARTESIAN_POINT('Ctrl Pts',(-1.37885416306956,85.4686706593374,15.0969467637316));
#54627=CARTESIAN_POINT('Ctrl Pts',(-1.40593323842989,85.4730171092322,15.0746029575893));
#54628=CARTESIAN_POINT('Ctrl Pts',(-1.43248354583059,85.4773548432448,15.0516468824975));
#54629=CARTESIAN_POINT('Ctrl Pts',(-1.45847454204963,85.4816860870913,15.0281093092908));
#54630=CARTESIAN_POINT('Ctrl Pts',(-1.52224430076374,85.4923129354312,14.9703591041253));
#54631=CARTESIAN_POINT('Ctrl Pts',(-1.58264666015608,85.5029020136033,14.9091046547943));
#54632=CARTESIAN_POINT('Ctrl Pts',(-1.63925983456805,85.5134987315104,14.8447737486644));
#54633=CARTESIAN_POINT('Ctrl Pts',(-1.66132902818519,85.5176295901246,14.8196959953376));
#54634=CARTESIAN_POINT('Ctrl Pts',(-1.68282215637449,85.5217615402645,14.7941512317421));
#54635=CARTESIAN_POINT('Ctrl Pts',(-1.70371345048146,85.5258970048648,14.7681667857281));
#54636=CARTESIAN_POINT('Ctrl Pts',(-1.76028445623371,85.537095324629,14.6978041630301));
#54637=CARTESIAN_POINT('Ctrl Pts',(-1.81244692662518,85.5483211266438,14.6242103361006));
#54638=CARTESIAN_POINT('Ctrl Pts',(-1.85972127513458,85.559624746755,14.547900063256));
#54639=CARTESIAN_POINT('Ctrl Pts',(-1.89367710308096,85.5677438174935,14.4930885517925));
#54640=CARTESIAN_POINT('Ctrl Pts',(-1.92511333523625,85.5759046014839,14.4368689671084));
#54641=CARTESIAN_POINT('Ctrl Pts',(-1.95403426143239,85.5840476265648,14.379509940392));
#54642=CARTESIAN_POINT('Ctrl Pts',(-1.97873669193148,85.5910028848352,14.3305174786241));
#54643=CARTESIAN_POINT('Ctrl Pts',(-2.00160476850795,85.5979452903245,14.2806930952608));
#54644=CARTESIAN_POINT('Ctrl Pts',(-2.02265084584226,85.6048415150376,14.2301758752017));
#54645=CARTESIAN_POINT('Ctrl Pts',(-2.04252541445498,85.61135386834,14.1824706453748));
#54646=CARTESIAN_POINT('Ctrl Pts',(-2.0608382214117,85.6177998058383,14.1341696797806));
#54647=CARTESIAN_POINT('Ctrl Pts',(-2.07736330535239,85.6242383657981,14.0853321146169));
#54648=CARTESIAN_POINT('Ctrl Pts',(-2.07737361122409,85.6242423812072,14.0853016570602));
#54649=CARTESIAN_POINT('Ctrl Pts',(-2.07738391640524,85.6242463966153,14.085271199281));
#54650=CARTESIAN_POINT('Ctrl Pts',(-2.07739422089578,85.6242504120224,14.0852407412793));
#54651=CARTESIAN_POINT('Ctrl Pts',(-2.1056363322918,85.635255669621,14.0017627398374));
#54652=CARTESIAN_POINT('Ctrl Pts',(-2.12868661691511,85.6462530293967,13.9166120894235));
#54653=CARTESIAN_POINT('Ctrl Pts',(-2.14654462688974,85.6572293599512,13.830517545662));
#54654=CARTESIAN_POINT('Ctrl Pts',(-2.1554400693894,85.6626968962244,13.7876320805596));
#54655=CARTESIAN_POINT('Ctrl Pts',(-2.16304797070316,85.6681592180648,13.7445127102601));
#54656=CARTESIAN_POINT('Ctrl Pts',(-2.16937291772459,85.6736147227104,13.7012506486903));
#54657=CARTESIAN_POINT('Ctrl Pts',(-2.18348150270599,85.6857839077877,13.6047492123843));
#54658=CARTESIAN_POINT('Ctrl Pts',(-2.19120685055952,85.6979185862962,13.5075430979988));
#54659=CARTESIAN_POINT('Ctrl Pts',(-2.19272683986784,85.7099902568241,13.4105047651033));
#54660=CARTESIAN_POINT('Ctrl Pts',(-2.1932627237712,85.7142462169727,13.3762931556381));
#54661=CARTESIAN_POINT('Ctrl Pts',(-2.19302736957254,85.7184943969047,13.342101936231));
#54662=CARTESIAN_POINT('Ctrl Pts',(-2.19202867229371,85.7227337162504,13.3079677997703));
#54663=CARTESIAN_POINT('Ctrl Pts',(-2.18972666727752,85.7325053804033,13.2292883490288));
#54664=CARTESIAN_POINT('Ctrl Pts',(-2.18325512765311,85.7422675366945,13.1509103876415));
#54665=CARTESIAN_POINT('Ctrl Pts',(-2.17252809072558,85.7520617636974,13.0733018247896));
#54666=CARTESIAN_POINT('Ctrl Pts',(-2.16041077600243,85.7631253716506,12.9856348028857));
#54667=CARTESIAN_POINT('Ctrl Pts',(-2.14301603860399,85.7741841235684,12.8989044883875));
#54668=CARTESIAN_POINT('Ctrl Pts',(-2.12049810978086,85.7852055215527,12.8137492567095));
#54669=CARTESIAN_POINT('Ctrl Pts',(-2.10991922310414,85.7903833565663,12.7737434660825));
#54670=CARTESIAN_POINT('Ctrl Pts',(-2.09820942748147,85.7955530435581,12.7340845889984));
#54671=CARTESIAN_POINT('Ctrl Pts',(-2.08538332695612,85.8007117279222,12.6948351177941));
#54672=CARTESIAN_POINT('Ctrl Pts',(-2.08087301405098,85.8025257851732,12.6810329963977));
#54673=CARTESIAN_POINT('Ctrl Pts',(-2.07622196108099,85.8043392611061,12.6672831277786));
#54674=CARTESIAN_POINT('Ctrl Pts',(-2.07143054132808,85.8061521035593,12.6535889336444));
#54675=CARTESIAN_POINT('Ctrl Pts',(-2.03761720726742,85.8189454405303,12.5569481914783));
#54676=CARTESIAN_POINT('Ctrl Pts',(-1.99678759074661,85.8317154373978,12.4630196046196));
#54677=CARTESIAN_POINT('Ctrl Pts',(-1.94965472372998,85.8444511391352,12.3726400604358));
#54678=CARTESIAN_POINT('Ctrl Pts',(-1.92466095163749,85.8512046690351,12.3247132978148));
#54679=CARTESIAN_POINT('Ctrl Pts',(-1.89789554386139,85.8579485588001,12.2777842042162));
#54680=CARTESIAN_POINT('Ctrl Pts',(-1.86946983044227,85.8646811993344,12.2319746290926));
#54681=CARTESIAN_POINT('Ctrl Pts',(-1.84427599796428,85.8706483676955,12.1913734049637));
#54682=CARTESIAN_POINT('Ctrl Pts',(-1.81777343950555,85.8766078475087,12.1516435507219));
#54683=CARTESIAN_POINT('Ctrl Pts',(-1.79002936519016,85.8825606311471,12.112856091873));
#54684=CARTESIAN_POINT('Ctrl Pts',(-1.73338972844886,85.8947132623378,12.0336713422091));
#54685=CARTESIAN_POINT('Ctrl Pts',(-1.67157844640131,85.9068376065722,11.9584157437827));
#54686=CARTESIAN_POINT('Ctrl Pts',(-1.60516341445492,85.9189396249287,11.8877212899944));
#54687=CARTESIAN_POINT('Ctrl Pts',(-1.55877487549976,85.9273924545595,11.8383437270035));
#54688=CARTESIAN_POINT('Ctrl Pts',(-1.51013566687496,85.9358350725433,11.7911882303987));
#54689=CARTESIAN_POINT('Ctrl Pts',(-1.45945516253797,85.9442662349374,11.746492423482));
#54690=CARTESIAN_POINT('Ctrl Pts',(-1.40689565818163,85.9530099860579,11.7001395016024));
#54691=CARTESIAN_POINT('Ctrl Pts',(-1.35214290410151,85.9617410168069,11.6564345510999));
#54692=CARTESIAN_POINT('Ctrl Pts',(-1.29544445557113,85.9704565291059,11.6156446939042));
#54693=CARTESIAN_POINT('Ctrl Pts',(-1.26602067521519,85.9749794627351,11.5944767108291));
#54694=CARTESIAN_POINT('Ctrl Pts',(-1.23607299956117,85.9794982164894,11.5740936820641));
#54695=CARTESIAN_POINT('Ctrl Pts',(-1.20563653337144,85.9840124069116,11.5545320720605));
#54696=CARTESIAN_POINT('Ctrl Pts',(-1.14789912716765,85.9925757415794,11.517424064326));
#54697=CARTESIAN_POINT('Ctrl Pts',(-1.08838658087924,86.0011250138468,11.4832623636639));
#54698=CARTESIAN_POINT('Ctrl Pts',(-1.02745354005985,86.0096568784892,11.4521231749894));
#54699=CARTESIAN_POINT('Ctrl Pts',(-0.94386043544844,86.0213616128005,11.409403799403));
#54700=CARTESIAN_POINT('Ctrl Pts',(-0.857598536648726,86.0330332693885,
11.3723694275982));
#54701=CARTESIAN_POINT('Ctrl Pts',(-0.76944192380994,86.0446822694564,11.3411524244976));
#54702=CARTESIAN_POINT('Ctrl Pts',(-0.691317422046363,86.0550056280456,
11.3134878768789));
#54703=CARTESIAN_POINT('Ctrl Pts',(-0.611699432378367,86.0653117654048,
11.2903921933378));
#54704=CARTESIAN_POINT('Ctrl Pts',(-0.531153098320537,86.0756035528523,
11.2719893478682));
#54705=CARTESIAN_POINT('Ctrl Pts',(-0.458525437424364,86.0848835338408,
11.255395723392));
#54706=CARTESIAN_POINT('Ctrl Pts',(-0.38514209479568,86.094151937621,11.2426181124793));
#54707=CARTESIAN_POINT('Ctrl Pts',(-0.311435688106232,86.1034086958724,
11.2337551633241));
#54708=CARTESIAN_POINT('Ctrl Pts',(-0.238682851706116,86.112545695611,11.2250068778104));
#54709=CARTESIAN_POINT('Ctrl Pts',(-0.165620646191976,86.121670678586,11.2200741771137));
#54710=CARTESIAN_POINT('Ctrl Pts',(-0.0926926687191226,86.1307804095427,
11.2190476294884));
#54711=CARTESIAN_POINT('Ctrl Pts',(-0.0562286799826961,86.135335275021,
11.2185343556758));
#54712=CARTESIAN_POINT('Ctrl Pts',(-0.0197983505282224,86.1398863186216,
11.2189975242646));
#54713=CARTESIAN_POINT('Ctrl Pts',(0.0165385415952809,86.1444325963023,
11.2204469529167));
#54714=CARTESIAN_POINT('Ctrl Pts',(0.0399353092095739,86.1473598747841,
11.221380217799));
#54715=CARTESIAN_POINT('Ctrl Pts',(0.0632933654262581,86.1502851805774,
11.2227223403635));
#54716=CARTESIAN_POINT('Ctrl Pts',(0.0865968599813805,86.1532082693327,
11.2244755760557));
#54717=CARTESIAN_POINT('Ctrl Pts',(0.0994853976637726,86.1548249513064,
11.2254452436836));
#54718=CARTESIAN_POINT('Ctrl Pts',(0.11235721855426,86.1564409516198,11.2265406589319));
#54719=CARTESIAN_POINT('Ctrl Pts',(0.125209734053258,86.1580562396112,11.2277621732103));
#54720=CARTESIAN_POINT('Ctrl Pts',(0.128217964667065,86.1584343102532,11.2280480780705));
#54721=CARTESIAN_POINT('Ctrl Pts',(0.131225481812053,86.1588123851195,11.2283409236405));
#54722=CARTESIAN_POINT('Ctrl Pts',(0.134232252914399,86.1591904631379,11.2286406963865));
#54723=CARTESIAN_POINT('Ctrl Pts',(0.208296467641036,86.1685034605656,11.236024841129));
#54724=CARTESIAN_POINT('Ctrl Pts',(0.281912245284535,86.1777978241537,11.2474397120406));
#54725=CARTESIAN_POINT('Ctrl Pts',(0.354666541325209,86.1870585500772,11.2625926851528));
#54726=CARTESIAN_POINT('Ctrl Pts',(0.394190407050775,86.1920894514513,11.2708245574575));
#54727=CARTESIAN_POINT('Ctrl Pts',(0.433460589407465,86.1971104925907,11.2801588611131));
#54728=CARTESIAN_POINT('Ctrl Pts',(0.472415368569644,86.2021197389829,11.2905441633557));
#54729=CARTESIAN_POINT('Ctrl Pts',(0.534557023315216,86.2101106162652,11.3071110616995));
#54730=CARTESIAN_POINT('Ctrl Pts',(0.595835813232674,86.2180940280176,11.3265969447972));
#54731=CARTESIAN_POINT('Ctrl Pts',(0.6559314307771,86.2260751400724,11.3489557008859));
#54732=CARTESIAN_POINT('Ctrl Pts',(0.668305522587851,86.2277185047195,11.3535595191329));
#54733=CARTESIAN_POINT('Ctrl Pts',(0.680629304585579,86.2293617496992,11.3582850437761));
#54734=CARTESIAN_POINT('Ctrl Pts',(0.692899759446579,86.231004885655,11.3631317129012));
#54735=CARTESIAN_POINT('Ctrl Pts',(0.765403576032029,86.2407138678654,11.391769771822));
#54736=CARTESIAN_POINT('Ctrl Pts',(0.836055207746743,86.2504213336074,11.4246483009801));
#54737=CARTESIAN_POINT('Ctrl Pts',(0.904500120349563,86.2601222775762,11.4613903906077));
#54738=CARTESIAN_POINT('Ctrl Pts',(0.938664938422471,86.2649645802869,11.4797304944958));
#54739=CARTESIAN_POINT('Ctrl Pts',(0.972280452183966,86.2698053410186,11.499033886941));
#54740=CARTESIAN_POINT('Ctrl Pts',(1.00530510272826,86.2746444305799,11.5192577787572));
#54741=CARTESIAN_POINT('Ctrl Pts',(1.06566332829293,86.2834886985573,11.5562204173897));
#54742=CARTESIAN_POINT('Ctrl Pts',(1.12404746474599,86.2923269766047,11.596254733523));
#54743=CARTESIAN_POINT('Ctrl Pts',(1.18020954435636,86.3011525071915,11.639042249067));
#54744=CARTESIAN_POINT('Ctrl Pts',(1.21812799415023,86.3071111618706,11.6679307138678));
#54745=CARTESIAN_POINT('Ctrl Pts',(1.25503449232313,86.3130641449343,11.6980747398789));
#54746=CARTESIAN_POINT('Ctrl Pts',(1.29086261803481,86.3190111209621,11.7293852566626));
#54747=CARTESIAN_POINT('Ctrl Pts',(1.33996474078547,86.3271613979055,11.7722960371726));
#54748=CARTESIAN_POINT('Ctrl Pts',(1.38715976654319,86.3352962476721,11.8172746685806));
#54749=CARTESIAN_POINT('Ctrl Pts',(1.43210367693323,86.3434197286818,11.8642591724474));
#54750=CARTESIAN_POINT('Ctrl Pts',(1.46722021146806,86.3497669401049,11.9009701069949));
#54751=CARTESIAN_POINT('Ctrl Pts',(1.50096157546203,86.35610708799,11.9389049525626));
#54752=CARTESIAN_POINT('Ctrl Pts',(1.53315161550813,86.3624394499366,11.9780157327345));
#54753=CARTESIAN_POINT('Ctrl Pts',(1.57078773637092,86.3698431542882,12.023743481053));
#54754=CARTESIAN_POINT('Ctrl Pts',(1.60629743009283,86.377235316054,12.0710738570216));
#54755=CARTESIAN_POINT('Ctrl Pts',(1.63946452713218,86.384608410176,12.1198220306397));
#54756=CARTESIAN_POINT('Ctrl Pts',(1.63947500513543,86.3846107394514,12.119837430948));
#54757=CARTESIAN_POINT('Ctrl Pts',(1.63948548291179,86.3846130687265,12.1198528314077));
#54758=CARTESIAN_POINT('Ctrl Pts',(1.6394959604613,86.3846153980011,12.1198682320187));
#54759=CARTESIAN_POINT('Ctrl Pts',(1.67022382831318,86.3914465413803,12.1650341307656));
#54760=CARTESIAN_POINT('Ctrl Pts',(1.69899746025832,86.3982737087366,12.2114985087682));
#54761=CARTESIAN_POINT('Ctrl Pts',(1.72590647901298,86.4050960556312,12.2589798079562));
#54762=CARTESIAN_POINT('Ctrl Pts',(1.74453701810428,86.4098195277753,12.2918536265333));
#54763=CARTESIAN_POINT('Ctrl Pts',(1.76227457177008,86.4145408243226,12.3252156347984));
#54764=CARTESIAN_POINT('Ctrl Pts',(1.77915760078136,86.4192614835819,12.358984027978));
#54765=CARTESIAN_POINT('Ctrl Pts',(1.80599207024908,86.426764662465,12.4126566784926));
#54766=CARTESIAN_POINT('Ctrl Pts',(1.83037459651115,86.4342610632331,12.4675115617748));
#54767=CARTESIAN_POINT('Ctrl Pts',(1.85212092003114,86.4417461899231,12.5233549926801));
#54768=CARTESIAN_POINT('Ctrl Pts',(1.85342475374555,86.4421949720138,12.5267031700341));
#54769=CARTESIAN_POINT('Ctrl Pts',(1.85471910483101,86.4426437116355,12.5300548867865));
#54770=CARTESIAN_POINT('Ctrl Pts',(1.85600393140411,86.4430924070764,12.5334100956869));
#54771=CARTESIAN_POINT('Ctrl Pts',(1.88345940271119,86.4526805842379,12.6051075867109));
#54772=CARTESIAN_POINT('Ctrl Pts',(1.90656724760835,86.462249602248,12.6784082342829));
#54773=CARTESIAN_POINT('Ctrl Pts',(1.92532599157067,86.4717990261399,12.7527206972875));
#54774=CARTESIAN_POINT('Ctrl Pts',(1.92893798087512,86.4736377642255,12.7670295349207));
#54775=CARTESIAN_POINT('Ctrl Pts',(1.93238877781421,86.4754757953809,12.7813760310092));
#54776=CARTESIAN_POINT('Ctrl Pts',(1.93567843562627,86.477313144432,12.7957561739071));
#54777=CARTESIAN_POINT('Ctrl Pts',(1.94676872399542,86.4835073238803,12.8442353594752));
#54778=CARTESIAN_POINT('Ctrl Pts',(1.95602776336883,86.489693485882,12.8930943654376));
#54779=CARTESIAN_POINT('Ctrl Pts',(1.96346201828368,86.4958720801445,12.9421725457636));
#54780=CARTESIAN_POINT('Ctrl Pts',(1.9634626427527,86.4958725991395,12.9421766682754));
#54781=CARTESIAN_POINT('Ctrl Pts',(1.96346326720883,86.4958731181344,12.9421807907887));
#54782=CARTESIAN_POINT('Ctrl Pts',(1.96346389165207,86.4958736371292,12.9421849133036));
#54783=CARTESIAN_POINT('Ctrl Pts',(1.97980904419184,86.5094586186453,13.0500940566911));
#54784=CARTESIAN_POINT('Ctrl Pts',(1.98731687215541,86.523004321378,13.1590501095082));
#54785=CARTESIAN_POINT('Ctrl Pts',(1.98606675423098,86.5365162111106,13.2675656801686));
#54786=CARTESIAN_POINT('Ctrl Pts',(1.98592165106773,86.5380845575068,13.2801612539596));
#54787=CARTESIAN_POINT('Ctrl Pts',(1.98565855348114,86.5396524552529,13.2927509506411));
#54788=CARTESIAN_POINT('Ctrl Pts',(1.98527758153155,86.5412199183297,13.3053324891015));
#54789=CARTESIAN_POINT('Ctrl Pts',(1.98200427250365,86.5546875530095,13.4134330027269));
#54790=CARTESIAN_POINT('Ctrl Pts',(1.9700285914733,86.5681226133291,13.5209272274796));
#54791=CARTESIAN_POINT('Ctrl Pts',(1.94939563689838,86.5815289559032,13.6263512189734));
#54792=CARTESIAN_POINT('Ctrl Pts',(1.93702813098904,86.5895647910234,13.6895429365265));
#54793=CARTESIAN_POINT('Ctrl Pts',(1.92154959718462,86.5975901872483,13.7519910158248));
#54794=CARTESIAN_POINT('Ctrl Pts',(1.90310360485767,86.6056252202187,13.8134428707539));
#54795=CARTESIAN_POINT('Ctrl Pts',(1.90310313421279,86.6056254252306,13.8134444386826));
#54796=CARTESIAN_POINT('Ctrl Pts',(1.90310266356597,86.6056256302425,13.8134460066107));
#54797=CARTESIAN_POINT('Ctrl Pts',(1.90310219291721,86.6056258352544,13.8134475745382));
#54798=CARTESIAN_POINT('Ctrl Pts',(1.88322106565787,86.6142859394332,13.879679908975));
#54799=CARTESIAN_POINT('Ctrl Pts',(1.85987118572338,86.6229700370676,13.9448473259692));
#54800=CARTESIAN_POINT('Ctrl Pts',(1.83321509731142,86.6316621062262,14.0086036405804));
#54801=CARTESIAN_POINT('Ctrl Pts',(1.82023954841902,86.635893198448,14.0396386958612));
#54802=CARTESIAN_POINT('Ctrl Pts',(1.80648118824268,86.6401261010684,14.070338872207));
#54803=CARTESIAN_POINT('Ctrl Pts',(1.79196237419654,86.644358518421,14.1006616505208));
#54804=CARTESIAN_POINT('Ctrl Pts',(1.7612003388457,86.653326039584,14.1649086596403));
#54805=CARTESIAN_POINT('Ctrl Pts',(1.72702084431151,86.6622913395971,14.2274623376558));
#54806=CARTESIAN_POINT('Ctrl Pts',(1.68962141635329,86.6712349621095,14.2879479750166));
#54807=CARTESIAN_POINT('Ctrl Pts',(1.67151087394331,86.6755658800847,14.3172379337251));
#54808=CARTESIAN_POINT('Ctrl Pts',(1.65264573837256,86.6798916154611,14.3460423212767));
#54809=CARTESIAN_POINT('Ctrl Pts',(1.63305141385878,86.6842094013902,14.3743153998403));
#54810=CARTESIAN_POINT('Ctrl Pts',(1.59149760888243,86.6933661566691,14.4342742921148));
#54811=CARTESIAN_POINT('Ctrl Pts',(1.54666032422409,86.7024876153277,14.4918478973936));
#54812=CARTESIAN_POINT('Ctrl Pts',(1.49877179469734,86.7115535415646,14.5466349552409));
#54813=CARTESIAN_POINT('Ctrl Pts',(1.48613823530509,86.7139452399252,14.5610884278382));
#54814=CARTESIAN_POINT('Ctrl Pts',(1.47329245360296,86.716333037697,14.5753477214595));
#54815=CARTESIAN_POINT('Ctrl Pts',(1.46023903547238,86.7187164865721,14.5894049591195));
#54816=CARTESIAN_POINT('Ctrl Pts',(1.41325526961805,86.7272953432941,14.6400018185911));
#54817=CARTESIAN_POINT('Ctrl Pts',(1.36357366042792,86.7358192158463,14.6879893655017));
#54818=CARTESIAN_POINT('Ctrl Pts',(1.31157081868928,86.7443078715575,14.7331579898203));
#54819=CARTESIAN_POINT('Ctrl Pts',(1.28411715180015,86.7487892560057,14.7570036937169));
#54820=CARTESIAN_POINT('Ctrl Pts',(1.2560159093463,86.7532609375692,14.7800643605444));
#54821=CARTESIAN_POINT('Ctrl Pts',(1.2273178425336,86.7577265764004,14.8023126050758));
#54822=CARTESIAN_POINT('Ctrl Pts',(1.17439232635883,86.7659621917724,14.8433432373304));
#54823=CARTESIAN_POINT('Ctrl Pts',(1.11944030892327,86.7741773740838,14.8816097757969));
#54824=CARTESIAN_POINT('Ctrl Pts',(1.06281422527155,86.7823917988784,14.9169269152696));
#54825=CARTESIAN_POINT('Ctrl Pts',(1.03305716092283,86.7867084874331,14.9354861078559));
#54826=CARTESIAN_POINT('Ctrl Pts',(1.00283730149674,86.7910250727261,14.9532315306584));
#54827=CARTESIAN_POINT('Ctrl Pts',(0.972201963296686,86.7953451119987,14.9701405604313));
#54828=CARTESIAN_POINT('Ctrl Pts',(0.910907554326699,86.8039885371901,15.0039717190566));
#54829=CARTESIAN_POINT('Ctrl Pts',(0.848021729394301,86.8126752636963,15.0345737226639));
#54830=CARTESIAN_POINT('Ctrl Pts',(0.783848924808002,86.8213883418196,15.0615990991142));
#54831=CARTESIAN_POINT('Ctrl Pts',(0.783848520579898,86.8213883967038,15.0615992693486));
#54832=CARTESIAN_POINT('Ctrl Pts',(0.783848116351681,86.821388451588,15.0615994395828));
#54833=CARTESIAN_POINT('Ctrl Pts',(0.783847712123454,86.8213885064722,15.0615996098169));
#54834=CARTESIAN_POINT('Ctrl Pts',(0.721414990646742,86.8298653217929,15.087892123917));
#54835=CARTESIAN_POINT('Ctrl Pts',(0.657516237819578,86.8383405656427,15.1106698963487));
#54836=CARTESIAN_POINT('Ctrl Pts',(0.592633671262873,86.8468293039448,15.1300234260879));
#54837=CARTESIAN_POINT('Ctrl Pts',(0.577895031346258,86.8487575947603,15.1344197488766));
#54838=CARTESIAN_POINT('Ctrl Pts',(0.563105513678014,86.8506866034954,15.1386395573276));
#54839=CARTESIAN_POINT('Ctrl Pts',(0.548270556918788,86.8526165447307,15.1426842140146));
#54840=CARTESIAN_POINT('Ctrl Pts',(0.461094783647308,86.8639576037097,15.1664521346111));
#54841=CARTESIAN_POINT('Ctrl Pts',(0.37226458310481,86.8752806243441,15.1839658043471));
#54842=CARTESIAN_POINT('Ctrl Pts',(0.282698134797612,86.8865587791263,15.195203053839));
#54843=CARTESIAN_POINT('Ctrl Pts',(0.272753347866309,86.8878110208799,15.1964507537758));
#54844=CARTESIAN_POINT('Ctrl Pts',(0.262799536699278,86.8890627025563,15.197621073035));
#54845=CARTESIAN_POINT('Ctrl Pts',(0.252837997486953,86.8903137822262,15.1987139805477));
#54846=CARTESIAN_POINT('Ctrl Pts',(0.151596656409499,86.9030287834805,15.2098214429493));
#54847=CARTESIAN_POINT('Ctrl Pts',(0.0495542348767872,86.9156819229246,
15.2129326990221));
#54848=CARTESIAN_POINT('Ctrl Pts',(-0.0519316765197526,86.9282562131738,
15.2081145534845));
#54849=CARTESIAN_POINT('Ctrl Pts',(-0.12577716399082,86.9374058042872,15.2046086648243));
#54850=CARTESIAN_POINT('Ctrl Pts',(-0.199325178028885,86.9465381530459,
15.1969949063302));
#54851=CARTESIAN_POINT('Ctrl Pts',(-0.272112643727955,86.9556902110132,
15.185419349973));
#54852=CARTESIAN_POINT('Ctrl Pts',(-0.297826380840842,86.9589233722498,
15.1813300358275));
#54853=CARTESIAN_POINT('Ctrl Pts',(-0.323445645008111,86.9621590502286,
15.1767461231077));
#54854=CARTESIAN_POINT('Ctrl Pts',(-0.348951420595469,86.9653990604897,
15.171673402345));
#54855=CARTESIAN_POINT('Ctrl Pts',(-0.414296657323316,86.9736998955998,
15.1586772031915));
#54856=CARTESIAN_POINT('Ctrl Pts',(-0.478875702308195,86.9819941913341,
15.1423604742402));
#54857=CARTESIAN_POINT('Ctrl Pts',(-0.54233299428946,86.990285143946,15.122737145446));
#54858=CARTESIAN_POINT('Ctrl Pts',(-0.601424607188846,86.9980057028764,
15.1044638452042));
#54859=CARTESIAN_POINT('Ctrl Pts',(-0.659541456820396,87.005723176856,15.0833220070137));
#54860=CARTESIAN_POINT('Ctrl Pts',(-0.716346504498371,87.0134336695245,
15.0593409104506));
#54861=CARTESIAN_POINT('Ctrl Pts',(-0.756521593973039,87.018886877391,15.0423803983218));
#54862=CARTESIAN_POINT('Ctrl Pts',(-0.796044236638958,87.0243371173727,
15.0239979434333));
#54863=CARTESIAN_POINT('Ctrl Pts',(-0.834781273075395,87.0297808148747,
15.0042158688955));
#54864=CARTESIAN_POINT('Ctrl Pts',(-0.842694572762417,87.0308928671559,
15.0001747367221));
#54865=CARTESIAN_POINT('Ctrl Pts',(-0.850575023390869,87.0320046354225,
14.9960752616351));
#54866=CARTESIAN_POINT('Ctrl Pts',(-0.858421481083709,87.0331160844941,
14.9919176945264));
#54867=CARTESIAN_POINT('Ctrl Pts',(-0.871869504001222,87.0350209940943,
14.9847920513447));
#54868=CARTESIAN_POINT('Ctrl Pts',(-0.885226167153093,87.0369261692669,
14.9774912591352));
#54869=CARTESIAN_POINT('Ctrl Pts',(-0.898487724760393,87.0388314679397,
14.9700193179692));
#54870=CARTESIAN_POINT('Ctrl Pts',(-0.957724092911548,87.047342004708,14.9366438525206));
#54871=CARTESIAN_POINT('Ctrl Pts',(-1.01506075333272,87.0558549640507,14.8998503526552));
#54872=CARTESIAN_POINT('Ctrl Pts',(-1.07017472155257,87.0643573017716,14.8600243674868));
#54873=CARTESIAN_POINT('Ctrl Pts',(-1.11798186153755,87.0717324275837,14.825478380154));
#54874=CARTESIAN_POINT('Ctrl Pts',(-1.16411199520861,87.0790986962611,14.7886568310092));
#54875=CARTESIAN_POINT('Ctrl Pts',(-1.20840348567075,87.0864532140857,14.7498029301005));
#54876=CARTESIAN_POINT('Ctrl Pts',(-1.26404616884484,87.0956925758896,14.7009914027443));
#54877=CARTESIAN_POINT('Ctrl Pts',(-1.31678836032053,87.1049133973009,14.6489741308252));
#54878=CARTESIAN_POINT('Ctrl Pts',(-1.36637013897849,87.1141192370507,14.594182850602));
#54879=CARTESIAN_POINT('Ctrl Pts',(-1.41492233008917,87.1231339134694,14.5405293355286));
#54880=CARTESIAN_POINT('Ctrl Pts',(-1.46044816149065,87.1321347906823,14.4842129136124));
#54881=CARTESIAN_POINT('Ctrl Pts',(-1.5027129202905,87.1411293042985,14.4255986400942));
#54882=CARTESIAN_POINT('Ctrl Pts',(-1.54108354214404,87.1492950927834,14.3723848944524));
#54883=CARTESIAN_POINT('Ctrl Pts',(-1.57676605792366,87.1574556736497,14.3172762698622));
#54884=CARTESIAN_POINT('Ctrl Pts',(-1.60956384536974,87.1656148278677,14.2605489621672));
#54885=CARTESIAN_POINT('Ctrl Pts',(-1.65172019680466,87.1761021259267,14.1876350095697));
#54886=CARTESIAN_POINT('Ctrl Pts',(-1.6891043370142,87.1865858576639,14.112054063435));
#54887=CARTESIAN_POINT('Ctrl Pts',(-1.7212562882911,87.1970656158005,14.0344520515893));
#54888=CARTESIAN_POINT('Ctrl Pts',(-1.74400080531818,87.2044790705961,13.979555841261));
#54889=CARTESIAN_POINT('Ctrl Pts',(-1.76412704221989,87.2118908720056,13.923645613687));
#54890=CARTESIAN_POINT('Ctrl Pts',(-1.78146519609074,87.2192969185211,13.8669827924128));
#54891=CARTESIAN_POINT('Ctrl Pts',(-1.79082264284032,87.2232939810924,13.8364017203618));
#54892=CARTESIAN_POINT('Ctrl Pts',(-1.79936815660371,87.2272893570071,13.8056016005041));
#54893=CARTESIAN_POINT('Ctrl Pts',(-1.80707658092626,87.2312823862284,13.7746241054396));
#54894=CARTESIAN_POINT('Ctrl Pts',(-1.81228345944445,87.2339795934922,13.7536994589944));
#54895=CARTESIAN_POINT('Ctrl Pts',(-1.81710844901457,87.2366757471703,13.7326937530584));
#54896=CARTESIAN_POINT('Ctrl Pts',(-1.82154402001871,87.2393705891091,13.7116203057941));
#54897=CARTESIAN_POINT('Ctrl Pts',(-1.8227088833876,87.2400783046787,13.7060860269489));
#54898=CARTESIAN_POINT('Ctrl Pts',(-1.82384688503378,87.2407859262489,13.7005471038925));
#54899=CARTESIAN_POINT('Ctrl Pts',(-1.82495789188927,87.2414934483205,13.6950037848465));
#54900=CARTESIAN_POINT('Ctrl Pts',(-1.82849882850422,87.2437484216329,13.6773364398777));
#54901=CARTESIAN_POINT('Ctrl Pts',(-1.83176749276105,87.2460036280045,13.6596146915391));
#54902=CARTESIAN_POINT('Ctrl Pts',(-1.83476522961432,87.2482588636572,13.6418473814649));
#54903=CARTESIAN_POINT('Ctrl Pts',(-1.85052148869291,87.2601124982372,13.5484614859171));
#54904=CARTESIAN_POINT('Ctrl Pts',(-1.858995252252,87.2720661047975,13.4538717853143));
#54905=CARTESIAN_POINT('Ctrl Pts',(-1.86049494309029,87.2841335328508,13.3591675845272));
#54906=CARTESIAN_POINT('Ctrl Pts',(-1.86066832354394,87.2855286578305,13.3482187563581));
#54907=CARTESIAN_POINT('Ctrl Pts',(-1.86074854517825,87.2869253067998,13.3372683859944));
#54908=CARTESIAN_POINT('Ctrl Pts',(-1.86073612666572,87.2883235032261,13.3263181449444));
#54909=CARTESIAN_POINT('Ctrl Pts',(-1.86064011634269,87.299133275347,13.2416593601076));
#54910=CARTESIAN_POINT('Ctrl Pts',(-1.85481726974304,87.3099420578236,13.1569945172455));
#54911=CARTESIAN_POINT('Ctrl Pts',(-1.84339274582698,87.3206951048813,13.073114438799));
#54912=CARTESIAN_POINT('Ctrl Pts',(-1.84013719955878,87.323759306285,13.0492118693467));
#54913=CARTESIAN_POINT('Ctrl Pts',(-1.83642689728324,87.3268189405755,13.0253733261439));
#54914=CARTESIAN_POINT('Ctrl Pts',(-1.83226506783929,87.329872642938,13.001617801452));
#54915=CARTESIAN_POINT('Ctrl Pts',(-1.81700736138336,87.3410678384354,12.9145275380628));
#54916=CARTESIAN_POINT('Ctrl Pts',(-1.79567938969836,87.352182746695,12.8285491371846));
#54917=CARTESIAN_POINT('Ctrl Pts',(-1.76844235872489,87.3631643408786,12.7445658358575));
#54918=CARTESIAN_POINT('Ctrl Pts',(-1.76198621289887,87.3657673695831,12.7246588041092));
#54919=CARTESIAN_POINT('Ctrl Pts',(-1.75519805973124,87.3683628785936,12.7048640974078));
#54920=CARTESIAN_POINT('Ctrl Pts',(-1.74808007397611,87.3709501072558,12.6851939066978));
#54921=CARTESIAN_POINT('Ctrl Pts',(-1.74048231479114,87.373711722832,12.6641978865766));
#54922=CARTESIAN_POINT('Ctrl Pts',(-1.73250877200948,87.3764640732795,12.6433431848717));
#54923=CARTESIAN_POINT('Ctrl Pts',(-1.72416207515673,87.3792064987491,12.6226439922819));
#54924=CARTESIAN_POINT('Ctrl Pts',(-1.69900946105979,87.3874707463603,12.5602673644356));
#54925=CARTESIAN_POINT('Ctrl Pts',(-1.67046335546784,87.3956456577967,12.4992940896072));
#54926=CARTESIAN_POINT('Ctrl Pts',(-1.63875379046976,87.4037990054521,12.4400890054315));
#54927=CARTESIAN_POINT('Ctrl Pts',(-1.61934357112186,87.4087898738673,12.4038480897826));
#54928=CARTESIAN_POINT('Ctrl Pts',(-1.59874775495104,87.4137727941147,12.3682687028105));
#54929=CARTESIAN_POINT('Ctrl Pts',(-1.57701513166543,87.4187645446387,12.3334258341915));
#54930=CARTESIAN_POINT('Ctrl Pts',(-1.54481145156513,87.426161384629,12.2817952242997));
#54931=CARTESIAN_POINT('Ctrl Pts',(-1.51011578198423,87.4335774190229,12.2317891981794));
#54932=CARTESIAN_POINT('Ctrl Pts',(-1.473138259013,87.4410791254027,12.1836603400649));
#54933=CARTESIAN_POINT('Ctrl Pts',(-1.46272989641304,87.4431906913986,12.1701131209294));
#54934=CARTESIAN_POINT('Ctrl Pts',(-1.45214068606608,87.4453090801691,12.1567143190081));
#54935=CARTESIAN_POINT('Ctrl Pts',(-1.44137514837776,87.4474358559827,12.1434688465559));
#54936=CARTESIAN_POINT('Ctrl Pts',(-1.44137425478021,87.4474360325166,12.1434677471104));
#54937=CARTESIAN_POINT('Ctrl Pts',(-1.44137336118143,87.4474362090505,12.143466647666));
#54938=CARTESIAN_POINT('Ctrl Pts',(-1.44137246758145,87.4474363855844,12.1434655482226));
#54939=CARTESIAN_POINT('Ctrl Pts',(-1.39101091584534,87.4573854946928,12.0815030647946));
#54940=CARTESIAN_POINT('Ctrl Pts',(-1.33647766114576,87.467392088894,12.0229029464975));
#54941=CARTESIAN_POINT('Ctrl Pts',(-1.27841784629724,87.4774419721174,11.9680691834789));
#54942=CARTESIAN_POINT('Ctrl Pts',(-1.26329237318812,87.4800601209841,11.9537841463981));
#54943=CARTESIAN_POINT('Ctrl Pts',(-1.24792777761632,87.4826812052219,11.9397545561443));
#54944=CARTESIAN_POINT('Ctrl Pts',(-1.23233589478026,87.4853049682812,11.9259871749623));
#54945=CARTESIAN_POINT('Ctrl Pts',(-1.18930223958667,87.4925465641801,11.8879891511871));
#54946=CARTESIAN_POINT('Ctrl Pts',(-1.14449165882802,87.4997752125975,11.8520203055084));
#54947=CARTESIAN_POINT('Ctrl Pts',(-1.09807718852408,87.5069390398801,11.8182605077424));
#54948=CARTESIAN_POINT('Ctrl Pts',(-1.04481898304741,87.5151591613837,11.779522884874));
#54949=CARTESIAN_POINT('Ctrl Pts',(-0.989444610882565,87.5232931326331,
11.7436921266958));
#54950=CARTESIAN_POINT('Ctrl Pts',(-0.932350031533391,87.5314234278476,
11.7108513383722));
#54951=CARTESIAN_POINT('Ctrl Pts',(-0.902344114133361,87.5356962847357,
11.6935919418933));
#54952=CARTESIAN_POINT('Ctrl Pts',(-0.871862264367964,87.5399682327544,
11.6771580391405));
#54953=CARTESIAN_POINT('Ctrl Pts',(-0.840956431741857,87.5442519439667,
11.6615602120205));
#54954=CARTESIAN_POINT('Ctrl Pts',(-0.765170396769674,87.5547562876508,
11.6233118501041));
#54955=CARTESIAN_POINT('Ctrl Pts',(-0.686821867297662,87.5653245554962,
11.5901000346244));
#54956=CARTESIAN_POINT('Ctrl Pts',(-0.60662585798347,87.5759007361351,11.5624241040996));
#54957=CARTESIAN_POINT('Ctrl Pts',(-0.591470758289319,87.5778993776303,
11.5571940248249));
#54958=CARTESIAN_POINT('Ctrl Pts',(-0.576249829363261,87.5798982871302,
11.5521616209458));
#54959=CARTESIAN_POINT('Ctrl Pts',(-0.560968099442974,87.5818970663421,
11.5473302197285));
#54960=CARTESIAN_POINT('Ctrl Pts',(-0.512918338158728,87.5881817516815,
11.5321390289164));
#54961=CARTESIAN_POINT('Ctrl Pts',(-0.464270820839121,87.5944646868323,
11.5189370519895));
#54962=CARTESIAN_POINT('Ctrl Pts',(-0.415211156722598,87.6007417399278,
11.5078130698807));
#54963=CARTESIAN_POINT('Ctrl Pts',(-0.415204728478864,87.6007425624044,
11.5078116123153));
#54964=CARTESIAN_POINT('Ctrl Pts',(-0.415198300228143,87.6007433848809,
11.5078101547856));
#54965=CARTESIAN_POINT('Ctrl Pts',(-0.415191871970263,87.6007442073574,
11.5078086972915));
#54966=CARTESIAN_POINT('Ctrl Pts',(-0.342013499774578,87.6101071618813,
11.4912167924111));
#54967=CARTESIAN_POINT('Ctrl Pts',(-0.267776092093042,87.6194751514263,
11.4792174936022));
#54968=CARTESIAN_POINT('Ctrl Pts',(-0.193127907198049,87.6288868543772,
11.4717089230663));
#54969=CARTESIAN_POINT('Ctrl Pts',(-0.165660691881416,87.6323499428878,
11.4689461027255));
#54970=CARTESIAN_POINT('Ctrl Pts',(-0.138137640107208,87.6358189881235,
11.4667908242157));
#54971=CARTESIAN_POINT('Ctrl Pts',(-0.110590144787841,87.639296049334,11.4652365025014));
#54972=CARTESIAN_POINT('Ctrl Pts',(-0.0476869054798448,87.6472357335367,
11.4616872915976));
#54973=CARTESIAN_POINT('Ctrl Pts',(0.0153469194529463,87.6552271176462,
11.461258093696));
#54974=CARTESIAN_POINT('Ctrl Pts',(0.0782235425313569,87.6631729756329,
11.46403749939));
#54975=CARTESIAN_POINT('Ctrl Pts',(0.117717443844533,87.6681639073308,11.4657832924815));
#54976=CARTESIAN_POINT('Ctrl Pts',(0.157148304694915,87.6731367448581,11.4687952727436));
#54977=CARTESIAN_POINT('Ctrl Pts',(0.19643443378675,87.6780660744701,11.473096436831));
#54978=CARTESIAN_POINT('Ctrl Pts',(0.258913712979031,87.6859055070682,11.4799368570527));
#54979=CARTESIAN_POINT('Ctrl Pts',(0.321042510094577,87.6936371567403,11.4900390146791));
#54980=CARTESIAN_POINT('Ctrl Pts',(0.382499517997052,87.701366890297,11.5032417822576));
#54981=CARTESIAN_POINT('Ctrl Pts',(0.420344625002122,87.7061268453219,11.5113720210834));
#54982=CARTESIAN_POINT('Ctrl Pts',(0.45793601954607,87.7108862059206,11.5206781857904));
#54983=CARTESIAN_POINT('Ctrl Pts',(0.495207915089243,87.7156709452667,11.5311257413606));
#54984=CARTESIAN_POINT('Ctrl Pts',(0.564662168559991,87.724587060063,11.5505942218914));
#54985=CARTESIAN_POINT('Ctrl Pts',(0.633005826499264,87.7335729138838,11.574053893625));
#54986=CARTESIAN_POINT('Ctrl Pts',(0.699650543610617,87.7425720167499,11.6014808758488));
#54987=CARTESIAN_POINT('Ctrl Pts',(0.726842547412994,87.7462437802439,11.6126714793541));
#54988=CARTESIAN_POINT('Ctrl Pts',(0.753751596036412,87.7499177120451,11.6245219608091));
#54989=CARTESIAN_POINT('Ctrl Pts',(0.780337490612665,87.7535898219369,11.6370282006477));
#54990=CARTESIAN_POINT('Ctrl Pts',(0.780342623922537,87.7535905309625,11.637030615402));
#54991=CARTESIAN_POINT('Ctrl Pts',(0.780347757220298,87.7535912399879,11.6370330301808));
#54992=CARTESIAN_POINT('Ctrl Pts',(0.780352890506075,87.7535919490133,11.637035444984));
#54993=CARTESIAN_POINT('Ctrl Pts',(0.845149084363128,87.7625418007781,11.6675169075431));
#54994=CARTESIAN_POINT('Ctrl Pts',(0.908191355610745,87.7715038926297,11.7019756421812));
#54995=CARTESIAN_POINT('Ctrl Pts',(0.969038721500143,87.7804952283994,11.7399995261093));
#54996=CARTESIAN_POINT('Ctrl Pts',(0.988865924246788,87.783425068248,11.7523896640362));
#54997=CARTESIAN_POINT('Ctrl Pts',(1.00846034970323,87.7863580284901,11.7651580339999));
#54998=CARTESIAN_POINT('Ctrl Pts',(1.02780758733243,87.7892947413097,11.7782895534611));
#54999=CARTESIAN_POINT('Ctrl Pts',(1.07935239418913,87.7971187158729,11.8132744772697));
#55000=CARTESIAN_POINT('Ctrl Pts',(1.12919874277126,87.805067212262,11.8507433490639));
#55001=CARTESIAN_POINT('Ctrl Pts',(1.1770597969767,87.8130203292175,11.8905859275645));
#55002=CARTESIAN_POINT('Ctrl Pts',(1.2030573924211,87.81734037441,11.9122279756664));
#55003=CARTESIAN_POINT('Ctrl Pts',(1.22846846239111,87.8216616649534,11.9345698767102));
#55004=CARTESIAN_POINT('Ctrl Pts',(1.25324230398937,87.8259641561577,11.9575896824997));
#55005=CARTESIAN_POINT('Ctrl Pts',(1.29843034189763,87.833811995778,11.9995783200927));
#55006=CARTESIAN_POINT('Ctrl Pts',(1.34150266569588,87.8415978526089,12.0438253121523));
#55007=CARTESIAN_POINT('Ctrl Pts',(1.38221287964598,87.849273068026,12.0901586822617));
#55008=CARTESIAN_POINT('Ctrl Pts',(1.42907158746814,87.8581074769324,12.1434898156975));
#55009=CARTESIAN_POINT('Ctrl Pts',(1.47280826837788,87.8667962940535,12.1995957113147));
#55010=CARTESIAN_POINT('Ctrl Pts',(1.51315182483763,87.875451535543,12.2580557607923));
#55011=CARTESIAN_POINT('Ctrl Pts',(1.52746736513253,87.8785227684529,12.2787997721631));
#55012=CARTESIAN_POINT('Ctrl Pts',(1.54135593784631,87.8815898355959,12.2998405968929));
#55013=CARTESIAN_POINT('Ctrl Pts',(1.554806184572,87.8846579438377,12.3211608065961));
#55014=CARTESIAN_POINT('Ctrl Pts',(1.58625856364909,87.8918324816316,12.3710164955856));
#55015=CARTESIAN_POINT('Ctrl Pts',(1.61530778467838,87.8990122165708,12.4223904699846));
#55016=CARTESIAN_POINT('Ctrl Pts',(1.64187713257101,87.9063567629279,12.4749710935669));
#55017=CARTESIAN_POINT('Ctrl Pts',(1.64187731304286,87.9063568128156,12.4749714507199));
#55018=CARTESIAN_POINT('Ctrl Pts',(1.64187749351458,87.9063568627034,12.4749718078729));
#55019=CARTESIAN_POINT('Ctrl Pts',(1.6418776739862,87.9063569125911,12.4749721650261));
#55020=CARTESIAN_POINT('Ctrl Pts',(1.67730216625862,87.9161492934952,12.5450771977862));
#55021=CARTESIAN_POINT('Ctrl Pts',(1.70814817108906,87.925967252164,12.6176216607258));
#55022=CARTESIAN_POINT('Ctrl Pts',(1.73428736600347,87.9358261368229,12.6918722517605));
#55023=CARTESIAN_POINT('Ctrl Pts',(1.74642716092138,87.9404048867909,12.7263563646281));
#55024=CARTESIAN_POINT('Ctrl Pts',(1.75755245209159,87.9449924866275,12.7612082692873));
#55025=CARTESIAN_POINT('Ctrl Pts',(1.76765412568267,87.9495905875376,12.7963539180686));
#55026=CARTESIAN_POINT('Ctrl Pts',(1.79008450091673,87.9598004926438,12.8743934709112));
#55027=CARTESIAN_POINT('Ctrl Pts',(1.80750655283606,87.9701045834727,12.9538701551679));
#55028=CARTESIAN_POINT('Ctrl Pts',(1.81973107546707,87.980385882292,13.0341223380985));
#55029=CARTESIAN_POINT('Ctrl Pts',(1.82497045288055,87.9847924024026,13.0685180758562));
#55030=CARTESIAN_POINT('Ctrl Pts',(1.8292549235937,87.9891946458021,13.1030556274193));
#55031=CARTESIAN_POINT('Ctrl Pts',(1.83256928930156,87.9935830047605,13.1376800255061));
#55032=CARTESIAN_POINT('Ctrl Pts',(1.83925384484729,88.0024336361624,13.2075120032204));
#55033=CARTESIAN_POINT('Ctrl Pts',(1.8419944645236,88.0112285812271,13.2777043565843));
#55034=CARTESIAN_POINT('Ctrl Pts',(1.84068559032576,88.0199224757906,13.3478415445535));
#55035=CARTESIAN_POINT('Ctrl Pts',(1.83932265563101,88.028975454719,13.4208756123289));
#55036=CARTESIAN_POINT('Ctrl Pts',(1.83356649796163,88.0379217844587,13.4938703271618));
#55037=CARTESIAN_POINT('Ctrl Pts',(1.82344883881245,88.0468916383222,13.5662803970993));
#55038=CARTESIAN_POINT('Ctrl Pts',(1.81869376825403,88.0511072664029,13.6003114893328));
#55039=CARTESIAN_POINT('Ctrl Pts',(1.81297541791176,88.0553281874975,13.6342141987128));
#55040=CARTESIAN_POINT('Ctrl Pts',(1.80629704617942,88.0595684223687,13.6679358503882));
#55041=CARTESIAN_POINT('Ctrl Pts',(1.80629558330172,88.0595693511796,13.6679432370168));
#55042=CARTESIAN_POINT('Ctrl Pts',(1.806294120378,88.0595702799918,13.6679506236375));
#55043=CARTESIAN_POINT('Ctrl Pts',(1.80629265740831,88.0595712088052,13.6679580102498));
#55044=CARTESIAN_POINT('Ctrl Pts',(1.79016685367163,88.0698091938604,13.7493780568618));
#55045=CARTESIAN_POINT('Ctrl Pts',(1.76844788885588,88.0801916177454,13.8298081726634));
#55046=CARTESIAN_POINT('Ctrl Pts',(1.74145615672971,88.0906541470781,13.9085141050726));
#55047=CARTESIAN_POINT('Ctrl Pts',(1.72776654791466,88.0959605102678,13.9484320110843));
#55048=CARTESIAN_POINT('Ctrl Pts',(1.71272141550676,88.1012874255911,13.9879060619226));
#55049=CARTESIAN_POINT('Ctrl Pts',(1.69636745940177,88.1066261760139,14.0268391250695));
#55050=CARTESIAN_POINT('Ctrl Pts',(1.65636758146645,88.1196841397183,14.1220648773907));
#55051=CARTESIAN_POINT('Ctrl Pts',(1.6085350209467,88.1328099107082,14.2140570169254));
#55052=CARTESIAN_POINT('Ctrl Pts',(1.55351118181306,88.1458809240025,14.3015262562322));
#55053=CARTESIAN_POINT('Ctrl Pts',(1.54047893831842,88.1489767572024,14.3222431026553));
#55054=CARTESIAN_POINT('Ctrl Pts',(1.52704340476911,88.1520694839144,14.3427060322565));
#55055=CARTESIAN_POINT('Ctrl Pts',(1.51321335128793,88.1551574118775,14.3628975762197));
#55056=CARTESIAN_POINT('Ctrl Pts',(1.46295848126945,88.1663781507289,14.4362684723428));
#55057=CARTESIAN_POINT('Ctrl Pts',(1.4074923193835,88.1775357371721,14.5060644133476));
#55058=CARTESIAN_POINT('Ctrl Pts',(1.34718108012025,88.1885732098478,14.5715037031576));
#55059=CARTESIAN_POINT('Ctrl Pts',(1.34133852868256,88.1896424467369,14.5778430260008));
#55060=CARTESIAN_POINT('Ctrl Pts',(1.33545049497421,88.1907105539787,14.5841414261415));
#55061=CARTESIAN_POINT('Ctrl Pts',(1.32951730389984,88.1917774782276,14.5903981679766));
#55062=CARTESIAN_POINT('Ctrl Pts',(1.28832435836357,88.1991849174837,14.6338374610005));
#55063=CARTESIAN_POINT('Ctrl Pts',(1.24495035848387,88.2065370847293,14.6752741735538));
#55064=CARTESIAN_POINT('Ctrl Pts',(1.19957882997783,88.21391659331,14.7144876613134));
#55065=CARTESIAN_POINT('Ctrl Pts',(1.19955451748868,88.213920547645,14.7145086739953));
#55066=CARTESIAN_POINT('Ctrl Pts',(1.19953020442998,88.2139245019899,14.7145296860377));
#55067=CARTESIAN_POINT('Ctrl Pts',(1.19950589080182,88.2139284563447,14.7145506974405));
#55068=CARTESIAN_POINT('Ctrl Pts',(1.11593767417127,88.2275199440433,14.7867688564188));
#55069=CARTESIAN_POINT('Ctrl Pts',(1.02563776716874,88.2412286460027,14.8514295213002));
#55070=CARTESIAN_POINT('Ctrl Pts',(0.930258331206905,88.2550166677362,14.9077789696688));
#55071=CARTESIAN_POINT('Ctrl Pts',(0.91569495183748,88.2571219453491,14.9163829038982));
#55072=CARTESIAN_POINT('Ctrl Pts',(0.901013232173689,88.259229067882,14.924793124328));
#55073=CARTESIAN_POINT('Ctrl Pts',(0.886219137823221,88.2613378957927,14.933007010672));
#55074=CARTESIAN_POINT('Ctrl Pts',(0.772572838848434,88.2775376361449,14.9961050118797));
#55075=CARTESIAN_POINT('Ctrl Pts',(0.652292830893653,88.2938360567285,15.0476168609656));
#55076=CARTESIAN_POINT('Ctrl Pts',(0.527979550470253,88.3101507799825,15.0863944018198));
#55077=CARTESIAN_POINT('Ctrl Pts',(0.424448048992129,88.3237381279225,15.1186893988996));
#55078=CARTESIAN_POINT('Ctrl Pts',(0.318119568450548,88.3373355083416,15.1421548104238));
#55079=CARTESIAN_POINT('Ctrl Pts',(0.21043485802571,88.3509009945917,15.1561212148862));
#55080=CARTESIAN_POINT('Ctrl Pts',(0.193733636880033,88.353004916169,15.1582873163561));
#55081=CARTESIAN_POINT('Ctrl Pts',(0.176999815718304,88.3551080656399,15.1602248287819));
#55082=CARTESIAN_POINT('Ctrl Pts',(0.160238800968447,88.3572102812538,15.16193114556));
#55083=CARTESIAN_POINT('Ctrl Pts',(0.141476024033436,88.3595635637501,15.1638412471597));
#55084=CARTESIAN_POINT('Ctrl Pts',(0.122678954636867,88.3619157260795,15.1654616709255));
#55085=CARTESIAN_POINT('Ctrl Pts',(0.10385496296275,88.3642666004607,15.1667887242495));
#55086=CARTESIAN_POINT('Ctrl Pts',(0.0922631908627425,88.3657142636628,
15.1676059207275));
#55087=CARTESIAN_POINT('Ctrl Pts',(0.0806612020310315,88.3671614397823,
15.1683118679641));
#55088=CARTESIAN_POINT('Ctrl Pts',(0.0690508883100946,88.3686087156104,
15.1689060565451));
#55089=CARTESIAN_POINT('Ctrl Pts',(0.0690284406559001,88.3686115138076,
15.1689072053633));
#55090=CARTESIAN_POINT('Ctrl Pts',(0.0690059929749823,88.3686143120047,
15.1689083537636));
#55091=CARTESIAN_POINT('Ctrl Pts',(0.0689835452673973,88.3686171102018,
15.1689095017459));
#55092=CARTESIAN_POINT('Ctrl Pts',(-0.070287697526535,88.3859778310131,
15.1760318739227));
#55093=CARTESIAN_POINT('Ctrl Pts',(-0.210584287670222,88.4033360018279,
15.1670707961934));
#55094=CARTESIAN_POINT('Ctrl Pts',(-0.348542202327559,88.42073729513,15.1429176745781));
#55095=CARTESIAN_POINT('Ctrl Pts',(-0.358190763821437,88.4219543144573,
15.1412284429037));
#55096=CARTESIAN_POINT('Ctrl Pts',(-0.36782789330803,88.4231715456873,15.139464881447));
#55097=CARTESIAN_POINT('Ctrl Pts',(-0.377452442644003,88.4243890048776,
15.1376272862118));
#55098=CARTESIAN_POINT('Ctrl Pts',(-0.525784711087892,88.443152323256,15.1093065139653));
#55099=CARTESIAN_POINT('Ctrl Pts',(-0.67112756312192,88.4619706881551,15.0634013115342));
#55100=CARTESIAN_POINT('Ctrl Pts',(-0.809209684749959,88.4808904252129,
15.0010065114326));
#55101=CARTESIAN_POINT('Ctrl Pts',(-0.915286597597981,88.4954248723616,
14.95307381968));
#55102=CARTESIAN_POINT('Ctrl Pts',(-1.01707635697222,88.5100191074381,14.8954089399599));
#55103=CARTESIAN_POINT('Ctrl Pts',(-1.11262549323639,88.5246831062465,14.8285262668702));
#55104=CARTESIAN_POINT('Ctrl Pts',(-1.11264320870511,88.524685825053,14.8285138663614));
#55105=CARTESIAN_POINT('Ctrl Pts',(-1.11266092395628,88.5246885438601,14.8285014655372));
#55106=CARTESIAN_POINT('Ctrl Pts',(-1.11267863898987,88.5246912626678,14.8284890643975));
#55107=CARTESIAN_POINT('Ctrl Pts',(-1.14330389067457,88.5293914609561,14.8070503229886));
#55108=CARTESIAN_POINT('Ctrl Pts',(-1.17327906528719,88.5340934965997,14.784668819843));
#55109=CARTESIAN_POINT('Ctrl Pts',(-1.20256533457562,88.5387822359258,14.7613880173182));
#55110=CARTESIAN_POINT('Ctrl Pts',(-1.28076835270619,88.5513025594575,14.6992213751961));
#55111=CARTESIAN_POINT('Ctrl Pts',(-1.3540720573365,88.5637289006479,14.6306356532594));
#55112=CARTESIAN_POINT('Ctrl Pts',(-1.42175796014288,88.5761351624016,14.5566053511265));
#55113=CARTESIAN_POINT('Ctrl Pts',(-1.43743837137839,88.5790092510689,14.5394551686926));
#55114=CARTESIAN_POINT('Ctrl Pts',(-1.45281720496687,88.58188227308,14.5220125780203));
#55115=CARTESIAN_POINT('Ctrl Pts',(-1.46788535457596,88.5847551667695,14.5042893392683));
#55116=CARTESIAN_POINT('Ctrl Pts',(-1.54742303947419,88.5999198232771,14.4107366857705));
#55117=CARTESIAN_POINT('Ctrl Pts',(-1.61830131596351,88.6150824282435,14.3093661358428));
#55118=CARTESIAN_POINT('Ctrl Pts',(-1.67907078711494,88.6303616915243,14.2020380497371));
#55119=CARTESIAN_POINT('Ctrl Pts',(-1.72593318368016,88.6421443001519,14.1192719627797));
#55120=CARTESIAN_POINT('Ctrl Pts',(-1.76678510767278,88.6540094323558,14.0329658365348));
#55121=CARTESIAN_POINT('Ctrl Pts',(-1.80094213854806,88.6659640695943,13.9440350260138));
#55122=CARTESIAN_POINT('Ctrl Pts',(-1.81020183570973,88.6692048758842,13.9199265964265));
#55123=CARTESIAN_POINT('Ctrl Pts',(-1.81896979445852,88.6724522611031,13.8956253788955));
#55124=CARTESIAN_POINT('Ctrl Pts',(-1.82723302397085,88.6757063666283,13.8711497962955));
#55125=CARTESIAN_POINT('Ctrl Pts',(-1.83276921354094,88.6778865487279,13.8547516719411));
#55126=CARTESIAN_POINT('Ctrl Pts',(-1.83807983876247,88.6800728975008,13.8382761995627));
#55127=CARTESIAN_POINT('Ctrl Pts',(-1.84316024200901,88.6822630488197,13.8217285750483));
#55128=CARTESIAN_POINT('Ctrl Pts',(-1.84316638864592,88.6822656986222,13.8217085545431));
#55129=CARTESIAN_POINT('Ctrl Pts',(-1.84317253494513,88.6822683484268,13.82168853393));
#55130=CARTESIAN_POINT('Ctrl Pts',(-1.84317868090663,88.6822709982337,13.8216685132089));
#55131=CARTESIAN_POINT('Ctrl Pts',(-1.86892231542519,88.6933702638707,13.7378075702968));
#55132=CARTESIAN_POINT('Ctrl Pts',(-1.88874221743413,88.7045085538322,13.6520510803805));
#55133=CARTESIAN_POINT('Ctrl Pts',(-1.90260347940684,88.7155397309517,13.5651986453666));
#55134=CARTESIAN_POINT('Ctrl Pts',(-1.91714044322766,88.727108650362,13.4741123714014));
#55135=CARTESIAN_POINT('Ctrl Pts',(-1.92513147837901,88.7385629232425,13.381790520261));
#55136=CARTESIAN_POINT('Ctrl Pts',(-1.92658457169027,88.7499864935363,13.2891274507891));
#55137=CARTESIAN_POINT('Ctrl Pts',(-1.92669666596446,88.7508677286303,13.281979252228));
#55138=CARTESIAN_POINT('Ctrl Pts',(-1.92676982938156,88.7517487820746,13.2748290153574));
#55139=CARTESIAN_POINT('Ctrl Pts',(-1.92680405313675,88.7526296929277,13.2676771474935));
#55140=CARTESIAN_POINT('Ctrl Pts',(-1.9272815806858,88.764921131969,13.1678864052528));
#55141=CARTESIAN_POINT('Ctrl Pts',(-1.92017781361939,88.7771855323595,13.0677812152398));
#55142=CARTESIAN_POINT('Ctrl Pts',(-1.90552280605296,88.7896695333862,12.9686089262628));
#55143=CARTESIAN_POINT('Ctrl Pts',(-1.8932155739099,88.8001535606385,12.8853243303956));
#55144=CARTESIAN_POINT('Ctrl Pts',(-1.87553987749642,88.8106760280621,12.8026900340916));
#55145=CARTESIAN_POINT('Ctrl Pts',(-1.85250168192507,88.8212112017768,12.7215222233453));
#55146=CARTESIAN_POINT('Ctrl Pts',(-1.8485508230959,88.8230178964009,12.7076026192366));
#55147=CARTESIAN_POINT('Ctrl Pts',(-1.84444237869501,88.8248249636679,12.6937261229755));
#55148=CARTESIAN_POINT('Ctrl Pts',(-1.84017653107027,88.8266322725088,12.679896816798));
#55149=CARTESIAN_POINT('Ctrl Pts',(-1.82788403118873,88.8318402278008,12.6400461799487));
#55150=CARTESIAN_POINT('Ctrl Pts',(-1.81428462719994,88.8370499829996,12.6005891431198));
#55151=CARTESIAN_POINT('Ctrl Pts',(-1.79938852578499,88.8422591879168,12.5616287924912));
#55152=CARTESIAN_POINT('Ctrl Pts',(-1.79938643079468,88.8422599205403,12.5616233131007));
#55153=CARTESIAN_POINT('Ctrl Pts',(-1.7993843357787,88.8422606531638,12.5616178337199));
#55154=CARTESIAN_POINT('Ctrl Pts',(-1.79938224073711,88.8422613857873,12.561612354349));
#55155=CARTESIAN_POINT('Ctrl Pts',(-1.75550406698741,88.8576053197836,12.446853397281));
#55156=CARTESIAN_POINT('Ctrl Pts',(-1.70034180852954,88.8731353030725,12.3361735205915));
#55157=CARTESIAN_POINT('Ctrl Pts',(-1.63522825572563,88.8886956056469,12.2313434824035));
#55158=CARTESIAN_POINT('Ctrl Pts',(-1.62643500288793,88.890796945059,12.2171867210063));
#55159=CARTESIAN_POINT('Ctrl Pts',(-1.617458928175,88.892896337484,12.2031358116288));
#55160=CARTESIAN_POINT('Ctrl Pts',(-1.60830260955541,88.894993274374,12.1891943641998));
#55161=CARTESIAN_POINT('Ctrl Pts',(-1.54062215107708,88.9104931336528,12.0861438268552));
#55162=CARTESIAN_POINT('Ctrl Pts',(-1.46308219877645,88.9258613603039,11.9890520800018));
#55163=CARTESIAN_POINT('Ctrl Pts',(-1.37699019122256,88.9412219523006,11.8996963459718));
#55164=CARTESIAN_POINT('Ctrl Pts',(-1.31131188603211,88.952940318241,11.8315281926566));
#55165=CARTESIAN_POINT('Ctrl Pts',(-1.24065405095072,88.9646548994021,11.7678683169257));
#55166=CARTESIAN_POINT('Ctrl Pts',(-1.16569620874684,88.9764421092307,11.7095709213478));
#55167=CARTESIAN_POINT('Ctrl Pts',(-1.14618501867988,88.979510267072,11.6943963707993));
#55168=CARTESIAN_POINT('Ctrl Pts',(-1.12638263452638,88.9825833522257,11.6795849184114));
#55169=CARTESIAN_POINT('Ctrl Pts',(-1.10630132330414,88.9856627252353,11.6651511174682));
#55170=CARTESIAN_POINT('Ctrl Pts',(-1.0644720027289,88.9920770514396,11.6350855465456));
#55171=CARTESIAN_POINT('Ctrl Pts',(-1.02143273510767,88.998514613264,11.6066601662151));
#55172=CARTESIAN_POINT('Ctrl Pts',(-0.977289395214185,89.0049551134961,
11.5800067458424));
#55173=CARTESIAN_POINT('Ctrl Pts',(-0.97728531593376,89.0049557086619,11.5800042828032));
#55174=CARTESIAN_POINT('Ctrl Pts',(-0.977281236643895,89.0049563038278,
11.5800018197791));
#55175=CARTESIAN_POINT('Ctrl Pts',(-0.977277157344618,89.0049568989936,
11.5799993567702));
#55176=CARTESIAN_POINT('Ctrl Pts',(-0.88357127860379,89.0186284969469,11.5234214005323));
#55177=CARTESIAN_POINT('Ctrl Pts',(-0.784840679583591,89.032320993757,11.4747921042201));
#55178=CARTESIAN_POINT('Ctrl Pts',(-0.682527944527905,89.0460419552663,
11.4344753065681));
#55179=CARTESIAN_POINT('Ctrl Pts',(-0.625672812331476,89.0536666862448,
11.4120712836574));
#55180=CARTESIAN_POINT('Ctrl Pts',(-0.56771688018984,89.0612994637232,11.3922360142513));
#55181=CARTESIAN_POINT('Ctrl Pts',(-0.50887542212368,89.0689454292853,11.3750286892932));
#55182=CARTESIAN_POINT('Ctrl Pts',(-0.467551151634506,89.0743151797882,
11.3629440099815));
#55183=CARTESIAN_POINT('Ctrl Pts',(-0.425786136417242,89.0796919274121,
11.3521549132987));
#55184=CARTESIAN_POINT('Ctrl Pts',(-0.383665898479768,89.0850759437852,
11.3426887221775));
#55185=CARTESIAN_POINT('Ctrl Pts',(-0.318657542679909,89.0933856321715,
11.3280786071685));
#55186=CARTESIAN_POINT('Ctrl Pts',(-0.252811363603994,89.1017115284866,
11.3166234226641));
#55187=CARTESIAN_POINT('Ctrl Pts',(-0.18650142947116,89.110047498965,11.308425057102));
#55188=CARTESIAN_POINT('Ctrl Pts',(-0.14355625558476,89.115446233052,11.303115441895));
#55189=CARTESIAN_POINT('Ctrl Pts',(-0.100418764458797,89.1208489327816,
11.2991716018796));
#55190=CARTESIAN_POINT('Ctrl Pts',(-0.0571844508449886,89.1262547580831,
11.2966164159531));
#55191=CARTESIAN_POINT('Ctrl Pts',(0.0604709601886317,89.1409658647172,
11.289662877772));
#55192=CARTESIAN_POINT('Ctrl Pts',(0.178885143680646,89.1557053730745,11.2929852068958));
#55193=CARTESIAN_POINT('Ctrl Pts',(0.296359922324314,89.1704838848156,11.3070610843454));
#55194=CARTESIAN_POINT('Ctrl Pts',(0.331361481102446,89.1748871359077,11.3112549858585));
#55195=CARTESIAN_POINT('Ctrl Pts',(0.366269713742105,89.1792926013931,11.3164027192666));
#55196=CARTESIAN_POINT('Ctrl Pts',(0.401039572772554,89.1837003908852,11.3224841858637));
#55197=CARTESIAN_POINT('Ctrl Pts',(0.48654720070858,89.1945402284463,11.3374400067266));
#55198=CARTESIAN_POINT('Ctrl Pts',(0.571217792866004,89.2053941230983,11.3580424414153));
#55199=CARTESIAN_POINT('Ctrl Pts',(0.65438387511388,89.2162637405947,11.3839978508651));
#55200=CARTESIAN_POINT('Ctrl Pts',(0.732063173523896,89.2264162479426,11.4082408828981));
#55201=CARTESIAN_POINT('Ctrl Pts',(0.808426473979414,89.2365818485877,11.4371497096827));
#55202=CARTESIAN_POINT('Ctrl Pts',(0.882998816270637,89.2467715336368,11.4705286918841));
#55203=CARTESIAN_POINT('Ctrl Pts',(0.938928072989054,89.2544137974237,11.4955629285351));
#55204=CARTESIAN_POINT('Ctrl Pts',(0.993849744945934,89.2620695979862,11.5231124143193));
#55205=CARTESIAN_POINT('Ctrl Pts',(1.04755755838892,89.2697437728252,11.5531086165209));
#55206=CARTESIAN_POINT('Ctrl Pts',(1.12368721025552,89.2806217479538,11.595627577628));
#55207=CARTESIAN_POINT('Ctrl Pts',(1.19736134207103,89.2915347285946,11.6430608663885));
#55208=CARTESIAN_POINT('Ctrl Pts',(1.26780855661208,89.3024701535888,11.6950965809544));
#55209=CARTESIAN_POINT('Ctrl Pts',(1.3071334156102,89.3085744977958,11.7241438208133));
#55210=CARTESIAN_POINT('Ctrl Pts',(1.34545485670253,89.3146861324596,11.7546259588067));
#55211=CARTESIAN_POINT('Ctrl Pts',(1.38263475452757,89.3208015576538,11.7864757641263));
#55212=CARTESIAN_POINT('Ctrl Pts',(1.40493679414824,89.3244698424786,11.8055805939321));
#55213=CARTESIAN_POINT('Ctrl Pts',(1.42682784486132,89.3281394352485,11.8251771159743));
#55214=CARTESIAN_POINT('Ctrl Pts',(1.44827864572589,89.3318094905473,11.8452492171506));
#55215=CARTESIAN_POINT('Ctrl Pts',(1.46185725747976,89.3341326791467,11.8579550956247));
#55216=CARTESIAN_POINT('Ctrl Pts',(1.47525947650682,89.3364560529941,11.870851522993));
#55217=CARTESIAN_POINT('Ctrl Pts',(1.48847807565657,89.3387793967194,11.8839342377171));
#55218=CARTESIAN_POINT('Ctrl Pts',(1.48919006313926,89.3389045379414,11.8846389061179));
#55219=CARTESIAN_POINT('Ctrl Pts',(1.48990151699167,89.3390296789076,11.8853441139905));
#55220=CARTESIAN_POINT('Ctrl Pts',(1.49061243900187,89.3391548200955,11.8860498635413));
#55221=CARTESIAN_POINT('Ctrl Pts',(1.53796667828799,89.3474904260729,11.9330595673163));
#55222=CARTESIAN_POINT('Ctrl Pts',(1.58303905039154,89.3558409301251,11.9825522306307));
#55223=CARTESIAN_POINT('Ctrl Pts',(1.62563651172041,89.3642002299135,12.034208949601));
#55224=CARTESIAN_POINT('Ctrl Pts',(1.66017048461133,89.3709771556569,12.0760873075337));
#55225=CARTESIAN_POINT('Ctrl Pts',(1.69307497363486,89.3777591313303,12.1193826302394));
#55226=CARTESIAN_POINT('Ctrl Pts',(1.72427118536988,89.3845466705138,12.1639448302362));
#55227=CARTESIAN_POINT('Ctrl Pts',(1.7723601786545,89.3950096693223,12.2326375085202));
#55228=CARTESIAN_POINT('Ctrl Pts',(1.81639346664075,89.4054859067877,12.3043386438082));
#55229=CARTESIAN_POINT('Ctrl Pts',(1.856114219698,89.415988959184,12.3785926830031));
#55230=CARTESIAN_POINT('Ctrl Pts',(1.88283639958516,89.4230548991247,12.4285471687565));
#55231=CARTESIAN_POINT('Ctrl Pts',(1.90760721690775,89.43013345873,12.4796614282811));
#55232=CARTESIAN_POINT('Ctrl Pts',(1.9303286602954,89.4372260301786,12.5317815956755));
#55233=CARTESIAN_POINT('Ctrl Pts',(1.95628446216158,89.4453282170028,12.5913209794656));
#55234=CARTESIAN_POINT('Ctrl Pts',(1.97956412584269,89.4534482687498,12.6521701956165));
#55235=CARTESIAN_POINT('Ctrl Pts',(2.00001176280668,89.4615857304721,12.7140795605838));
#55236=CARTESIAN_POINT('Ctrl Pts',(2.02192190428606,89.4703052190825,12.7804169543727));
#55237=CARTESIAN_POINT('Ctrl Pts',(2.040576579806,89.4790439672403,12.8479664224331));
#55238=CARTESIAN_POINT('Ctrl Pts',(2.05577954694863,89.4877940034291,12.9163579397568));
#55239=CARTESIAN_POINT('Ctrl Pts',(2.06935354874347,89.4956064919925,12.9774214525693));
#55240=CARTESIAN_POINT('Ctrl Pts',(2.08017563594528,89.5034283277029,13.0391587881085));
#55241=CARTESIAN_POINT('Ctrl Pts',(2.08812177108522,89.5112493390432,13.1012674024404));
#55242=CARTESIAN_POINT('Ctrl Pts',(2.09005648935272,89.5131535922737,13.1163895553614));
#55243=CARTESIAN_POINT('Ctrl Pts',(2.09182208300424,89.5150589979386,13.1315432490946));
#55244=CARTESIAN_POINT('Ctrl Pts',(2.0934187011358,89.5169654566193,13.1467240255892));
#55245=CARTESIAN_POINT('Ctrl Pts',(2.10074709634374,89.5257160040317,13.2164030098854));
#55246=CARTESIAN_POINT('Ctrl Pts',(2.10451285347956,89.534488708651,13.2866526735456));
#55247=CARTESIAN_POINT('Ctrl Pts',(2.10475057987297,89.5432733544065,13.3570336583967));
#55248=CARTESIAN_POINT('Ctrl Pts',(2.10501914391959,89.5531975364809,13.4365444010816));
#55249=CARTESIAN_POINT('Ctrl Pts',(2.10078732204221,89.5631359980126,13.5162144357751));
#55250=CARTESIAN_POINT('Ctrl Pts',(2.09213952711942,89.5730846102658,13.5954956988927));
#55251=CARTESIAN_POINT('Ctrl Pts',(2.08571265698564,89.5804782221093,13.6544159654634));
#55252=CARTESIAN_POINT('Ctrl Pts',(2.07684811118568,89.587876932403,13.7131175816072));
#55253=CARTESIAN_POINT('Ctrl Pts',(2.06558085022872,89.5952817283004,13.7713987939231));
#55254=CARTESIAN_POINT('Ctrl Pts',(2.05436939552993,89.6026498485627,13.829391341905));
#55255=CARTESIAN_POINT('Ctrl Pts',(2.04077868025402,89.6100243673617,13.8869707059215));
#55256=CARTESIAN_POINT('Ctrl Pts',(2.02483599892223,89.6174076406047,13.9439492280045));
#55257=CARTESIAN_POINT('Ctrl Pts',(2.00307053176937,89.6274875254061,14.0217381598037));
#55258=CARTESIAN_POINT('Ctrl Pts',(1.97692397415145,89.6375839353334,14.098410238515));
#55259=CARTESIAN_POINT('Ctrl Pts',(1.94641313496093,89.6477506886991,14.1735369875866));
#55260=CARTESIAN_POINT('Ctrl Pts',(1.94377149502577,89.6486309300302,14.1800414897836));
#55261=CARTESIAN_POINT('Ctrl Pts',(1.9410971101864,89.6495116986406,14.1865343945289));
#55262=CARTESIAN_POINT('Ctrl Pts',(1.93838997466722,89.6503930294411,14.193015415411));
#55263=CARTESIAN_POINT('Ctrl Pts',(1.9089497892047,89.6599775301189,14.2634967250478));
#55264=CARTESIAN_POINT('Ctrl Pts',(1.87562502392566,89.6696089976808,14.3325947961261));
#55265=CARTESIAN_POINT('Ctrl Pts',(1.8385115263671,89.6792235000755,14.3997602950827));
#55266=CARTESIAN_POINT('Ctrl Pts',(1.82827175689371,89.6818761815687,14.4182915376527));
#55267=CARTESIAN_POINT('Ctrl Pts',(1.8177438556117,89.6845275722367,14.4366757891377));
#55268=CARTESIAN_POINT('Ctrl Pts',(1.80693046342033,89.6871763309873,14.4549018348219));
#55269=CARTESIAN_POINT('Ctrl Pts',(1.8068646824474,89.6871924441482,14.4550127090968));
#55270=CARTESIAN_POINT('Ctrl Pts',(1.80679889060703,89.6872085573509,14.4551235780121));
#55271=CARTESIAN_POINT('Ctrl Pts',(1.80673308789959,89.6872246705955,14.4552344415652));
#55272=CARTESIAN_POINT('Ctrl Pts',(1.76972370936136,89.6962872333995,14.5175873653615));
#55273=CARTESIAN_POINT('Ctrl Pts',(1.72927268942425,89.7053630621505,14.5782422687359));
#55274=CARTESIAN_POINT('Ctrl Pts',(1.68570332980984,89.71444840587,14.6368121121542));
#55275=CARTESIAN_POINT('Ctrl Pts',(1.66295094763571,89.7191928688211,14.6673979062335));
#55276=CARTESIAN_POINT('Ctrl Pts',(1.63934899938293,89.7239399221334,14.6974154466037));
#55277=CARTESIAN_POINT('Ctrl Pts',(1.61494840448925,89.728689001459,14.7268123931874));
#55278=CARTESIAN_POINT('Ctrl Pts',(1.56533763931517,89.738344727487,14.7865816332472));
#55279=CARTESIAN_POINT('Ctrl Pts',(1.51242342376077,89.7480091484005,14.8437830380337));
#55280=CARTESIAN_POINT('Ctrl Pts',(1.45664814402652,89.7576945147177,14.8980214692319));
#55281=CARTESIAN_POINT('Ctrl Pts',(1.4475441902962,89.7592754144861,14.9068745699315));
#55282=CARTESIAN_POINT('Ctrl Pts',(1.43836408598314,89.7608568712848,14.9156488128494));
#55283=CARTESIAN_POINT('Ctrl Pts',(1.42910983920534,89.7624389371867,14.9243425814522));
#55284=CARTESIAN_POINT('Ctrl Pts',(1.37930610290667,89.7709531679907,14.9711299828834));
#55285=CARTESIAN_POINT('Ctrl Pts',(1.32736213493766,89.7794681696918,15.0155896551332));
#55286=CARTESIAN_POINT('Ctrl Pts',(1.2734092069618,89.7880180567517,15.0576107838982));
#55287=CARTESIAN_POINT('Ctrl Pts',(1.24821863978466,89.7920099903208,15.0772304061639));
#55288=CARTESIAN_POINT('Ctrl Pts',(1.2225895882429,89.7960095299081,15.0963179304627));
#55289=CARTESIAN_POINT('Ctrl Pts',(1.19653285737242,89.8000201534158,15.1148591442773));
#55290=CARTESIAN_POINT('Ctrl Pts',(1.10396081883357,89.8142687403077,15.1807307215037));
#55291=CARTESIAN_POINT('Ctrl Pts',(1.00595061054925,89.8286342969753,15.239732538508));
#55292=CARTESIAN_POINT('Ctrl Pts',(0.903574269901593,89.8430052181643,15.2907907530602));
#55293=CARTESIAN_POINT('Ctrl Pts',(0.846152658837509,89.8510656884051,15.3194286680227));
#55294=CARTESIAN_POINT('Ctrl Pts',(0.787363081876542,89.8591270242994,15.3455643649816));
#55295=CARTESIAN_POINT('Ctrl Pts',(0.727444049749919,89.867165541212,15.369003265404));
#55296=CARTESIAN_POINT('Ctrl Pts',(0.727402714504093,89.8671710865965,15.3690194347692));
#55297=CARTESIAN_POINT('Ctrl Pts',(0.727361378695082,89.8671766319729,15.3690356028621));
#55298=CARTESIAN_POINT('Ctrl Pts',(0.727320042322842,89.8671821773411,15.3690517696829));
#55299=CARTESIAN_POINT('Ctrl Pts',(0.633926362663027,89.8797111515772,15.4055784118837));
#55300=CARTESIAN_POINT('Ctrl Pts',(0.537655586078528,89.8921986464091,15.4356068382399));
#55301=CARTESIAN_POINT('Ctrl Pts',(0.439549471909447,89.9047021655974,15.4589748238371));
#55302=CARTESIAN_POINT('Ctrl Pts',(0.391781509366459,89.9107901412684,15.4703527187845));
#55303=CARTESIAN_POINT('Ctrl Pts',(0.343578845031173,89.9168818983963,15.4801522981313));
#55304=CARTESIAN_POINT('Ctrl Pts',(0.295063468373458,89.9229839676533,15.4883589325666));
#55305=CARTESIAN_POINT('Ctrl Pts',(0.21733041195195,89.932760919344,15.501507893196));
#55306=CARTESIAN_POINT('Ctrl Pts',(0.138781505009049,89.9425667517482,15.5105715366972));
#55307=CARTESIAN_POINT('Ctrl Pts',(0.0598350709781667,89.9524389190382,
15.5154971229762));
#55308=CARTESIAN_POINT('Ctrl Pts',(-0.0907905799123581,89.9712744958698,
15.5248948829688));
#55309=CARTESIAN_POINT('Ctrl Pts',(-0.242935126360048,89.9903610793247,
15.5192327218574));
#55310=CARTESIAN_POINT('Ctrl Pts',(-0.393543685354344,90.0094943828665,
15.4981219338294));
#55311=CARTESIAN_POINT('Ctrl Pts',(-0.482069985530059,90.0207407594603,
15.4857132103784));
#55312=CARTESIAN_POINT('Ctrl Pts',(-0.570055749724395,90.0320010766183,
15.4679628941004));
#55313=CARTESIAN_POINT('Ctrl Pts',(-0.656768808477112,90.0432243027483,
15.4448295293634));
#55314=CARTESIAN_POINT('Ctrl Pts',(-0.677209396973242,90.0458699174944,
15.4393763762176));
#55315=CARTESIAN_POINT('Ctrl Pts',(-0.697579335379399,90.048513473307,15.4336243185246));
#55316=CARTESIAN_POINT('Ctrl Pts',(-0.717869188378609,90.0511543057617,
15.4275732122971));
#55317=CARTESIAN_POINT('Ctrl Pts',(-0.717876542771937,90.0511552629752,
15.4275710189734));
#55318=CARTESIAN_POINT('Ctrl Pts',(-0.717883897155325,90.0511562201883,
15.4275688256103));
#55319=CARTESIAN_POINT('Ctrl Pts',(-0.717891251528768,90.0511571774009,
15.4275666322078));
#55320=CARTESIAN_POINT('Ctrl Pts',(-0.827736790592108,90.0654541855691,
15.3948057879492));
#55321=CARTESIAN_POINT('Ctrl Pts',(-0.935357513734576,90.0796566860487,
15.3532510554188));
#55322=CARTESIAN_POINT('Ctrl Pts',(-1.03947911611388,90.0939337420625,15.3036333564526));
#55323=CARTESIAN_POINT('Ctrl Pts',(-1.07355714578967,90.0986064893829,15.287393946194));
#55324=CARTESIAN_POINT('Ctrl Pts',(-1.10726283864037,90.1032874756028,15.270290017163));
#55325=CARTESIAN_POINT('Ctrl Pts',(-1.14055784633631,90.1079830971342,15.2523436669056));
#55326=CARTESIAN_POINT('Ctrl Pts',(-1.24204696389607,90.1222961884534,15.1976399927789));
#55327=CARTESIAN_POINT('Ctrl Pts',(-1.33973260938104,90.136747990413,15.1351046176306));
#55328=CARTESIAN_POINT('Ctrl Pts',(-1.4324719090101,90.1512892718812,15.0654270397336));
#55329=CARTESIAN_POINT('Ctrl Pts',(-1.52576652305736,90.1659176252087,14.9953322388925));
#55330=CARTESIAN_POINT('Ctrl Pts',(-1.61405200452164,90.1806357466517,14.9180044120357));
#55331=CARTESIAN_POINT('Ctrl Pts',(-1.69606313870812,90.1953674578192,14.8342235573276));
#55332=CARTESIAN_POINT('Ctrl Pts',(-1.7617816118829,90.2071725081308,14.7670869434116));
#55333=CARTESIAN_POINT('Ctrl Pts',(-1.8234694431867,90.2189855359406,14.6958054663359));
#55334=CARTESIAN_POINT('Ctrl Pts',(-1.88045323053108,90.2307614340735,14.620850866844));
#55335=CARTESIAN_POINT('Ctrl Pts',(-1.89458042316835,90.233680867638,14.6022684223379));
#55336=CARTESIAN_POINT('Ctrl Pts',(-1.90841870829354,90.236598021982,14.5834603467572));
#55337=CARTESIAN_POINT('Ctrl Pts',(-1.92195827198616,90.2395122155635,14.5644340605548));
#55338=CARTESIAN_POINT('Ctrl Pts',(-1.92196095332451,90.2395127926824,14.5644302926409));
#55339=CARTESIAN_POINT('Ctrl Pts',(-1.92196363465126,90.2395133698013,14.5644265247183));
#55340=CARTESIAN_POINT('Ctrl Pts',(-1.92196631596654,90.23951394692,14.5644227567868));
#55341=CARTESIAN_POINT('Ctrl Pts',(-1.96439769823558,90.2486467574422,14.5047958479319));
#55342=CARTESIAN_POINT('Ctrl Pts',(-2.00393984298306,90.2577467821853,14.4429711086769));
#55343=CARTESIAN_POINT('Ctrl Pts',(-2.04045806000607,90.2668733450591,14.3792626217406));
#55344=CARTESIAN_POINT('Ctrl Pts',(-2.11723191437586,90.2860605197375,14.2453254666193));
#55345=CARTESIAN_POINT('Ctrl Pts',(-2.18065510084425,90.3053667354458,14.1030416821444));
#55346=CARTESIAN_POINT('Ctrl Pts',(-2.22975564814591,90.3247803034858,13.9553143987107));
#55347=CARTESIAN_POINT('Ctrl Pts',(-2.27591121519674,90.3430294736195,13.8164475853966));
#55348=CARTESIAN_POINT('Ctrl Pts',(-2.30940974774325,90.3613731262018,13.6727721598186));
#55349=CARTESIAN_POINT('Ctrl Pts',(-2.32943424498219,90.3798185934638,13.5267076351754));
#55350=CARTESIAN_POINT('Ctrl Pts',(-2.34701020656248,90.3960086041321,13.398503443942));
#55351=CARTESIAN_POINT('Ctrl Pts',(-2.35420629851879,90.4122771501022,13.2684594600005));
#55352=CARTESIAN_POINT('Ctrl Pts',(-2.35046331881443,90.4286438543728,13.1382034562168));
#55353=CARTESIAN_POINT('Ctrl Pts',(-2.35020431696362,90.4297763763293,13.1291901703524));
#55354=CARTESIAN_POINT('Ctrl Pts',(-2.34989293127384,90.4309093744856,13.1201758622685));
#55355=CARTESIAN_POINT('Ctrl Pts',(-2.34952903634181,90.4320427289652,13.1111610895567));
#55356=CARTESIAN_POINT('Ctrl Pts',(-2.34952837932184,90.4320447752606,13.1111448131945));
#55357=CARTESIAN_POINT('Ctrl Pts',(-2.34952772213086,90.4320468215568,13.1111285368325));
#55358=CARTESIAN_POINT('Ctrl Pts',(-2.34952706476887,90.4320488678537,13.1111122604705));
#55359=CARTESIAN_POINT('Ctrl Pts',(-2.34569136950774,90.4439889730878,13.0161399848232));
#55360=CARTESIAN_POINT('Ctrl Pts',(-2.33603579895137,90.4559546637623,12.9211722629142));
#55361=CARTESIAN_POINT('Ctrl Pts',(-2.32065263668303,90.4679454242299,12.8269115977101));
#55362=CARTESIAN_POINT('Ctrl Pts',(-2.30526601779872,90.4799388790366,12.7326297520156));
#55363=CARTESIAN_POINT('Ctrl Pts',(-2.2841475829805,90.4919571483405,12.6390547729888));
#55364=CARTESIAN_POINT('Ctrl Pts',(-2.25738210024256,90.503983664951,12.5469301646683));
#55365=CARTESIAN_POINT('Ctrl Pts',(-2.23074507497194,90.5159524618529,12.455247696472));
#55366=CARTESIAN_POINT('Ctrl Pts',(-2.19851342075431,90.5279290824648,12.3650020717527));
#55367=CARTESIAN_POINT('Ctrl Pts',(-2.1607880251354,90.5398858435885,12.2769672126659));
#55368=CARTESIAN_POINT('Ctrl Pts',(-2.13579511881785,90.547807144498,12.218644511214));
#55369=CARTESIAN_POINT('Ctrl Pts',(-2.10839141453715,90.5557194907249,12.1612930342263));
#55370=CARTESIAN_POINT('Ctrl Pts',(-2.07861575088476,90.5636133483745,12.1051455331855));
#55371=CARTESIAN_POINT('Ctrl Pts',(-2.07860974192645,90.5636149414158,12.1051342021872));
#55372=CARTESIAN_POINT('Ctrl Pts',(-2.0786037328715,90.5636165344548,12.1051228712357));
#55373=CARTESIAN_POINT('Ctrl Pts',(-2.07859772372004,90.5636181274914,12.1051115403313));
#55374=CARTESIAN_POINT('Ctrl Pts',(-2.04044817041101,90.5737316413858,12.0331764348937));
#55375=CARTESIAN_POINT('Ctrl Pts',(-1.99840413134336,90.5837520713751,11.9631304559366));
#55376=CARTESIAN_POINT('Ctrl Pts',(-1.95275133842558,90.5937882050271,11.8953265040634));
#55377=CARTESIAN_POINT('Ctrl Pts',(-1.88053299889385,90.609664405832,11.7880671557298));
#55378=CARTESIAN_POINT('Ctrl Pts',(-1.7992771670741,90.6255814097833,11.6864053235378));
#55379=CARTESIAN_POINT('Ctrl Pts',(-1.71023485897269,90.6416652727592,11.5915359226003));
#55380=CARTESIAN_POINT('Ctrl Pts',(-1.69318039702198,90.6447458491166,11.5733653852112));
#55381=CARTESIAN_POINT('Ctrl Pts',(-1.67584042436733,90.6478325277532,11.5554441003856));
#55382=CARTESIAN_POINT('Ctrl Pts',(-1.65822392842862,90.6509261671784,11.5377805595999));
#55383=CARTESIAN_POINT('Ctrl Pts',(-1.55690232746079,90.6687192913317,11.4361883793274));
#55384=CARTESIAN_POINT('Ctrl Pts',(-1.44646841097967,90.6866617835674,11.3430843777608));
#55385=CARTESIAN_POINT('Ctrl Pts',(-1.32863445590084,90.7046686978522,11.2598702682155));
#55386=CARTESIAN_POINT('Ctrl Pts',(-1.31660531051532,90.7065069437953,11.2513753091761));
#55387=CARTESIAN_POINT('Ctrl Pts',(-1.30449900161314,90.7083458653439,11.242983411804));
#55388=CARTESIAN_POINT('Ctrl Pts',(-1.29231732047533,90.7101853750474,11.2346960652191));
#55389=CARTESIAN_POINT('Ctrl Pts',(-1.20417827695615,90.7234949194345,11.1747339965159));
#55390=CARTESIAN_POINT('Ctrl Pts',(-1.1120907816292,90.7368358015747,11.1202407727964));
#55391=CARTESIAN_POINT('Ctrl Pts',(-1.01666699720766,90.7503325163293,11.0718745497284));
#55392=CARTESIAN_POINT('Ctrl Pts',(-0.990650113791305,90.754012337418,11.058687707533));
#55393=CARTESIAN_POINT('Ctrl Pts',(-0.964385361909007,90.7577037136244,
11.0459565830478));
#55394=CARTESIAN_POINT('Ctrl Pts',(-0.937885500959489,90.761409102389,11.0336950931625));
#55395=CARTESIAN_POINT('Ctrl Pts',(-0.8572604977869,90.7726826325209,10.9963898913434));
#55396=CARTESIAN_POINT('Ctrl Pts',(-0.774431577449996,90.7840915228087,
10.9634240026405));
#55397=CARTESIAN_POINT('Ctrl Pts',(-0.689887365874428,90.7954885709355,
10.9350906935229));
#55398=CARTESIAN_POINT('Ctrl Pts',(-0.62448651218742,90.8043049838289,10.913172899631));
#55399=CARTESIAN_POINT('Ctrl Pts',(-0.558059054054031,90.8131144022974,
10.8940262664436));
#55400=CARTESIAN_POINT('Ctrl Pts',(-0.490820708754846,90.8218507127328,
10.8777679086565));
#55401=CARTESIAN_POINT('Ctrl Pts',(-0.465155870456856,90.8251853574752,
10.8715621027024));
#55402=CARTESIAN_POINT('Ctrl Pts',(-0.439375156471158,90.82850937082,10.8657777826168));
#55403=CARTESIAN_POINT('Ctrl Pts',(-0.413493044403973,90.8318197572746,
10.8604218548983));
#55404=CARTESIAN_POINT('Ctrl Pts',(-0.413478074513194,90.8318216719609,
10.8604187570965));
#55405=CARTESIAN_POINT('Ctrl Pts',(-0.413463104582681,90.8318235866456,
10.8604156594385));
#55406=CARTESIAN_POINT('Ctrl Pts',(-0.413448134612573,90.8318255013288,
10.8604125619243));
#55407=CARTESIAN_POINT('Ctrl Pts',(-0.333529509966445,90.8420472217721,
10.8438761848016));
#55408=CARTESIAN_POINT('Ctrl Pts',(-0.252479021499226,90.8522261073672,
10.8314406872672));
#55409=CARTESIAN_POINT('Ctrl Pts',(-0.170791271286606,90.8623925468392,
10.8231091301441));
#55410=CARTESIAN_POINT('Ctrl Pts',(-0.0888772994115235,90.872587140702,
10.8147545000548));
#55411=CARTESIAN_POINT('Ctrl Pts',(-0.006322974021356,90.8827697010739,
10.8105251555397));
#55412=CARTESIAN_POINT('Ctrl Pts',(0.0764170553935699,90.8929762453701,
10.8104036016593));
#55413=CARTESIAN_POINT('Ctrl Pts',(0.159274164449316,90.9031972322349,10.8102818757764));
#55414=CARTESIAN_POINT('Ctrl Pts',(0.242317594805092,90.9134426941975,10.8142782626444));
#55415=CARTESIAN_POINT('Ctrl Pts',(0.325137423376013,90.9237474031384,10.8223751710848));
#55416=CARTESIAN_POINT('Ctrl Pts',(0.350440559585788,90.9268957005744,10.8248489407204));
#55417=CARTESIAN_POINT('Ctrl Pts',(0.375723142416177,90.9300494945329,10.8277055381386));
#55418=CARTESIAN_POINT('Ctrl Pts',(0.400974295891035,90.9332096597013,10.8309447386746));
#55419=CARTESIAN_POINT('Ctrl Pts',(2.7026896336633,109.940943033253,11.4686318458822));
#55420=CARTESIAN_POINT('Ctrl Pts',(3.26735297233184,110.066470556496,12.3011813254344));
#55421=CARTESIAN_POINT('Ctrl Pts',(3.54872189103824,110.31458662676,14.4925410642362));
#55422=CARTESIAN_POINT('Ctrl Pts',(1.2278560935176,110.683943140033,16.8126341319678));
#55423=CARTESIAN_POINT('Ctrl Pts',(-1.98815709271125,111.048104563125,16.4106880643088));
#55424=CARTESIAN_POINT('Ctrl Pts',(-3.4441229434605,111.368813519898,13.9701597426272));
#55425=CARTESIAN_POINT('Ctrl Pts',(-2.93831080545766,111.646687017574,11.690169137757));
#55426=CARTESIAN_POINT('Ctrl Pts',(-1.49830702440856,111.882714715422,10.3371241303155));
#55427=CARTESIAN_POINT('Ctrl Pts',(0.280737125628576,112.096881644401,10.0718010286459));
#55428=CARTESIAN_POINT('Ctrl Pts',(1.74904768178971,112.289662909091,10.662271337796));
#55429=CARTESIAN_POINT('Ctrl Pts',(3.02452688847434,112.518914294108,12.0562658471873));
#55430=CARTESIAN_POINT('Ctrl Pts',(3.11698085316947,112.697773863978,13.6322209732873));
#55431=CARTESIAN_POINT('Ctrl Pts',(2.67727559417373,112.828040954899,14.5802342731525));
#55432=CARTESIAN_POINT('Ctrl Pts',(2.53266799104064,112.865192170059,14.8405243568169));
#55433=CARTESIAN_POINT('Ctrl Pts',(2.38092755732967,112.897610736312,15.0523028856687));
#55434=CARTESIAN_POINT('Ctrl Pts',(2.23522000283791,112.925334087009,15.2199637994609));
#55435=CARTESIAN_POINT('Ctrl Pts',(2.13400663653402,112.943798822738,15.3278891434887));
#55436=CARTESIAN_POINT('Ctrl Pts',(2.0001787117739,112.966847391524,15.455301731792));
#55437=CARTESIAN_POINT('Ctrl Pts',(1.85738520662406,112.989851815714,15.5720267197933));
#55438=CARTESIAN_POINT('Ctrl Pts',(1.73828449576717,113.008229097572,15.6586262836342));
#55439=CARTESIAN_POINT('Ctrl Pts',(1.51431603254412,113.041887977247,15.808876006038));
#55440=CARTESIAN_POINT('Ctrl Pts',(0.956180939097246,113.119679718823,16.0934532359472));
#55441=CARTESIAN_POINT('Ctrl Pts',(0.273313501728111,113.204429118413,16.2098273011314));
#55442=CARTESIAN_POINT('Ctrl Pts',(-0.303493560391393,113.276579576405,
16.1618219259865));
#55443=CARTESIAN_POINT('Ctrl Pts',(-0.681851442858624,113.324549589041,
16.0917776669268));
#55444=CARTESIAN_POINT('Ctrl Pts',(-1.13601080272643,113.384261897672,15.933918065193));
#55445=CARTESIAN_POINT('Ctrl Pts',(-1.62932968530997,113.455513991744,15.6408930038963));
#55446=CARTESIAN_POINT('Ctrl Pts',(-2.19233238507603,113.549976853383,15.1296830484934));
#55447=CARTESIAN_POINT('Ctrl Pts',(-2.77518491629114,113.690435180344,14.1396792195023));
#55448=CARTESIAN_POINT('Ctrl Pts',(-2.81554662440005,113.874922446606,12.5934052944144));
#55449=CARTESIAN_POINT('Ctrl Pts',(-1.8804390341719,114.078615238882,11.163100039376));
#55450=CARTESIAN_POINT('Ctrl Pts',(-0.329416415584754,114.278390904853,
10.5298412194754));
#55451=CARTESIAN_POINT('Ctrl Pts',(1.27457905533916,114.474208054262,10.8825417553195));
#55452=CARTESIAN_POINT('Ctrl Pts',(2.37162054973234,114.666047218268,12.0600861420246));
#55453=CARTESIAN_POINT('Ctrl Pts',(2.56321987131624,114.822601276229,13.3585258539676));
#55454=CARTESIAN_POINT('Ctrl Pts',(2.26157455097497,114.945869817376,14.3109533766938));
#55455=CARTESIAN_POINT('Ctrl Pts',(1.83956712796069,115.037340055854,14.9205049468466));
#55456=CARTESIAN_POINT('Ctrl Pts',(1.26089548214983,115.127834416872,15.3697004555521));
#55457=CARTESIAN_POINT('Ctrl Pts',(0.129036300584683,115.277046540176,15.8016347440481));
#55458=CARTESIAN_POINT('Ctrl Pts',(-1.6256382048639,115.481461223343,15.3540088207721));
#55459=CARTESIAN_POINT('Ctrl Pts',(-2.54430496499387,115.735983946442,13.2862198412236));
#55460=CARTESIAN_POINT('Ctrl Pts',(-1.50310124092006,115.982628746918,11.3521388995005));
#55461=CARTESIAN_POINT('Ctrl Pts',(0.236180153310175,116.182036367951,11.051152222629));
#55462=CARTESIAN_POINT('Ctrl Pts',(1.36095280562168,116.338203952737,11.6748599396884));
#55463=CARTESIAN_POINT('Ctrl Pts',(1.91039880018758,116.453732635065,12.4476155138811));
#55464=CARTESIAN_POINT('Ctrl Pts',(2.06279366972351,116.567757542103,13.3735551461719));
#55465=CARTESIAN_POINT('Ctrl Pts',(1.79847542918091,116.680374431451,14.2604126259241));
#55466=CARTESIAN_POINT('Ctrl Pts',(1.17979853787208,116.791679755757,14.9348521268195));
#55467=CARTESIAN_POINT('Ctrl Pts',(0.337632386723327,116.901777224248,15.2667461038567));
#55468=CARTESIAN_POINT('Ctrl Pts',(-0.555414918986166,117.010790218224,
15.1973087665612));
#55469=CARTESIAN_POINT('Ctrl Pts',(-1.32234103769279,117.118784767411,14.7474799210793));
#55470=CARTESIAN_POINT('Ctrl Pts',(-1.80775797452488,117.225962200641,14.0149830105422));
#55471=CARTESIAN_POINT('Ctrl Pts',(-1.97092422810024,117.367688877029,12.8570909938671));
#55472=CARTESIAN_POINT('Ctrl Pts',(-1.15746163758973,117.543956302063,11.5274758002029));
#55473=CARTESIAN_POINT('Ctrl Pts',(0.372235631248106,117.717274790277,11.3409644660964));
#55474=CARTESIAN_POINT('Ctrl Pts',(1.35279634366171,117.85835091102,11.9701895143167));
#55475=CARTESIAN_POINT('Ctrl Pts',(1.63946046051867,117.926140628132,12.4263768287653));
#55476=CARTESIAN_POINT('Ctrl Pts',(1.74059764913481,117.963005556155,12.7174919546938));
#55477=CARTESIAN_POINT('Ctrl Pts',(2.46682853611889,110.148827126478,11.5762898043294));
#55478=CARTESIAN_POINT('Ctrl Pts',(2.99203546797916,110.264626975476,12.3415064920099));
#55479=CARTESIAN_POINT('Ctrl Pts',(3.25843192948515,110.492593339858,14.353787870894));
#55480=CARTESIAN_POINT('Ctrl Pts',(1.15008059527702,110.829525057485,16.4792175839857));
#55481=CARTESIAN_POINT('Ctrl Pts',(-1.76690846020068,111.15965328974,16.128044193202));
#55482=CARTESIAN_POINT('Ctrl Pts',(-3.09069428562109,111.44884856996,13.9338798976915));
#55483=CARTESIAN_POINT('Ctrl Pts',(-2.64792112441307,111.698505687743,11.8828823533875));
#55484=CARTESIAN_POINT('Ctrl Pts',(-1.364387090511,111.910048500832,10.6624900785378));
#55485=CARTESIAN_POINT('Ctrl Pts',(0.22560775652403,112.101620567308,10.4155318988324));
#55486=CARTESIAN_POINT('Ctrl Pts',(1.54073116051239,112.273844336496,10.9347895473236));
#55487=CARTESIAN_POINT('Ctrl Pts',(2.6872815763924,112.478483531869,12.1719261697143));
#55488=CARTESIAN_POINT('Ctrl Pts',(2.77889252277574,112.638026520578,13.5772495408711));
#55489=CARTESIAN_POINT('Ctrl Pts',(2.39223612973147,112.754241083453,14.4256655835251));
#55490=CARTESIAN_POINT('Ctrl Pts',(2.26476199794164,112.787385971573,14.6587625565873));
#55491=CARTESIAN_POINT('Ctrl Pts',(2.13063450055583,112.816309995904,14.8486316482196));
#55492=CARTESIAN_POINT('Ctrl Pts',(2.0016185710066,112.841046449208,14.9991113435169));
#55493=CARTESIAN_POINT('Ctrl Pts',(1.91194642227727,112.857522512299,15.0960249822623));
#55494=CARTESIAN_POINT('Ctrl Pts',(1.79328146006558,112.878089723521,15.2105312140984));
#55495=CARTESIAN_POINT('Ctrl Pts',(1.66654088102953,112.898619590859,15.3155646046583));
#55496=CARTESIAN_POINT('Ctrl Pts',(1.56075776911136,112.915021115362,15.3935753724432));
#55497=CARTESIAN_POINT('Ctrl Pts',(1.36174741141507,112.945063107886,15.5290360812719));
#55498=CARTESIAN_POINT('Ctrl Pts',(0.865207509480216,113.014505004717,15.7864600922824));
#55499=CARTESIAN_POINT('Ctrl Pts',(0.256010777506312,113.090196121383,15.8946003979176));
#55500=CARTESIAN_POINT('Ctrl Pts',(-0.259785089431699,113.154673519109,
15.8552288750756));
#55501=CARTESIAN_POINT('Ctrl Pts',(-0.598435642469266,113.197551777644,
15.7949356824436));
#55502=CARTESIAN_POINT('Ctrl Pts',(-1.00556611563695,113.250949337017,15.656567674988));
#55503=CARTESIAN_POINT('Ctrl Pts',(-1.44883854704915,113.31470577837,15.3974131488982));
#55504=CARTESIAN_POINT('Ctrl Pts',(-1.95617230760116,113.399287438372,14.9431569756853));
#55505=CARTESIAN_POINT('Ctrl Pts',(-2.48502734798563,113.525200413102,14.0593681219646));
#55506=CARTESIAN_POINT('Ctrl Pts',(-2.53170030021554,113.69095996749,12.6702784722711));
#55507=CARTESIAN_POINT('Ctrl Pts',(-1.69849632391851,113.874606866753,11.3742009089813));
#55508=CARTESIAN_POINT('Ctrl Pts',(-0.298732928026003,114.055469640001,
10.789850139448));
#55509=CARTESIAN_POINT('Ctrl Pts',(1.16312748155585,114.233611654871,11.0990481403683));
#55510=CARTESIAN_POINT('Ctrl Pts',(2.17562557368189,114.409112848813,12.1681746471377));
#55511=CARTESIAN_POINT('Ctrl Pts',(2.36194092480953,114.553242740846,13.3621756745578));
#55512=CARTESIAN_POINT('Ctrl Pts',(2.08943327339976,114.667328450305,14.2459096374332));
#55513=CARTESIAN_POINT('Ctrl Pts',(1.7016995736089,114.752299492816,14.8151631946314));
#55514=CARTESIAN_POINT('Ctrl Pts',(1.16513580383993,114.836691425922,15.2382255534932));
#55515=CARTESIAN_POINT('Ctrl Pts',(0.108551867838543,114.976407891281,15.6507895457554));
#55516=CARTESIAN_POINT('Ctrl Pts',(-1.55298113289362,115.169459669971,15.2450202857454));
#55517=CARTESIAN_POINT('Ctrl Pts',(-2.45397706454464,115.413280794756,13.2740017965845));
#55518=CARTESIAN_POINT('Ctrl Pts',(-1.4615503617417,115.653269049662,11.3806804618505));
#55519=CARTESIAN_POINT('Ctrl Pts',(0.256442440862655,115.85056737016,11.0643865721294));
#55520=CARTESIAN_POINT('Ctrl Pts',(1.38946688731323,116.007124891132,11.6807892864116));
#55521=CARTESIAN_POINT('Ctrl Pts',(1.95126218052327,116.123983761119,12.4582101085309));
#55522=CARTESIAN_POINT('Ctrl Pts',(2.11418980813084,116.240372536293,13.4022205649728));
#55523=CARTESIAN_POINT('Ctrl Pts',(1.848811260865,116.356379449463,14.3179598059507));
#55524=CARTESIAN_POINT('Ctrl Pts',(1.21085031354557,116.472090186163,15.0239715497253));
#55525=CARTESIAN_POINT('Ctrl Pts',(0.329812066379183,116.587595407081,15.378710756044));
#55526=CARTESIAN_POINT('Ctrl Pts',(-0.616220706596642,116.702997505549,
15.3119803645535));
#55527=CARTESIAN_POINT('Ctrl Pts',(-1.43882357083797,116.818354430523,14.8373638391765));
#55528=CARTESIAN_POINT('Ctrl Pts',(-1.96737039240484,116.933817619422,14.0514453373533));
#55529=CARTESIAN_POINT('Ctrl Pts',(-2.15291016394976,117.087869167659,12.7950288806392));
#55530=CARTESIAN_POINT('Ctrl Pts',(-1.27267889437544,117.281528367953,11.3234188443989));
#55531=CARTESIAN_POINT('Ctrl Pts',(0.436407543225603,117.475511187756,11.1026070944465));
#55532=CARTESIAN_POINT('Ctrl Pts',(1.54224885923002,117.633776918282,11.802189669093));
#55533=CARTESIAN_POINT('Ctrl Pts',(1.87412331095756,117.711599788581,12.3238494146484));
#55534=CARTESIAN_POINT('Ctrl Pts',(1.98777482999691,117.752566587265,12.6463749810985));
#55535=CARTESIAN_POINT('Ctrl Pts',(2.23096743857449,110.356711219704,11.6839477627767));
#55536=CARTESIAN_POINT('Ctrl Pts',(2.71671796362648,110.462783394457,12.3818316585855));
#55537=CARTESIAN_POINT('Ctrl Pts',(2.96814196793207,110.670600052954,14.2150346775519));
#55538=CARTESIAN_POINT('Ctrl Pts',(1.07230509703644,110.975106974938,16.1458010360037));
#55539=CARTESIAN_POINT('Ctrl Pts',(-1.54565982769012,111.271202016355,15.8454003220953));
#55540=CARTESIAN_POINT('Ctrl Pts',(-2.73726562778171,111.528883620023,13.8976000527558));
#55541=CARTESIAN_POINT('Ctrl Pts',(-2.35753144336851,111.750324357911,12.0755955690179));
#55542=CARTESIAN_POINT('Ctrl Pts',(-1.23046715661347,111.93738228624,10.9878560267602));
#55543=CARTESIAN_POINT('Ctrl Pts',(0.170478387419463,112.106359490217,10.7592627690187));
#55544=CARTESIAN_POINT('Ctrl Pts',(1.33241463923504,112.258025763899,11.2073077568512));
#55545=CARTESIAN_POINT('Ctrl Pts',(2.35003626431044,112.438052769629,12.2875864922412));
#55546=CARTESIAN_POINT('Ctrl Pts',(2.440804192382,112.578279177178,13.5222781084548));
#55547=CARTESIAN_POINT('Ctrl Pts',(2.10719666528918,112.680441212008,14.2710968938976));
#55548=CARTESIAN_POINT('Ctrl Pts',(1.99685600484262,112.709579773087,14.4770007563578));
#55549=CARTESIAN_POINT('Ctrl Pts',(1.88034144378197,112.735009255498,14.6449604107706));
#55550=CARTESIAN_POINT('Ctrl Pts',(1.76801713917526,112.756758811409,14.778258887573));
#55551=CARTESIAN_POINT('Ctrl Pts',(1.68988620802049,112.771246201861,14.8641608210362));
#55552=CARTESIAN_POINT('Ctrl Pts',(1.58638420835724,112.789332055518,14.965760696405));
#55553=CARTESIAN_POINT('Ctrl Pts',(1.47569655543498,112.807387366005,15.0591024895235));
#55554=CARTESIAN_POINT('Ctrl Pts',(1.38323104245549,112.821813133151,15.1285244612521));
#55555=CARTESIAN_POINT('Ctrl Pts',(1.20917879028598,112.848238238525,15.2491961565059));
#55556=CARTESIAN_POINT('Ctrl Pts',(0.774234079863162,112.90933029061,15.4794669486178));
#55557=CARTESIAN_POINT('Ctrl Pts',(0.238708053284494,112.975963124354,15.5793734947038));
#55558=CARTESIAN_POINT('Ctrl Pts',(-0.216076618472028,113.032767461814,
15.5486358241645));
#55559=CARTESIAN_POINT('Ctrl Pts',(-0.515019842079931,113.070553966245,
15.4980936979603));
#55560=CARTESIAN_POINT('Ctrl Pts',(-0.87512142854749,113.117636776362,15.3792172847831));
#55561=CARTESIAN_POINT('Ctrl Pts',(-1.26834740878835,113.173897564996,15.1539332939003));
#55562=CARTESIAN_POINT('Ctrl Pts',(-1.72001223012634,113.248598023361,14.7566309028774));
#55563=CARTESIAN_POINT('Ctrl Pts',(-2.19486977968014,113.359965645859,13.9790570244268));
#55564=CARTESIAN_POINT('Ctrl Pts',(-2.24785397603106,113.506997488377,12.7471516501278));
#55565=CARTESIAN_POINT('Ctrl Pts',(-1.51655361366513,113.670598494623,11.5853017785865));
#55566=CARTESIAN_POINT('Ctrl Pts',(-0.268049440467267,113.83254837515,11.0498590594206));
#55567=CARTESIAN_POINT('Ctrl Pts',(1.05167590777252,113.99301525548,11.3155545254172));
#55568=CARTESIAN_POINT('Ctrl Pts',(1.97963059763142,114.152178479358,12.2762631522508));
#55569=CARTESIAN_POINT('Ctrl Pts',(2.16066197830282,114.283884205462,13.3658254951479));
#55570=CARTESIAN_POINT('Ctrl Pts',(1.91729199582453,114.388787083235,14.1808658981726));
#55571=CARTESIAN_POINT('Ctrl Pts',(1.56383201925712,114.467258929776,14.7098214424163));
#55572=CARTESIAN_POINT('Ctrl Pts',(1.06937612553001,114.545548434972,15.106750651434));
#55573=CARTESIAN_POINT('Ctrl Pts',(0.0880674350923923,114.675769242385,
15.4999443474628));
#55574=CARTESIAN_POINT('Ctrl Pts',(-1.48032406092335,114.857458116598,15.136031750719));
#55575=CARTESIAN_POINT('Ctrl Pts',(-2.36364916409543,115.090577643069,13.2617837519454));
#55576=CARTESIAN_POINT('Ctrl Pts',(-1.41999948256334,115.323909352405,11.4092220242003));
#55577=CARTESIAN_POINT('Ctrl Pts',(0.276704728415126,115.51909837237,11.0776209216297));
#55578=CARTESIAN_POINT('Ctrl Pts',(1.41798096900478,115.676045829526,11.6867186331346));
#55579=CARTESIAN_POINT('Ctrl Pts',(1.99212556085894,115.794234887173,12.4688047031807));
#55580=CARTESIAN_POINT('Ctrl Pts',(2.16558594653818,115.912987530482,13.4308859837738));
#55581=CARTESIAN_POINT('Ctrl Pts',(1.89914709254908,116.032384467474,14.3755069859774));
#55582=CARTESIAN_POINT('Ctrl Pts',(1.24190208921908,116.15250061657,15.1130909726311));
#55583=CARTESIAN_POINT('Ctrl Pts',(0.321991746035035,116.273413589914,15.4906754082313));
#55584=CARTESIAN_POINT('Ctrl Pts',(-0.677026494207119,116.395204792873,
15.4266519625457));
#55585=CARTESIAN_POINT('Ctrl Pts',(-1.55530610398315,116.517924093635,14.9272477572735));
#55586=CARTESIAN_POINT('Ctrl Pts',(-2.12698281028479,116.641673038203,14.0879076641644));
#55587=CARTESIAN_POINT('Ctrl Pts',(-2.33489609979927,116.80804945829,12.7329667674113));
#55588=CARTESIAN_POINT('Ctrl Pts',(-1.38789615116117,117.019100433844,11.1193618885948));
#55589=CARTESIAN_POINT('Ctrl Pts',(0.5005794552031,117.233747585235,10.8642497227967));
#55590=CARTESIAN_POINT('Ctrl Pts',(1.73170137479832,117.409202925543,11.6341898238695));
#55591=CARTESIAN_POINT('Ctrl Pts',(2.10878616139645,117.49705894903,12.2213220005316));
#55592=CARTESIAN_POINT('Ctrl Pts',(2.23495201085903,117.542127618376,12.575258007503));
#55593=CARTESIAN_POINT('Ctrl Pts',(1.99510634103008,110.564595312929,11.7916057212239));
#55594=CARTESIAN_POINT('Ctrl Pts',(2.44140045927379,110.660939813437,12.4221568251609));
#55595=CARTESIAN_POINT('Ctrl Pts',(2.67785200637898,110.848606766051,14.0762814842097));
#55596=CARTESIAN_POINT('Ctrl Pts',(0.994529598795843,111.120688892391,15.8123844880218));
#55597=CARTESIAN_POINT('Ctrl Pts',(-1.32441119517955,111.38275074297,15.5627564509884));
#55598=CARTESIAN_POINT('Ctrl Pts',(-2.38383696994232,111.608918670085,13.8613202078201));
#55599=CARTESIAN_POINT('Ctrl Pts',(-2.06714176232395,111.80214302808,12.2683087846484));
#55600=CARTESIAN_POINT('Ctrl Pts',(-1.09654722271593,111.96471607165,11.3132219749825));
#55601=CARTESIAN_POINT('Ctrl Pts',(0.115349018314891,112.111098413124,11.1029936392051));
#55602=CARTESIAN_POINT('Ctrl Pts',(1.1240981179577,112.242207191303,11.4798259663788));
#55603=CARTESIAN_POINT('Ctrl Pts',(2.01279095222846,112.397622007389,12.4032468147681));
#55604=CARTESIAN_POINT('Ctrl Pts',(2.10271586198826,112.518531833778,13.4673066760386));
#55605=CARTESIAN_POINT('Ctrl Pts',(1.82215720084688,112.606641340562,14.1165282042701));
#55606=CARTESIAN_POINT('Ctrl Pts',(1.72895001174359,112.6317735746,14.2952389561282));
#55607=CARTESIAN_POINT('Ctrl Pts',(1.63004838700809,112.65370851509,14.4412891733214));
#55608=CARTESIAN_POINT('Ctrl Pts',(1.53441570734393,112.672471173608,14.557406431629));
#55609=CARTESIAN_POINT('Ctrl Pts',(1.46782599376371,112.684969891422,14.6322966598098));
#55610=CARTESIAN_POINT('Ctrl Pts',(1.37948695664889,112.700574387516,14.7209901787116));
#55611=CARTESIAN_POINT('Ctrl Pts',(1.28485222984041,112.71615514115,14.8026403743885));
#55612=CARTESIAN_POINT('Ctrl Pts',(1.20570431579963,112.72860515094,14.863473550061));
#55613=CARTESIAN_POINT('Ctrl Pts',(1.05661016915688,112.751413369165,14.9693562317397));
#55614=CARTESIAN_POINT('Ctrl Pts',(0.683260650246095,112.804155576505,15.1724738049531));
#55615=CARTESIAN_POINT('Ctrl Pts',(0.221405329062661,112.861730127325,15.26414659149));
#55616=CARTESIAN_POINT('Ctrl Pts',(-0.172368147512368,112.910861404517,
15.2420427732535));
#55617=CARTESIAN_POINT('Ctrl Pts',(-0.431604041690608,112.943556154848,
15.2012517134772));
#55618=CARTESIAN_POINT('Ctrl Pts',(-0.744676741458043,112.984324215706,
15.1018668945781));
#55619=CARTESIAN_POINT('Ctrl Pts',(-1.08785627052756,113.033089351621,14.9104534389022));
#55620=CARTESIAN_POINT('Ctrl Pts',(-1.48385215265151,113.09790860835,14.5701048300693));
#55621=CARTESIAN_POINT('Ctrl Pts',(-1.90471221137466,113.194730878618,13.898745926889));
#55622=CARTESIAN_POINT('Ctrl Pts',(-1.96400765184658,113.323035009261,12.8240248279844));
#55623=CARTESIAN_POINT('Ctrl Pts',(-1.33461090341178,113.466590122495,11.7964026481919));
#55624=CARTESIAN_POINT('Ctrl Pts',(-0.237365952908544,113.609627110298,
11.3098679793932));
#55625=CARTESIAN_POINT('Ctrl Pts',(0.940224333989188,113.752418856088,11.532060910466));
#55626=CARTESIAN_POINT('Ctrl Pts',(1.78363562158095,113.895244109902,12.3843516573639));
#55627=CARTESIAN_POINT('Ctrl Pts',(1.95938303179607,114.014525670079,13.369475315738));
#55628=CARTESIAN_POINT('Ctrl Pts',(1.7451507182493,114.110245716165,14.1158221589119));
#55629=CARTESIAN_POINT('Ctrl Pts',(1.42596446490531,114.182218366739,14.6044796902011));
#55630=CARTESIAN_POINT('Ctrl Pts',(0.973616447220085,114.254405444024,14.9752757493749));
#55631=CARTESIAN_POINT('Ctrl Pts',(0.0675830023462311,114.375130593489,
15.3490991491701));
#55632=CARTESIAN_POINT('Ctrl Pts',(-1.40766698895308,114.545456563225,15.0270432156924));
#55633=CARTESIAN_POINT('Ctrl Pts',(-2.27332126364622,114.767874491383,13.2495657073064));
#55634=CARTESIAN_POINT('Ctrl Pts',(-1.378448603385,114.994549655149,11.4377635865502));
#55635=CARTESIAN_POINT('Ctrl Pts',(0.296967015967595,115.187629374578,11.0908552711301));
#55636=CARTESIAN_POINT('Ctrl Pts',(1.44649505069631,115.34496676792,11.6926479798579));
#55637=CARTESIAN_POINT('Ctrl Pts',(2.03298894119462,115.464486013225,12.4793992978305));
#55638=CARTESIAN_POINT('Ctrl Pts',(2.21698208494551,115.585602524672,13.4595514025747));
#55639=CARTESIAN_POINT('Ctrl Pts',(1.94948292423316,115.708389485485,14.433054166004));
#55640=CARTESIAN_POINT('Ctrl Pts',(1.27295386489257,115.832911046977,15.202210395537));
#55641=CARTESIAN_POINT('Ctrl Pts',(0.314171425690885,115.959231772748,15.6026400604184));
#55642=CARTESIAN_POINT('Ctrl Pts',(-0.7378322818176,116.087412080197,15.541323560538));
#55643=CARTESIAN_POINT('Ctrl Pts',(-1.67178863712833,116.217493756747,15.0171316753708));
#55644=CARTESIAN_POINT('Ctrl Pts',(-2.28659522816475,116.349528456984,14.1243699909755));
#55645=CARTESIAN_POINT('Ctrl Pts',(-2.51688203564877,116.52822974892,12.6709046541834));
#55646=CARTESIAN_POINT('Ctrl Pts',(-1.50311340794689,116.756672499734,10.9153049327907));
#55647=CARTESIAN_POINT('Ctrl Pts',(0.564751367180597,116.991983982712,10.6258923511469));
#55648=CARTESIAN_POINT('Ctrl Pts',(1.92115389036661,117.184628932805,11.4661899786458));
#55649=CARTESIAN_POINT('Ctrl Pts',(2.34344901183535,117.282518109478,12.1187945864147));
#55650=CARTESIAN_POINT('Ctrl Pts',(2.48212919172115,117.331688649487,12.5041410339076));
#55651=CARTESIAN_POINT('Ctrl Pts',(2.02616441126019,110.570072536149,11.8332575276011));
#55652=CARTESIAN_POINT('Ctrl Pts',(2.07105841806764,110.5799782663,11.8994551216819));
#55653=CARTESIAN_POINT('Ctrl Pts',(2.11271517883406,110.589880303591,11.9677392355203));
#55654=CARTESIAN_POINT('Ctrl Pts',(2.150854785792,110.599777995315,12.0378250846901));
#55655=CARTESIAN_POINT('Ctrl Pts',(2.21680176610504,110.616892038519,12.1590101330969));
#55656=CARTESIAN_POINT('Ctrl Pts',(2.2722299692091,110.633993066787,12.2855838404137));
#55657=CARTESIAN_POINT('Ctrl Pts',(2.31677087589169,110.651078126608,12.4156052564564));
#55658=CARTESIAN_POINT('Ctrl Pts',(2.36131178257429,110.66816318643,12.5456266724991));
#55659=CARTESIAN_POINT('Ctrl Pts',(2.39496518711439,110.685232280206,12.679094248793));
#55660=CARTESIAN_POINT('Ctrl Pts',(2.41741513700149,110.702282852658,12.8140429117563));
#55661=CARTESIAN_POINT('Ctrl Pts',(2.43988375218285,110.719347601265,12.949103773478));
#55662=CARTESIAN_POINT('Ctrl Pts',(2.45113018384618,110.736393800202,13.0856466048275));
#55663=CARTESIAN_POINT('Ctrl Pts',(2.45108056364822,110.753419241551,13.2216340677291));
#55664=CARTESIAN_POINT('Ctrl Pts',(2.4510338049192,110.76946286957,13.3497794840631));
#55665=CARTESIAN_POINT('Ctrl Pts',(2.44095668751521,110.785488069839,13.4774306472446));
#55666=CARTESIAN_POINT('Ctrl Pts',(2.42083288203555,110.80149325887,13.6029010654533));
#55667=CARTESIAN_POINT('Ctrl Pts',(2.41960137626499,110.802472719871,13.6105794115899));
#55668=CARTESIAN_POINT('Ctrl Pts',(2.41833225938017,110.803452106003,13.618249599689));
#55669=CARTESIAN_POINT('Ctrl Pts',(2.41702553304493,110.804431416933,13.6259112469578));
#55670=CARTESIAN_POINT('Ctrl Pts',(2.39711608043204,110.819352325794,13.7426451024876));
#55671=CARTESIAN_POINT('Ctrl Pts',(2.36847436955913,110.834255763845,13.8573939856762));
#55672=CARTESIAN_POINT('Ctrl Pts',(2.33187245113042,110.849140695019,13.9690689169625));
#55673=CARTESIAN_POINT('Ctrl Pts',(2.29493346737928,110.864162700815,14.0817722573688));
#55674=CARTESIAN_POINT('Ctrl Pts',(2.24971683798023,110.879122738555,14.1917657288957));
#55675=CARTESIAN_POINT('Ctrl Pts',(2.19688540562185,110.894023372537,14.2978493398295));
#55676=CARTESIAN_POINT('Ctrl Pts',(2.14287094573794,110.909257668874,14.4063084273715));
#55677=CARTESIAN_POINT('Ctrl Pts',(2.08089735143869,110.924429872065,14.5106795218075));
#55678=CARTESIAN_POINT('Ctrl Pts',(2.01172744446461,110.939543288332,14.609689996179));
#55679=CARTESIAN_POINT('Ctrl Pts',(1.94246035028488,110.954677939709,14.7088395852574));
#55680=CARTESIAN_POINT('Ctrl Pts',(1.86597744060666,110.969753642001,14.8026124080882));
#55681=CARTESIAN_POINT('Ctrl Pts',(1.78308899230302,110.984774243601,14.8897563710569));
#55682=CARTESIAN_POINT('Ctrl Pts',(1.74400542036187,110.991856759624,14.9308465038273));
#55683=CARTESIAN_POINT('Ctrl Pts',(1.70349826534003,110.998927032353,14.9704633071913));
#55684=CARTESIAN_POINT('Ctrl Pts',(1.66165516189832,111.005985502709,15.0084785524507));
#55685=CARTESIAN_POINT('Ctrl Pts',(1.57189245452912,111.021127482077,15.0900296577731));
#55686=CARTESIAN_POINT('Ctrl Pts',(1.47598082711947,111.036215118535,15.1642072274403));
#55687=CARTESIAN_POINT('Ctrl Pts',(1.37535440147532,111.051253158905,15.2305278229256));
#55688=CARTESIAN_POINT('Ctrl Pts',(1.27713452752472,111.065931553971,15.2952623147571));
#55689=CARTESIAN_POINT('Ctrl Pts',(1.17442386833893,111.080562702085,15.3525109927783));
#55690=CARTESIAN_POINT('Ctrl Pts',(1.06856206414412,111.095151398066,15.4018724805979));
#55691=CARTESIAN_POINT('Ctrl Pts',(1.00819936982575,111.103469912971,15.4300185378375));
#55692=CARTESIAN_POINT('Ctrl Pts',(0.946812152352576,111.111774631939,15.4556011230402));
#55693=CARTESIAN_POINT('Ctrl Pts',(0.884647485524478,111.1200664917,15.4785533978928));
#55694=CARTESIAN_POINT('Ctrl Pts',(0.778155140070371,111.134271017184,15.5178722217082));
#55695=CARTESIAN_POINT('Ctrl Pts',(0.668870322291868,111.148439910411,15.5496459177179));
#55696=CARTESIAN_POINT('Ctrl Pts',(0.557997038053399,111.162573434211,15.573352552203));
#55697=CARTESIAN_POINT('Ctrl Pts',(0.454890603246509,111.175716882249,15.5953984993381));
#55698=CARTESIAN_POINT('Ctrl Pts',(0.350411649690433,111.188829748195,15.6104681156522));
#55699=CARTESIAN_POINT('Ctrl Pts',(0.245551686144082,111.201912534831,15.6181747144393));
#55700=CARTESIAN_POINT('Ctrl Pts',(0.132554486325984,111.216010558572,15.6264793528695));
#55701=CARTESIAN_POINT('Ctrl Pts',(0.0191157451671066,111.230073651892,
15.6262326699005));
#55702=CARTESIAN_POINT('Ctrl Pts',(-0.0934940464264922,111.244102823594,
15.6177560420854));
#55703=CARTESIAN_POINT('Ctrl Pts',(-0.207107639837214,111.2582570511,15.6092038537503));
#55704=CARTESIAN_POINT('Ctrl Pts',(-0.319876196950842,111.272376752,15.5922746446226));
#55705=CARTESIAN_POINT('Ctrl Pts',(-0.430499467262996,111.286463273381,
15.5673513736807));
#55706=CARTESIAN_POINT('Ctrl Pts',(-0.538949137192655,111.30027301332,15.5429178119211));
#55707=CARTESIAN_POINT('Ctrl Pts',(-0.645335908803491,111.314050868474,
15.5108017573914));
#55708=CARTESIAN_POINT('Ctrl Pts',(-0.748456234475894,111.327798357861,
15.4714082566281));
#55709=CARTESIAN_POINT('Ctrl Pts',(-0.792969010146538,111.333732579919,
15.4544037131405));
#55710=CARTESIAN_POINT('Ctrl Pts',(-0.836873522602974,111.339661146824,
15.4360436907805));
#55711=CARTESIAN_POINT('Ctrl Pts',(-0.880075005513976,111.345584192991,
15.4163630345393));
#55712=CARTESIAN_POINT('Ctrl Pts',(-0.967742555981023,111.357603663475,
15.3764256340614));
#55713=CARTESIAN_POINT('Ctrl Pts',(-1.05251344069536,111.369600393746,15.3310492160238));
#55714=CARTESIAN_POINT('Ctrl Pts',(-1.13381079222952,111.381575608866,15.2808146713564));
#55715=CARTESIAN_POINT('Ctrl Pts',(-1.23687530433488,111.396757157592,15.2171299542127));
#55716=CARTESIAN_POINT('Ctrl Pts',(-1.33483881624213,111.411901639041,15.1453343047575));
#55717=CARTESIAN_POINT('Ctrl Pts',(-1.42644767653091,111.427007716472,15.0664071530192));
#55718=CARTESIAN_POINT('Ctrl Pts',(-1.52183861320501,111.442737449066,14.9842214898682));
#55719=CARTESIAN_POINT('Ctrl Pts',(-1.61033830423551,111.458425541663,14.8943038098277));
#55720=CARTESIAN_POINT('Ctrl Pts',(-1.69054419706743,111.474070759423,14.7978142078287));
#55721=CARTESIAN_POINT('Ctrl Pts',(-1.71359526602133,111.478567174595,14.7700832221058));
#55722=CARTESIAN_POINT('Ctrl Pts',(-1.73596141980438,111.483060050031,14.7418097120366));
#55723=CARTESIAN_POINT('Ctrl Pts',(-1.75760974856578,111.487549360252,14.7130219020379));
#55724=CARTESIAN_POINT('Ctrl Pts',(-1.83337735574986,111.503261625946,14.6122666195535));
#55725=CARTESIAN_POINT('Ctrl Pts',(-1.900348686991,111.518930202763,14.5052088222496));
#55726=CARTESIAN_POINT('Ctrl Pts',(-1.95788793805633,111.534554187242,14.3936106861671));
#55727=CARTESIAN_POINT('Ctrl Pts',(-2.01516628970205,111.550107328108,14.2825185679489));
#55728=CARTESIAN_POINT('Ctrl Pts',(-2.06309747735693,111.565616282983,14.1669285606128));
#55729=CARTESIAN_POINT('Ctrl Pts',(-2.10109971794726,111.581080353661,14.0486007782592));
#55730=CARTESIAN_POINT('Ctrl Pts',(-2.13867283810188,111.596369804405,13.9316091505303));
#55731=CARTESIAN_POINT('Ctrl Pts',(-2.16653964038307,111.611615381789,13.8119425199339));
#55732=CARTESIAN_POINT('Ctrl Pts',(-2.18418791701896,111.626816556935,13.6913036358071));
#55733=CARTESIAN_POINT('Ctrl Pts',(-2.18759336745963,111.629749809267,13.6680248902622));
#55734=CARTESIAN_POINT('Ctrl Pts',(-2.19061849851063,111.632681408674,13.6447099149796));
#55735=CARTESIAN_POINT('Ctrl Pts',(-2.19326586556019,111.635611352551,13.62137083067));
#55736=CARTESIAN_POINT('Ctrl Pts',(-2.20853875159818,111.652514448384,13.4867256650321));
#55737=CARTESIAN_POINT('Ctrl Pts',(-2.21127460479025,111.669401214344,13.3509280781189));
#55738=CARTESIAN_POINT('Ctrl Pts',(-2.20180594533087,111.686258620309,13.2162593571699));
#55739=CARTESIAN_POINT('Ctrl Pts',(-2.19192191780219,111.703855521469,13.0756830326308));
#55740=CARTESIAN_POINT('Ctrl Pts',(-2.16873902135966,111.721420426645,12.9363382358816));
#55741=CARTESIAN_POINT('Ctrl Pts',(-2.13268966365534,111.738938750505,12.8008348741085));
#55742=CARTESIAN_POINT('Ctrl Pts',(-2.11529365920093,111.747392405697,12.7354462726159));
#55743=CARTESIAN_POINT('Ctrl Pts',(-2.09490230517816,111.755835217512,12.6709522842583));
#55744=CARTESIAN_POINT('Ctrl Pts',(-2.07156848851267,111.764265569171,12.6076457448401));
#55745=CARTESIAN_POINT('Ctrl Pts',(-2.03725839797215,111.776661575057,12.5145596830789));
#55746=CARTESIAN_POINT('Ctrl Pts',(-1.99658601558772,111.789030637564,12.4240413943406));
#55747=CARTESIAN_POINT('Ctrl Pts',(-1.95009563404642,111.801367552442,12.3368816460376));
#55748=CARTESIAN_POINT('Ctrl Pts',(-1.91126430847799,111.811672022791,12.2640810268427));
#55749=CARTESIAN_POINT('Ctrl Pts',(-1.86836584858189,111.821954361973,12.1936062082923));
#55750=CARTESIAN_POINT('Ctrl Pts',(-1.82171032815555,111.832216330656,12.1259096426039));
#55751=CARTESIAN_POINT('Ctrl Pts',(-1.71916930753833,111.854770419276,11.9771239281903));
#55752=CARTESIAN_POINT('Ctrl Pts',(-1.5984785936281,111.877226132562,11.8417605416273));
#55753=CARTESIAN_POINT('Ctrl Pts',(-1.46349508310159,111.899604249647,11.7238186713924));
#55754=CARTESIAN_POINT('Ctrl Pts',(-1.33345583594095,111.921162686579,11.6101968522957));
#55755=CARTESIAN_POINT('Ctrl Pts',(-1.19015285597994,111.942649116998,11.5127440729284));
#55756=CARTESIAN_POINT('Ctrl Pts',(-1.03799495393243,111.964078910758,11.4339687121288));
#55757=CARTESIAN_POINT('Ctrl Pts',(-1.03212606544161,111.964905480185,11.4309302645547));
#55758=CARTESIAN_POINT('Ctrl Pts',(-1.02624347565069,111.965731969523,11.4279193094611));
#55759=CARTESIAN_POINT('Ctrl Pts',(-1.02034743996064,111.966558377551,11.424936009145));
#55760=CARTESIAN_POINT('Ctrl Pts',(-0.914279455406906,111.981425220029,
11.3712672953711));
#55761=CARTESIAN_POINT('Ctrl Pts',(-0.803856893658385,111.996265733511,
11.3265518361342));
#55762=CARTESIAN_POINT('Ctrl Pts',(-0.690702167200723,112.01107401304,11.2913328576768));
#55763=CARTESIAN_POINT('Ctrl Pts',(-0.63469380078121,112.018403689597,11.273900466542));
#55764=CARTESIAN_POINT('Ctrl Pts',(-0.57801663387521,112.025725471586,11.2587940617592));
#55765=CARTESIAN_POINT('Ctrl Pts',(-0.520869988068662,112.033038657505,
11.2460756243719));
#55766=CARTESIAN_POINT('Ctrl Pts',(-0.434661659822516,112.044070932863,
11.2268892800188));
#55767=CARTESIAN_POINT('Ctrl Pts',(-0.347384900232451,112.055083644211,
11.2131379985066));
#55768=CARTESIAN_POINT('Ctrl Pts',(-0.259754285009278,112.066074050324,
11.2048613130971));
#55769=CARTESIAN_POINT('Ctrl Pts',(-0.172104732923932,112.077066831449,
11.1965828391066));
#55770=CARTESIAN_POINT('Ctrl Pts',(-0.0841014946280306,112.088037297831,
11.1937813409176));
#55771=CARTESIAN_POINT('Ctrl Pts',(0.0035241847171541,112.098982505872,
11.1964691503483));
#55772=CARTESIAN_POINT('Ctrl Pts',(0.070833532300197,112.107390027706,11.1985337814081));
#55773=CARTESIAN_POINT('Ctrl Pts',(0.137920067271792,112.115782646876,11.2038370278667));
#55774=CARTESIAN_POINT('Ctrl Pts',(0.204476565983255,112.124159351449,11.2123021908646));
#55775=CARTESIAN_POINT('Ctrl Pts',(0.311391191145362,112.137615471391,11.2259004081141));
#55776=CARTESIAN_POINT('Ctrl Pts',(0.41701049350247,112.151091212913,11.2476786332973));
#55777=CARTESIAN_POINT('Ctrl Pts',(0.52015968341684,112.164555091108,11.277359160353));
#55778=CARTESIAN_POINT('Ctrl Pts',(0.641972232071245,112.180455063944,11.3124099508543));
#55779=CARTESIAN_POINT('Ctrl Pts',(0.760341260980355,112.196338439093,11.3584803657846));
#55780=CARTESIAN_POINT('Ctrl Pts',(0.873367208190062,112.212153314227,11.414744343162));
#55781=CARTESIAN_POINT('Ctrl Pts',(0.915519447094673,112.218051361634,11.4357276012074));
#55782=CARTESIAN_POINT('Ctrl Pts',(0.956928340724595,112.22393989858,11.4581291137113));
#55783=CARTESIAN_POINT('Ctrl Pts',(0.997494416208606,112.229816296784,11.4819076757352));
#55784=CARTESIAN_POINT('Ctrl Pts',(1.02723895372284,112.234125087928,11.4993429913707));
#55785=CARTESIAN_POINT('Ctrl Pts',(1.05653034425799,112.238427353575,11.5175186823741));
#55786=CARTESIAN_POINT('Ctrl Pts',(1.0853496526665,112.24272208655,11.5364004717887));
#55787=CARTESIAN_POINT('Ctrl Pts',(1.12874878866787,112.24918954572,11.5648346498451));
#55788=CARTESIAN_POINT('Ctrl Pts',(1.17108400605649,112.255635802411,11.5948729432256));
#55789=CARTESIAN_POINT('Ctrl Pts',(1.21226984262544,112.262062150019,11.6263868296338));
#55790=CARTESIAN_POINT('Ctrl Pts',(1.28075499720787,112.27274809077,11.6787891495076));
#55791=CARTESIAN_POINT('Ctrl Pts',(1.34606065426729,112.283378992512,11.7352730013004));
#55792=CARTESIAN_POINT('Ctrl Pts',(1.40709547802075,112.293960799461,11.7956640737622));
#55793=CARTESIAN_POINT('Ctrl Pts',(1.47358143037869,112.305487686398,11.8614487802562));
#55794=CARTESIAN_POINT('Ctrl Pts',(1.53499864940514,112.316956325139,11.9318693556024));
#55795=CARTESIAN_POINT('Ctrl Pts',(1.59110341104185,112.328373946553,12.0059858413882));
#55796=CARTESIAN_POINT('Ctrl Pts',(1.6400490793677,112.338334653889,12.070644897499));
#55797=CARTESIAN_POINT('Ctrl Pts',(1.68495205813288,112.348256530576,12.1381157758824));
#55798=CARTESIAN_POINT('Ctrl Pts',(1.72568000847627,112.35814416662,12.2077610316259));
#55799=CARTESIAN_POINT('Ctrl Pts',(1.79993921911069,112.376172278554,12.3347451217247));
#55800=CARTESIAN_POINT('Ctrl Pts',(1.86059771124178,112.394452726721,12.4696551328169));
#55801=CARTESIAN_POINT('Ctrl Pts',(1.90679617182559,112.412832166683,12.6090877257604));
#55802=CARTESIAN_POINT('Ctrl Pts',(1.95492570256377,112.431979857092,12.7543485241327));
#55803=CARTESIAN_POINT('Ctrl Pts',(1.98736213974189,112.451234856573,12.904514998465));
#55804=CARTESIAN_POINT('Ctrl Pts',(2.00319042751117,112.470431295237,13.0557422024043));
#55805=CARTESIAN_POINT('Ctrl Pts',(2.01850854964172,112.48900900852,13.2020951632027));
#55806=CARTESIAN_POINT('Ctrl Pts',(2.01827389738594,112.50753184538,13.3494399658853));
#55807=CARTESIAN_POINT('Ctrl Pts',(2.00168493092275,112.525857411218,13.4943278262554));
#55808=CARTESIAN_POINT('Ctrl Pts',(1.99504403705843,112.533193500419,13.5523293241235));
#55809=CARTESIAN_POINT('Ctrl Pts',(1.98578241830288,112.540498069348,13.6099376212333));
#55810=CARTESIAN_POINT('Ctrl Pts',(1.97384878709611,112.547762372644,13.6669338487352));
#55811=CARTESIAN_POINT('Ctrl Pts',(1.95170130268851,112.561244106845,13.7727124703485));
#55812=CARTESIAN_POINT('Ctrl Pts',(1.92035116401533,112.57458697814,13.8763818579387));
#55813=CARTESIAN_POINT('Ctrl Pts',(1.88079178001759,112.587737377759,13.9768971580619));
#55814=CARTESIAN_POINT('Ctrl Pts',(1.86229565658681,112.593885891461,14.0238934256951));
#55815=CARTESIAN_POINT('Ctrl Pts',(1.84199429112812,112.600024904622,14.0701690994365));
#55816=CARTESIAN_POINT('Ctrl Pts',(1.82003100565933,112.606132195475,14.1155636062622));
#55817=CARTESIAN_POINT('Ctrl Pts',(1.79806772019048,112.612239486328,14.160958113088));
#55818=CARTESIAN_POINT('Ctrl Pts',(1.77444697332014,112.618315383671,14.2054667607652));
#55819=CARTESIAN_POINT('Ctrl Pts',(1.7492409607065,112.624417619916,14.2489991213253));
#55820=CARTESIAN_POINT('Ctrl Pts',(1.69882893547932,112.636622092406,14.3360638424454));
#55821=CARTESIAN_POINT('Ctrl Pts',(1.64207244780588,112.648932109483,14.4192317980716));
#55822=CARTESIAN_POINT('Ctrl Pts',(1.57976552279001,112.661382636358,14.4977141891418));
#55823=CARTESIAN_POINT('Ctrl Pts',(1.56418879153601,112.664495268077,14.5173347869093));
#55824=CARTESIAN_POINT('Ctrl Pts',(1.54826497583986,112.667616660155,14.5366624552061));
#55825=CARTESIAN_POINT('Ctrl Pts',(1.53200277927876,112.670748758568,14.5556873852558));
#55826=CARTESIAN_POINT('Ctrl Pts',(1.51574058271771,112.673880856982,14.5747123153055));
#55827=CARTESIAN_POINT('Ctrl Pts',(1.49913994586673,112.677023645936,14.5934345229931));
#55828=CARTESIAN_POINT('Ctrl Pts',(1.48221260175302,112.680176475423,14.6118418109419));
#55829=CARTESIAN_POINT('Ctrl Pts',(1.44835791352547,112.686482134398,14.6486563868397));
#55830=CARTESIAN_POINT('Ctrl Pts',(1.41319659887146,112.69282812446,14.6842116298549));
#55831=CARTESIAN_POINT('Ctrl Pts',(1.37681223588142,112.699211097522,14.7184142822241));
#55832=CARTESIAN_POINT('Ctrl Pts',(1.34042787289152,112.705594070583,14.7526169345931));
#55833=CARTESIAN_POINT('Ctrl Pts',(1.30282015964494,112.712014031624,14.7854671449969));
#55834=CARTESIAN_POINT('Ctrl Pts',(1.26407541691761,112.718458396915,14.8168681460656));
#55835=CARTESIAN_POINT('Ctrl Pts',(1.24470304555387,112.721680579561,14.8325686465999));
#55836=CARTESIAN_POINT('Ctrl Pts',(1.2250464318216,112.724908824614,14.8479067314702));
#55837=CARTESIAN_POINT('Ctrl Pts',(1.20511700835775,112.728141268808,14.8628693722048));
#55838=CARTESIAN_POINT('Ctrl Pts',(1.1851875848939,112.731373713001,14.8778320129395));
#55839=CARTESIAN_POINT('Ctrl Pts',(1.16498534336991,112.734610366165,14.8924192263057));
#55840=CARTESIAN_POINT('Ctrl Pts',(1.14452107077328,112.737848258061,14.9066191521569));
#55841=CARTESIAN_POINT('Ctrl Pts',(1.07551966046412,112.748765778155,14.9544984454665));
#55842=CARTESIAN_POINT('Ctrl Pts',(1.00351907227778,112.759699351886,14.9979865816682));
#55843=CARTESIAN_POINT('Ctrl Pts',(0.929049646054122,112.770470348169,15.0365818477437));
#55844=CARTESIAN_POINT('Ctrl Pts',(0.885727266263003,112.77673634504,15.059034535509));
#55845=CARTESIAN_POINT('Ctrl Pts',(0.841568966091264,112.782947462598,15.0798321837866));
#55846=CARTESIAN_POINT('Ctrl Pts',(0.796674188449058,112.789069756842,15.0988824177858));
#55847=CARTESIAN_POINT('Ctrl Pts',(0.776887372027841,112.791768082095,15.1072785721432));
#55848=CARTESIAN_POINT('Ctrl Pts',(0.756966200111399,112.794453444134,15.1153273887977));
#55849=CARTESIAN_POINT('Ctrl Pts',(0.736918996296125,112.797127253964,15.1230191201535));
#55850=CARTESIAN_POINT('Ctrl Pts',(0.645860534818585,112.809272239949,15.1579565223873));
#55851=CARTESIAN_POINT('Ctrl Pts',(0.552198065392748,112.821179417709,15.1855252225106));
#55852=CARTESIAN_POINT('Ctrl Pts',(0.45708651516146,112.832977001361,15.2058637026304));
#55853=CARTESIAN_POINT('Ctrl Pts',(0.363501094122257,112.844585284799,15.2258758380722));
#55854=CARTESIAN_POINT('Ctrl Pts',(0.268513439141321,112.856087470962,15.238886823475));
#55855=CARTESIAN_POINT('Ctrl Pts',(0.173264500148235,112.867599127254,15.2450567386434));
#55856=CARTESIAN_POINT('Ctrl Pts',(0.123678453456399,112.873592028933,15.2482687607914));
#55857=CARTESIAN_POINT('Ctrl Pts',(0.0740222107504112,112.879587387402,
15.2496272954867));
#55858=CARTESIAN_POINT('Ctrl Pts',(0.0244600145184373,112.885600776115,
15.2491594789169));
#55859=CARTESIAN_POINT('Ctrl Pts',(-0.0412455943053918,112.893572847501,
15.2485392850015));
#55860=CARTESIAN_POINT('Ctrl Pts',(-0.106844975386639,112.901622991693,
15.2446804600296));
#55861=CARTESIAN_POINT('Ctrl Pts',(-0.172029570959803,112.909741286633,
15.2376655680879));
#55862=CARTESIAN_POINT('Ctrl Pts',(-0.237214166532639,112.917859581573,
15.2306506761462));
#55863=CARTESIAN_POINT('Ctrl Pts',(-0.301982877658334,112.926046223778,
15.2204802566568));
#55864=CARTESIAN_POINT('Ctrl Pts',(-0.366044349703285,112.934319107027,
15.2071971382874));
#55865=CARTESIAN_POINT('Ctrl Pts',(-0.4498680025377,112.945144073599,15.1898163403256));
#55866=CARTESIAN_POINT('Ctrl Pts',(-0.532491721702338,112.9561206548,15.1671022838396));
#55867=CARTESIAN_POINT('Ctrl Pts',(-0.613238339944968,112.967172236378,
15.1391944730737));
#55868=CARTESIAN_POINT('Ctrl Pts',(-0.655911473821721,112.973012798255,
15.1244456975716));
#55869=CARTESIAN_POINT('Ctrl Pts',(-0.698060521253093,112.978874378959,
15.1082455289309));
#55870=CARTESIAN_POINT('Ctrl Pts',(-0.739585621711384,112.984746166875,
15.0906086159743));
#55871=CARTESIAN_POINT('Ctrl Pts',(-0.805721120318868,112.994097947298,
15.0625189540733));
#55872=CARTESIAN_POINT('Ctrl Pts',(-0.870421140646448,113.003273205557,
15.0309142321559));
#55873=CARTESIAN_POINT('Ctrl Pts',(-0.933111481160008,113.012360497,14.995775707463));
#55874=CARTESIAN_POINT('Ctrl Pts',(-0.984264268635237,113.019775360025,
14.9671040896176));
#55875=CARTESIAN_POINT('Ctrl Pts',(-1.03407813945666,113.027131583293,14.9360802842284));
#55876=CARTESIAN_POINT('Ctrl Pts',(-1.0822286157556,113.034475136326,14.9027164917897));
#55877=CARTESIAN_POINT('Ctrl Pts',(-1.09551238897994,113.03650107876,14.8935120749962));
#55878=CARTESIAN_POINT('Ctrl Pts',(-1.10866659778872,113.038526765791,14.884130539298));
#55879=CARTESIAN_POINT('Ctrl Pts',(-1.12168576942057,113.040551140475,14.8745739213863));
#55880=CARTESIAN_POINT('Ctrl Pts',(-1.18082309055915,113.04974651013,14.8311646478608));
#55881=CARTESIAN_POINT('Ctrl Pts',(-1.23717002182144,113.058914423756,14.7841428010402));
#55882=CARTESIAN_POINT('Ctrl Pts',(-1.29056167062862,113.067958734826,14.7340613357618));
#55883=CARTESIAN_POINT('Ctrl Pts',(-1.32023833118964,113.072985830928,14.7062245732967));
#55884=CARTESIAN_POINT('Ctrl Pts',(-1.34900291901271,113.077974825316,14.6774426155162));
#55885=CARTESIAN_POINT('Ctrl Pts',(-1.37683398123715,113.082909852143,14.6478095523937));
#55886=CARTESIAN_POINT('Ctrl Pts',(-1.43576652310271,113.093359818902,14.5850612562996));
#55887=CARTESIAN_POINT('Ctrl Pts',(-1.49037860544055,113.103700466767,14.518454453204));
#55888=CARTESIAN_POINT('Ctrl Pts',(-1.5403799994995,113.11404766848,14.4486413038854));
#55889=CARTESIAN_POINT('Ctrl Pts',(-1.59082828366944,113.124487348857,14.3782041958426));
#55890=CARTESIAN_POINT('Ctrl Pts',(-1.63658247480435,113.134933726513,14.3045016220919));
#55891=CARTESIAN_POINT('Ctrl Pts',(-1.67729431638225,113.145498604884,14.2282170002687));
#55892=CARTESIAN_POINT('Ctrl Pts',(-1.71800615796016,113.156063483255,14.1519323784454));
#55893=CARTESIAN_POINT('Ctrl Pts',(-1.75367481419996,113.166746881571,14.0730644726455));
#55894=CARTESIAN_POINT('Ctrl Pts',(-1.78391312089489,113.177653109242,13.9923311803759));
#55895=CARTESIAN_POINT('Ctrl Pts',(-1.81639568597374,113.189368786766,13.9056059398844));
#55896=CARTESIAN_POINT('Ctrl Pts',(-1.84294959853395,113.201151265024,13.8164938284703));
#55897=CARTESIAN_POINT('Ctrl Pts',(-1.86312229070193,113.212953778618,13.7259876268165));
#55898=CARTESIAN_POINT('Ctrl Pts',(-1.88328780697174,113.224752093781,13.6355136203343));
#55899=CARTESIAN_POINT('Ctrl Pts',(-1.89707654058327,113.236570421787,13.5436479245573));
#55900=CARTESIAN_POINT('Ctrl Pts',(-1.90408663867269,113.248364731642,13.4513914373198));
#55901=CARTESIAN_POINT('Ctrl Pts',(-1.9103535641621,113.2589086727,13.3689154827672));
#55902=CARTESIAN_POINT('Ctrl Pts',(-1.91120360612133,113.269433451235,13.2861279371684));
#55903=CARTESIAN_POINT('Ctrl Pts',(-1.90638424863131,113.279909496623,13.2037368741416));
#55904=CARTESIAN_POINT('Ctrl Pts',(-1.90101550237794,113.291579772079,13.1119535374928));
#55905=CARTESIAN_POINT('Ctrl Pts',(-1.88861111438651,113.303189521236,13.0206636313188));
#55906=CARTESIAN_POINT('Ctrl Pts',(-1.8696893135162,113.314700554774,12.930815106266));
#55907=CARTESIAN_POINT('Ctrl Pts',(-1.86421797282472,113.318029032155,12.9048349210521));
#55908=CARTESIAN_POINT('Ctrl Pts',(-1.85820194747901,113.321349274027,12.8789750215176));
#55909=CARTESIAN_POINT('Ctrl Pts',(-1.85165429717006,113.324660401611,12.8532577127581));
#55910=CARTESIAN_POINT('Ctrl Pts',(-1.8139098913597,113.343747637085,12.7050084183747));
#55911=CARTESIAN_POINT('Ctrl Pts',(-1.75815042366791,113.362808373553,12.5612993295427));
#55912=CARTESIAN_POINT('Ctrl Pts',(-1.68647983649764,113.381817099869,12.4262346560924));
#55913=CARTESIAN_POINT('Ctrl Pts',(-1.61509127707076,113.400751025792,12.291701469638));
#55914=CARTESIAN_POINT('Ctrl Pts',(-1.52791766723889,113.419633337063,12.1657437558088));
#55915=CARTESIAN_POINT('Ctrl Pts',(-1.42700095731129,113.438443549802,12.0523818342241));
#55916=CARTESIAN_POINT('Ctrl Pts',(-1.3742256782145,113.448280515631,11.9930982224727));
#55917=CARTESIAN_POINT('Ctrl Pts',(-1.31769115211554,113.458097843159,11.9372588477645));
#55918=CARTESIAN_POINT('Ctrl Pts',(-1.25793332652008,113.467893141606,11.8851505147714));
#55919=CARTESIAN_POINT('Ctrl Pts',(-1.17824342337142,113.480955638053,11.8156615738991));
#55920=CARTESIAN_POINT('Ctrl Pts',(-1.09267156863032,113.494102139066,11.752899313121));
#55921=CARTESIAN_POINT('Ctrl Pts',(-1.00257765073903,113.507273859013,11.6975680362558));
#55922=CARTESIAN_POINT('Ctrl Pts',(-0.912702867067373,113.520413541564,
11.6423713409079));
#55923=CARTESIAN_POINT('Ctrl Pts',(-0.818329378978895,113.53357830804,11.594568740537));
#55924=CARTESIAN_POINT('Ctrl Pts',(-0.72078335804855,113.546715920029,11.5548141484263));
#55925=CARTESIAN_POINT('Ctrl Pts',(-0.624393699727143,113.559697791752,
11.5155308284743));
#55926=CARTESIAN_POINT('Ctrl Pts',(-0.524907134494272,113.57265314922,11.4841048235255));
#55927=CARTESIAN_POINT('Ctrl Pts',(-0.423563428596022,113.585537647891,
11.4611363065296));
#55928=CARTESIAN_POINT('Ctrl Pts',(-0.397189752790417,113.588890708527,
11.4551589819823));
#55929=CARTESIAN_POINT('Ctrl Pts',(-0.370690056589949,113.592239002449,
11.4497543218409));
#55930=CARTESIAN_POINT('Ctrl Pts',(-0.344085649406526,113.595581816386,
11.4449326952993));
#55931=CARTESIAN_POINT('Ctrl Pts',(-0.304309169060675,113.600579686549,
11.4377238395618));
#55932=CARTESIAN_POINT('Ctrl Pts',(-0.264298682867311,113.605565300418,
11.4318182612747));
#55933=CARTESIAN_POINT('Ctrl Pts',(-0.224135251006277,113.61053639555,11.4271969543473));
#55934=CARTESIAN_POINT('Ctrl Pts',(-0.101602384479631,113.625702493368,
11.4130980101415));
#55935=CARTESIAN_POINT('Ctrl Pts',(0.0223203186210237,113.640935225879,
11.411305960043));
#55936=CARTESIAN_POINT('Ctrl Pts',(0.145279970667435,113.656210437031,11.4213565568666));
#55937=CARTESIAN_POINT('Ctrl Pts',(0.273664818503302,113.672159617327,11.4318506036729));
#55938=CARTESIAN_POINT('Ctrl Pts',(0.40100068878535,113.68815506243,11.4552540383412));
#55939=CARTESIAN_POINT('Ctrl Pts',(0.524656749220729,113.704174053909,11.4910735016288));
#55940=CARTESIAN_POINT('Ctrl Pts',(0.648312809656087,113.720193045389,11.5268929649164));
#55941=CARTESIAN_POINT('Ctrl Pts',(0.768290962354242,113.736235570847,11.5751273944758));
#55942=CARTESIAN_POINT('Ctrl Pts',(0.881984751217859,113.752283974349,11.6353358343203));
#55943=CARTESIAN_POINT('Ctrl Pts',(0.882892274744216,113.752412075487,11.6358164285215));
#55944=CARTESIAN_POINT('Ctrl Pts',(0.883799397894364,113.752540177027,11.6362977859758));
#55945=CARTESIAN_POINT('Ctrl Pts',(0.884706119714493,113.752668278962,11.6367799057436));
#55946=CARTESIAN_POINT('Ctrl Pts',(1.0015731765502,113.769179292267,11.6989201532376));
#55947=CARTESIAN_POINT('Ctrl Pts',(1.11180876568798,113.785647483982,11.7736386330667));
#55948=CARTESIAN_POINT('Ctrl Pts',(1.21324751846698,113.802093628618,11.8589369614855));
#55949=CARTESIAN_POINT('Ctrl Pts',(1.31494598569875,113.818581880449,11.9444536798991));
#55950=CARTESIAN_POINT('Ctrl Pts',(1.40780070899976,113.835047985294,12.040604518117));
#55951=CARTESIAN_POINT('Ctrl Pts',(1.489625666257,113.851508552278,12.1453250436702));
#55952=CARTESIAN_POINT('Ctrl Pts',(1.52019706814189,113.85765854154,12.1844506769683));
#55953=CARTESIAN_POINT('Ctrl Pts',(1.54922891015762,113.863807713567,12.2247720616797));
#55954=CARTESIAN_POINT('Ctrl Pts',(1.57660788908141,113.869956774867,12.2661797750255));
#55955=CARTESIAN_POINT('Ctrl Pts',(1.61355739161657,113.878255285806,12.3220618593612));
#55956=CARTESIAN_POINT('Ctrl Pts',(1.6474964294779,113.886553606289,12.379922545847));
#55957=CARTESIAN_POINT('Ctrl Pts',(1.6782919101032,113.8948532276,12.4394029605775));
#55958=CARTESIAN_POINT('Ctrl Pts',(1.73060015251952,113.908950705369,12.5404345369508));
#55959=CARTESIAN_POINT('Ctrl Pts',(1.77385041320905,113.923098873948,12.6463124511045));
#55960=CARTESIAN_POINT('Ctrl Pts',(1.80738463447079,113.937272366587,12.7552379913748));
#55961=CARTESIAN_POINT('Ctrl Pts',(1.84108649701919,113.951516714085,12.8647080624866));
#55962=CARTESIAN_POINT('Ctrl Pts',(1.86497526047677,113.965786630972,12.9772547645406));
#55963=CARTESIAN_POINT('Ctrl Pts',(1.87843343938246,113.980060002704,13.09106124097));
#55964=CARTESIAN_POINT('Ctrl Pts',(1.88092944207235,113.982707194013,13.1121682030104));
#55965=CARTESIAN_POINT('Ctrl Pts',(1.88306679711195,113.985354514367,13.1333185578355));
#55966=CARTESIAN_POINT('Ctrl Pts',(1.88484173947483,113.988001836676,13.1545008107529));
#55967=CARTESIAN_POINT('Ctrl Pts',(1.89437491676183,114.002220547905,13.2682702359599));
#55968=CARTESIAN_POINT('Ctrl Pts',(1.89345088064779,114.016439019261,13.3829565767269));
#55969=CARTESIAN_POINT('Ctrl Pts',(1.88243167837123,114.030639723897,13.4966779852143));
#55970=CARTESIAN_POINT('Ctrl Pts',(1.88061871925501,114.032976126867,13.5153882565255));
#55971=CARTESIAN_POINT('Ctrl Pts',(1.87853255565419,114.035312057001,13.5340725027145));
#55972=CARTESIAN_POINT('Ctrl Pts',(1.87617486875342,114.037647445818,13.55272246098));
#55973=CARTESIAN_POINT('Ctrl Pts',(1.86655495834301,114.047176374865,13.6288186243906));
#55974=CARTESIAN_POINT('Ctrl Pts',(1.85221077682933,114.056768339644,13.7043762570556));
#55975=CARTESIAN_POINT('Ctrl Pts',(1.83333831805893,114.066383332898,13.7788221911929));
#55976=CARTESIAN_POINT('Ctrl Pts',(1.81450602722814,114.075977861702,13.8531096753993));
#55977=CARTESIAN_POINT('Ctrl Pts',(1.79116575510658,114.085595317157,13.9262903578577));
#55978=CARTESIAN_POINT('Ctrl Pts',(1.76350377931296,114.095202596919,13.9978452840769));
#55979=CARTESIAN_POINT('Ctrl Pts',(1.75224022547414,114.099114541375,14.0269814083334));
#55980=CARTESIAN_POINT('Ctrl Pts',(1.74025994822911,114.103024875785,14.0558485498393));
#55981=CARTESIAN_POINT('Ctrl Pts',(1.72757452580162,114.10693168425,14.0844139255362));
#55982=CARTESIAN_POINT('Ctrl Pts',(1.7246540013776,114.107831136327,14.0909904410508));
#55983=CARTESIAN_POINT('Ctrl Pts',(1.72169609805543,114.108730402288,14.0975509668185));
#55984=CARTESIAN_POINT('Ctrl Pts',(1.71870115960148,114.109629460138,14.1040952011984));
#55985=CARTESIAN_POINT('Ctrl Pts',(1.68460319538879,114.119865410846,14.1786025986353));
#55986=CARTESIAN_POINT('Ctrl Pts',(1.64570302328899,114.130075418171,14.2509379872603));
#55987=CARTESIAN_POINT('Ctrl Pts',(1.60231893835089,114.140291869123,14.3205285350877));
#55988=CARTESIAN_POINT('Ctrl Pts',(1.55908196278321,114.150473677518,14.3898831110905));
#55989=CARTESIAN_POINT('Ctrl Pts',(1.51139041367417,114.160661886031,14.4565108632169));
#55990=CARTESIAN_POINT('Ctrl Pts',(1.45958440528606,114.170881855668,14.5198003353242));
#55991=CARTESIAN_POINT('Ctrl Pts',(1.44146294455037,114.174456745614,14.5419386493819));
#55992=CARTESIAN_POINT('Ctrl Pts',(1.42283834826223,114.178035461616,14.5636681470598));
#55993=CARTESIAN_POINT('Ctrl Pts',(1.4037262280594,114.181618894535,14.5849615914187));
#55994=CARTESIAN_POINT('Ctrl Pts',(1.34963797453741,114.191760188444,14.645223101111));
#55995=CARTESIAN_POINT('Ctrl Pts',(1.2916537876328,114.20193073026,14.7020775314085));
#55996=CARTESIAN_POINT('Ctrl Pts',(1.23024906046308,114.212102978335,14.7550620501643));
#55997=CARTESIAN_POINT('Ctrl Pts',(1.20128249758313,114.216901551297,14.7800565329173));
#55998=CARTESIAN_POINT('Ctrl Pts',(1.17155430541961,114.221700602415,14.8041904370712));
#55999=CARTESIAN_POINT('Ctrl Pts',(1.14111156484312,114.22649777038,14.8274180150671));
#56000=CARTESIAN_POINT('Ctrl Pts',(1.08268323793745,114.235704907871,14.8719983811796));
#56001=CARTESIAN_POINT('Ctrl Pts',(1.02162475849868,114.244904825821,14.9132392737883));
#56002=CARTESIAN_POINT('Ctrl Pts',(0.958396033709798,114.254084367512,14.9510161522063));
#56003=CARTESIAN_POINT('Ctrl Pts',(0.895142743528231,114.263267475604,14.9888077075588));
#56004=CARTESIAN_POINT('Ctrl Pts',(0.829703764380408,114.272442907348,15.0230456312068));
#56005=CARTESIAN_POINT('Ctrl Pts',(0.762474537595148,114.281633884579,15.053425384448));
#56006=CARTESIAN_POINT('Ctrl Pts',(0.69557730914607,114.290779473974,15.0836551132428));
#56007=CARTESIAN_POINT('Ctrl Pts',(0.626907143147252,114.299940452914,15.1100637585344));
#56008=CARTESIAN_POINT('Ctrl Pts',(0.556901841504499,114.309133156748,15.1323347236969));
#56009=CARTESIAN_POINT('Ctrl Pts',(0.512618724374969,114.314948167483,15.1464226246949));
#56010=CARTESIAN_POINT('Ctrl Pts',(0.467802359643517,114.320775742032,15.1588545741462));
#56011=CARTESIAN_POINT('Ctrl Pts',(0.422574251125431,114.326618658521,15.1695496006069));
#56012=CARTESIAN_POINT('Ctrl Pts',(0.370903099081658,114.333293937152,15.1817682044016));
#56013=CARTESIAN_POINT('Ctrl Pts',(0.318677340747473,114.339968686744,15.1918946382465));
#56014=CARTESIAN_POINT('Ctrl Pts',(0.266059723068317,114.346643823215,15.1998412406741));
#56015=CARTESIAN_POINT('Ctrl Pts',(0.158565375490708,114.360280689945,15.2160756290992));
#56016=CARTESIAN_POINT('Ctrl Pts',(0.0494326964004417,114.373919388781,
15.2232102815474));
#56017=CARTESIAN_POINT('Ctrl Pts',(-0.0597427169427481,114.387565093632,
15.2212594404747));
#56018=CARTESIAN_POINT('Ctrl Pts',(-0.170767016892279,114.401441888616,
15.2192755618908));
#56019=CARTESIAN_POINT('Ctrl Pts',(-0.28183445108275,114.415325944726,15.2078949509118));
#56020=CARTESIAN_POINT('Ctrl Pts',(-0.39122717706073,114.429219030687,15.1871685859229));
#56021=CARTESIAN_POINT('Ctrl Pts',(-0.491373073849375,114.44193775161,15.1681941944318));
#56022=CARTESIAN_POINT('Ctrl Pts',(-0.590114080078031,114.454664000419,
15.1413872200997));
#56023=CARTESIAN_POINT('Ctrl Pts',(-0.686117135667628,114.46739636212,15.1068219806883));
#56024=CARTESIAN_POINT('Ctrl Pts',(-0.789246990602818,114.481073912351,
15.0696907862235));
#56025=CARTESIAN_POINT('Ctrl Pts',(-0.889216089163326,114.494758557921,
15.0236063636402));
#56026=CARTESIAN_POINT('Ctrl Pts',(-0.98465074834828,114.508445266388,14.9694708212781));
#56027=CARTESIAN_POINT('Ctrl Pts',(-1.07262703043059,114.521062335859,14.9195660614539));
#56028=CARTESIAN_POINT('Ctrl Pts',(-1.15674895065018,114.533681120127,14.8628200486013));
#56029=CARTESIAN_POINT('Ctrl Pts',(-1.23595733003204,114.546294984981,14.7999749220962));
#56030=CARTESIAN_POINT('Ctrl Pts',(-1.31918266794619,114.559548546954,14.733942679921));
#56031=CARTESIAN_POINT('Ctrl Pts',(-1.3973579774902,114.572850791295,14.6609217524408));
#56032=CARTESIAN_POINT('Ctrl Pts',(-1.46920564745209,114.586189872428,14.5817105294917));
#56033=CARTESIAN_POINT('Ctrl Pts',(-1.47400615624047,114.587081124381,14.5764180242218));
#56034=CARTESIAN_POINT('Ctrl Pts',(-1.47877843046163,114.587972542245,14.571097897212));
#56035=CARTESIAN_POINT('Ctrl Pts',(-1.48352209509887,114.588864123114,14.5657503919148));
#56036=CARTESIAN_POINT('Ctrl Pts',(-1.55486081320341,114.602272372035,14.4853306737995));
#56037=CARTESIAN_POINT('Ctrl Pts',(-1.61972500331757,114.615717153408,14.3987170746629));
#56038=CARTESIAN_POINT('Ctrl Pts',(-1.67718661091241,114.629190209967,14.3072323840924));
#56039=CARTESIAN_POINT('Ctrl Pts',(-1.7067243286291,114.636115935822,14.2602053502418));
#56040=CARTESIAN_POINT('Ctrl Pts',(-1.73430678768296,114.643049198262,14.2118915549311));
#56041=CARTESIAN_POINT('Ctrl Pts',(-1.75981311677507,114.649989287947,14.1624718054398));
#56042=CARTESIAN_POINT('Ctrl Pts',(-1.79735780595881,114.660204929296,14.0897271494964));
#56043=CARTESIAN_POINT('Ctrl Pts',(-1.83040344750843,114.670435305712,14.01458652634));
#56044=CARTESIAN_POINT('Ctrl Pts',(-1.85898458022629,114.680679658673,13.9375759235067));
#56045=CARTESIAN_POINT('Ctrl Pts',(-1.88759691899623,114.690935196839,13.860481237341));
#56046=CARTESIAN_POINT('Ctrl Pts',(-1.91173453636451,114.70120474346,13.7815128709255));
#56047=CARTESIAN_POINT('Ctrl Pts',(-1.93046590239181,114.711488593118,13.7013890695747));
#56048=CARTESIAN_POINT('Ctrl Pts',(-1.95494309196695,114.724927001042,13.5966873904613));
#56049=CARTESIAN_POINT('Ctrl Pts',(-1.97018939645756,114.738389712462,13.4900147287906));
#56050=CARTESIAN_POINT('Ctrl Pts',(-1.97669816577161,114.751880528984,13.382740900891));
#56051=CARTESIAN_POINT('Ctrl Pts',(-1.97950230514057,114.757692707585,13.3365246732821));
#56052=CARTESIAN_POINT('Ctrl Pts',(-1.98068500018267,114.763510148179,13.2901963152702));
#56053=CARTESIAN_POINT('Ctrl Pts',(-1.98028688445897,114.769333357617,13.2438625847752));
#56054=CARTESIAN_POINT('Ctrl Pts',(-1.97954805877451,114.780140106616,13.1578761539258));
#56055=CARTESIAN_POINT('Ctrl Pts',(-1.97289380418289,114.790974816052,13.0715794340183));
#56056=CARTESIAN_POINT('Ctrl Pts',(-1.9605397664933,114.801824596246,12.9858061993644));
#56057=CARTESIAN_POINT('Ctrl Pts',(-1.94786271893812,114.812958055843,12.8977903294124));
#56058=CARTESIAN_POINT('Ctrl Pts',(-1.92918479688155,114.824107361028,12.8103265434447));
#56059=CARTESIAN_POINT('Ctrl Pts',(-1.90478500616689,114.835262997105,12.7242861190374));
#56060=CARTESIAN_POINT('Ctrl Pts',(-1.88009678708559,114.846550503244,12.637228616272));
#56061=CARTESIAN_POINT('Ctrl Pts',(-1.84955162894026,114.857844478874,12.5516289980619));
#56062=CARTESIAN_POINT('Ctrl Pts',(-1.8134705797214,114.869139784872,12.4683481216365));
#56063=CARTESIAN_POINT('Ctrl Pts',(-1.77754236835707,114.880387244414,12.3854200196108));
#56064=CARTESIAN_POINT('Ctrl Pts',(-1.73612605171753,114.891636026099,12.3047913928028));
#56065=CARTESIAN_POINT('Ctrl Pts',(-1.68955508506549,114.902885753633,12.2272636927215));
#56066=CARTESIAN_POINT('Ctrl Pts',(-1.64330270306537,114.914058523552,12.1502663474324));
#56067=CARTESIAN_POINT('Ctrl Pts',(-1.59196679225601,114.925232233742,12.0763277294864));
#56068=CARTESIAN_POINT('Ctrl Pts',(-1.53587670389948,114.936411078823,12.006181951572));
#56069=CARTESIAN_POINT('Ctrl Pts',(-1.49448130670192,114.944661248254,11.9544132269439));
#56070=CARTESIAN_POINT('Ctrl Pts',(-1.45049655134422,114.952914309089,11.9047092579959));
#56071=CARTESIAN_POINT('Ctrl Pts',(-1.4040520209068,114.961173521084,11.8573471711196));
#56072=CARTESIAN_POINT('Ctrl Pts',(-1.33819344786587,114.972885124393,11.7901874985266));
#56073=CARTESIAN_POINT('Ctrl Pts',(-1.26739146386725,114.984608878134,11.7277382796105));
#56074=CARTESIAN_POINT('Ctrl Pts',(-1.19260201353219,114.996358577999,11.6703739518762));
#56075=CARTESIAN_POINT('Ctrl Pts',(-1.10707777757756,115.009794752475,11.6047759259708));
#56076=CARTESIAN_POINT('Ctrl Pts',(-1.01575429987191,115.023248783164,11.5458756839365));
#56077=CARTESIAN_POINT('Ctrl Pts',(-0.919995153934207,115.036721605789,
11.4944557145685));
#56078=CARTESIAN_POINT('Ctrl Pts',(-0.820781337934725,115.050680482844,
11.4411806844957));
#56079=CARTESIAN_POINT('Ctrl Pts',(-0.716807783998793,115.064659495539,
11.3959350914759));
#56080=CARTESIAN_POINT('Ctrl Pts',(-0.609588924382951,115.078665979716,
11.3595353194296));
#56081=CARTESIAN_POINT('Ctrl Pts',(-0.58708529063664,115.081605731091,11.3518955521209));
#56082=CARTESIAN_POINT('Ctrl Pts',(-0.564438636161258,115.0845467151,11.3446452862742));
#56083=CARTESIAN_POINT('Ctrl Pts',(-0.541662845511286,115.087489035339,
11.3377918074298));
#56084=CARTESIAN_POINT('Ctrl Pts',(-0.433090865926177,115.101515048218,
11.3051213383066));
#56085=CARTESIAN_POINT('Ctrl Pts',(-0.32158728440439,115.115570919231,11.2814705209975));
#56086=CARTESIAN_POINT('Ctrl Pts',(-0.208740093011524,115.129671734795,
11.2670225831313));
#56087=CARTESIAN_POINT('Ctrl Pts',(-0.0954959987621371,115.143822145337,
11.2525238293985));
#56088=CARTESIAN_POINT('Ctrl Pts',(0.0191003291196167,115.158017820759,
11.2472915730283));
#56089=CARTESIAN_POINT('Ctrl Pts',(0.133489161976199,115.1722803876,11.2514841753134));
#56090=CARTESIAN_POINT('Ctrl Pts',(0.247877994832781,115.186542954441,11.2556767775986));
#56091=CARTESIAN_POINT('Ctrl Pts',(0.362059023130047,115.200872423394,11.2692930525077));
#56092=CARTESIAN_POINT('Ctrl Pts',(0.474526150140969,115.215296677043,11.2924828105989));
#56093=CARTESIAN_POINT('Ctrl Pts',(0.50602381165388,115.219336348643,11.2989773585645));
#56094=CARTESIAN_POINT('Ctrl Pts',(0.537387379013572,115.223383491721,11.3062227970019));
#56095=CARTESIAN_POINT('Ctrl Pts',(0.568587127550378,115.227438802565,11.3141998098193));
#56096=CARTESIAN_POINT('Ctrl Pts',(0.685283669077595,115.242606897581,11.344036262072));
#56097=CARTESIAN_POINT('Ctrl Pts',(0.799648242264584,115.257737894668,11.3846662327927));
#56098=CARTESIAN_POINT('Ctrl Pts',(0.909979583555605,115.272847673227,11.435094383272));
#56099=CARTESIAN_POINT('Ctrl Pts',(1.0238062785511,115.288436137351,11.4871201235251));
#56100=CARTESIAN_POINT('Ctrl Pts',(1.13334103054777,115.304001984215,11.5495729775517));
#56101=CARTESIAN_POINT('Ctrl Pts',(1.23676642008008,115.31957053264,11.6213794977147));
#56102=CARTESIAN_POINT('Ctrl Pts',(1.29353921225325,115.328116499624,11.6607958988936));
#56103=CARTESIAN_POINT('Ctrl Pts',(1.34847195375019,115.336663420413,11.7030312412126));
#56104=CARTESIAN_POINT('Ctrl Pts',(1.4012683470544,115.345216495727,11.7479129855167));
#56105=CARTESIAN_POINT('Ctrl Pts',(1.48226718234083,115.358338398479,11.8167693748784));
#56106=CARTESIAN_POINT('Ctrl Pts',(1.55835527482928,115.371540344119,11.8917233631653));
#56107=CARTESIAN_POINT('Ctrl Pts',(1.62837464185511,115.384802618524,11.9721818737286));
#56108=CARTESIAN_POINT('Ctrl Pts',(1.67307949990156,115.393270105733,12.0235517510375));
#56109=CARTESIAN_POINT('Ctrl Pts',(1.71531050678469,115.401762119113,12.077164434722));
#56110=CARTESIAN_POINT('Ctrl Pts',(1.75476984556133,115.410272829667,12.1328549792085));
#56111=CARTESIAN_POINT('Ctrl Pts',(1.81716417373831,115.423730228696,12.2209145923894));
#56112=CARTESIAN_POINT('Ctrl Pts',(1.87262649087647,115.437234543671,12.3141708941146));
#56113=CARTESIAN_POINT('Ctrl Pts',(1.92073481534129,115.450759946289,12.411281384807));
#56114=CARTESIAN_POINT('Ctrl Pts',(1.93704224606978,115.455344694744,12.4441992346302));
#56115=CARTESIAN_POINT('Ctrl Pts',(1.95250500725449,115.459931837736,12.4775596439822));
#56116=CARTESIAN_POINT('Ctrl Pts',(1.96710777417235,115.464520282047,12.5113095315961));
#56117=CARTESIAN_POINT('Ctrl Pts',(2.02284203773276,115.482032960706,12.6401224573922));
#56118=CARTESIAN_POINT('Ctrl Pts',(2.06613025176284,115.499578000723,12.7749773920369));
#56119=CARTESIAN_POINT('Ctrl Pts',(2.09613795233903,115.517181179691,12.9131906279659));
#56120=CARTESIAN_POINT('Ctrl Pts',(2.12402968913341,115.533543087638,13.0416578921684));
#56121=CARTESIAN_POINT('Ctrl Pts',(2.14044852787112,115.549955270481,13.1730279986298));
#56122=CARTESIAN_POINT('Ctrl Pts',(2.14468284862367,115.566441721781,13.3051600237124));
#56123=CARTESIAN_POINT('Ctrl Pts',(2.14632244725498,115.572825546854,13.3563237168141));
#56124=CARTESIAN_POINT('Ctrl Pts',(2.14613462261372,115.579220540859,13.4076016959267));
#56125=CARTESIAN_POINT('Ctrl Pts',(2.14407588116522,115.585628222627,13.4588695760761));
#56126=CARTESIAN_POINT('Ctrl Pts',(2.14147055810292,115.59373709958,13.5237487237737));
#56127=CARTESIAN_POINT('Ctrl Pts',(2.13586729158356,115.601856107239,13.5885460652796));
#56128=CARTESIAN_POINT('Ctrl Pts',(2.12719321699842,115.609986063637,13.6530007834056));
#56129=CARTESIAN_POINT('Ctrl Pts',(2.10699154461732,115.628920500274,13.8031139840954));
#56130=CARTESIAN_POINT('Ctrl Pts',(2.07013478074693,115.647914195593,13.9513654573672));
#56131=CARTESIAN_POINT('Ctrl Pts',(2.01824822471315,115.666978611439,14.0946950219294));
#56132=CARTESIAN_POINT('Ctrl Pts',(1.98042961867447,115.680874111302,14.1991637851355));
#56133=CARTESIAN_POINT('Ctrl Pts',(1.9346262410061,115.694807222267,14.3010187640065));
#56134=CARTESIAN_POINT('Ctrl Pts',(1.88146178409473,115.708783002571,14.3990916206313));
#56135=CARTESIAN_POINT('Ctrl Pts',(1.83036747451932,115.722214586131,14.4933456615536));
#56136=CARTESIAN_POINT('Ctrl Pts',(1.77222890192354,115.735622945604,14.5842203077108));
#56137=CARTESIAN_POINT('Ctrl Pts',(1.70764755970895,115.749035808859,14.6705866225551));
#56138=CARTESIAN_POINT('Ctrl Pts',(1.64306632820495,115.76244864912,14.7569527893432));
#56139=CARTESIAN_POINT('Ctrl Pts',(1.5720435452874,115.77586600016,14.8388103433535));
#56140=CARTESIAN_POINT('Ctrl Pts',(1.49519464604144,115.789320521743,14.9150797911722));
#56141=CARTESIAN_POINT('Ctrl Pts',(1.44760010886154,115.797653259544,14.9623154588983));
#56142=CARTESIAN_POINT('Ctrl Pts',(1.39777106681861,115.806000351625,15.0074087322159));
#56143=CARTESIAN_POINT('Ctrl Pts',(1.34585358646912,115.814370484018,15.0501131939447));
#56144=CARTESIAN_POINT('Ctrl Pts',(1.3071473427463,115.820610701807,15.0819508195884));
#56145=CARTESIAN_POINT('Ctrl Pts',(1.26728031463752,115.826863740542,15.1124608690016));
#56146=CARTESIAN_POINT('Ctrl Pts',(1.22636916842543,115.83313345591,15.1415957736095));
#56147=CARTESIAN_POINT('Ctrl Pts',(1.12810170945666,115.848193141466,15.2115770209762));
#56148=CARTESIAN_POINT('Ctrl Pts',(1.02382909071115,115.863353703261,15.2736274831145));
#56149=CARTESIAN_POINT('Ctrl Pts',(0.914955216940758,115.878572923054,15.3270233660414));
#56150=CARTESIAN_POINT('Ctrl Pts',(0.819226999552299,115.891954542816,15.3739721197823));
#56151=CARTESIAN_POINT('Ctrl Pts',(0.719941095969984,115.905381408066,15.4142287706305));
#56152=CARTESIAN_POINT('Ctrl Pts',(0.618066703704985,115.918820787105,15.4472718233318));
#56153=CARTESIAN_POINT('Ctrl Pts',(0.51392554880499,115.932559199901,15.4810501025758));
#56154=CARTESIAN_POINT('Ctrl Pts',(0.407078861767362,115.946310694998,15.5072896988209));
#56155=CARTESIAN_POINT('Ctrl Pts',(0.29865525520882,115.960036151081,15.5255720386239));
#56156=CARTESIAN_POINT('Ctrl Pts',(0.182916754998672,115.974687607091,15.5450878125065));
#56157=CARTESIAN_POINT('Ctrl Pts',(0.0653436635643293,115.989459403803,
15.5557348502609));
#56158=CARTESIAN_POINT('Ctrl Pts',(-0.052617637522511,116.0043251002,15.5570067734007));
#56159=CARTESIAN_POINT('Ctrl Pts',(-0.106561210549434,116.011123166785,
15.5575884224512));
#56160=CARTESIAN_POINT('Ctrl Pts',(-0.160585503936932,116.017940835553,
15.5562100758667));
#56161=CARTESIAN_POINT('Ctrl Pts',(-0.214550364991037,116.024775405707,
15.5528264578072));
#56162=CARTESIAN_POINT('Ctrl Pts',(-0.33323579887121,116.039806741067,15.5453848343205));
#56163=CARTESIAN_POINT('Ctrl Pts',(-0.451633874569923,116.054919990971,
15.5282403430295));
#56164=CARTESIAN_POINT('Ctrl Pts',(-0.568252849555415,116.070084823131,
15.5019345828368));
#56165=CARTESIAN_POINT('Ctrl Pts',(-0.618392857246718,116.076604901028,
15.4906244935605));
#56166=CARTESIAN_POINT('Ctrl Pts',(-0.668203943852332,116.083134483099,
15.4776215571167));
#56167=CARTESIAN_POINT('Ctrl Pts',(-0.717567805806733,116.089671019621,
15.4629717731698));
#56168=CARTESIAN_POINT('Ctrl Pts',(-0.834150577526599,116.105108376323,
15.4283733371885));
#56169=CARTESIAN_POINT('Ctrl Pts',(-0.948364145641417,116.120416762755,
15.3843060231208));
#56170=CARTESIAN_POINT('Ctrl Pts',(-1.05868732191905,116.135659632901,15.3314168528225));
#56171=CARTESIAN_POINT('Ctrl Pts',(-1.17134192991175,116.151224626758,15.2774099890968));
#56172=CARTESIAN_POINT('Ctrl Pts',(-1.27994059980948,116.166721298147,15.2142059500083));
#56173=CARTESIAN_POINT('Ctrl Pts',(-1.3829147316966,116.182224708343,15.1424762192239));
#56174=CARTESIAN_POINT('Ctrl Pts',(-1.46501198386403,116.194584971577,15.0852889073409));
#56175=CARTESIAN_POINT('Ctrl Pts',(-1.54353541226832,116.206949668497,15.0226822699764));
#56176=CARTESIAN_POINT('Ctrl Pts',(-1.6177072454825,116.219360164099,14.9549803930063));
#56177=CARTESIAN_POINT('Ctrl Pts',(-1.65858238845539,116.22619942855,14.9176707596756));
#56178=CARTESIAN_POINT('Ctrl Pts',(-1.69813562227692,116.233084387951,14.8788675694272));
#56179=CARTESIAN_POINT('Ctrl Pts',(-1.73623654775755,116.240006145925,14.8386078818976));
#56180=CARTESIAN_POINT('Ctrl Pts',(-1.81330527686961,116.254007146783,14.7571725121994));
#56181=CARTESIAN_POINT('Ctrl Pts',(-1.88443502621154,116.268159127004,14.6697767096657));
#56182=CARTESIAN_POINT('Ctrl Pts',(-1.94907960847239,116.282383109819,14.5774327095694));
#56183=CARTESIAN_POINT('Ctrl Pts',(-2.01507679914757,116.296904711988,14.4831565247923));
#56184=CARTESIAN_POINT('Ctrl Pts',(-2.07431366250875,116.311501363033,14.3837217163799));
#56185=CARTESIAN_POINT('Ctrl Pts',(-2.12616402378042,116.326082039708,14.280234204363));
#56186=CARTESIAN_POINT('Ctrl Pts',(-2.15709073675296,116.33477884319,14.2185079501598));
#56187=CARTESIAN_POINT('Ctrl Pts',(-2.18538879693703,116.343469830457,14.1553405405778));
#56188=CARTESIAN_POINT('Ctrl Pts',(-2.21092009295596,116.352134539812,14.0909736700272));
#56189=CARTESIAN_POINT('Ctrl Pts',(-2.25486215680431,116.367047422083,13.9801914702771));
#56190=CARTESIAN_POINT('Ctrl Pts',(-2.29069844177545,116.381944676096,13.8657330971959));
#56191=CARTESIAN_POINT('Ctrl Pts',(-2.31776617764799,116.396846147778,13.7489725582936));
#56192=CARTESIAN_POINT('Ctrl Pts',(-2.34458345574813,116.411609736136,13.6332924047112));
#56193=CARTESIAN_POINT('Ctrl Pts',(-2.36279367397774,116.426377473984,13.5153537393306));
#56194=CARTESIAN_POINT('Ctrl Pts',(-2.37180242101775,116.441170795581,13.3964950169532));
#56195=CARTESIAN_POINT('Ctrl Pts',(-2.37576502392796,116.447677811368,13.3442136156545));
#56196=CARTESIAN_POINT('Ctrl Pts',(-2.37794800011267,116.454189804121,13.291754121448));
#56197=CARTESIAN_POINT('Ctrl Pts',(-2.37830389938607,116.460708723163,13.239229683751));
#56198=CARTESIAN_POINT('Ctrl Pts',(-2.37875671095951,116.469002760856,13.1724027047287));
#56199=CARTESIAN_POINT('Ctrl Pts',(-2.37625184052921,116.47730800462,13.1054707115953));
#56200=CARTESIAN_POINT('Ctrl Pts',(-2.37087518211755,116.485628716616,13.0386819501779));
#56201=CARTESIAN_POINT('Ctrl Pts',(-2.36133029276527,116.500400024228,12.9201154933015));
#56202=CARTESIAN_POINT('Ctrl Pts',(-2.34267915449744,116.515221006775,12.8017184202899));
#56203=CARTESIAN_POINT('Ctrl Pts',(-2.31529268428084,116.530091783787,12.6848953499409));
#56204=CARTESIAN_POINT('Ctrl Pts',(-2.28681456295353,116.54555532431,12.5634155993591));
#56205=CARTESIAN_POINT('Ctrl Pts',(-2.24889100388477,116.561072708035,12.4436391012527));
#56206=CARTESIAN_POINT('Ctrl Pts',(-2.20199445050019,116.576644531451,12.3271461148292));
#56207=CARTESIAN_POINT('Ctrl Pts',(-2.15535223441636,116.592131903128,12.2112849128245));
#56208=CARTESIAN_POINT('Ctrl Pts',(-2.09983465091386,116.607673129599,12.0986729808405));
#56209=CARTESIAN_POINT('Ctrl Pts',(-2.03595400084272,116.623269211091,11.9908465165357));
#56210=CARTESIAN_POINT('Ctrl Pts',(-1.97448327236903,116.63827692453,11.8870878462313));
#56211=CARTESIAN_POINT('Ctrl Pts',(-1.90526922618553,116.653335437877,11.7877612621495));
#56212=CARTESIAN_POINT('Ctrl Pts',(-1.82880326091235,116.668445952396,11.6942030383103));
#56213=CARTESIAN_POINT('Ctrl Pts',(-1.80048378080912,116.674042192681,11.6595533709839));
#56214=CARTESIAN_POINT('Ctrl Pts',(-1.77116991909143,116.679645568285,11.6256945101545));
#56215=CARTESIAN_POINT('Ctrl Pts',(-1.74088766295243,116.685256149272,11.592692791068));
#56216=CARTESIAN_POINT('Ctrl Pts',(-1.65765618047929,116.70067696108,11.5019868016883));
#56217=CARTESIAN_POINT('Ctrl Pts',(-1.56710879023825,116.71615218637,11.4177594726791));
#56218=CARTESIAN_POINT('Ctrl Pts',(-1.47063466401891,116.731682286979,11.3407084361487));
#56219=CARTESIAN_POINT('Ctrl Pts',(-1.41290748548492,116.740975026138,11.2946034428585));
#56220=CARTESIAN_POINT('Ctrl Pts',(-1.35305845127679,116.750287418186,11.251066977279));
#56221=CARTESIAN_POINT('Ctrl Pts',(-1.29138505495245,116.759619604489,11.2102394704746));
#56222=CARTESIAN_POINT('Ctrl Pts',(-1.18962354774155,116.775017772912,11.1428738172807));
#56223=CARTESIAN_POINT('Ctrl Pts',(-1.08223578712878,116.790146385918,11.0827796079039));
#56224=CARTESIAN_POINT('Ctrl Pts',(-0.970545703476898,116.805179784118,
11.0306873682955));
#56225=CARTESIAN_POINT('Ctrl Pts',(-0.856018421282094,116.82059506703,10.977271859678));
#56226=CARTESIAN_POINT('Ctrl Pts',(-0.73696885781619,116.835910228986,10.9322685711069));
#56227=CARTESIAN_POINT('Ctrl Pts',(-0.614794195145899,116.85132342974,10.8964200289001));
#56228=CARTESIAN_POINT('Ctrl Pts',(-0.491954171599043,116.86682057049,10.8603762562179));
#56229=CARTESIAN_POINT('Ctrl Pts',(-0.365955633575362,116.882416841384,
10.833585519513));
#56230=CARTESIAN_POINT('Ctrl Pts',(-0.238172442065973,116.898323679995,
10.8167817358934));
#56231=CARTESIAN_POINT('Ctrl Pts',(-0.196656945584479,116.903491654707,
10.8113223526092));
#56232=CARTESIAN_POINT('Ctrl Pts',(-0.154952671188114,116.90869248821,10.8069170728641));
#56233=CARTESIAN_POINT('Ctrl Pts',(-0.113105562718294,116.913933652364,
10.8035910556126));
#56234=CARTESIAN_POINT('Ctrl Pts',(1.89583865317118,21.7883719873226,13.197232071317));
#56235=CARTESIAN_POINT('Ctrl Pts',(1.91781707633732,21.8441218058461,13.6730473758255));
#56236=CARTESIAN_POINT('Ctrl Pts',(1.69642718260873,21.9440513975239,14.4537819826606));
#56237=CARTESIAN_POINT('Ctrl Pts',(0.672633958004841,22.0991544508714,15.2803835560697));
#56238=CARTESIAN_POINT('Ctrl Pts',(-0.60319738394239,22.250832522417,15.3221596893961));
#56239=CARTESIAN_POINT('Ctrl Pts',(-1.34901622678997,22.3564371611312,14.8505318619346));
#56240=CARTESIAN_POINT('Ctrl Pts',(-1.63086999297234,22.4127847437298,14.497109087338));
#56241=CARTESIAN_POINT('Ctrl Pts',(-1.67292082684555,22.4214691961456,14.4416712469716));
#56242=CARTESIAN_POINT('Ctrl Pts',(-1.74278673487562,22.4366802475148,14.3416803032928));
#56243=CARTESIAN_POINT('Ctrl Pts',(-1.86710205946279,22.4671818233788,14.1308312671578));
#56244=CARTESIAN_POINT('Ctrl Pts',(-2.04999258960691,22.528452716599,13.6722180537393));
#56245=CARTESIAN_POINT('Ctrl Pts',(-2.10140414959869,22.6167364856815,12.9515240914931));
#56246=CARTESIAN_POINT('Ctrl Pts',(-1.80799633762795,22.7240819881822,12.1227672472193));
#56247=CARTESIAN_POINT('Ctrl Pts',(-1.19990303017822,22.8328298152915,11.4720954721768));
#56248=CARTESIAN_POINT('Ctrl Pts',(-0.371002901919627,22.9431012190898,
11.1145961507936));
#56249=CARTESIAN_POINT('Ctrl Pts',(0.467762943195029,23.0455895703631,11.1178807055511));
#56250=CARTESIAN_POINT('Ctrl Pts',(1.1824163516888,23.1399165325713,11.3911664755444));
#56251=CARTESIAN_POINT('Ctrl Pts',(1.72621929731623,23.2257405437626,11.8251312591644));
#56252=CARTESIAN_POINT('Ctrl Pts',(2.05162663549235,23.2980233626201,12.3127044160272));
#56253=CARTESIAN_POINT('Ctrl Pts',(2.21469313453867,23.3563366579963,12.7519562978106));
#56254=CARTESIAN_POINT('Ctrl Pts',(2.35722297838454,23.4442829398336,13.4441616523464));
#56255=CARTESIAN_POINT('Ctrl Pts',(2.15527130903289,23.57796993702,14.5485148077445));
#56256=CARTESIAN_POINT('Ctrl Pts',(1.059145585634,23.7602399209507,15.6184220519286));
#56257=CARTESIAN_POINT('Ctrl Pts',(-0.529239386701929,23.9513951638177,
15.8648208380125));
#56258=CARTESIAN_POINT('Ctrl Pts',(-1.51756572472491,24.0834106661585,15.3439163457973));
#56259=CARTESIAN_POINT('Ctrl Pts',(-1.89463460506064,24.1527410864499,14.9357054885149));
#56260=CARTESIAN_POINT('Ctrl Pts',(2.09579517948206,21.7240373735623,13.1885007805612));
#56261=CARTESIAN_POINT('Ctrl Pts',(2.12135717463155,21.7843405351804,13.7037820948012));
#56262=CARTESIAN_POINT('Ctrl Pts',(1.87919305520299,21.8956866809261,14.5752420688376));
#56263=CARTESIAN_POINT('Ctrl Pts',(0.751099816146643,22.0664628760232,15.485969451142));
#56264=CARTESIAN_POINT('Ctrl Pts',(-0.657449610166076,22.2341318757709,
15.5386353888612));
#56265=CARTESIAN_POINT('Ctrl Pts',(-1.48093958778983,22.3504810823427,15.0191831835147));
#56266=CARTESIAN_POINT('Ctrl Pts',(-1.79271008834924,22.4125981058827,14.6305718396412));
#56267=CARTESIAN_POINT('Ctrl Pts',(-1.83921057775072,22.4221669865294,14.5696025279449));
#56268=CARTESIAN_POINT('Ctrl Pts',(-1.91649095560331,22.4389268751508,14.4596450638053));
#56269=CARTESIAN_POINT('Ctrl Pts',(-2.05404081986639,22.4725216181623,14.2277761229944));
#56270=CARTESIAN_POINT('Ctrl Pts',(-2.2567629418467,22.5399786177802,13.7234303602587));
#56271=CARTESIAN_POINT('Ctrl Pts',(-2.31535246183976,22.6371070814728,12.9307537793653));
#56272=CARTESIAN_POINT('Ctrl Pts',(-1.99544618564001,22.7549947273253,12.019912280396));
#56273=CARTESIAN_POINT('Ctrl Pts',(-1.33067454399223,22.8742133079875,11.3050824355626));
#56274=CARTESIAN_POINT('Ctrl Pts',(-0.424988525149834,22.9948313849074,
10.9118644483054));
#56275=CARTESIAN_POINT('Ctrl Pts',(0.490380343808289,23.1066820811408,10.913245367816));
#56276=CARTESIAN_POINT('Ctrl Pts',(1.26931089246893,23.2094023340903,11.2089165793694));
#56277=CARTESIAN_POINT('Ctrl Pts',(1.86149576703992,23.3026720706013,11.6790480189558));
#56278=CARTESIAN_POINT('Ctrl Pts',(2.21572530831819,23.3810697334384,12.2069903102016));
#56279=CARTESIAN_POINT('Ctrl Pts',(2.39354512758931,23.4442083621846,12.682127093083));
#56280=CARTESIAN_POINT('Ctrl Pts',(2.54968537849172,23.5393281857135,13.4304282224035));
#56281=CARTESIAN_POINT('Ctrl Pts',(2.33419451824951,23.6835362613187,14.6221100361887));
#56282=CARTESIAN_POINT('Ctrl Pts',(1.15975669052109,23.879193993993,15.7729786483405));
#56283=CARTESIAN_POINT('Ctrl Pts',(-0.536296867408047,24.0833794822401,
16.03953727275));
#56284=CARTESIAN_POINT('Ctrl Pts',(-1.5873348158791,24.2236364673292,15.4881545619776));
#56285=CARTESIAN_POINT('Ctrl Pts',(-1.9878959091456,24.2970685263766,15.0568812348725));
#56286=CARTESIAN_POINT('Ctrl Pts',(2.29575170579295,21.6597027598019,13.1797694898055));
#56287=CARTESIAN_POINT('Ctrl Pts',(2.32489727292579,21.7245592645148,13.7345168137768));
#56288=CARTESIAN_POINT('Ctrl Pts',(2.06195892779723,21.8473219643282,14.6967021550147));
#56289=CARTESIAN_POINT('Ctrl Pts',(0.829565674288447,22.033771301175,15.6915553462145));
#56290=CARTESIAN_POINT('Ctrl Pts',(-0.711701836389763,22.2174312291249,
15.7551110883264));
#56291=CARTESIAN_POINT('Ctrl Pts',(-1.61286294878969,22.3445250035544,15.1878345050949));
#56292=CARTESIAN_POINT('Ctrl Pts',(-1.95455018372616,22.4124114680356,14.7640345919444));
#56293=CARTESIAN_POINT('Ctrl Pts',(-2.0055003286559,22.4228647769132,14.6975338089182));
#56294=CARTESIAN_POINT('Ctrl Pts',(-2.09019517633101,22.4411735027868,14.5776098243179));
#56295=CARTESIAN_POINT('Ctrl Pts',(-2.24097958027,22.4778614129459,14.3247209788311));
#56296=CARTESIAN_POINT('Ctrl Pts',(-2.4635332940865,22.5515045189613,13.774642666778));
#56297=CARTESIAN_POINT('Ctrl Pts',(-2.52930077408085,22.6574776772641,12.9099834672373));
#56298=CARTESIAN_POINT('Ctrl Pts',(-2.18289603365208,22.7859074664684,11.9170573135726));
#56299=CARTESIAN_POINT('Ctrl Pts',(-1.46144605780623,22.9155968006837,11.1380693989486));
#56300=CARTESIAN_POINT('Ctrl Pts',(-0.478974148380045,23.0465615507249,
10.7091327458171));
#56301=CARTESIAN_POINT('Ctrl Pts',(0.512997744421549,23.1677745919185,10.7086100300809));
#56302=CARTESIAN_POINT('Ctrl Pts',(1.35620543324907,23.2788881356092,11.0266666831942));
#56303=CARTESIAN_POINT('Ctrl Pts',(1.99677223676361,23.37960359744,11.5329647787473));
#56304=CARTESIAN_POINT('Ctrl Pts',(2.37982398114403,23.4641161042566,12.1012762043759));
#56305=CARTESIAN_POINT('Ctrl Pts',(2.57239712063998,23.5320800663729,12.6122978883554));
#56306=CARTESIAN_POINT('Ctrl Pts',(2.7421477785989,23.6343734315934,13.4166947924605));
#56307=CARTESIAN_POINT('Ctrl Pts',(2.51311772746614,23.7891025856174,14.695705264633));
#56308=CARTESIAN_POINT('Ctrl Pts',(1.26036779540819,23.9981480670354,15.9275352447523));
#56309=CARTESIAN_POINT('Ctrl Pts',(-0.543354348114162,24.2153638006625,
16.2142537074874));
#56310=CARTESIAN_POINT('Ctrl Pts',(-1.6571039070333,24.3638622684998,15.632392778158));
#56311=CARTESIAN_POINT('Ctrl Pts',(-2.08115721323056,24.4413959663033,15.1780569812301));
#56312=CARTESIAN_POINT('Ctrl Pts',(2.49570823210383,21.5953681460417,13.1710381990497));
#56313=CARTESIAN_POINT('Ctrl Pts',(2.52843737122002,21.6647779938492,13.7652515327526));
#56314=CARTESIAN_POINT('Ctrl Pts',(2.24472480039148,21.7989572477304,14.8181622411917));
#56315=CARTESIAN_POINT('Ctrl Pts',(0.908031532430251,22.0010797263267,15.8971412412869));
#56316=CARTESIAN_POINT('Ctrl Pts',(-0.765954062613445,22.2007305824788,
15.9715867877915));
#56317=CARTESIAN_POINT('Ctrl Pts',(-1.74478630978955,22.338568924766,15.3564858266751));
#56318=CARTESIAN_POINT('Ctrl Pts',(-2.11639027910306,22.4122248301885,14.8974973442476));
#56319=CARTESIAN_POINT('Ctrl Pts',(-2.17179007956105,22.4235625672971,14.8254650898915));
#56320=CARTESIAN_POINT('Ctrl Pts',(-2.2638993970587,22.4434201304229,14.6955745848305));
#56321=CARTESIAN_POINT('Ctrl Pts',(-2.42791834067359,22.4832012077294,14.4216658346677));
#56322=CARTESIAN_POINT('Ctrl Pts',(-2.67030364632629,22.5630304201425,13.8258549732975));
#56323=CARTESIAN_POINT('Ctrl Pts',(-2.74324908632193,22.6778482730553,12.8892131551093));
#56324=CARTESIAN_POINT('Ctrl Pts',(-2.37034588166413,22.8168202056115,11.8142023467493));
#56325=CARTESIAN_POINT('Ctrl Pts',(-1.59221757162024,22.9569802933797,10.9710563623344));
#56326=CARTESIAN_POINT('Ctrl Pts',(-0.532959771610249,23.0982917165424,
10.5064010433289));
#56327=CARTESIAN_POINT('Ctrl Pts',(0.535615145034812,23.2288671026962,10.5039746923458));
#56328=CARTESIAN_POINT('Ctrl Pts',(1.4430999740292,23.3483739371282,10.8444167870192));
#56329=CARTESIAN_POINT('Ctrl Pts',(2.1320487064873,23.4565351242787,11.3868815385387));
#56330=CARTESIAN_POINT('Ctrl Pts',(2.54392265396986,23.5471624750749,11.9955620985503));
#56331=CARTESIAN_POINT('Ctrl Pts',(2.75124911369062,23.6199517705612,12.5424686836278));
#56332=CARTESIAN_POINT('Ctrl Pts',(2.93461017870607,23.7294186774733,13.4029613625176));
#56333=CARTESIAN_POINT('Ctrl Pts',(2.69204093668275,23.8946689099161,14.7693004930773));
#56334=CARTESIAN_POINT('Ctrl Pts',(1.36097890029528,24.1171021400777,16.0820918411643));
#56335=CARTESIAN_POINT('Ctrl Pts',(-0.55041182882028,24.3473481190849,16.3889701422247));
#56336=CARTESIAN_POINT('Ctrl Pts',(-1.7268729981875,24.5040880696705,15.7766309943384));
#56337=CARTESIAN_POINT('Ctrl Pts',(-2.17441851731554,24.5857234062301,15.2992327275877));
#56338=CARTESIAN_POINT('',(1.9,21.8,13.3));
#56339=CARTESIAN_POINT('Ctrl Pts',(-3.1635730752188,29.2100860618195,12.4907938897549));
#56340=CARTESIAN_POINT('Ctrl Pts',(-2.98085158893828,29.3019317286879,11.7779528294547));
#56341=CARTESIAN_POINT('Ctrl Pts',(-2.12224476023707,29.4834174338966,10.5004848443473));
#56342=CARTESIAN_POINT('Ctrl Pts',(0.0593203066058203,29.7539464610308,
9.80303601328355));
#56343=CARTESIAN_POINT('Ctrl Pts',(2.1830045028505,30.0213429575011,10.5869226484086));
#56344=CARTESIAN_POINT('Ctrl Pts',(3.36867072083526,30.2873651789924,12.5013119695689));
#56345=CARTESIAN_POINT('Ctrl Pts',(3.12820931026034,30.5516392506713,14.7255047004695));
#56346=CARTESIAN_POINT('Ctrl Pts',(1.58055854613697,30.8138087120526,16.3181541366838));
#56347=CARTESIAN_POINT('Ctrl Pts',(-0.593576583725148,31.0735240541513,
16.6192226195957));
#56348=CARTESIAN_POINT('Ctrl Pts',(-2.69414652544478,31.3590120613392,15.4093240673898));
#56349=CARTESIAN_POINT('Ctrl Pts',(-3.29228396144786,31.6123375258171,13.2621475022427));
#56350=CARTESIAN_POINT('Ctrl Pts',(-2.59121784125708,31.8344343538493,11.5764220916364));
#56351=CARTESIAN_POINT('Ctrl Pts',(-1.26416080201115,32.0543699991392,10.3503143566391));
#56352=CARTESIAN_POINT('Ctrl Pts',(1.11608957290045,32.3250666810991,10.167546191111));
#56353=CARTESIAN_POINT('Ctrl Pts',(3.06291956153987,32.6425883170784,12.194735374529));
#56354=CARTESIAN_POINT('Ctrl Pts',(2.72096138219714,32.9523804802361,14.9138117217176));
#56355=CARTESIAN_POINT('Ctrl Pts',(0.661085756377314,33.2289591199972,16.2180280599844));
#56356=CARTESIAN_POINT('Ctrl Pts',(-1.37468245683901,33.4743218620618,15.7903827762575));
#56357=CARTESIAN_POINT('Ctrl Pts',(-2.55899077373492,33.6904057619936,14.3988045569796));
#56358=CARTESIAN_POINT('Ctrl Pts',(-2.63218467362997,33.9017075317211,12.6113846899565));
#56359=CARTESIAN_POINT('Ctrl Pts',(-1.61587194033675,34.1082261165484,11.1894758647939));
#56360=CARTESIAN_POINT('Ctrl Pts',(0.0216236752264965,34.3099896601507,
10.7039018687867));
#56361=CARTESIAN_POINT('Ctrl Pts',(1.57455705156837,34.5070605714621,11.3135848522268));
#56362=CARTESIAN_POINT('Ctrl Pts',(2.40467660737928,34.6995310564001,12.7155627750386));
#56363=CARTESIAN_POINT('Ctrl Pts',(2.20227690752673,34.8875249955867,14.2941075319982));
#56364=CARTESIAN_POINT('Ctrl Pts',(1.09822533438088,35.071196858881,15.3888766878108));
#56365=CARTESIAN_POINT('Ctrl Pts',(-0.410767088927198,35.2507283443733,
15.5694539058736));
#56366=CARTESIAN_POINT('Ctrl Pts',(-1.68341513267947,35.426332789423,14.8014468984984));
#56367=CARTESIAN_POINT('Ctrl Pts',(-2.20404781770678,35.5982453338191,13.4424781480868));
#56368=CARTESIAN_POINT('Ctrl Pts',(-1.78749563440858,35.7667271053238,12.0784119565304));
#56369=CARTESIAN_POINT('Ctrl Pts',(-0.643778855103036,35.932070046999,11.2723067128195));
#56370=CARTESIAN_POINT('Ctrl Pts',(0.73153021794509,36.0945712336176,11.3404925776424));
#56371=CARTESIAN_POINT('Ctrl Pts',(1.64179858012663,36.2367845423708,12.1262687862789));
#56372=CARTESIAN_POINT('Ctrl Pts',(1.9482293952285,36.3598159578115,13.0895347694922));
#56373=CARTESIAN_POINT('Ctrl Pts',(1.85369636211229,36.4469825000565,13.798453582504));
#56374=CARTESIAN_POINT('Ctrl Pts',(1.47997487612049,36.5510130076167,14.5486099218439));
#56375=CARTESIAN_POINT('Ctrl Pts',(0.566464679004626,36.6888005486365,15.2755886466896));
#56376=CARTESIAN_POINT('Ctrl Pts',(-1.08230306928676,36.8765589250003,15.0981146135781));
#56377=CARTESIAN_POINT('Ctrl Pts',(-2.07361092665276,37.0801652535577,13.5967024919891));
#56378=CARTESIAN_POINT('Ctrl Pts',(-1.53672541544744,37.2835003657197,11.878050082411));
#56379=CARTESIAN_POINT('Ctrl Pts',(-0.287225265330017,37.4364977401447,
11.3697244603319));
#56380=CARTESIAN_POINT('Ctrl Pts',(0.527796451225459,37.5389857152615,11.5096660141286));
#56381=CARTESIAN_POINT('Ctrl Pts',(0.911332139704861,37.5903389447939,11.6650339396913));
#56382=CARTESIAN_POINT('Ctrl Pts',(1.25141660620714,37.6418223573826,11.9028228864947));
#56383=CARTESIAN_POINT('Ctrl Pts',(1.81663055575573,37.745068412759,12.5140494449059));
#56384=CARTESIAN_POINT('Ctrl Pts',(2.08083561316247,37.9010949500106,13.8665607540922));
#56385=CARTESIAN_POINT('Ctrl Pts',(1.09046525980936,38.0772682104256,15.0644393884671));
#56386=CARTESIAN_POINT('Ctrl Pts',(0.0831693118407307,38.2024111697257,
15.2788956384127));
#56387=CARTESIAN_POINT('Ctrl Pts',(-0.493207305974611,38.2744972359008,
15.2113913577473));
#56388=CARTESIAN_POINT('Ctrl Pts',(-1.13701083528365,38.3590598197545,14.9858687442177));
#56389=CARTESIAN_POINT('Ctrl Pts',(-1.62678194860183,38.438406077977,14.5394092422429));
#56390=CARTESIAN_POINT('Ctrl Pts',(-1.89003400591192,38.5124054303739,14.0059075559346));
#56391=CARTESIAN_POINT('Ctrl Pts',(-2.0123635600116,38.5619472407965,13.6273203186704));
#56392=CARTESIAN_POINT('Ctrl Pts',(-2.07807778344679,38.6491924001683,12.9236404751012));
#56393=CARTESIAN_POINT('Ctrl Pts',(-1.70129941197566,38.7817933966652,11.8800756686743));
#56394=CARTESIAN_POINT('Ctrl Pts',(-0.530033200738386,38.9492091008822,
11.08169568024));
#56395=CARTESIAN_POINT('Ctrl Pts',(0.971298069111551,39.1268911505188,11.1790603421398));
#56396=CARTESIAN_POINT('Ctrl Pts',(2.12042035653773,39.3086127292394,12.2018320841821));
#56397=CARTESIAN_POINT('Ctrl Pts',(2.40348688354293,39.4945780381313,13.7505416118132));
#56398=CARTESIAN_POINT('Ctrl Pts',(1.65633965148822,39.6849522632223,15.1783632769377));
#56399=CARTESIAN_POINT('Ctrl Pts',(0.153843856789891,39.8798713203778,15.8603192806378));
#56400=CARTESIAN_POINT('Ctrl Pts',(-1.5117895621889,40.082247120361,15.4578268916728));
#56401=CARTESIAN_POINT('Ctrl Pts',(-2.23537839550422,40.2213853862984,14.5227049097605));
#56402=CARTESIAN_POINT('Ctrl Pts',(-2.40936181605783,40.2932541501529,13.973655276375));
#56403=CARTESIAN_POINT('Ctrl Pts',(-2.92629472497856,29.4179684483559,12.5960680234318));
#56404=CARTESIAN_POINT('Ctrl Pts',(-2.76138775259638,29.5026895656743,11.9375438339818));
#56405=CARTESIAN_POINT('Ctrl Pts',(-1.97719584338124,29.6696011470536,10.758957925939));
#56406=CARTESIAN_POINT('Ctrl Pts',(0.015402096841181,29.9170685318067,10.1112724173248));
#56407=CARTESIAN_POINT('Ctrl Pts',(1.95218792289976,30.160475832036,10.8151677022721));
#56408=CARTESIAN_POINT('Ctrl Pts',(3.03574990303937,30.4015596582338,12.5445656333449));
#56409=CARTESIAN_POINT('Ctrl Pts',(2.82945645491073,30.640115457994,14.5535401432159));
#56410=CARTESIAN_POINT('Ctrl Pts',(1.44515074433655,30.875958282617,15.9940382879077));
#56411=CARTESIAN_POINT('Ctrl Pts',(-0.503543948338917,31.1089181877232,
16.2753332904309));
#56412=CARTESIAN_POINT('Ctrl Pts',(-2.38977678760907,31.3643973010523,15.2037252502747));
#56413=CARTESIAN_POINT('Ctrl Pts',(-2.93561468713809,31.5906395890231,13.2892387819801));
#56414=CARTESIAN_POINT('Ctrl Pts',(-2.31979249603111,31.7888143338793,11.7809918345825));
#56415=CARTESIAN_POINT('Ctrl Pts',(-1.14312719269392,31.9850045730985,10.6794452452593));
#56416=CARTESIAN_POINT('Ctrl Pts',(0.979061516434718,32.2264711689806,10.501921826214));
#56417=CARTESIAN_POINT('Ctrl Pts',(2.73106530068917,32.5100878415069,12.2999468250575));
#56418=CARTESIAN_POINT('Ctrl Pts',(2.44365929372652,32.787535794297,14.7375889155685));
#56419=CARTESIAN_POINT('Ctrl Pts',(0.600736122514384,33.0362449227899,15.9254527144148));
#56420=CARTESIAN_POINT('Ctrl Pts',(-1.24209186022815,33.2579671676477,15.5536554486613));
#56421=CARTESIAN_POINT('Ctrl Pts',(-2.32798389553084,33.4542136726261,14.2984585777842));
#56422=CARTESIAN_POINT('Ctrl Pts',(-2.40845416463362,33.6472578291654,12.6659148675607));
#56423=CARTESIAN_POINT('Ctrl Pts',(-1.48469324396317,33.837219137125,11.3499581269052));
#56424=CARTESIAN_POINT('Ctrl Pts',(0.0293175997728939,34.0242361660808,
10.8866770372192));
#56425=CARTESIAN_POINT('Ctrl Pts',(1.4862388177494,34.2084721656006,11.4438683239473));
#56426=CARTESIAN_POINT('Ctrl Pts',(2.28151421256803,34.3901049120333,12.7599797022223));
#56427=CARTESIAN_POINT('Ctrl Pts',(2.10215476067396,34.5693315081312,14.2667586136253));
#56428=CARTESIAN_POINT('Ctrl Pts',(1.04753394126703,34.7463652392864,15.3317290281059));
#56429=CARTESIAN_POINT('Ctrl Pts',(-0.422450344249625,34.9214325139325,
15.521267960528));
#56430=CARTESIAN_POINT('Ctrl Pts',(-1.68574655436693,35.0947769203036,14.7745304523423));
#56431=CARTESIAN_POINT('Ctrl Pts',(-2.21864288212407,35.2666485810103,13.4204718245856));
#56432=CARTESIAN_POINT('Ctrl Pts',(-1.80906271554523,35.4373090813338,12.0348032210116));
#56433=CARTESIAN_POINT('Ctrl Pts',(-0.642302665493085,35.6070351214264,
11.1969323185357));
#56434=CARTESIAN_POINT('Ctrl Pts',(0.789341950991395,35.7760953652428,11.2553442171803));
#56435=CARTESIAN_POINT('Ctrl Pts',(1.75615824041296,35.9260332895441,12.0758907724877));
#56436=CARTESIAN_POINT('Ctrl Pts',(2.09012664466646,36.0571669403208,13.100444798061));
#56437=CARTESIAN_POINT('Ctrl Pts',(1.99369880813117,36.1508702947937,13.8633320157786));
#56438=CARTESIAN_POINT('Ctrl Pts',(1.59431997007155,36.2634037419873,14.6772718381349));
#56439=CARTESIAN_POINT('Ctrl Pts',(0.604424275445722,36.4136786035501,15.4777199943844));
#56440=CARTESIAN_POINT('Ctrl Pts',(-1.22018400546081,36.6212451623359,15.2974085367834));
#56441=CARTESIAN_POINT('Ctrl Pts',(-2.34526308970448,36.8494970463802,13.6232597140238));
#56442=CARTESIAN_POINT('Ctrl Pts',(-1.75053035885031,37.0802123528408,11.6681136226245));
#56443=CARTESIAN_POINT('Ctrl Pts',(-0.322212675623461,37.2555496913766,
11.076003369181));
#56444=CARTESIAN_POINT('Ctrl Pts',(0.617280561858399,37.3735732858669,11.232771728576));
#56445=CARTESIAN_POINT('Ctrl Pts',(1.06059919597652,37.432818095883,11.4099591023423));
#56446=CARTESIAN_POINT('Ctrl Pts',(1.45487125813752,37.4923081870011,11.6829606520691));
#56447=CARTESIAN_POINT('Ctrl Pts',(2.11223415117922,37.6117895248485,12.387289389157));
#56448=CARTESIAN_POINT('Ctrl Pts',(2.42724419526393,37.7929549642751,13.9563315796829));
#56449=CARTESIAN_POINT('Ctrl Pts',(1.28030667711334,37.998112670535,15.3568131965243));
#56450=CARTESIAN_POINT('Ctrl Pts',(0.107531631002896,38.1439241470239,15.611556567592));
#56451=CARTESIAN_POINT('Ctrl Pts',(-0.564258585336392,38.2278995539426,
15.5356922322688));
#56452=CARTESIAN_POINT('Ctrl Pts',(-1.3152122433605,38.3263864203009,15.2760924235049));
#56453=CARTESIAN_POINT('Ctrl Pts',(-1.8872897452656,38.4187324752531,14.7586807581235));
#56454=CARTESIAN_POINT('Ctrl Pts',(-2.19582729846917,38.504752419654,14.1397159838506));
#56455=CARTESIAN_POINT('Ctrl Pts',(-2.33973729772146,38.5623090280121,13.7004335879123));
#56456=CARTESIAN_POINT('Ctrl Pts',(-2.41926993441258,38.6635838660802,12.883831736637));
#56457=CARTESIAN_POINT('Ctrl Pts',(-1.98711383676784,38.8171825551677,11.6733444960647));
#56458=CARTESIAN_POINT('Ctrl Pts',(-0.638418491717066,39.0103777078726,
10.7475025569123));
#56459=CARTESIAN_POINT('Ctrl Pts',(1.08598908609963,39.2144028706223,10.8539224233017));
#56460=CARTESIAN_POINT('Ctrl Pts',(2.40151564006302,39.4218705163401,12.0176971105041));
#56461=CARTESIAN_POINT('Ctrl Pts',(2.72774771937741,39.6328055416103,13.7735316474361));
#56462=CARTESIAN_POINT('Ctrl Pts',(1.89084099938846,39.8472061753517,15.384068077044));
#56463=CARTESIAN_POINT('Ctrl Pts',(0.213666374113039,40.0650504690902,16.1509694319914));
#56464=CARTESIAN_POINT('Ctrl Pts',(-1.63409073970178,40.2893948535753,15.7098779610265));
#56465=CARTESIAN_POINT('Ctrl Pts',(-2.43214397021945,40.4423057604741,14.6842115864192));
#56466=CARTESIAN_POINT('Ctrl Pts',(-2.62499374027519,40.5209217307929,14.0844157329642));
#56467=CARTESIAN_POINT('Ctrl Pts',(-2.68901637473833,29.6258508348922,12.7013421571086));
#56468=CARTESIAN_POINT('Ctrl Pts',(-2.54192391625449,29.7034474026606,12.097134838509));
#56469=CARTESIAN_POINT('Ctrl Pts',(-1.83214692652542,29.8557848602106,11.0174310075307));
#56470=CARTESIAN_POINT('Ctrl Pts',(-0.0285161129234559,30.0801906025827,
10.4195088213662));
#56471=CARTESIAN_POINT('Ctrl Pts',(1.72137134294901,30.2996087065708,11.0434127561354));
#56472=CARTESIAN_POINT('Ctrl Pts',(2.70282908524349,30.5157541374752,12.5878192971209));
#56473=CARTESIAN_POINT('Ctrl Pts',(2.53070359956114,30.7285916653165,14.3815755859622));
#56474=CARTESIAN_POINT('Ctrl Pts',(1.30974294253613,30.9381078531812,15.6699224391317));
#56475=CARTESIAN_POINT('Ctrl Pts',(-0.413511312952687,31.1443123212953,
15.9314439612661));
#56476=CARTESIAN_POINT('Ctrl Pts',(-2.08540704977334,31.3697825407651,14.9981264331597));
#56477=CARTESIAN_POINT('Ctrl Pts',(-2.57894541282835,31.5689416522291,13.3163300617175));
#56478=CARTESIAN_POINT('Ctrl Pts',(-2.04836715080512,31.7431943139094,11.9855615775284));
#56479=CARTESIAN_POINT('Ctrl Pts',(-1.02209358337669,31.915639147058,11.0085761338793));
#56480=CARTESIAN_POINT('Ctrl Pts',(0.842033459968995,32.1278756568622,10.8362974613168));
#56481=CARTESIAN_POINT('Ctrl Pts',(2.39921103983848,32.3775873659353,12.4051582755859));
#56482=CARTESIAN_POINT('Ctrl Pts',(2.16635720525591,32.622691108358,14.5613661094194));
#56483=CARTESIAN_POINT('Ctrl Pts',(0.540386488651459,32.8435307255826,15.632877368845));
#56484=CARTESIAN_POINT('Ctrl Pts',(-1.10950126361728,33.0416124732336,15.3169281210652));
#56485=CARTESIAN_POINT('Ctrl Pts',(-2.09697701732676,33.2180215832585,14.1981125985888));
#56486=CARTESIAN_POINT('Ctrl Pts',(-2.18472365563727,33.3928081266097,12.7204450451649));
#56487=CARTESIAN_POINT('Ctrl Pts',(-1.35351454758958,33.5662121577014,11.5104403890166));
#56488=CARTESIAN_POINT('Ctrl Pts',(0.0370115243192905,33.7384826720109,
11.0694522056516));
#56489=CARTESIAN_POINT('Ctrl Pts',(1.39792058393044,33.9098837597389,11.5741517956677));
#56490=CARTESIAN_POINT('Ctrl Pts',(2.15835181775678,34.0806787676664,12.8043966294061));
#56491=CARTESIAN_POINT('Ctrl Pts',(2.00203261382117,34.2511380206756,14.2394096952522));
#56492=CARTESIAN_POINT('Ctrl Pts',(0.996842548153175,34.4215336196919,15.274581368401));
#56493=CARTESIAN_POINT('Ctrl Pts',(-0.434133599572046,34.5921366834918,
15.4730820151823));
#56494=CARTESIAN_POINT('Ctrl Pts',(-1.6880779760544,34.7632210511842,14.747614006186));
#56495=CARTESIAN_POINT('Ctrl Pts',(-2.23323794654136,34.9350518282015,13.3984655010846));
#56496=CARTESIAN_POINT('Ctrl Pts',(-1.83062979668189,35.1078910573438,11.9911944854927));
#56497=CARTESIAN_POINT('Ctrl Pts',(-0.64082647588313,35.2820001958536,11.121557924252));
#56498=CARTESIAN_POINT('Ctrl Pts',(0.847153684037699,35.4576194968682,11.1701958567181));
#56499=CARTESIAN_POINT('Ctrl Pts',(1.87051790069932,35.6152820367172,12.0255127586967));
#56500=CARTESIAN_POINT('Ctrl Pts',(2.23202389410442,35.7545179228302,13.1113548266299));
#56501=CARTESIAN_POINT('Ctrl Pts',(2.13370125415005,35.8547580895309,13.9282104490533));
#56502=CARTESIAN_POINT('Ctrl Pts',(1.70866506402261,35.975794476358,14.8059337544259));
#56503=CARTESIAN_POINT('Ctrl Pts',(0.642383871886817,36.1385566584636,15.6798513420792));
#56504=CARTESIAN_POINT('Ctrl Pts',(-1.35806494163484,36.3659313996715,15.4967024599889));
#56505=CARTESIAN_POINT('Ctrl Pts',(-2.61691525275619,36.6188288392025,13.6498169360587));
#56506=CARTESIAN_POINT('Ctrl Pts',(-1.96433530225319,36.8769243399619,11.4581771628379));
#56507=CARTESIAN_POINT('Ctrl Pts',(-0.3572000859169,37.0746016426084,10.7822822780298));
#56508=CARTESIAN_POINT('Ctrl Pts',(0.706764672491346,37.2081608564722,10.9558774430233));
#56509=CARTESIAN_POINT('Ctrl Pts',(1.20986625224818,37.2752972469721,11.1548842649935));
#56510=CARTESIAN_POINT('Ctrl Pts',(1.65832591006791,37.3427940166194,11.4630984176435));
#56511=CARTESIAN_POINT('Ctrl Pts',(2.40783774660274,37.4785106369379,12.260529333408));
#56512=CARTESIAN_POINT('Ctrl Pts',(2.7736527773654,37.6848149785396,14.0461024052735));
#56513=CARTESIAN_POINT('Ctrl Pts',(1.47014809441732,37.9189571306446,15.6491870045816));
#56514=CARTESIAN_POINT('Ctrl Pts',(0.131893950165078,38.0854371243222,15.9442174967714));
#56515=CARTESIAN_POINT('Ctrl Pts',(-0.635309864698155,38.1813018719843,
15.8599931067902));
#56516=CARTESIAN_POINT('Ctrl Pts',(-1.49341365143733,38.2937130208473,15.5663161027921));
#56517=CARTESIAN_POINT('Ctrl Pts',(-2.14779754192937,38.3990588725292,14.9779522740042));
#56518=CARTESIAN_POINT('Ctrl Pts',(-2.50162059102639,38.4970994089341,14.2735244117667));
#56519=CARTESIAN_POINT('Ctrl Pts',(-2.6671110354313,38.5626708152278,13.7735468571544));
#56520=CARTESIAN_POINT('Ctrl Pts',(-2.76046208537834,38.6779753319921,12.8440229981729));
#56521=CARTESIAN_POINT('Ctrl Pts',(-2.27292826156003,38.8525717136702,11.4666133234551));
#56522=CARTESIAN_POINT('Ctrl Pts',(-0.746803782695733,39.0715463148632,
10.4133094335848));
#56523=CARTESIAN_POINT('Ctrl Pts',(1.20068010308772,39.3019145907256,10.5287845044635));
#56524=CARTESIAN_POINT('Ctrl Pts',(2.68261092358831,39.5351283034409,11.833562136826));
#56525=CARTESIAN_POINT('Ctrl Pts',(3.05200855521192,39.7710330450894,13.796521683059));
#56526=CARTESIAN_POINT('Ctrl Pts',(2.12534234728874,40.0094600874809,15.5897728771503));
#56527=CARTESIAN_POINT('Ctrl Pts',(0.273488891436192,40.2502296178026,16.441619583345));
#56528=CARTESIAN_POINT('Ctrl Pts',(-1.75639191721469,40.4965425867897,15.9619290303801));
#56529=CARTESIAN_POINT('Ctrl Pts',(-2.62890954493469,40.66322613465,14.8457182630777));
#56530=CARTESIAN_POINT('Ctrl Pts',(-2.84062566449253,40.7485893114329,14.1951761895533));
#56531=CARTESIAN_POINT('Ctrl Pts',(-2.45173802449808,29.8337332214285,12.8066162907855));
#56532=CARTESIAN_POINT('Ctrl Pts',(-2.32246007991259,29.9042052396469,12.2567258430361));
#56533=CARTESIAN_POINT('Ctrl Pts',(-1.68709800966959,30.0419685733677,11.2759040891224));
#56534=CARTESIAN_POINT('Ctrl Pts',(-0.0724343226880954,30.2433126733586,
10.7277452254075));
#56535=CARTESIAN_POINT('Ctrl Pts',(1.49055476299827,30.4387415811056,11.2716578099989));
#56536=CARTESIAN_POINT('Ctrl Pts',(2.36990826744761,30.6299486167167,12.6310729608969));
#56537=CARTESIAN_POINT('Ctrl Pts',(2.23195074421154,30.8170678726391,14.2096110287086));
#56538=CARTESIAN_POINT('Ctrl Pts',(1.17433514073571,31.0002574237457,15.3458065903555));
#56539=CARTESIAN_POINT('Ctrl Pts',(-0.323478677566458,31.1797064548672,
15.5875546321013));
#56540=CARTESIAN_POINT('Ctrl Pts',(-1.78103731193763,31.3751677804782,14.7925276160446));
#56541=CARTESIAN_POINT('Ctrl Pts',(-2.22227613851859,31.5472437154351,13.3434213414549));
#56542=CARTESIAN_POINT('Ctrl Pts',(-1.77694180557915,31.6975742939395,12.1901313204743));
#56543=CARTESIAN_POINT('Ctrl Pts',(-0.901059974059453,31.8462737210174,
11.3377070224995));
#56544=CARTESIAN_POINT('Ctrl Pts',(0.705005403503267,32.0292801447437,11.1706730964197));
#56545=CARTESIAN_POINT('Ctrl Pts',(2.06735677898778,32.2450868903637,12.5103697261144));
#56546=CARTESIAN_POINT('Ctrl Pts',(1.88905511678531,32.4578464224189,14.3851433032702));
#56547=CARTESIAN_POINT('Ctrl Pts',(0.480036854788531,32.6508165283753,15.3403020232754));
#56548=CARTESIAN_POINT('Ctrl Pts',(-0.976910667006417,32.8252577788194,
15.080200793469));
#56549=CARTESIAN_POINT('Ctrl Pts',(-1.86597013912268,32.981829493891,14.0977666193934));
#56550=CARTESIAN_POINT('Ctrl Pts',(-1.9609931466409,33.138358424054,12.7749752227692));
#56551=CARTESIAN_POINT('Ctrl Pts',(-1.222335851216,33.295205178278,11.6709226511278));
#56552=CARTESIAN_POINT('Ctrl Pts',(0.0447054488656896,33.4527291779409,
11.2522273740842));
#56553=CARTESIAN_POINT('Ctrl Pts',(1.30960235011147,33.6112953538774,11.7044352673884));
#56554=CARTESIAN_POINT('Ctrl Pts',(2.03518942294553,33.7712526232996,12.8488135565898));
#56555=CARTESIAN_POINT('Ctrl Pts',(1.90191046696839,33.9329445332202,14.2120607768793));
#56556=CARTESIAN_POINT('Ctrl Pts',(0.946151155039321,34.0967020000973,15.2174337086961));
#56557=CARTESIAN_POINT('Ctrl Pts',(-0.445816854894472,34.262840853051,15.4248960698368));
#56558=CARTESIAN_POINT('Ctrl Pts',(-1.69040939774186,34.4316651820648,14.7206975600299));
#56559=CARTESIAN_POINT('Ctrl Pts',(-2.24783301095865,34.6034550753927,13.3764591775835));
#56560=CARTESIAN_POINT('Ctrl Pts',(-1.85219687781853,34.7784730333538,11.9475857499739));
#56561=CARTESIAN_POINT('Ctrl Pts',(-0.639350286273178,34.956965270281,11.0461835299682));
#56562=CARTESIAN_POINT('Ctrl Pts',(0.904965417084006,35.1391436284935,11.0850474962561));
#56563=CARTESIAN_POINT('Ctrl Pts',(1.98487756098567,35.3045307838904,11.9751347449056));
#56564=CARTESIAN_POINT('Ctrl Pts',(2.37392114354237,35.4518689053395,13.1222648551988));
#56565=CARTESIAN_POINT('Ctrl Pts',(2.27370370016894,35.5586458842682,13.9930888823279));
#56566=CARTESIAN_POINT('Ctrl Pts',(1.82301015797368,35.6881852107287,14.9345956707169));
#56567=CARTESIAN_POINT('Ctrl Pts',(0.680343468327914,35.8634347133772,15.8819826897739));
#56568=CARTESIAN_POINT('Ctrl Pts',(-1.49594587780887,36.1106176370072,15.6959963831942));
#56569=CARTESIAN_POINT('Ctrl Pts',(-2.8885674158079,36.388160632025,13.6763741580934));
#56570=CARTESIAN_POINT('Ctrl Pts',(-2.17814024565606,36.6736363270831,11.2482407030514));
#56571=CARTESIAN_POINT('Ctrl Pts',(-0.392187496210338,36.8936535938402,
10.4885611868789));
#56572=CARTESIAN_POINT('Ctrl Pts',(0.796248783124293,37.0427484270776,10.6789831574706));
#56573=CARTESIAN_POINT('Ctrl Pts',(1.35913330851984,37.1177763980612,10.8998094276445));
#56574=CARTESIAN_POINT('Ctrl Pts',(1.8617805619983,37.1932798462378,11.2432361832178));
#56575=CARTESIAN_POINT('Ctrl Pts',(2.70344134202624,37.3452317490274,12.133769277659));
#56576=CARTESIAN_POINT('Ctrl Pts',(3.12006135946686,37.576674992804,14.1358732308642));
#56577=CARTESIAN_POINT('Ctrl Pts',(1.65998951172128,37.8398015907541,15.9415608126388));
#56578=CARTESIAN_POINT('Ctrl Pts',(0.156256269327249,38.0269501016204,16.2768784259508));
#56579=CARTESIAN_POINT('Ctrl Pts',(-0.70636114405993,38.134704190026,16.1842939813117));
#56580=CARTESIAN_POINT('Ctrl Pts',(-1.67161505951417,38.2610396213937,15.8565397820794));
#56581=CARTESIAN_POINT('Ctrl Pts',(-2.40830533859313,38.3793852698053,15.1972237898848));
#56582=CARTESIAN_POINT('Ctrl Pts',(-2.80741388358363,38.4894463982141,14.4073328396828));
#56583=CARTESIAN_POINT('Ctrl Pts',(-2.99448477314115,38.5630326024434,13.8466601263963));
#56584=CARTESIAN_POINT('Ctrl Pts',(-3.10165423634411,38.692366797904,12.8042142597087));
#56585=CARTESIAN_POINT('Ctrl Pts',(-2.55874268635221,38.8879608721727,11.2598821508456));
#56586=CARTESIAN_POINT('Ctrl Pts',(-0.85518907367441,39.1327149218537,10.0791163102571));
#56587=CARTESIAN_POINT('Ctrl Pts',(1.3153711200758,39.3894263108291,10.2036465856254));
#56588=CARTESIAN_POINT('Ctrl Pts',(2.9637062071136,39.6483860905416,11.649427163148));
#56589=CARTESIAN_POINT('Ctrl Pts',(3.37626939104641,39.9092605485685,13.8195117186819));
#56590=CARTESIAN_POINT('Ctrl Pts',(2.35984369518899,40.1717139996104,15.7954776772565));
#56591=CARTESIAN_POINT('Ctrl Pts',(0.333311408759341,40.435408766515,16.7322697346985));
#56592=CARTESIAN_POINT('Ctrl Pts',(-1.87869309472757,40.703690320004,16.2139800997338));
#56593=CARTESIAN_POINT('Ctrl Pts',(-2.82567511964993,40.8841465088258,15.0072249397364));
#56594=CARTESIAN_POINT('Ctrl Pts',(-3.05625758870988,40.9762568920729,14.3059366461423));
#56595=CARTESIAN_POINT('Ctrl Pts',(-2.44274827128758,29.838337858154,12.7680189512445));
#56596=CARTESIAN_POINT('Ctrl Pts',(-2.42196823404112,29.8489350089282,12.6853451231868));
#56597=CARTESIAN_POINT('Ctrl Pts',(-2.39698720300911,29.8595261018564,12.6038716896438));
#56598=CARTESIAN_POINT('Ctrl Pts',(-2.36787154345866,29.8701089694672,12.5240551021937));
#56599=CARTESIAN_POINT('Ctrl Pts',(-2.31025919725116,29.8910497223843,12.3661187565886));
#56600=CARTESIAN_POINT('Ctrl Pts',(-2.23645492891969,29.9119582841016,12.2146710441957));
#56601=CARTESIAN_POINT('Ctrl Pts',(-2.14864857255502,29.932817762837,12.0724757850767));
#56602=CARTESIAN_POINT('Ctrl Pts',(-2.06203074205937,29.9533948926501,11.9322052470248));
#56603=CARTESIAN_POINT('Ctrl Pts',(-1.96178841628673,29.9739242552252,11.8009397307871));
#56604=CARTESIAN_POINT('Ctrl Pts',(-1.85006327768778,29.9943894361018,11.68130383456));
#56605=CARTESIAN_POINT('Ctrl Pts',(-1.79581670015234,30.0043260182813,11.6232162993635));
#56606=CARTESIAN_POINT('Ctrl Pts',(-1.73886360095515,30.0142474672897,11.5678698348704));
#56607=CARTESIAN_POINT('Ctrl Pts',(-1.67945137841709,30.0241518912863,11.515560943049));
#56608=CARTESIAN_POINT('Ctrl Pts',(-1.64243351653922,30.0303230221383,11.4829689400956));
#56609=CARTESIAN_POINT('Ctrl Pts',(-1.60446101984903,30.0364875434917,11.4515561004382));
#56610=CARTESIAN_POINT('Ctrl Pts',(-1.56561882847456,30.0426450002698,11.4213583465077));
#56611=CARTESIAN_POINT('Ctrl Pts',(-1.45706661729979,30.059853235048,11.3369647310686));
#56612=CARTESIAN_POINT('Ctrl Pts',(-1.34152150050918,30.0769963094119,11.2619269962897));
#56613=CARTESIAN_POINT('Ctrl Pts',(-1.22082683447683,30.09408254954,11.1971234500698));
#56614=CARTESIAN_POINT('Ctrl Pts',(-1.09768405092722,30.1115153594475,11.1310054572227));
#56615=CARTESIAN_POINT('Ctrl Pts',(-0.969181964878691,30.1288890092631,
11.0755416740165));
#56616=CARTESIAN_POINT('Ctrl Pts',(-0.837309041203365,30.1462130613069,
11.0316212565457));
#56617=CARTESIAN_POINT('Ctrl Pts',(-0.762543115457978,30.1560350077127,
11.0067203854662));
#56618=CARTESIAN_POINT('Ctrl Pts',(-0.686694124051804,30.1658410243016,
10.9855291380402));
#56619=CARTESIAN_POINT('Ctrl Pts',(-0.610126278689872,30.1756329466738,
10.9682023184446));
#56620=CARTESIAN_POINT('Ctrl Pts',(-0.474744503754916,30.1929463218185,
10.9375662782146));
#56621=CARTESIAN_POINT('Ctrl Pts',(-0.337116377370077,30.2102156045636,
10.9190142580986));
#56622=CARTESIAN_POINT('Ctrl Pts',(-0.199388743815463,30.2274514298725,
10.9122941898254));
#56623=CARTESIAN_POINT('Ctrl Pts',(-0.159208742874418,30.232479727094,10.9103337092554));
#56624=CARTESIAN_POINT('Ctrl Pts',(-0.119020181269218,30.2375051802885,
10.9093799156681));
#56625=CARTESIAN_POINT('Ctrl Pts',(-0.0788760557749174,30.242528061848,
10.9094257637442));
#56626=CARTESIAN_POINT('Ctrl Pts',(0.0678310697193201,30.2608842349174,
10.9095933160168));
#56627=CARTESIAN_POINT('Ctrl Pts',(0.214244052085658,30.2791737309075,10.9231318775133));
#56628=CARTESIAN_POINT('Ctrl Pts',(0.35778396157455,30.2973981541035,10.9498237837861));
#56629=CARTESIAN_POINT('Ctrl Pts',(0.429694880758075,30.3065282631323,10.9631959499081));
#56630=CARTESIAN_POINT('Ctrl Pts',(0.500884521694379,30.315642047562,10.979868550339));
#56631=CARTESIAN_POINT('Ctrl Pts',(0.571028493519116,30.3247397523455,10.9998093390544));
#56632=CARTESIAN_POINT('Ctrl Pts',(0.717608994568639,30.3437513094454,11.0414797880635));
#56633=CARTESIAN_POINT('Ctrl Pts',(0.859621141625087,30.3626926187303,11.0974254453251));
#56634=CARTESIAN_POINT('Ctrl Pts',(0.994627001001719,30.3815664136494,11.1660292863854));
#56635=CARTESIAN_POINT('Ctrl Pts',(1.12273921019856,30.3994764775102,11.2311300877743));
#56636=CARTESIAN_POINT('Ctrl Pts',(1.24454136035637,30.4173257532032,11.3076281085764));
#56637=CARTESIAN_POINT('Ctrl Pts',(1.35798428375087,30.4351169376783,11.3941042276715));
#56638=CARTESIAN_POINT('Ctrl Pts',(1.36408858742464,30.4360742718998,11.3987574618767));
#56639=CARTESIAN_POINT('Ctrl Pts',(1.3701686979687,30.4370314379966,11.4034395804063));
#56640=CARTESIAN_POINT('Ctrl Pts',(1.37622429993115,30.4379884364142,11.4081503599416));
#56641=CARTESIAN_POINT('Ctrl Pts',(1.44635601674792,30.4490717180495,11.4627072905992));
#56642=CARTESIAN_POINT('Ctrl Pts',(1.51327887302001,30.4601379581592,11.5211715138177));
#56643=CARTESIAN_POINT('Ctrl Pts',(1.57648124486681,30.4711863237015,11.5832172662626));
#56644=CARTESIAN_POINT('Ctrl Pts',(1.67691112938004,30.4887424065359,11.6818092584696));
#56645=CARTESIAN_POINT('Ctrl Pts',(1.76794459317642,30.5062533435147,11.7894464993758));
#56646=CARTESIAN_POINT('Ctrl Pts',(1.84846801190238,30.5237160607871,11.9040329244706));
#56647=CARTESIAN_POINT('Ctrl Pts',(1.92946837864217,30.5412822114265,12.0192980560675));
#56648=CARTESIAN_POINT('Ctrl Pts',(1.99983309317883,30.5587995713156,12.1415935824012));
#56649=CARTESIAN_POINT('Ctrl Pts',(2.05846999096913,30.5762652652364,12.2687553226759));
#56650=CARTESIAN_POINT('Ctrl Pts',(2.10222528400445,30.5892982970707,12.3636443672583));
#56651=CARTESIAN_POINT('Ctrl Pts',(2.13945102208768,30.6023025653927,12.4612422930058));
#56652=CARTESIAN_POINT('Ctrl Pts',(2.16971195499725,30.6152769569668,12.5606457179209));
#56653=CARTESIAN_POINT('Ctrl Pts',(2.18052629082065,30.6199136093796,12.5961694746484));
#56654=CARTESIAN_POINT('Ctrl Pts',(2.19045129627119,30.6245464467463,12.631923811111));
#56655=CARTESIAN_POINT('Ctrl Pts',(2.19948820868409,30.6291754219654,12.6678632506624));
#56656=CARTESIAN_POINT('Ctrl Pts',(2.23322305814674,30.6464554148488,12.8020253989318));
#56657=CARTESIAN_POINT('Ctrl Pts',(2.25463691153548,30.6636810587727,12.9390103776527));
#56658=CARTESIAN_POINT('Ctrl Pts',(2.26369433941869,30.6808537617852,13.0764695738017));
#56659=CARTESIAN_POINT('Ctrl Pts',(2.27294068816789,30.6983846549999,13.2167959095747));
#56660=CARTESIAN_POINT('Ctrl Pts',(2.26930961671449,30.7158603786077,13.3576149318399));
#56661=CARTESIAN_POINT('Ctrl Pts',(2.25281502826568,30.7332826999064,13.4964154152252));
#56662=CARTESIAN_POINT('Ctrl Pts',(2.24530913109389,30.741210763863,13.5595768671716));
#56663=CARTESIAN_POINT('Ctrl Pts',(2.23514026573485,30.7491277730461,13.6223203079521));
#56664=CARTESIAN_POINT('Ctrl Pts',(2.22231329878194,30.757033909312,13.6844096143821));
#56665=CARTESIAN_POINT('Ctrl Pts',(2.19406213713589,30.7744470307822,13.8211601836231));
#56666=CARTESIAN_POINT('Ctrl Pts',(2.15291407120517,30.7918073982712,13.9547354647172));
#56667=CARTESIAN_POINT('Ctrl Pts',(2.10014400624926,30.809117156191,14.0830014177723));
#56668=CARTESIAN_POINT('Ctrl Pts',(2.09289656173198,30.811494479589,14.1006174729923));
#56669=CARTESIAN_POINT('Ctrl Pts',(2.08542996170936,30.8138708486099,14.1181334333907));
#56670=CARTESIAN_POINT('Ctrl Pts',(2.07774756551514,30.8162462690207,14.1355438241986));
#56671=CARTESIAN_POINT('Ctrl Pts',(2.02467765540868,30.8326556476153,14.2558146162445));
#56672=CARTESIAN_POINT('Ctrl Pts',(1.96120585753199,30.8490178230599,14.3712740668969));
#56673=CARTESIAN_POINT('Ctrl Pts',(1.88835924779461,30.8653347463125,14.48005627632));
#56674=CARTESIAN_POINT('Ctrl Pts',(1.8418770836055,30.8757462933759,14.5494683263453));
#56675=CARTESIAN_POINT('Ctrl Pts',(1.79157910837346,30.8861394205734,14.6161618235882));
#56676=CARTESIAN_POINT('Ctrl Pts',(1.73774244381333,30.8965146738698,14.6796559969216));
#56677=CARTESIAN_POINT('Ctrl Pts',(1.65276651649938,30.9128909998771,14.7798753604747));
#56678=CARTESIAN_POINT('Ctrl Pts',(1.55897310285119,30.929222790903,14.8721217226433));
#56679=CARTESIAN_POINT('Ctrl Pts',(1.45818189935036,30.9455123441436,14.9552484286278));
#56680=CARTESIAN_POINT('Ctrl Pts',(1.35899011513395,30.9615434043345,15.0370560268728));
#56681=CARTESIAN_POINT('Ctrl Pts',(1.25302215367939,30.9775335605754,15.1100304370351));
#56682=CARTESIAN_POINT('Ctrl Pts',(1.14203363308923,30.9934850837824,15.1731235323804));
#56683=CARTESIAN_POINT('Ctrl Pts',(1.12828417076023,30.9954611878539,15.180939621225));
#56684=CARTESIAN_POINT('Ctrl Pts',(1.11445767230228,30.9974366990959,15.1886041290523));
#56685=CARTESIAN_POINT('Ctrl Pts',(1.10055748367544,30.9994116218689,15.1961151198218));
#56686=CARTESIAN_POINT('Ctrl Pts',(1.01945222563121,31.0109349634163,15.239940485137));
#56687=CARTESIAN_POINT('Ctrl Pts',(0.935736602491525,31.0224359380682,15.2785957311915));
#56688=CARTESIAN_POINT('Ctrl Pts',(0.850042474603389,31.0339140990372,15.3116694251567));
#56689=CARTESIAN_POINT('Ctrl Pts',(0.697695191681105,31.0543200087496,15.3704679395469));
#56690=CARTESIAN_POINT('Ctrl Pts',(0.53909305013005,31.0746538032239,15.4116226011244));
#56691=CARTESIAN_POINT('Ctrl Pts',(0.378368286442902,31.0949133795375,15.4348761056207));
#56692=CARTESIAN_POINT('Ctrl Pts',(0.210968964531451,31.1160142930453,15.4590952787925));
#56693=CARTESIAN_POINT('Ctrl Pts',(0.0412688522094594,31.1370346971868,
15.463895194311));
#56694=CARTESIAN_POINT('Ctrl Pts',(-0.126042124647733,31.1579724194978,
15.4490351635858));
#56695=CARTESIAN_POINT('Ctrl Pts',(-0.155858747679507,31.1617037477407,
15.4463869456225));
#56696=CARTESIAN_POINT('Ctrl Pts',(-0.185599483668016,31.16543245056,15.4431144788636));
#56697=CARTESIAN_POINT('Ctrl Pts',(-0.215237792528509,31.1691585162582,
15.4392165752889));
#56698=CARTESIAN_POINT('Ctrl Pts',(-0.241067690235736,31.1724057965361,
15.435819537655));
#56699=CARTESIAN_POINT('Ctrl Pts',(-0.26681979264175,31.1756510738736,15.4319474699778));
#56700=CARTESIAN_POINT('Ctrl Pts',(-0.292478263844604,31.1788943402646,
15.4276076162629));
#56701=CARTESIAN_POINT('Ctrl Pts',(-0.404942206081367,31.1931099387376,
15.4085855531928));
#56702=CARTESIAN_POINT('Ctrl Pts',(-0.515745857045101,31.2072831735665,
15.3805525726697));
#56703=CARTESIAN_POINT('Ctrl Pts',(-0.623480220379473,31.2214215485108,
15.3440899505627));
#56704=CARTESIAN_POINT('Ctrl Pts',(-0.732116475755987,31.2356782820499,
15.3073220837066));
#56705=CARTESIAN_POINT('Ctrl Pts',(-0.837630583917693,31.2498995747238,
15.2619832741019));
#56706=CARTESIAN_POINT('Ctrl Pts',(-0.938587011709799,31.264093035378,15.2087209901736));
#56707=CARTESIAN_POINT('Ctrl Pts',(-1.02874118139081,31.276767806942,15.1611577285975));
#56708=CARTESIAN_POINT('Ctrl Pts',(-1.11526033311846,31.2894203850643,15.1072768321492));
#56709=CARTESIAN_POINT('Ctrl Pts',(-1.19714077195967,31.3020560818323,15.0475692572935));
#56710=CARTESIAN_POINT('Ctrl Pts',(-1.2887998903919,31.3162008133813,14.9807310264236));
#56711=CARTESIAN_POINT('Ctrl Pts',(-1.37464498386398,31.330324398641,14.9065918943779));
#56712=CARTESIAN_POINT('Ctrl Pts',(-1.45380783575241,31.3444342064886,14.8264398549102));
#56713=CARTESIAN_POINT('Ctrl Pts',(-1.47311040217982,31.3478746523134,14.8068960912735));
#56714=CARTESIAN_POINT('Ctrl Pts',(-1.49201589588182,31.3513142777609,14.7869949336528));
#56715=CARTESIAN_POINT('Ctrl Pts',(-1.51051217688639,31.3547531871258,14.7667552233025));
#56716=CARTESIAN_POINT('Ctrl Pts',(-1.59341041892996,31.3701659904255,14.6760431278765));
#56717=CARTESIAN_POINT('Ctrl Pts',(-1.66839697393664,31.3855608261987,14.5782105380559));
#56718=CARTESIAN_POINT('Ctrl Pts',(-1.73426396540107,31.4009219748068,14.4748066584378));
#56719=CARTESIAN_POINT('Ctrl Pts',(-1.78136888379819,31.411907532756,14.4008571550058));
#56720=CARTESIAN_POINT('Ctrl Pts',(-1.8238100093497,31.4228758696061,14.324059535432));
#56721=CARTESIAN_POINT('Ctrl Pts',(-1.86115467699472,31.4338213642457,14.2449938261685));
#56722=CARTESIAN_POINT('Ctrl Pts',(-1.91439815727384,31.4494267040368,14.132267330061));
#56723=CARTESIAN_POINT('Ctrl Pts',(-1.95727950591873,31.4649855913012,14.0149300293415));
#56724=CARTESIAN_POINT('Ctrl Pts',(-1.98947075991055,31.4804820573484,13.8950139757259));
#56725=CARTESIAN_POINT('Ctrl Pts',(-2.02139363255055,31.4958493279778,13.7760976729303));
#56726=CARTESIAN_POINT('Ctrl Pts',(-2.04280382665317,31.5111552129038,13.654646979972));
#56727=CARTESIAN_POINT('Ctrl Pts',(-2.05343045590844,31.5263846168744,13.5326520605381));
#56728=CARTESIAN_POINT('Ctrl Pts',(-2.06203008984398,31.5387090610662,13.4339272792433));
#56729=CARTESIAN_POINT('Ctrl Pts',(-2.06356855702891,31.550983427265,13.3348465698476));
#56730=CARTESIAN_POINT('Ctrl Pts',(-2.05792666153141,31.5631999535903,13.2364585189257));
#56731=CARTESIAN_POINT('Ctrl Pts',(-2.05465700605132,31.570279813943,13.1794395560583));
#56732=CARTESIAN_POINT('Ctrl Pts',(-2.04897624877365,31.5773402524126,13.1226530653411));
#56733=CARTESIAN_POINT('Ctrl Pts',(-2.04096326871604,31.5843798059197,13.0662885712664));
#56734=CARTESIAN_POINT('Ctrl Pts',(-2.01971503210113,31.6030467809409,12.9168253131316));
#56735=CARTESIAN_POINT('Ctrl Pts',(-1.98187006982237,31.6219887666393,12.769983414429));
#56736=CARTESIAN_POINT('Ctrl Pts',(-1.92874023134007,31.6409279597721,12.6292055825379));
#56737=CARTESIAN_POINT('Ctrl Pts',(-1.88143333025758,31.657791450453,12.503856754871));
#56738=CARTESIAN_POINT('Ctrl Pts',(-1.82201060129564,31.6746528082086,12.3833146748631));
#56739=CARTESIAN_POINT('Ctrl Pts',(-1.75138393764471,31.6913244567762,12.269978209581));
#56740=CARTESIAN_POINT('Ctrl Pts',(-1.74242152111319,31.6934400637015,12.25559598398));
#56741=CARTESIAN_POINT('Ctrl Pts',(-1.73327864082616,31.6955526272835,12.2413297586781));
#56742=CARTESIAN_POINT('Ctrl Pts',(-1.72395920171074,31.6976617745041,12.2271828790924));
#56743=CARTESIAN_POINT('Ctrl Pts',(-1.64133954993399,31.7163600037378,12.1017665047132));
#56744=CARTESIAN_POINT('Ctrl Pts',(-1.54502778443523,31.7348138805689,11.9860617173297));
#56745=CARTESIAN_POINT('Ctrl Pts',(-1.43778289097727,31.7532672501976,11.8824706610493));
#56746=CARTESIAN_POINT('Ctrl Pts',(-1.33743650048451,31.7705336110932,11.7855430755028));
#56747=CARTESIAN_POINT('Ctrl Pts',(-1.22751550117257,31.7877994957642,11.6992227228509));
#56748=CARTESIAN_POINT('Ctrl Pts',(-1.11030205415889,31.8052541547949,11.6255177712851));
#56749=CARTESIAN_POINT('Ctrl Pts',(-1.10224399339743,31.8064541084403,11.6204507845761));
#56750=CARTESIAN_POINT('Ctrl Pts',(-1.09415148531256,31.8076549499904,11.6154434300847));
#56751=CARTESIAN_POINT('Ctrl Pts',(-1.08602527998824,31.808856739018,11.6104963641596));
#56752=CARTESIAN_POINT('Ctrl Pts',(-1.06702481750994,31.8116667279873,11.5989292751264));
#56753=CARTESIAN_POINT('Ctrl Pts',(-1.04783273466549,31.814473144343,11.587681052775));
#56754=CARTESIAN_POINT('Ctrl Pts',(-1.02845837876467,31.8172761349334,11.5767607902904));
#56755=CARTESIAN_POINT('Ctrl Pts',(-0.932432776307541,31.8311686669748,
11.5226364214886));
#56756=CARTESIAN_POINT('Ctrl Pts',(-0.831925975220367,31.8449771046457,
11.4765709736407));
#56757=CARTESIAN_POINT('Ctrl Pts',(-0.728418797670314,31.858718963986,11.4389723918552));
#56758=CARTESIAN_POINT('Ctrl Pts',(-0.621971400335677,31.8728511739056,
11.4003057866084));
#56759=CARTESIAN_POINT('Ctrl Pts',(-0.512351751409975,31.8869129825135,
11.3705945925219));
#56760=CARTESIAN_POINT('Ctrl Pts',(-0.401210092076274,31.9009225319703,
11.3502436116426));
#56761=CARTESIAN_POINT('Ctrl Pts',(-0.292675692779608,31.9146034329379,
11.3303700421991));
#56762=CARTESIAN_POINT('Ctrl Pts',(-0.182691166041161,31.9282345021004,
11.3194230274057));
#56763=CARTESIAN_POINT('Ctrl Pts',(-0.0728127663338156,31.9418316621078,
11.317735693246));
#56764=CARTESIAN_POINT('Ctrl Pts',(0.0437903629785101,31.9562609895356,
11.3159450916015));
#56765=CARTESIAN_POINT('Ctrl Pts',(0.160272454760996,31.9706521517856,11.3245826806894));
#56766=CARTESIAN_POINT('Ctrl Pts',(0.274808143983138,31.9850228251252,11.3431313784676));
#56767=CARTESIAN_POINT('Ctrl Pts',(0.381688629761689,31.9984330080815,11.360440339915));
#56768=CARTESIAN_POINT('Ctrl Pts',(0.486873017161923,32.0118253421599,11.3863791828463));
#56769=CARTESIAN_POINT('Ctrl Pts',(0.588897233847645,32.0252130151719,11.4204822323603));
#56770=CARTESIAN_POINT('Ctrl Pts',(0.596204612076822,32.0261718933038,11.4229248277525));
#56771=CARTESIAN_POINT('Ctrl Pts',(0.603495791630528,32.0271307470184,11.4254092871624));
#56772=CARTESIAN_POINT('Ctrl Pts',(0.610770241051819,32.0280895809249,11.4279354310596));
#56773=CARTESIAN_POINT('Ctrl Pts',(0.703451489250528,32.0403057526409,11.4601201581727));
#56774=CARTESIAN_POINT('Ctrl Pts',(0.793790709316334,32.052477282463,11.4991421659039));
#56775=CARTESIAN_POINT('Ctrl Pts',(0.880635423141395,32.0646158795974,11.5447626760918));
#56776=CARTESIAN_POINT('Ctrl Pts',(0.9709443166876,32.0772386775563,11.5922029590593));
#56777=CARTESIAN_POINT('Ctrl Pts',(1.0574729549825,32.0898258752061,11.6467793001905));
#56778=CARTESIAN_POINT('Ctrl Pts',(1.1392501848813,32.1023897826209,11.7076411287499));
#56779=CARTESIAN_POINT('Ctrl Pts',(1.22205093153323,32.1151109388168,11.7692646987039));
#56780=CARTESIAN_POINT('Ctrl Pts',(1.29997950085949,32.1278082267835,11.8373315058902));
#56781=CARTESIAN_POINT('Ctrl Pts',(1.37204471200167,32.140493354182,11.9109079805667));
#56782=CARTESIAN_POINT('Ctrl Pts',(1.44313956607502,32.153007676516,11.9834937490319));
#56783=CARTESIAN_POINT('Ctrl Pts',(1.50852688728067,32.165510166579,12.061441002164));
#56784=CARTESIAN_POINT('Ctrl Pts',(1.56728690689341,32.1780109501769,12.1438150100309));
#56785=CARTESIAN_POINT('Ctrl Pts',(1.5792518897322,32.1805564166727,12.160588380717));
#56786=CARTESIAN_POINT('Ctrl Pts',(1.59094222109023,32.1831018085915,12.1775451923054));
#56787=CARTESIAN_POINT('Ctrl Pts',(1.6023503594251,32.1856472054933,12.1946774015542));
#56788=CARTESIAN_POINT('Ctrl Pts',(1.65837536411523,32.198147568758,12.2788131365305));
#56789=CARTESIAN_POINT('Ctrl Pts',(1.70759069972438,32.2106481500889,12.3671801108344));
#56790=CARTESIAN_POINT('Ctrl Pts',(1.74962554120705,32.223157648365,12.4585038781202));
#56791=CARTESIAN_POINT('Ctrl Pts',(1.7711114065368,32.2295518058263,12.5051834918905));
#56792=CARTESIAN_POINT('Ctrl Pts',(1.79072200965433,32.2359482733096,12.5526353940308));
#56793=CARTESIAN_POINT('Ctrl Pts',(1.80841311943544,32.2423480863489,12.6006887752399));
#56794=CARTESIAN_POINT('Ctrl Pts',(1.84263044751356,32.2547263093723,12.693631407468));
#56795=CARTESIAN_POINT('Ctrl Pts',(1.8698543877587,32.2671506035997,12.7892761903362));
#56796=CARTESIAN_POINT('Ctrl Pts',(1.88961745460196,32.2796024374238,12.8864421648003));
#56797=CARTESIAN_POINT('Ctrl Pts',(1.9041958679578,32.288787650527,12.9581175657436));
#56798=CARTESIAN_POINT('Ctrl Pts',(1.91471528070787,32.2979878603318,13.0306196649456));
#56799=CARTESIAN_POINT('Ctrl Pts',(1.92100302500379,32.3071958304518,13.1034643427965));
#56800=CARTESIAN_POINT('Ctrl Pts',(1.929607641116,32.3197967003864,13.2031504081363));
#56801=CARTESIAN_POINT('Ctrl Pts',(1.93028508731108,32.332412077683,13.3034776626971));
#56802=CARTESIAN_POINT('Ctrl Pts',(1.92325688603922,32.3450239724341,13.4031967692286));
#56803=CARTESIAN_POINT('Ctrl Pts',(1.91616768070292,32.3577453371348,13.5037814273522));
#56804=CARTESIAN_POINT('Ctrl Pts',(1.90123879798748,32.3704631561137,13.603746011088));
#56805=CARTESIAN_POINT('Ctrl Pts',(1.87875011820394,32.3831596370036,13.7018138996038));
#56806=CARTESIAN_POINT('Ctrl Pts',(1.85671101886068,32.3956022973258,13.797921272655));
#56807=CARTESIAN_POINT('Ctrl Pts',(1.82741189099095,32.4080244653577,13.8922059091036));
#56808=CARTESIAN_POINT('Ctrl Pts',(1.79115973386811,32.4204100398556,13.9834895606174));
#56809=CARTESIAN_POINT('Ctrl Pts',(1.78287518904698,32.4232404603108,14.0043502089876));
#56810=CARTESIAN_POINT('Ctrl Pts',(1.77422769435617,32.4260689723749,14.0250542706439));
#56811=CARTESIAN_POINT('Ctrl Pts',(1.76522119840476,32.4288953886433,14.0455879505822));
#56812=CARTESIAN_POINT('Ctrl Pts',(1.73494946027227,32.4383952578036,14.114603712688));
#56813=CARTESIAN_POINT('Ctrl Pts',(1.70062150205205,32.4478714334674,14.181693485297));
#56814=CARTESIAN_POINT('Ctrl Pts',(1.66260821968523,32.4573169635298,14.2464279481209));
#56815=CARTESIAN_POINT('Ctrl Pts',(1.60951641862903,32.4705091998147,14.336840272649));
#56816=CARTESIAN_POINT('Ctrl Pts',(1.54901546843582,32.4836859639085,14.4230562711579));
#56817=CARTESIAN_POINT('Ctrl Pts',(1.48193781563378,32.4968456700971,14.5038310671862));
#56818=CARTESIAN_POINT('Ctrl Pts',(1.41238016704888,32.5104919171006,14.5875922699407));
#56819=CARTESIAN_POINT('Ctrl Pts',(1.33575093107518,32.52411982678,14.6655012662401));
#56820=CARTESIAN_POINT('Ctrl Pts',(1.25303283309184,32.5377272887717,14.7361782469831));
#56821=CARTESIAN_POINT('Ctrl Pts',(1.22974157025398,32.5415587958001,14.7560790446949));
#56822=CARTESIAN_POINT('Ctrl Pts',(1.20596785715059,32.5453886793708,14.7754065734702));
#56823=CARTESIAN_POINT('Ctrl Pts',(1.18173429457685,32.5492168868397,14.7941303591961));
#56824=CARTESIAN_POINT('Ctrl Pts',(1.09534944980345,32.5628632133734,14.860874624245));
#56825=CARTESIAN_POINT('Ctrl Pts',(1.00311865038569,32.5764882753401,14.9199439829922));
#56826=CARTESIAN_POINT('Ctrl Pts',(0.906622652138212,32.5900893986078,14.9707896365649));
#56827=CARTESIAN_POINT('Ctrl Pts',(0.81108545122454,32.603555379269,15.0211300808235));
#56828=CARTESIAN_POINT('Ctrl Pts',(0.711368759496013,32.6169978965796,15.0634089499655));
#56829=CARTESIAN_POINT('Ctrl Pts',(0.609029104604093,32.6304139103144,15.0971378774218));
#56830=CARTESIAN_POINT('Ctrl Pts',(0.511871895826564,32.643150541572,15.1291587832005));
#56831=CARTESIAN_POINT('Ctrl Pts',(0.412351793888545,32.6558632839847,15.1534736836662));
#56832=CARTESIAN_POINT('Ctrl Pts',(0.311802793307576,32.6685491354378,15.1697081915185));
#56833=CARTESIAN_POINT('Ctrl Pts',(0.208558134510143,32.6815750869367,15.1863779367599));
#56834=CARTESIAN_POINT('Ctrl Pts',(0.103949096816314,32.6945739279686,15.1946208003383));
#56835=CARTESIAN_POINT('Ctrl Pts',(-0.000630729312437852,32.7075672723265,
15.1939083446255));
#56836=CARTESIAN_POINT('Ctrl Pts',(-0.108565855569122,32.7209774902976,
15.1931730307495));
#56837=CARTESIAN_POINT('Ctrl Pts',(-0.216469187659061,32.7343818782785,
15.1828970181674));
#56838=CARTESIAN_POINT('Ctrl Pts',(-0.322774198061109,32.7478011574229,
15.1635746582427));
#56839=CARTESIAN_POINT('Ctrl Pts',(-0.429563384388784,32.7612815559057,
15.1441642928564));
#56840=CARTESIAN_POINT('Ctrl Pts',(-0.534738489088845,32.7747769922733,
15.1156245921934));
#56841=CARTESIAN_POINT('Ctrl Pts',(-0.636690050051503,32.7883051517794,
15.0785041312197));
#56842=CARTESIAN_POINT('Ctrl Pts',(-0.729799500108899,32.8006600336469,
15.044603073948));
#56843=CARTESIAN_POINT('Ctrl Pts',(-0.820219225911066,32.8130421740493,
15.0035455200694));
#56844=CARTESIAN_POINT('Ctrl Pts',(-0.90672160595063,32.8254625387955,14.9557872785077));
#56845=CARTESIAN_POINT('Ctrl Pts',(-0.992623125835422,32.8377966295886,
14.9083607737653));
#56846=CARTESIAN_POINT('Ctrl Pts',(-1.07491738151294,32.8500285650052,14.8544705816298));
#56847=CARTESIAN_POINT('Ctrl Pts',(-1.15243288169613,32.8622104398304,14.7944450637593));
#56848=CARTESIAN_POINT('Ctrl Pts',(-1.15914061004674,32.8632645865099,14.7892508140024));
#56849=CARTESIAN_POINT('Ctrl Pts',(-1.16581252965613,32.86431835469,14.7840106424791));
#56850=CARTESIAN_POINT('Ctrl Pts',(-1.17244786797231,32.8653717760498,14.7787247741989));
#56851=CARTESIAN_POINT('Ctrl Pts',(-1.24908094773948,32.8775379866099,14.7176770406468));
#56852=CARTESIAN_POINT('Ctrl Pts',(-1.32083679360994,32.8896584354967,14.6505303561686));
#56853=CARTESIAN_POINT('Ctrl Pts',(-1.3870201362254,32.9017786069914,14.5782416312114));
#56854=CARTESIAN_POINT('Ctrl Pts',(-1.45282361211481,32.9138292134009,14.5063678155078));
#56855=CARTESIAN_POINT('Ctrl Pts',(-1.51311717830069,32.9258795506478,14.4294104113911));
#56856=CARTESIAN_POINT('Ctrl Pts',(-1.5672020311935,32.9379683126868,14.3483584759315));
#56857=CARTESIAN_POINT('Ctrl Pts',(-1.62047948805187,32.949876609808,14.268516509766));
#56858=CARTESIAN_POINT('Ctrl Pts',(-1.66773094040675,32.9618221869895,14.1847013810081));
#56859=CARTESIAN_POINT('Ctrl Pts',(-1.70829171716438,32.9738362028301,14.0979083023651));
#56860=CARTESIAN_POINT('Ctrl Pts',(-1.71708953534038,32.976442097869,14.0790824862472));
#56861=CARTESIAN_POINT('Ctrl Pts',(-1.7255726275999,32.9790511909054,14.0601167502762));
#56862=CARTESIAN_POINT('Ctrl Pts',(-1.73373432566236,32.981663763421,14.0410215561971));
#56863=CARTESIAN_POINT('Ctrl Pts',(-1.77656675841202,32.9953744931885,13.9408103489242));
#56864=CARTESIAN_POINT('Ctrl Pts',(-1.8109159376224,33.0090631847566,13.8368942431182));
#56865=CARTESIAN_POINT('Ctrl Pts',(-1.83585249184895,33.0227376840039,13.7306630244244));
#56866=CARTESIAN_POINT('Ctrl Pts',(-1.86269959886161,33.0374598762242,13.6162927361141));
#56867=CARTESIAN_POINT('Ctrl Pts',(-1.878634692129,33.0521656495421,13.4992392863367));
#56868=CARTESIAN_POINT('Ctrl Pts',(-1.883725334327,33.0668631824395,13.3816644247428));
#56869=CARTESIAN_POINT('Ctrl Pts',(-1.88546801883735,33.071894603216,13.3414149076608));
#56870=CARTESIAN_POINT('Ctrl Pts',(-1.88594018725234,33.0769250387225,13.3011045808627));
#56871=CARTESIAN_POINT('Ctrl Pts',(-1.88514570139615,33.0819547552135,13.2608209354391));
#56872=CARTESIAN_POINT('Ctrl Pts',(-1.88282680887894,33.0966351574431,13.1432437083416));
#56873=CARTESIAN_POINT('Ctrl Pts',(-1.86971355688606,33.1113096089662,13.0258933344761));
#56874=CARTESIAN_POINT('Ctrl Pts',(-1.84584025664775,33.1259822303606,12.9108475780895));
#56875=CARTESIAN_POINT('Ctrl Pts',(-1.83891474206808,33.1302386780396,12.8774734297634));
#56876=CARTESIAN_POINT('Ctrl Pts',(-1.8310840467261,33.1344949564262,12.8442932527195));
#56877=CARTESIAN_POINT('Ctrl Pts',(-1.8223498458544,33.1387511284261,12.8113577463972));
#56878=CARTESIAN_POINT('Ctrl Pts',(-1.82073903271537,33.1395360769154,12.8052835849365));
#56879=CARTESIAN_POINT('Ctrl Pts',(-1.81909742698397,33.1403210550766,12.7992172539458));
#56880=CARTESIAN_POINT('Ctrl Pts',(-1.81742503007901,33.1411060616138,12.7931590691915));
#56881=CARTESIAN_POINT('Ctrl Pts',(-1.78341351893815,33.157070727961,12.6699538553742));
#56882=CARTESIAN_POINT('Ctrl Pts',(-1.73666257370683,33.1730470449138,12.5501188149469));
#56883=CARTESIAN_POINT('Ctrl Pts',(-1.67844835802018,33.1890253691034,12.4360236729034));
#56884=CARTESIAN_POINT('Ctrl Pts',(-1.61980323463689,33.2051219665153,12.3210839867176));
#56885=CARTESIAN_POINT('Ctrl Pts',(-1.54952556666188,33.221220599866,12.211970972486));
#56886=CARTESIAN_POINT('Ctrl Pts',(-1.46896446342868,33.2373124658053,12.111082370773));
#56887=CARTESIAN_POINT('Ctrl Pts',(-1.43201039406103,33.2446939427999,12.0648039034174));
#56888=CARTESIAN_POINT('Ctrl Pts',(-1.39289306392564,33.2520740104948,12.0202554815113));
#56889=CARTESIAN_POINT('Ctrl Pts',(-1.35174485230098,33.25945189343,11.9776655040048));
#56890=CARTESIAN_POINT('Ctrl Pts',(-1.28441558434642,33.2715240452313,11.9079771288725));
#56891=CARTESIAN_POINT('Ctrl Pts',(-1.21164898751506,33.2835903304337,11.8435330764808));
#56892=CARTESIAN_POINT('Ctrl Pts',(-1.1344413983556,33.2956475381849,11.7849360748564));
#56893=CARTESIAN_POINT('Ctrl Pts',(-1.04148000362451,33.3101649562435,11.7143826609062));
#56894=CARTESIAN_POINT('Ctrl Pts',(-0.941877414275713,33.3247120648009,
11.6522161259233));
#56895=CARTESIAN_POINT('Ctrl Pts',(-0.83734978707031,33.3392824870544,11.5995868551751));
#56896=CARTESIAN_POINT('Ctrl Pts',(-0.744966745445939,33.3521600387746,
11.5530723380069));
#56897=CARTESIAN_POINT('Ctrl Pts',(-0.648737949632954,33.3650557953688,
11.5140077083481));
#56898=CARTESIAN_POINT('Ctrl Pts',(-0.549871499941875,33.3779650443768,
11.4831626102079));
#56899=CARTESIAN_POINT('Ctrl Pts',(-0.438312571300595,33.3925315833127,
11.4483576170772));
#56900=CARTESIAN_POINT('Ctrl Pts',(-0.323396167968655,33.4071153107072,
11.4240193541309));
#56901=CARTESIAN_POINT('Ctrl Pts',(-0.207184444008096,33.4217090321553,
11.4102901892089));
#56902=CARTESIAN_POINT('Ctrl Pts',(-0.123751815319772,33.4321863962393,
11.4004335217393));
#56903=CARTESIAN_POINT('Ctrl Pts',(-0.0396519762126377,33.4426689014923,
11.3960441046249));
#56904=CARTESIAN_POINT('Ctrl Pts',(0.0443529895522357,33.4531537285205,
11.3971580099636));
#56905=CARTESIAN_POINT('Ctrl Pts',(0.161853849845441,33.4678192448338,11.3987160706615));
#56906=CARTESIAN_POINT('Ctrl Pts',(0.279401484675227,33.4825002502203,11.4109723352032));
#56907=CARTESIAN_POINT('Ctrl Pts',(0.394948071017141,33.4971989223994,11.4341338283749));
#56908=CARTESIAN_POINT('Ctrl Pts',(0.514048517686451,33.5123496808717,11.4580076983836));
#56909=CARTESIAN_POINT('Ctrl Pts',(0.63102160742065,33.5275192259303,11.4934689829188));
#56910=CARTESIAN_POINT('Ctrl Pts',(0.743781082859313,33.5427073447054,11.5396253014745));
#56911=CARTESIAN_POINT('Ctrl Pts',(0.855553128008094,33.5577624617219,11.5853774309647));
#56912=CARTESIAN_POINT('Ctrl Pts',(0.963183479473169,33.572835827222,11.6416380078028));
#56913=CARTESIAN_POINT('Ctrl Pts',(1.06464020010924,33.5879246703803,11.707488152597));
#56914=CARTESIAN_POINT('Ctrl Pts',(1.11819237326572,33.5958890549621,11.7422460112612));
#56915=CARTESIAN_POINT('Ctrl Pts',(1.17002466495448,33.6038577087437,11.779674763905));
#56916=CARTESIAN_POINT('Ctrl Pts',(1.2198406027858,33.6118299347862,11.8196338311499));
#56917=CARTESIAN_POINT('Ctrl Pts',(1.23077720451177,33.6135801590095,11.8284064533834));
#56918=CARTESIAN_POINT('Ctrl Pts',(1.24161921329453,33.6153307798915,11.8373021545097));
#56919=CARTESIAN_POINT('Ctrl Pts',(1.25236346546683,33.6170817856626,11.8463195476875));
#56920=CARTESIAN_POINT('Ctrl Pts',(1.34818864605216,33.6326985490752,11.9267433236571));
#56921=CARTESIAN_POINT('Ctrl Pts',(1.43623527057538,33.6483458472314,12.0168506157618));
#56922=CARTESIAN_POINT('Ctrl Pts',(1.51497948581664,33.6640158393301,12.114719325643));
#56923=CARTESIAN_POINT('Ctrl Pts',(1.59432892343071,33.6798062698606,12.2133402473869));
#56924=CARTESIAN_POINT('Ctrl Pts',(1.66423150396073,33.6956197442337,12.3198408590462));
#56925=CARTESIAN_POINT('Ctrl Pts',(1.72316823935652,33.7114492409151,12.4322227978785));
#56926=CARTESIAN_POINT('Ctrl Pts',(1.75583922438526,33.7202241627973,12.4945205925635));
#56927=CARTESIAN_POINT('Ctrl Pts',(1.78514127758445,33.729004025984,12.5586252496628));
#56928=CARTESIAN_POINT('Ctrl Pts',(1.81082243501288,33.7377877653431,12.6241947529243));
#56929=CARTESIAN_POINT('Ctrl Pts',(1.84406234849377,33.7491568298857,12.7090633816638));
#56930=CARTESIAN_POINT('Ctrl Pts',(1.87123582420496,33.760532379776,12.7963857198891));
#56931=CARTESIAN_POINT('Ctrl Pts',(1.89221941649866,33.7719123269017,12.8852340922583));
#56932=CARTESIAN_POINT('Ctrl Pts',(1.91979504835822,33.7868673083046,13.0019943673095));
#56933=CARTESIAN_POINT('Ctrl Pts',(1.93667000491097,33.8018622643777,13.1216242748102));
#56934=CARTESIAN_POINT('Ctrl Pts',(1.94246100425419,33.8168893377621,13.2420074258643));
#56935=CARTESIAN_POINT('Ctrl Pts',(1.94791422876764,33.8310399187047,13.3553689221148));
#56936=CARTESIAN_POINT('Ctrl Pts',(1.94353893132823,33.8452189754154,13.4693969758569));
#56937=CARTESIAN_POINT('Ctrl Pts',(1.92905494235689,33.85941951799,13.5823104299314));
#56938=CARTESIAN_POINT('Ctrl Pts',(1.91373349001847,33.8744411350781,13.7017525330971));
#56939=CARTESIAN_POINT('Ctrl Pts',(1.88710026331683,33.8894867991923,13.8199459974798));
#56940=CARTESIAN_POINT('Ctrl Pts',(1.84989387070444,33.9045476817596,13.9348618491369));
#56941=CARTESIAN_POINT('Ctrl Pts',(1.82591104626476,33.9142557581721,14.0089353215195));
#56942=CARTESIAN_POINT('Ctrl Pts',(1.79753617067424,33.9239701471483,14.0816471192062));
#56943=CARTESIAN_POINT('Ctrl Pts',(1.7649772391965,33.9336883689359,14.1524592800049));
#56944=CARTESIAN_POINT('Ctrl Pts',(1.71738845989287,33.9478927144375,14.2559597371549));
#56945=CARTESIAN_POINT('Ctrl Pts',(1.66083542209935,33.9621352393784,14.3556498016173));
#56946=CARTESIAN_POINT('Ctrl Pts',(1.59586126139288,33.9764102392548,14.449816937735));
#56947=CARTESIAN_POINT('Ctrl Pts',(1.58716866014967,33.978320027397,14.4624151360893));
#56948=CARTESIAN_POINT('Ctrl Pts',(1.57832540722809,33.9802303931489,14.4749144652241));
#56949=CARTESIAN_POINT('Ctrl Pts',(1.56933287225282,33.9821413194679,14.4873108132865));
#56950=CARTESIAN_POINT('Ctrl Pts',(1.5019605950614,33.9964580230454,14.5801845357819));
#56951=CARTESIAN_POINT('Ctrl Pts',(1.42620477900407,34.0108063984482,14.6672769838926));
#56952=CARTESIAN_POINT('Ctrl Pts',(1.34333605945917,34.0251777889364,14.747330386248));
#56953=CARTESIAN_POINT('Ctrl Pts',(1.26766405149073,34.0383010998975,14.8204315724882));
#56954=CARTESIAN_POINT('Ctrl Pts',(1.18606193623612,34.0514435727229,14.8876625063986));
#56955=CARTESIAN_POINT('Ctrl Pts',(1.09953154996117,34.0645967734331,14.9480816900527));
#56956=CARTESIAN_POINT('Ctrl Pts',(1.02738510699994,34.0755635180144,14.9984573947608));
#56957=CARTESIAN_POINT('Ctrl Pts',(0.951813477723499,34.0865376889597,15.0440978257523));
#56958=CARTESIAN_POINT('Ctrl Pts',(0.873525894036174,34.0975135015488,15.0845424501372));
#56959=CARTESIAN_POINT('Ctrl Pts',(0.787769630833399,34.1095364128321,15.1288455144358));
#56960=CARTESIAN_POINT('Ctrl Pts',(0.698708695046754,34.12160084351,15.1671765144296));
#56961=CARTESIAN_POINT('Ctrl Pts',(0.607157766262662,34.1337023607202,15.1988590604772));
#56962=CARTESIAN_POINT('Ctrl Pts',(0.57205723886613,34.1383420693722,15.2110061144755));
#56963=CARTESIAN_POINT('Ctrl Pts',(0.536591208756782,34.1429871705226,15.2221756861145));
#56964=CARTESIAN_POINT('Ctrl Pts',(0.500807535832861,34.1476371941549,15.2323291427542));
#56965=CARTESIAN_POINT('Ctrl Pts',(0.406723295000572,34.1598632712329,15.2590251239576));
#56966=CARTESIAN_POINT('Ctrl Pts',(0.310439509622285,34.1721237919042,15.27869614959));
#56967=CARTESIAN_POINT('Ctrl Pts',(0.213020585639545,34.1844061040476,15.2912643606359));
#56968=CARTESIAN_POINT('Ctrl Pts',(0.115639236100466,34.1966836789076,15.3038277241274));
#56969=CARTESIAN_POINT('Ctrl Pts',(0.017124022998488,34.2089830255298,15.3092926359667));
#56970=CARTESIAN_POINT('Ctrl Pts',(-0.0814129547883811,34.2212857146177,
15.3075978231872));
#56971=CARTESIAN_POINT('Ctrl Pts',(-0.179346761227685,34.2335130956363,
15.3059133848126));
#56972=CARTESIAN_POINT('Ctrl Pts',(-0.277301313740047,34.2457437686831,
15.2971556374653));
#56973=CARTESIAN_POINT('Ctrl Pts',(-0.374145174267623,34.2579540207722,
15.2812962511804));
#56974=CARTESIAN_POINT('Ctrl Pts',(-0.389865757957571,34.2599361008833,
15.2787218101368));
#56975=CARTESIAN_POINT('Ctrl Pts',(-0.405557004185956,34.2619176309858,
15.2759603217363));
#56976=CARTESIAN_POINT('Ctrl Pts',(-0.421213997593287,34.2638984958387,
15.2730117706197));
#56977=CARTESIAN_POINT('Ctrl Pts',(-0.528484965322997,34.2774700216221,
15.2528103230338));
#56978=CARTESIAN_POINT('Ctrl Pts',(-0.634408224075304,34.2910967149944,
15.2241298800896));
#56979=CARTESIAN_POINT('Ctrl Pts',(-0.737525673046703,34.3047670915336,
15.1869054434143));
#56980=CARTESIAN_POINT('Ctrl Pts',(-0.765105948676489,34.3084234344385,
15.1769492213209));
#56981=CARTESIAN_POINT('Ctrl Pts',(-0.792485268849016,34.3120828755897,
15.1663819527556));
#56982=CARTESIAN_POINT('Ctrl Pts',(-0.819635259472576,34.3157451367173,
15.1552028010352));
#56983=CARTESIAN_POINT('Ctrl Pts',(-0.924165319229743,34.3298451922132,
15.1121619980538));
#56984=CARTESIAN_POINT('Ctrl Pts',(-1.02529795183968,34.3439874686245,15.0600469893191));
#56985=CARTESIAN_POINT('Ctrl Pts',(-1.12166850413609,34.3581527213183,14.9997648521849));
#56986=CARTESIAN_POINT('Ctrl Pts',(-1.2180390564325,34.3723179740122,14.9394827150508));
#56987=CARTESIAN_POINT('Ctrl Pts',(-1.30964599532968,34.3865061987767,14.8710331408026));
#56988=CARTESIAN_POINT('Ctrl Pts',(-1.39511168057473,34.4006927818407,14.7953790118328));
#56989=CARTESIAN_POINT('Ctrl Pts',(-1.45900496212402,34.4112985277999,14.7388207504818));
#56990=CARTESIAN_POINT('Ctrl Pts',(-1.51946550307793,34.4219032450792,14.6782371434713));
#56991=CARTESIAN_POINT('Ctrl Pts',(-1.57592471557605,34.432494682015,14.6140865465418));
#56992=CARTESIAN_POINT('Ctrl Pts',(-1.64030234483855,34.444571570272,14.5409388145178));
#56993=CARTESIAN_POINT('Ctrl Pts',(-1.69979667045605,34.456725822996,14.4632206315149));
#56994=CARTESIAN_POINT('Ctrl Pts',(-1.75355035369345,34.4689396714447,14.3814837337769));
#56995=CARTESIAN_POINT('Ctrl Pts',(-1.77885528939668,34.4746894290626,14.3430054971748));
#56996=CARTESIAN_POINT('Ctrl Pts',(-1.80288757563606,34.4804523129785,14.3036372784954));
#56997=CARTESIAN_POINT('Ctrl Pts',(-1.8255558752418,34.4862260391538,14.2634401176226));
#56998=CARTESIAN_POINT('Ctrl Pts',(-1.87419314992058,34.4986141896016,14.1771927859445));
#56999=CARTESIAN_POINT('Ctrl Pts',(-1.91655123609662,34.5110526305101,14.0871258591308));
#57000=CARTESIAN_POINT('Ctrl Pts',(-1.95232334393682,34.5235145318038,13.9942455739322));
#57001=CARTESIAN_POINT('Ctrl Pts',(-1.9881487064555,34.5359949853883,13.9012270159277));
#57002=CARTESIAN_POINT('Ctrl Pts',(-2.01736730005151,34.5484989653802,13.8053868797165));
#57003=CARTESIAN_POINT('Ctrl Pts',(-2.03967635811788,34.5609937519823,13.7077874915789));
#57004=CARTESIAN_POINT('Ctrl Pts',(-2.06191038413533,34.573446514872,13.6105163594368));
#57005=CARTESIAN_POINT('Ctrl Pts',(-2.07728016684792,34.5858901361617,13.511498321101));
#57006=CARTESIAN_POINT('Ctrl Pts',(-2.08550835859991,34.5982866090211,13.4118309465753));
#57007=CARTESIAN_POINT('Ctrl Pts',(-2.08686771362955,34.6003345933461,13.3953651967562));
#57008=CARTESIAN_POINT('Ctrl Pts',(-2.08803222165053,34.6023812785661,13.3788818146423));
#57009=CARTESIAN_POINT('Ctrl Pts',(-2.08900072334537,34.6044264787915,13.362385851687));
#57010=CARTESIAN_POINT('Ctrl Pts',(-2.09505087338117,34.6172026755528,13.2593369345847));
#57011=CARTESIAN_POINT('Ctrl Pts',(-2.09379275692534,34.6300709245727,13.1555496116575));
#57012=CARTESIAN_POINT('Ctrl Pts',(-2.08489850256943,34.6430128630142,13.0521857152708));
#57013=CARTESIAN_POINT('Ctrl Pts',(-2.07600424821351,34.6559548014558,12.9488218188842));
#57014=CARTESIAN_POINT('Ctrl Pts',(-2.05947303519056,34.6689704298532,12.8458825466293));
#57015=CARTESIAN_POINT('Ctrl Pts',(-2.03502060520216,34.6820384222808,12.7445609029007));
#57016=CARTESIAN_POINT('Ctrl Pts',(-2.01078754340807,34.6949891788384,12.6441482381995));
#57017=CARTESIAN_POINT('Ctrl Pts',(-1.97877453893384,34.7079913583367,12.5453256332383));
#57018=CARTESIAN_POINT('Ctrl Pts',(-1.93960121624929,34.721021283644,12.4491543456727));
#57019=CARTESIAN_POINT('Ctrl Pts',(-1.90066566372906,34.7339721212643,12.3535667885971));
#57020=CARTESIAN_POINT('Ctrl Pts',(-1.85465672409422,34.7469503629058,12.2605997747385));
#57021=CARTESIAN_POINT('Ctrl Pts',(-1.80223260483086,34.7599300032335,12.1712873498045));
#57022=CARTESIAN_POINT('Ctrl Pts',(-1.77511199135633,34.7666447714225,12.1250832782981));
#57023=CARTESIAN_POINT('Ctrl Pts',(-1.74627526809702,34.7733598693225,12.0798570375199));
#57024=CARTESIAN_POINT('Ctrl Pts',(-1.7158184117152,34.7800714128729,12.0357491438004));
#57025=CARTESIAN_POINT('Ctrl Pts',(-1.65345660760091,34.7938136047442,11.9454362174255));
#57026=CARTESIAN_POINT('Ctrl Pts',(-1.58402369302544,34.8075815743873,11.8594688178559));
#57027=CARTESIAN_POINT('Ctrl Pts',(-1.50826910434011,34.8213778510084,11.779084292947));
#57028=CARTESIAN_POINT('Ctrl Pts',(-1.43238478499475,34.8351977539221,11.6985621085556));
#57029=CARTESIAN_POINT('Ctrl Pts',(-1.3501581967844,34.8490460627832,11.6236427885949));
#57030=CARTESIAN_POINT('Ctrl Pts',(-1.26237706405678,34.8629276107525,11.5555321768382));
#57031=CARTESIAN_POINT('Ctrl Pts',(-1.22019422314461,34.869598328154,11.5228019190836));
#57032=CARTESIAN_POINT('Ctrl Pts',(-1.17672911137699,34.8762767549658,11.4916433157153));
#57033=CARTESIAN_POINT('Ctrl Pts',(-1.13207088971541,34.8829636125416,11.462186235914));
#57034=CARTESIAN_POINT('Ctrl Pts',(-1.0391654958356,34.8968747158901,11.4009047629921));
#57035=CARTESIAN_POINT('Ctrl Pts',(-0.941096546679065,34.9108221682274,
11.3469906830712));
#57036=CARTESIAN_POINT('Ctrl Pts',(-0.839269891050978,34.924814044204,11.3007966198672));
#57037=CARTESIAN_POINT('Ctrl Pts',(-0.756439250854729,34.9361957009768,
11.2632201738487));
#57038=CARTESIAN_POINT('Ctrl Pts',(-0.671122639783257,34.9476067954979,
11.2307510245286));
#57039=CARTESIAN_POINT('Ctrl Pts',(-0.584072161961717,34.9590527132191,
11.2035539354153));
#57040=CARTESIAN_POINT('Ctrl Pts',(-0.488628455221114,34.9716022229025,
11.1737345586296));
#57041=CARTESIAN_POINT('Ctrl Pts',(-0.390726602951209,34.9841200356052,
11.1503536926679));
#57042=CARTESIAN_POINT('Ctrl Pts',(-0.291416536690167,34.9966287025253,
11.1336927912598));
#57043=CARTESIAN_POINT('Ctrl Pts',(-0.191662750098081,35.0091932585414,
11.1169574484485));
#57044=CARTESIAN_POINT('Ctrl Pts',(-0.0904893084113526,35.0217485877063,
11.1070017677132));
#57045=CARTESIAN_POINT('Ctrl Pts',(0.0110549133221134,35.034321965954,11.1040609066534));
#57046=CARTESIAN_POINT('Ctrl Pts',(0.111663768368748,35.0467795255076,11.1011471351061));
#57047=CARTESIAN_POINT('Ctrl Pts',(0.212635769790514,35.0592548166334,11.1051189721538));
#57048=CARTESIAN_POINT('Ctrl Pts',(0.312980537213609,35.0717785761591,11.1161641752063));
#57049=CARTESIAN_POINT('Ctrl Pts',(0.354563238902439,35.0769684008979,11.1207412886465));
#57050=CARTESIAN_POINT('Ctrl Pts',(0.39603865297577,35.0821665979529,11.1265326427681));
#57051=CARTESIAN_POINT('Ctrl Pts',(0.437338275206494,35.0873755604995,11.1335498581336));
#57052=CARTESIAN_POINT('Ctrl Pts',(0.537969048597282,35.1000677330017,11.1506480244398));
#57053=CARTESIAN_POINT('Ctrl Pts',(0.637552716687777,35.1128235383902,11.1750251213683));
#57054=CARTESIAN_POINT('Ctrl Pts',(0.735171372142909,35.1256804609482,11.2060979429132));
#57055=CARTESIAN_POINT('Ctrl Pts',(0.773683488592057,35.1307527219461,11.2183566665779));
#57056=CARTESIAN_POINT('Ctrl Pts',(0.811890305850365,35.1358407657357,11.2316573654777));
#57057=CARTESIAN_POINT('Ctrl Pts',(0.849737658810937,35.1409470657411,11.2459637968681));
#57058=CARTESIAN_POINT('Ctrl Pts',(0.947707097989359,35.1541649345924,11.2829965864906));
#57059=CARTESIAN_POINT('Ctrl Pts',(1.0433989754111,35.1672842684333,11.327229906532));
#57060=CARTESIAN_POINT('Ctrl Pts',(1.1357935857753,35.1803579422975,11.378068771267));
#57061=CARTESIAN_POINT('Ctrl Pts',(1.22877077542611,35.1935140500998,11.4292281922492));
#57062=CARTESIAN_POINT('Ctrl Pts',(1.31840915379737,35.2066239238815,11.4870753732865));
#57063=CARTESIAN_POINT('Ctrl Pts',(1.4037225305533,35.2197481807154,11.5510048238215));
#57064=CARTESIAN_POINT('Ctrl Pts',(1.48969353405072,35.2329736041257,11.615427065966));
#57065=CARTESIAN_POINT('Ctrl Pts',(1.57127304533912,35.2462136380493,11.6860245968205));
#57066=CARTESIAN_POINT('Ctrl Pts',(1.64750089208874,35.2595370691274,11.7621973008937));
#57067=CARTESIAN_POINT('Ctrl Pts',(1.71688416473284,35.2716641760898,11.8315303821772));
#57068=CARTESIAN_POINT('Ctrl Pts',(1.78183472093203,35.283860465245,11.9054822158681));
#57069=CARTESIAN_POINT('Ctrl Pts',(1.84165717256322,35.2961825380909,11.9836242232698));
#57070=CARTESIAN_POINT('Ctrl Pts',(1.89007784060195,35.3061561012357,12.046872854797));
#57071=CARTESIAN_POINT('Ctrl Pts',(1.93513961567416,35.3162121575097,12.1128669436503));
#57072=CARTESIAN_POINT('Ctrl Pts',(1.9767321176533,35.3263827890248,12.1811670535072));
#57073=CARTESIAN_POINT('Ctrl Pts',(2.04732472143141,35.3436448272904,12.2970889712496));
#57074=CARTESIAN_POINT('Ctrl Pts',(2.10750078383594,35.3608568635775,12.4198550539506));
#57075=CARTESIAN_POINT('Ctrl Pts',(2.15653326971147,35.3779993238944,12.5473875107866));
#57076=CARTESIAN_POINT('Ctrl Pts',(2.20490833640097,35.3949119410347,12.6732100342494));
#57077=CARTESIAN_POINT('Ctrl Pts',(2.24243678990059,35.4117568252121,12.803673780373));
#57078=CARTESIAN_POINT('Ctrl Pts',(2.26837232234277,35.4285132705407,12.9367900497168));
#57079=CARTESIAN_POINT('Ctrl Pts',(2.28097724825192,35.436657069105,13.0014858764218));
#57080=CARTESIAN_POINT('Ctrl Pts',(2.29084311874697,35.4447799499595,13.066808175581));
#57081=CARTESIAN_POINT('Ctrl Pts',(2.29787990453227,35.4528793804603,13.1325273964819));
#57082=CARTESIAN_POINT('Ctrl Pts',(2.30982452833639,35.4666277953348,13.244082784739));
#57083=CARTESIAN_POINT('Ctrl Pts',(2.3138378028793,35.4805105310546,13.3567710192135));
#57084=CARTESIAN_POINT('Ctrl Pts',(2.309470334525,35.4945049157327,13.4693880880878));
#57085=CARTESIAN_POINT('Ctrl Pts',(2.3077677789381,35.4999602999246,13.513289223537));
#57086=CARTESIAN_POINT('Ctrl Pts',(2.30479214590153,35.5054326336883,13.5571793091859));
#57087=CARTESIAN_POINT('Ctrl Pts',(2.30051887843916,35.5109205083467,13.6009863588756));
#57088=CARTESIAN_POINT('Ctrl Pts',(2.28952026653867,35.5250452978801,13.7137377235598));
#57089=CARTESIAN_POINT('Ctrl Pts',(2.26992175982311,35.5392731515272,13.8259386567223));
#57090=CARTESIAN_POINT('Ctrl Pts',(2.2422376442469,35.5535788875883,13.9363518841804));
#57091=CARTESIAN_POINT('Ctrl Pts',(2.22466925455505,35.5626573335029,14.0064203175309));
#57092=CARTESIAN_POINT('Ctrl Pts',(2.20384570461758,35.5717671119679,14.0757687630312));
#57093=CARTESIAN_POINT('Ctrl Pts',(2.17990896535464,35.5809014569378,14.1440838286613));
#57094=CARTESIAN_POINT('Ctrl Pts',(2.14635034373073,35.5937075464916,14.2398595904938));
#57095=CARTESIAN_POINT('Ctrl Pts',(2.10651065587268,35.6064377600827,14.3336643377711));
#57096=CARTESIAN_POINT('Ctrl Pts',(2.06068536231229,35.6190900050523,14.4247557447538));
#57097=CARTESIAN_POINT('Ctrl Pts',(2.0287405426921,35.6279098870855,14.4882555794286));
#57098=CARTESIAN_POINT('Ctrl Pts',(1.99388597884577,35.6366918727779,14.5504365845222));
#57099=CARTESIAN_POINT('Ctrl Pts',(1.95620943234504,35.6454351476554,14.6110386821541));
#57100=CARTESIAN_POINT('Ctrl Pts',(1.89941929774933,35.6586139499401,14.7023846679447));
#57101=CARTESIAN_POINT('Ctrl Pts',(1.83649321646789,35.6720045307769,14.7902445266212));
#57102=CARTESIAN_POINT('Ctrl Pts',(1.76776005935783,35.6855415139324,14.8735973647063));
#57103=CARTESIAN_POINT('Ctrl Pts',(1.69878203809106,35.6991267230403,14.9572471500475));
#57104=CARTESIAN_POINT('Ctrl Pts',(1.62395523020483,35.7128593721322,15.0363564294859));
#57105=CARTESIAN_POINT('Ctrl Pts',(1.54366230589861,35.7266690324148,15.1098820020039));
#57106=CARTESIAN_POINT('Ctrl Pts',(1.53437299398596,35.7282667104528,15.1183883801509));
#57107=CARTESIAN_POINT('Ctrl Pts',(1.52501057637243,35.7298654145769,15.1268200222165));
#57108=CARTESIAN_POINT('Ctrl Pts',(1.51557569077079,35.7314650320618,15.1351753160586));
#57109=CARTESIAN_POINT('Ctrl Pts',(1.4330658322613,35.7454539894191,15.208243940505));
#57110=CARTESIAN_POINT('Ctrl Pts',(1.34500969791181,35.7595131518695,15.2754720724962));
#57111=CARTESIAN_POINT('Ctrl Pts',(1.25246982545419,35.7735646598664,15.3363452613834));
#57112=CARTESIAN_POINT('Ctrl Pts',(1.16060338199091,35.787513912558,15.3967754653248));
#57113=CARTESIAN_POINT('Ctrl Pts',(1.06431899290268,35.8014556019814,15.4509418100831));
#57114=CARTESIAN_POINT('Ctrl Pts',(0.964698194865835,35.815309503174,15.498368792203));
#57115=CARTESIAN_POINT('Ctrl Pts',(0.895275351458995,35.8249638849098,15.5314192798306));
#57116=CARTESIAN_POINT('Ctrl Pts',(0.82423316316403,35.8345755496419,15.5611975082448));
#57117=CARTESIAN_POINT('Ctrl Pts',(0.751946479824379,35.8441162488206,15.5875547054492));
#57118=CARTESIAN_POINT('Ctrl Pts',(0.645472004486849,35.8581691959538,15.6263774680114));
#57119=CARTESIAN_POINT('Ctrl Pts',(0.535849238912219,35.8723112393953,15.6580927100499));
#57120=CARTESIAN_POINT('Ctrl Pts',(0.42419202346629,35.8865253717002,15.6821180843425));
#57121=CARTESIAN_POINT('Ctrl Pts',(0.31002375074205,35.9010591653924,15.7066837648817));
#57122=CARTESIAN_POINT('Ctrl Pts',(0.193729462674567,35.9156683284442,15.7232090673018));
#57123=CARTESIAN_POINT('Ctrl Pts',(0.0765387231235699,35.9303339918097,
15.7311091299798));
#57124=CARTESIAN_POINT('Ctrl Pts',(0.002302801237708,35.9396241374661,15.7361135222901));
#57125=CARTESIAN_POINT('Ctrl Pts',(-0.0722921063576966,35.9489369413425,
15.7376576178362));
#57126=CARTESIAN_POINT('Ctrl Pts',(-0.146928518635182,35.9582674656181,
15.7356023796385));
#57127=CARTESIAN_POINT('Ctrl Pts',(-0.263654577318513,35.9728597442512,
15.7323881327697));
#57128=CARTESIAN_POINT('Ctrl Pts',(-0.380481892466343,35.987495395391,15.7203675215166));
#57129=CARTESIAN_POINT('Ctrl Pts',(-0.496150807410281,36.0021549648982,
15.6999452043));
#57130=CARTESIAN_POINT('Ctrl Pts',(-0.61201357287156,36.0168391025026,15.6794886611485));
#57131=CARTESIAN_POINT('Ctrl Pts',(-0.726712811269431,36.0315472370525,
15.6506025637267));
#57132=CARTESIAN_POINT('Ctrl Pts',(-0.838990868169627,36.0462591964778,
15.6137450642979));
#57133=CARTESIAN_POINT('Ctrl Pts',(-0.948098901842568,36.0605557830833,
15.577928187877));
#57134=CARTESIAN_POINT('Ctrl Pts',(-1.05491953278933,36.074855977133,15.5345842283449));
#57135=CARTESIAN_POINT('Ctrl Pts',(-1.15832294224657,36.0891407325821,15.4841752608046));
#57136=CARTESIAN_POINT('Ctrl Pts',(-1.21709541126144,36.0972599072923,15.4555237927496));
#57137=CARTESIAN_POINT('Ctrl Pts',(-1.2747644534909,36.1053740850071,15.4245906504352));
#57138=CARTESIAN_POINT('Ctrl Pts',(-1.3311281040744,36.1134796962468,15.3914659386035));
#57139=CARTESIAN_POINT('Ctrl Pts',(-1.41782930028274,36.1259481255129,15.3405119618804));
#57140=CARTESIAN_POINT('Ctrl Pts',(-1.50170128593061,36.1382167085011,15.284051015274));
#57141=CARTESIAN_POINT('Ctrl Pts',(-1.58201073434815,36.1504911003073,15.2224436482496));
#57142=CARTESIAN_POINT('Ctrl Pts',(-1.6623201827657,36.1627654921136,15.1608362812252));
#57143=CARTESIAN_POINT('Ctrl Pts',(-1.73906775288705,36.1750457212604,15.0940833947862));
#57144=CARTESIAN_POINT('Ctrl Pts',(-1.81156843952179,36.1875454226321,15.0225226611708));
#57145=CARTESIAN_POINT('Ctrl Pts',(-2.47103868931813,45.357839245202,11.1663882923918));
#57146=CARTESIAN_POINT('Ctrl Pts',(-1.99114009165886,45.4494249512674,10.6112764926156));
#57147=CARTESIAN_POINT('Ctrl Pts',(-0.656229362054297,45.6306288317189,
9.85038323946594));
#57148=CARTESIAN_POINT('Ctrl Pts',(1.60578641174988,45.9008551469128,10.1937481051622));
#57149=CARTESIAN_POINT('Ctrl Pts',(3.16037369235198,46.168185471263,11.8386895923522));
#57150=CARTESIAN_POINT('Ctrl Pts',(3.3728671597752,46.4341378756677,14.0798681764736));
#57151=CARTESIAN_POINT('Ctrl Pts',(2.17028512256952,46.698340609565,15.9655340763413));
#57152=CARTESIAN_POINT('Ctrl Pts',(0.0773201111634047,46.9604366782597,
16.7050573116982));
#57153=CARTESIAN_POINT('Ctrl Pts',(-2.00387794111447,47.2200782068993,16.0098611361731));
#57154=CARTESIAN_POINT('Ctrl Pts',(-3.34740888722012,47.5054828051186,13.9930892616668));
#57155=CARTESIAN_POINT('Ctrl Pts',(-2.93140857362281,47.7587315319614,11.8055319684882));
#57156=CARTESIAN_POINT('Ctrl Pts',(-1.72466235251619,47.9530101577763,10.7548847842084));
#57157=CARTESIAN_POINT('Ctrl Pts',(-0.905164464225716,48.0632135666546,
10.4157099355514));
#57158=CARTESIAN_POINT('Ctrl Pts',(-0.0334441790798442,48.1728678644929,
10.2648701783387));
#57159=CARTESIAN_POINT('Ctrl Pts',(1.06769726965044,48.3088763459659,10.443208013525));
#57160=CARTESIAN_POINT('Ctrl Pts',(2.16156427422588,48.4703285006447,11.1953451702359));
#57161=CARTESIAN_POINT('Ctrl Pts',(2.81802762807523,48.6299590209922,12.3269396060619));
#57162=CARTESIAN_POINT('Ctrl Pts',(2.974514026944,48.8402909027348,14.0516430479399));
#57163=CARTESIAN_POINT('Ctrl Pts',(1.72043482337078,49.0983753877132,15.9523988771148));
#57164=CARTESIAN_POINT('Ctrl Pts',(-0.70728189930077,49.3748770710527,16.207909252572));
#57165=CARTESIAN_POINT('Ctrl Pts',(-2.33912222864486,49.6201738927179,14.9205630045294));
#57166=CARTESIAN_POINT('Ctrl Pts',(-2.78256706964164,49.8362026228524,13.148512449524));
#57167=CARTESIAN_POINT('Ctrl Pts',(-2.05415847844708,50.0474536524228,11.514775663013));
#57168=CARTESIAN_POINT('Ctrl Pts',(-0.512761213530604,50.2539262122794,
10.6922180050034));
#57169=CARTESIAN_POINT('Ctrl Pts',(1.17083770430258,50.4556490739761,10.9841762156852));
#57170=CARTESIAN_POINT('Ctrl Pts',(2.10312483044396,50.6198448176698,12.013824403281));
#57171=CARTESIAN_POINT('Ctrl Pts',(2.35342838183667,50.7489044626185,13.0320232163277));
#57172=CARTESIAN_POINT('Ctrl Pts',(2.28589273790721,50.8445659743367,13.8060200922857));
#57173=CARTESIAN_POINT('Ctrl Pts',(1.97284878571603,50.9391095454929,14.5069955309913));
#57174=CARTESIAN_POINT('Ctrl Pts',(1.2838833323123,51.0637032271118,15.2491157464924));
#57175=CARTESIAN_POINT('Ctrl Pts',(0.0559027336712221,51.2167483942124,
15.6590700042074));
#57176=CARTESIAN_POINT('Ctrl Pts',(-1.37675602413113,51.3962674798406,15.1503729666643));
#57177=CARTESIAN_POINT('Ctrl Pts',(-2.17574776022075,51.571865285863,13.8974135292959));
#57178=CARTESIAN_POINT('Ctrl Pts',(-2.03865062584112,51.7437789248239,12.4485435208909));
#57179=CARTESIAN_POINT('Ctrl Pts',(-1.06007972412022,51.9122667185844,11.4111368238105));
#57180=CARTESIAN_POINT('Ctrl Pts',(0.323635636007865,52.0776220908781,11.1968858539816));
#57181=CARTESIAN_POINT('Ctrl Pts',(1.52332687478463,52.240143186124,11.8680021577416));
#57182=CARTESIAN_POINT('Ctrl Pts',(2.11356223942205,52.417937375268,13.2553851052613));
#57183=CARTESIAN_POINT('Ctrl Pts',(1.49608399064576,52.6104181125041,14.8368849598406));
#57184=CARTESIAN_POINT('Ctrl Pts',(-0.243334784363091,52.8174139408632,
15.4076636569798));
#57185=CARTESIAN_POINT('Ctrl Pts',(-1.76917851156779,53.0222997300687,14.4310069810067));
#57186=CARTESIAN_POINT('Ctrl Pts',(-1.99104716195834,53.2259785337442,12.6470991678428));
#57187=CARTESIAN_POINT('Ctrl Pts',(-0.746338998632108,53.4293896457581,
11.343670999249));
#57188=CARTESIAN_POINT('Ctrl Pts',(0.74872675692419,53.5994584735607,11.4560002347665));
#57189=CARTESIAN_POINT('Ctrl Pts',(1.47519207623104,53.7191897502424,12.1215132223007));
#57190=CARTESIAN_POINT('Ctrl Pts',(1.7087783122541,53.7792769266905,12.5452878158475));
#57191=CARTESIAN_POINT('Ctrl Pts',(1.79980890764077,53.8136861005568,12.8059893771045));
#57192=CARTESIAN_POINT('Ctrl Pts',(1.95692666292302,53.8998241968474,13.4795291061361));
#57193=CARTESIAN_POINT('Ctrl Pts',(1.69127030416465,54.0125675191503,14.435805987514));
#57194=CARTESIAN_POINT('Ctrl Pts',(0.76219646379196,54.1530019391863,15.11932691662));
#57195=CARTESIAN_POINT('Ctrl Pts',(-0.379980518396253,54.2946959603654,
15.3548666883329));
#57196=CARTESIAN_POINT('Ctrl Pts',(-1.60280114527924,54.4504647292807,14.7380741477106));
#57197=CARTESIAN_POINT('Ctrl Pts',(-2.119511433952,54.6214417658209,13.3998286427744));
#57198=CARTESIAN_POINT('Ctrl Pts',(-1.84805341422617,54.7704180108169,12.1845180963029));
#57199=CARTESIAN_POINT('Ctrl Pts',(-1.15058454821746,54.8857021713809,11.5177200975638));
#57200=CARTESIAN_POINT('Ctrl Pts',(-0.607910694635962,54.9584165398788,
11.3000406935775));
#57201=CARTESIAN_POINT('Ctrl Pts',(-0.384084660020667,54.9872958550554,
11.240750409036));
#57202=CARTESIAN_POINT('Ctrl Pts',(-0.155451669286306,55.0162505934249,
11.2001667278884));
#57203=CARTESIAN_POINT('Ctrl Pts',(0.136236732568041,55.0525881695729,11.185156402327));
#57204=CARTESIAN_POINT('Ctrl Pts',(0.603307105703516,55.1110457654735,11.2384407723527));
#57205=CARTESIAN_POINT('Ctrl Pts',(1.16239040941207,55.1847091028723,11.4506788670608));
#57206=CARTESIAN_POINT('Ctrl Pts',(1.90854826039242,55.3038866520108,12.0680945425943));
#57207=CARTESIAN_POINT('Ctrl Pts',(2.38882431469308,55.4553824358178,13.2562329772914));
#57208=CARTESIAN_POINT('Ctrl Pts',(1.95430780379812,55.6414163194288,14.7710242764318));
#57209=CARTESIAN_POINT('Ctrl Pts',(0.650492552779959,55.8318581708404,15.7187839912398));
#57210=CARTESIAN_POINT('Ctrl Pts',(-0.999202214726866,56.0268417285148,
15.6629550914944));
#57211=CARTESIAN_POINT('Ctrl Pts',(-2.2951136204419,56.2264758696457,14.5776809166717));
#57212=CARTESIAN_POINT('Ctrl Pts',(-2.5366416601022,56.3627161449828,13.4507655792797));
#57213=CARTESIAN_POINT('Ctrl Pts',(-2.46825949632321,56.4316314111821,12.90289162838));
#57214=CARTESIAN_POINT('Ctrl Pts',(-2.30565904042138,45.5654608789673,11.3661975024612));
#57215=CARTESIAN_POINT('Ctrl Pts',(-1.86577890195538,45.6499463997848,10.8516310251641));
#57216=CARTESIAN_POINT('Ctrl Pts',(-0.641242660313543,45.816608935898,10.1460569362544));
#57217=CARTESIAN_POINT('Ctrl Pts',(1.42969953062964,46.063816421259,10.4501733917502));
#57218=CARTESIAN_POINT('Ctrl Pts',(2.85245049954171,46.3071808960092,11.9406026138709));
#57219=CARTESIAN_POINT('Ctrl Pts',(3.05558437982819,46.5482196321492,13.9708984611688));
#57220=CARTESIAN_POINT('Ctrl Pts',(1.97903980437475,46.7867293039377,15.6790675364112));
#57221=CARTESIAN_POINT('Ctrl Pts',(0.0997422031405143,47.0225246979377,
16.354867546064));
#57222=CARTESIAN_POINT('Ctrl Pts',(-1.77088105666362,47.2554368056156,15.7419502206933));
#57223=CARTESIAN_POINT('Ctrl Pts',(-2.98401760525766,47.51086192616,13.9441081235967));
#57224=CARTESIAN_POINT('Ctrl Pts',(-2.62426560333524,47.7370551058119,11.9878883323483));
#57225=CARTESIAN_POINT('Ctrl Pts',(-1.55347588276063,47.9104210528862,11.0433510057079));
#57226=CARTESIAN_POINT('Ctrl Pts',(-0.824271881901055,48.0087424085889,
10.735919171988));
#57227=CARTESIAN_POINT('Ctrl Pts',(-0.0474552309468843,48.1065648952709,
10.5962142445523));
#57228=CARTESIAN_POINT('Ctrl Pts',(0.936010136026854,48.2279002678246,10.7487686199371));
#57229=CARTESIAN_POINT('Ctrl Pts',(1.91678341410505,48.3719800511437,11.4133823393088));
#57230=CARTESIAN_POINT('Ctrl Pts',(2.50997870829564,48.5145262047812,12.4199295311954));
#57231=CARTESIAN_POINT('Ctrl Pts',(2.66061544197642,48.7025352976575,13.9605793923149));
#57232=CARTESIAN_POINT('Ctrl Pts',(1.55042730245208,48.933693873436,15.6717751203539));
#57233=CARTESIAN_POINT('Ctrl Pts',(-0.631040980438996,49.1823525442919,
15.9192311347505));
#57234=CARTESIAN_POINT('Ctrl Pts',(-2.11517929405329,49.4040324788164,14.7675119280446));
#57235=CARTESIAN_POINT('Ctrl Pts',(-2.53099693059846,49.6002436807348,13.161177305678));
#57236=CARTESIAN_POINT('Ctrl Pts',(-1.87785797182935,49.7932546220171,11.6628436256107));
#57237=CARTESIAN_POINT('Ctrl Pts',(-0.466299333288858,49.9831863709573,
10.8940833058664));
#57238=CARTESIAN_POINT('Ctrl Pts',(1.09679132198281,50.1701774524991,11.1511725961288));
#57239=CARTESIAN_POINT('Ctrl Pts',(1.97694730497387,50.323687610072,12.1062558702991));
#57240=CARTESIAN_POINT('Ctrl Pts',(2.2200660234861,50.4451967754876,13.0632246528585));
#57241=CARTESIAN_POINT('Ctrl Pts',(2.16179884776509,50.5357033682336,13.7960456107689));
#57242=CARTESIAN_POINT('Ctrl Pts',(1.86920332174121,50.6256087662742,14.4650083959747));
#57243=CARTESIAN_POINT('Ctrl Pts',(1.21604893869049,50.7447179086067,15.179547360442));
#57244=CARTESIAN_POINT('Ctrl Pts',(0.0359275727558463,50.8922368104418,
15.5854154119932));
#57245=CARTESIAN_POINT('Ctrl Pts',(-1.36579376356038,51.067295942977,15.1021068853405));
#57246=CARTESIAN_POINT('Ctrl Pts',(-2.16587787421377,51.2406358526476,13.8723096856617));
#57247=CARTESIAN_POINT('Ctrl Pts',(-2.04192832362877,51.4125085559133,12.4223936332311));
#57248=CARTESIAN_POINT('Ctrl Pts',(-1.0600778722892,51.5831728303628,11.362580099908));
#57249=CARTESIAN_POINT('Ctrl Pts',(0.358428055786465,51.7529069167004,11.1300684810987));
#57250=CARTESIAN_POINT('Ctrl Pts',(1.61263354696483,51.9219803428794,11.817572736803));
#57251=CARTESIAN_POINT('Ctrl Pts',(2.24744796919837,52.1094203899309,13.2748358269744));
#57252=CARTESIAN_POINT('Ctrl Pts',(1.6028084901359,52.3154665330345,14.9742750114912));
#57253=CARTESIAN_POINT('Ctrl Pts',(-0.284517802825563,52.5407640288737,
15.6132793684068));
#57254=CARTESIAN_POINT('Ctrl Pts',(-1.98108779736915,52.7672380367141,14.548338131115));
#57255=CARTESIAN_POINT('Ctrl Pts',(-2.24593225158725,52.9955367730046,12.5507060938727));
#57256=CARTESIAN_POINT('Ctrl Pts',(-0.844661895156112,53.2263011523758,
11.0610922239078));
#57257=CARTESIAN_POINT('Ctrl Pts',(0.869573113428819,53.4211666368392,11.1785206660127));
#57258=CARTESIAN_POINT('Ctrl Pts',(1.71083328229292,53.5591559476084,11.9415268412979));
#57259=CARTESIAN_POINT('Ctrl Pts',(1.98294590990857,53.6285762213412,12.4299124325736));
#57260=CARTESIAN_POINT('Ctrl Pts',(2.08959007456053,53.6683724708866,12.7309834583897));
#57261=CARTESIAN_POINT('Ctrl Pts',(2.27496720013922,53.7680712698251,13.5097709453007));
#57262=CARTESIAN_POINT('Ctrl Pts',(1.97222340842641,53.8989493845487,14.6215803669993));
#57263=CARTESIAN_POINT('Ctrl Pts',(0.89465038188734,54.0623411214105,15.421687269184));
#57264=CARTESIAN_POINT('Ctrl Pts',(-0.434402098507794,54.2273460490297,
15.7017375528132));
#57265=CARTESIAN_POINT('Ctrl Pts',(-1.86204774275957,54.4088330168871,14.988814832024));
#57266=CARTESIAN_POINT('Ctrl Pts',(-2.46935470263096,54.6077827186442,13.4337565694896));
#57267=CARTESIAN_POINT('Ctrl Pts',(-2.15929713050285,54.7807996593003,12.0210948829219));
#57268=CARTESIAN_POINT('Ctrl Pts',(-1.35423216557829,54.9143161276471,11.2458975817384));
#57269=CARTESIAN_POINT('Ctrl Pts',(-0.728176554458024,54.9983343641993,
10.9918842512178));
#57270=CARTESIAN_POINT('Ctrl Pts',(-0.470018856663394,55.031676775866,10.9223861532286));
#57271=CARTESIAN_POINT('Ctrl Pts',(-0.206362891446336,55.0650888123121,
10.8744933195446));
#57272=CARTESIAN_POINT('Ctrl Pts',(0.129892479094305,55.1069852111824,10.8558462463508));
#57273=CARTESIAN_POINT('Ctrl Pts',(0.668033059027686,55.1743021874798,10.9150750738386));
#57274=CARTESIAN_POINT('Ctrl Pts',(1.31164732367071,55.2589776680331,11.1565853466934));
#57275=CARTESIAN_POINT('Ctrl Pts',(2.16980807937479,55.395599927025,11.8612187217518));
#57276=CARTESIAN_POINT('Ctrl Pts',(2.72219984855538,55.5685285024121,13.2158867534057));
#57277=CARTESIAN_POINT('Ctrl Pts',(2.23437211680906,55.7795085295374,14.93536151132));
#57278=CARTESIAN_POINT('Ctrl Pts',(0.769178714778771,55.9939526145872,16.0068421910926));
#57279=CARTESIAN_POINT('Ctrl Pts',(-1.07457772221616,56.2118379980202,15.9496147996879));
#57280=CARTESIAN_POINT('Ctrl Pts',(-2.51436848419478,56.4331159822358,14.7506091228876));
#57281=CARTESIAN_POINT('Ctrl Pts',(-2.78329272553774,56.5828508457323,13.5127385387917));
#57282=CARTESIAN_POINT('Ctrl Pts',(-2.71099830929853,56.6582558952658,12.9129240239044));
#57283=CARTESIAN_POINT('Ctrl Pts',(-2.14027939152463,45.7730825127326,11.5660067125305));
#57284=CARTESIAN_POINT('Ctrl Pts',(-1.74041771225189,45.8504678483019,11.0919855577126));
#57285=CARTESIAN_POINT('Ctrl Pts',(-0.626255958572784,46.0025890400772,
10.441730633043));
#57286=CARTESIAN_POINT('Ctrl Pts',(1.25361264950939,46.226777695605,10.7065986783383));
#57287=CARTESIAN_POINT('Ctrl Pts',(2.54452730673143,46.4461763207554,12.0425156353896));
#57288=CARTESIAN_POINT('Ctrl Pts',(2.73830159988116,46.6623013886306,13.8619287458641));
#57289=CARTESIAN_POINT('Ctrl Pts',(1.78779448617996,46.8751179983104,15.3926009964812));
#57290=CARTESIAN_POINT('Ctrl Pts',(0.122164295117624,47.0846127176156,16.0046777804299));
#57291=CARTESIAN_POINT('Ctrl Pts',(-1.53788417221276,47.290795404332,15.4740393052136));
#57292=CARTESIAN_POINT('Ctrl Pts',(-2.62062632329518,47.5162410472015,13.8951269855267));
#57293=CARTESIAN_POINT('Ctrl Pts',(-2.31712263304767,47.7153786796623,12.1702446962084));
#57294=CARTESIAN_POINT('Ctrl Pts',(-1.38228941300507,47.8678319479962,11.3318172272074));
#57295=CARTESIAN_POINT('Ctrl Pts',(-0.743379299576394,47.9542712505232,
11.0561284084246));
#57296=CARTESIAN_POINT('Ctrl Pts',(-0.0614662828139273,48.0402619260491,
10.927558310766));
#57297=CARTESIAN_POINT('Ctrl Pts',(0.804323002403269,48.1469241896833,11.0543292263492));
#57298=CARTESIAN_POINT('Ctrl Pts',(1.67200255398421,48.2736316016426,11.6314195083817));
#57299=CARTESIAN_POINT('Ctrl Pts',(2.20192978851605,48.3990933885702,12.5129194563287));
#57300=CARTESIAN_POINT('Ctrl Pts',(2.34671685700884,48.5647796925803,13.8695157366898));
#57301=CARTESIAN_POINT('Ctrl Pts',(1.38041978153337,48.7690123591587,15.391151363593));
#57302=CARTESIAN_POINT('Ctrl Pts',(-0.554800061577224,48.989828017531,15.630553016929));
#57303=CARTESIAN_POINT('Ctrl Pts',(-1.89123635946174,49.187891064915,14.6144608515597));
#57304=CARTESIAN_POINT('Ctrl Pts',(-2.27942679155528,49.3642847386172,13.1738421618322));
#57305=CARTESIAN_POINT('Ctrl Pts',(-1.70155746521163,49.5390555916114,11.8109115882085));
#57306=CARTESIAN_POINT('Ctrl Pts',(-0.419837453047116,49.7124465296351,
11.0959486067296));
#57307=CARTESIAN_POINT('Ctrl Pts',(1.02274493966303,49.884705831022,11.3181689765725));
#57308=CARTESIAN_POINT('Ctrl Pts',(1.85076977950379,50.0275304024743,12.1986873373171));
#57309=CARTESIAN_POINT('Ctrl Pts',(2.08670366513554,50.1414890883567,13.0944260893894));
#57310=CARTESIAN_POINT('Ctrl Pts',(2.03770495762297,50.2268407621304,13.7860711292522));
#57311=CARTESIAN_POINT('Ctrl Pts',(1.76555785776637,50.3121079870555,14.423021260958));
#57312=CARTESIAN_POINT('Ctrl Pts',(1.14821454506869,50.4257325901016,15.1099789743916));
#57313=CARTESIAN_POINT('Ctrl Pts',(0.0159524118404732,50.5677252266712,
15.5117608197789));
#57314=CARTESIAN_POINT('Ctrl Pts',(-1.35483150298962,50.7383244061134,15.0538408040168));
#57315=CARTESIAN_POINT('Ctrl Pts',(-2.15600798820678,50.9094064194321,13.8472058420274));
#57316=CARTESIAN_POINT('Ctrl Pts',(-2.0452060214164,51.0812381870027,12.3962437455714));
#57317=CARTESIAN_POINT('Ctrl Pts',(-1.06007602045816,51.2540789421413,11.3140233760055));
#57318=CARTESIAN_POINT('Ctrl Pts',(0.393220475565066,51.4281917425227,11.0632511082158));
#57319=CARTESIAN_POINT('Ctrl Pts',(1.70194021914503,51.6038174996348,11.7671433158644));
#57320=CARTESIAN_POINT('Ctrl Pts',(2.3813336989747,51.8009034045937,13.2942865486876));
#57321=CARTESIAN_POINT('Ctrl Pts',(1.70953298962604,52.0205149535647,15.1116650631418));
#57322=CARTESIAN_POINT('Ctrl Pts',(-0.325700821288032,52.2641141168841,
15.8188950798337));
#57323=CARTESIAN_POINT('Ctrl Pts',(-2.19299708317051,52.5121763433595,14.6656692812233));
#57324=CARTESIAN_POINT('Ctrl Pts',(-2.50081734121616,52.7650950122649,12.4543130199027));
#57325=CARTESIAN_POINT('Ctrl Pts',(-0.942984791680106,53.0232126589936,
10.7785134485666));
#57326=CARTESIAN_POINT('Ctrl Pts',(0.990419469933448,53.2428748001176,10.9010410972588));
#57327=CARTESIAN_POINT('Ctrl Pts',(1.94647448835483,53.3991221449744,11.7615404602951));
#57328=CARTESIAN_POINT('Ctrl Pts',(2.25711350756306,53.4778755159918,12.3145370492997));
#57329=CARTESIAN_POINT('Ctrl Pts',(2.37937124148029,53.5230588412163,12.6559775396749));
#57330=CARTESIAN_POINT('Ctrl Pts',(2.59300773735541,53.6363183428028,13.5400127844654));
#57331=CARTESIAN_POINT('Ctrl Pts',(2.25317651268817,53.7853312499472,14.8073547464846));
#57332=CARTESIAN_POINT('Ctrl Pts',(1.02710429998273,53.9716803036347,15.7240476217481));
#57333=CARTESIAN_POINT('Ctrl Pts',(-0.488823678619321,54.159996137694,16.0486084172937));
#57334=CARTESIAN_POINT('Ctrl Pts',(-2.12129434023988,54.3672013044936,15.2395555163373));
#57335=CARTESIAN_POINT('Ctrl Pts',(-2.81919797130991,54.5941236714676,13.4676844962047));
#57336=CARTESIAN_POINT('Ctrl Pts',(-2.47054084677949,54.7911813077835,11.857671669541));
#57337=CARTESIAN_POINT('Ctrl Pts',(-1.55787978293911,54.9429300839132,10.9740750659129));
#57338=CARTESIAN_POINT('Ctrl Pts',(-0.848442414280066,55.0382521885198,
10.6837278088581));
#57339=CARTESIAN_POINT('Ctrl Pts',(-0.555953053306101,55.0760576966764,
10.6040218974212));
#57340=CARTESIAN_POINT('Ctrl Pts',(-0.257274113606343,55.1139270311992,
10.5488199112007));
#57341=CARTESIAN_POINT('Ctrl Pts',(0.123548225620592,55.1613822527919,10.5265360903747));
#57342=CARTESIAN_POINT('Ctrl Pts',(0.73275901235188,55.2375586094862,10.5917093753247));
#57343=CARTESIAN_POINT('Ctrl Pts',(1.46090423792938,55.3332462331937,10.862491826326));
#57344=CARTESIAN_POINT('Ctrl Pts',(2.43106789835719,55.4873132020393,11.6543429009093));
#57345=CARTESIAN_POINT('Ctrl Pts',(3.0555753824177,55.6816745690064,13.17554052952));
#57346=CARTESIAN_POINT('Ctrl Pts',(2.51443642982003,55.917600739646,15.0996987462084));
#57347=CARTESIAN_POINT('Ctrl Pts',(0.887864876777604,56.1560470583341,16.2949003909454));
#57348=CARTESIAN_POINT('Ctrl Pts',(-1.14995322970545,56.3968342675258,16.2362745078813));
#57349=CARTESIAN_POINT('Ctrl Pts',(-2.73362334794766,56.6397560948261,14.9235373291036));
#57350=CARTESIAN_POINT('Ctrl Pts',(-3.02994379097328,56.8029855464817,13.5747114983036));
#57351=CARTESIAN_POINT('Ctrl Pts',(-2.95373712227385,56.8848803793494,12.9229564194287));
#57352=CARTESIAN_POINT('Ctrl Pts',(-1.97489974262787,45.9807041464979,11.7658159225998));
#57353=CARTESIAN_POINT('Ctrl Pts',(-1.61505652254841,46.0509892968192,11.3323400902612));
#57354=CARTESIAN_POINT('Ctrl Pts',(-0.611269256832031,46.1885691442562,
10.7374043298315));
#57355=CARTESIAN_POINT('Ctrl Pts',(1.07752576838915,46.3897389699512,10.9630239649263));
#57356=CARTESIAN_POINT('Ctrl Pts',(2.23660411392116,46.5851717455016,12.1444286569083));
#57357=CARTESIAN_POINT('Ctrl Pts',(2.42101881993414,46.776383145112,13.7529590305592));
#57358=CARTESIAN_POINT('Ctrl Pts',(1.59654916798518,46.9635066926831,15.1061344565511));
#57359=CARTESIAN_POINT('Ctrl Pts',(0.144586387094734,47.1467007372936,15.6544880147957));
#57360=CARTESIAN_POINT('Ctrl Pts',(-1.30488728776191,47.3261540030483,15.2061283897338));
#57361=CARTESIAN_POINT('Ctrl Pts',(-2.25723504133272,47.5216201682429,13.8461458474566));
#57362=CARTESIAN_POINT('Ctrl Pts',(-2.00997966276009,47.6937022535128,12.3526010600685));
#57363=CARTESIAN_POINT('Ctrl Pts',(-1.2111029432495,47.8252428431062,11.620283448707));
#57364=CARTESIAN_POINT('Ctrl Pts',(-0.662486717251731,47.8998000924574,
11.3763376448611));
#57365=CARTESIAN_POINT('Ctrl Pts',(-0.0754773346809657,47.9739589568271,
11.2589023769796));
#57366=CARTESIAN_POINT('Ctrl Pts',(0.672635868779688,48.065948111542,11.3598898327613));
#57367=CARTESIAN_POINT('Ctrl Pts',(1.42722169386338,48.1752831521415,11.8494566774546));
#57368=CARTESIAN_POINT('Ctrl Pts',(1.89388086873647,48.2836605723592,12.6059093814622));
#57369=CARTESIAN_POINT('Ctrl Pts',(2.03281827204126,48.4270240875031,13.7784520810649));
#57370=CARTESIAN_POINT('Ctrl Pts',(1.21041226061467,48.6043308448814,15.1105276068321));
#57371=CARTESIAN_POINT('Ctrl Pts',(-0.47855914271545,48.7973034907702,15.3418748991076));
#57372=CARTESIAN_POINT('Ctrl Pts',(-1.66729342487016,48.9717496510135,14.4614097750748));
#57373=CARTESIAN_POINT('Ctrl Pts',(-2.0278566525121,49.1283257964996,13.1865070179862));
#57374=CARTESIAN_POINT('Ctrl Pts',(-1.5252569585939,49.2848565612056,11.9589795508061));
#57375=CARTESIAN_POINT('Ctrl Pts',(-0.373375572805371,49.441706688313,11.2978139075926));
#57376=CARTESIAN_POINT('Ctrl Pts',(0.948698557343252,49.599234209545,11.4851653570161));
#57377=CARTESIAN_POINT('Ctrl Pts',(1.7245922540337,49.7313731948764,12.2911188043351));
#57378=CARTESIAN_POINT('Ctrl Pts',(1.95334130678497,49.8377814012258,13.1256275259203));
#57379=CARTESIAN_POINT('Ctrl Pts',(1.91361106748085,49.9179781560273,13.7760966477355));
#57380=CARTESIAN_POINT('Ctrl Pts',(1.66191239379154,49.9986072078368,14.3810341259414));
#57381=CARTESIAN_POINT('Ctrl Pts',(1.08038015144688,50.1067472715965,15.0404105883413));
#57382=CARTESIAN_POINT('Ctrl Pts',(-0.00402274907490241,50.2432136429006,
15.4381062275646));
#57383=CARTESIAN_POINT('Ctrl Pts',(-1.34386924241886,50.4093528692499,15.0055747226929));
#57384=CARTESIAN_POINT('Ctrl Pts',(-2.14613810219979,50.5781769862165,13.822101998393));
#57385=CARTESIAN_POINT('Ctrl Pts',(-2.04848371920403,50.7499678180921,12.3700938579116));
#57386=CARTESIAN_POINT('Ctrl Pts',(-1.06007416862713,50.9249850539197,11.265466652103));
#57387=CARTESIAN_POINT('Ctrl Pts',(0.428012895343668,51.103476568345,10.996433735333));
#57388=CARTESIAN_POINT('Ctrl Pts',(1.79124689132523,51.2856546563901,11.7167138949258));
#57389=CARTESIAN_POINT('Ctrl Pts',(2.51521942875102,51.4923864192564,13.3137372704007));
#57390=CARTESIAN_POINT('Ctrl Pts',(1.81625748911618,51.725563374095,15.2490551147924));
#57391=CARTESIAN_POINT('Ctrl Pts',(-0.366883839750501,51.9874642048946,
16.0245107912607));
#57392=CARTESIAN_POINT('Ctrl Pts',(-2.40490636897185,52.2571146500049,14.7830004313315));
#57393=CARTESIAN_POINT('Ctrl Pts',(-2.75570243084506,52.5346532515253,12.3579199459325));
#57394=CARTESIAN_POINT('Ctrl Pts',(-1.0413076882041,52.8201241656114,10.4959346732253));
#57395=CARTESIAN_POINT('Ctrl Pts',(1.11126582643808,53.0645829633961,10.623561528505));
#57396=CARTESIAN_POINT('Ctrl Pts',(2.18211569441672,53.2390883423404,11.5815540792923));
#57397=CARTESIAN_POINT('Ctrl Pts',(2.53128110521754,53.3271748106425,12.1991616660258));
#57398=CARTESIAN_POINT('Ctrl Pts',(2.66915240840004,53.377745211546,12.58097162096));
#57399=CARTESIAN_POINT('Ctrl Pts',(2.91104827457162,53.5045654157805,13.57025462363));
#57400=CARTESIAN_POINT('Ctrl Pts',(2.53412961694995,53.6717131153456,14.99312912597));
#57401=CARTESIAN_POINT('Ctrl Pts',(1.15955821807812,53.8810194858589,16.0264079743121));
#57402=CARTESIAN_POINT('Ctrl Pts',(-0.543245258730856,54.0926462263583,
16.395479281774));
#57403=CARTESIAN_POINT('Ctrl Pts',(-2.38054093772021,54.3255695921,15.4902962006507));
#57404=CARTESIAN_POINT('Ctrl Pts',(-3.16904123998887,54.5804646242909,13.5016124229199));
#57405=CARTESIAN_POINT('Ctrl Pts',(-2.78178456305616,54.8015629562669,11.69424845616));
#57406=CARTESIAN_POINT('Ctrl Pts',(-1.76152740029993,54.9715440401794,10.7022525500875));
#57407=CARTESIAN_POINT('Ctrl Pts',(-0.968708274102122,55.0781700128403,
10.3755713664983));
#57408=CARTESIAN_POINT('Ctrl Pts',(-0.641887249948822,55.120438617487,10.2856576416139));
#57409=CARTESIAN_POINT('Ctrl Pts',(-0.308185335766365,55.1627652500864,
10.2231465028569));
#57410=CARTESIAN_POINT('Ctrl Pts',(0.117203972146864,55.2157792944013,10.1972259343985));
#57411=CARTESIAN_POINT('Ctrl Pts',(0.797484965676056,55.3008150314925,10.2683436768106));
#57412=CARTESIAN_POINT('Ctrl Pts',(1.61016115218803,55.4075147983545,10.5683983059585));
#57413=CARTESIAN_POINT('Ctrl Pts',(2.69232771733956,55.5790264770535,11.4474670800669));
#57414=CARTESIAN_POINT('Ctrl Pts',(3.38895091628001,55.7948206356007,13.1351943056343));
#57415=CARTESIAN_POINT('Ctrl Pts',(2.79450074283097,56.0556929497546,15.2640359810966));
#57416=CARTESIAN_POINT('Ctrl Pts',(1.00655103877642,56.318141502081,16.5829585907982));
#57417=CARTESIAN_POINT('Ctrl Pts',(-1.22532873719474,56.5818305370312,16.5229342160748));
#57418=CARTESIAN_POINT('Ctrl Pts',(-2.95287821170053,56.8463962074163,15.0964655353195));
#57419=CARTESIAN_POINT('Ctrl Pts',(-3.27659485640882,57.0231202472312,13.6366844578155));
#57420=CARTESIAN_POINT('Ctrl Pts',(-3.19647593524917,57.1115048634331,12.932988814953));
#57421=CARTESIAN_POINT('Ctrl Pts',(-1.95241364042681,45.9847503099714,11.7382273262856));
#57422=CARTESIAN_POINT('Ctrl Pts',(-1.8971421670987,45.9953436461596,11.6735188111325));
#57423=CARTESIAN_POINT('Ctrl Pts',(-1.83865442762089,46.0059232379815,11.6117345120665));
#57424=CARTESIAN_POINT('Ctrl Pts',(-1.77721585694918,46.0164890647086,11.5532444801427));
#57425=CARTESIAN_POINT('Ctrl Pts',(-1.64756344227922,46.0387858879122,11.4298142995552));
#57426=CARTESIAN_POINT('Ctrl Pts',(-1.50476811437305,46.0610213831347,11.3210572491992));
#57427=CARTESIAN_POINT('Ctrl Pts',(-1.35265282291184,46.0831958590439,11.2288377615449));
#57428=CARTESIAN_POINT('Ctrl Pts',(-1.20240674226712,46.1050978523524,11.137751477937));
#57429=CARTESIAN_POINT('Ctrl Pts',(-1.04307002516613,46.1269403212354,11.0627994520531));
#57430=CARTESIAN_POINT('Ctrl Pts',(-0.878344943658423,46.148723958966,11.0057329629921));
#57431=CARTESIAN_POINT('Ctrl Pts',(-0.823649496877625,46.1559570153244,
10.9867845606794));
#57432=CARTESIAN_POINT('Ctrl Pts',(-0.768360021367818,46.1631835884625,
10.9698076438706));
#57433=CARTESIAN_POINT('Ctrl Pts',(-0.71261202736178,46.1704037122867,10.9548650191242));
#57434=CARTESIAN_POINT('Ctrl Pts',(-0.66491427331565,46.176581220491,10.9420801709397));
#57435=CARTESIAN_POINT('Ctrl Pts',(-0.616880865738027,46.1827540075846,
10.930784497145));
#57436=CARTESIAN_POINT('Ctrl Pts',(-0.56860365505536,46.1889220994543,10.9209716054323));
#57437=CARTESIAN_POINT('Ctrl Pts',(-0.431265107463782,46.2064690282601,
10.893055984864));
#57438=CARTESIAN_POINT('Ctrl Pts',(-0.291751219692949,46.2239557050407,
10.8771188680412));
#57439=CARTESIAN_POINT('Ctrl Pts',(-0.152216507090954,46.2413863885295,
10.8730912299346));
#57440=CARTESIAN_POINT('Ctrl Pts',(-0.0102360917695286,46.2591225893281,
10.868992997169));
#57441=CARTESIAN_POINT('Ctrl Pts',(0.131764428199893,46.2768008194013,10.8772253772626));
#57442=CARTESIAN_POINT('Ctrl Pts',(0.271508687144479,46.2944261648867,10.8976631512315));
#57443=CARTESIAN_POINT('Ctrl Pts',(0.344537665980979,46.3036369975331,10.9083437314136));
#57444=CARTESIAN_POINT('Ctrl Pts',(0.416950487390888,46.3128333969747,10.9223567501107));
#57445=CARTESIAN_POINT('Ctrl Pts',(0.488423636868789,46.322016148492,10.939678813146));
#57446=CARTESIAN_POINT('Ctrl Pts',(0.625333006365584,46.3396060368582,10.9728598433073));
#57447=CARTESIAN_POINT('Ctrl Pts',(0.758792220052205,46.357145819602,11.0181848126039));
#57448=CARTESIAN_POINT('Ctrl Pts',(0.886906146962075,46.3746414549503,11.0744382700336));
#57449=CARTESIAN_POINT('Ctrl Pts',(0.922014005139931,46.3794358929896,11.0898537557118));
#57450=CARTESIAN_POINT('Ctrl Pts',(0.956720662856293,46.3842270184074,11.1060897099406));
#57451=CARTESIAN_POINT('Ctrl Pts',(0.990987645700955,46.389014959637,11.1231206684141));
#57452=CARTESIAN_POINT('Ctrl Pts',(1.11975164580951,46.4070064608965,11.1871173835225));
#57453=CARTESIAN_POINT('Ctrl Pts',(1.24256507675794,46.4249354693607,11.262486210778));
#57454=CARTESIAN_POINT('Ctrl Pts',(1.35732849364204,46.4428028920159,11.3479832212788));
#57455=CARTESIAN_POINT('Ctrl Pts',(1.4182011948596,46.4522801131578,11.3933324633676));
#57456=CARTESIAN_POINT('Ctrl Pts',(1.47680927481519,46.4617400153292,11.4415303145385));
#57457=CARTESIAN_POINT('Ctrl Pts',(1.53284192491298,46.4711827841931,11.4923857831166));
#57458=CARTESIAN_POINT('Ctrl Pts',(1.6392516195938,46.4891152244756,11.5889636689529));
#57459=CARTESIAN_POINT('Ctrl Pts',(1.73637042168925,46.5069858512471,11.6951278292034));
#57460=CARTESIAN_POINT('Ctrl Pts',(1.82297362114317,46.5247963431438,11.8087410688735));
#57461=CARTESIAN_POINT('Ctrl Pts',(1.90839933305812,46.5423646773326,11.9208095830045));
#57462=CARTESIAN_POINT('Ctrl Pts',(1.98359284293436,46.5598745051721,12.0401246246244));
#57463=CARTESIAN_POINT('Ctrl Pts',(2.04742465939072,46.5773277830352,12.1646161671583));
#57464=CARTESIAN_POINT('Ctrl Pts',(2.05618755650694,46.5797237868895,12.1817064935758));
#57465=CARTESIAN_POINT('Ctrl Pts',(2.06473641007925,46.5821187254778,12.1988943657412));
#57466=CARTESIAN_POINT('Ctrl Pts',(2.07306837637378,46.5845126043074,12.2161744218087));
#57467=CARTESIAN_POINT('Ctrl Pts',(2.11160201547555,46.5955838040237,12.2960911450196));
#57468=CARTESIAN_POINT('Ctrl Pts',(2.14554167347974,46.6066369948493,12.3780773092497));
#57469=CARTESIAN_POINT('Ctrl Pts',(2.17457606972679,46.6176715277991,12.4616120935857));
#57470=CARTESIAN_POINT('Ctrl Pts',(2.21973917011656,46.6348357806779,12.5915507297779));
#57471=CARTESIAN_POINT('Ctrl Pts',(2.2530307354994,46.6519548760391,12.725237010723));
#57472=CARTESIAN_POINT('Ctrl Pts',(2.27437953802083,46.6690266578218,12.8604588311141));
#57473=CARTESIAN_POINT('Ctrl Pts',(2.29577493171289,46.6861356966963,12.9959757567177));
#57474=CARTESIAN_POINT('Ctrl Pts',(2.3051753512887,46.7031972175615,13.1330334363911));
#57475=CARTESIAN_POINT('Ctrl Pts',(2.3025595800891,46.720209314466,13.2693972267247));
#57476=CARTESIAN_POINT('Ctrl Pts',(2.30042405253179,46.7340980680974,13.3807252481215));
#57477=CARTESIAN_POINT('Ctrl Pts',(2.29028047142328,46.7479538853357,13.4915902788484));
#57478=CARTESIAN_POINT('Ctrl Pts',(2.27214231801973,46.7617758427502,13.6007828735325));
#57479=CARTESIAN_POINT('Ctrl Pts',(2.26605711820078,46.7664129946634,13.6374160821408));
#57480=CARTESIAN_POINT('Ctrl Pts',(2.25907228475214,46.7710463362792,13.6738611409023));
#57481=CARTESIAN_POINT('Ctrl Pts',(2.25120957080458,46.7756758366425,13.7100774197308));
#57482=CARTESIAN_POINT('Ctrl Pts',(2.2210005603269,46.793462649938,13.8492224978668));
#57483=CARTESIAN_POINT('Ctrl Pts',(2.17776659788189,46.8111909930459,13.985265270644));
#57484=CARTESIAN_POINT('Ctrl Pts',(2.12261993130273,46.8288630348613,14.1158844579314));
#57485=CARTESIAN_POINT('Ctrl Pts',(2.06598742150198,46.8470112230183,14.250022980948));
#57486=CARTESIAN_POINT('Ctrl Pts',(1.99679213031932,46.8651000380505,14.3784402361469));
#57487=CARTESIAN_POINT('Ctrl Pts',(1.91629136575179,46.88313210643,14.4986320939029));
#57488=CARTESIAN_POINT('Ctrl Pts',(1.88585063708702,46.8899507907463,14.5440816961437));
#57489=CARTESIAN_POINT('Ctrl Pts',(1.8537938087849,46.8967613633154,14.5883553540662));
#57490=CARTESIAN_POINT('Ctrl Pts',(1.82019050855776,46.9035639746694,14.6313187155398));
#57491=CARTESIAN_POINT('Ctrl Pts',(1.73100455685324,46.9216186705947,14.7453470477436));
#57492=CARTESIAN_POINT('Ctrl Pts',(1.63092320563563,46.9396172750017,14.8501422182976));
#57493=CARTESIAN_POINT('Ctrl Pts',(1.52223787899297,46.9575628219442,14.9442418774281));
#57494=CARTESIAN_POINT('Ctrl Pts',(1.51188162730683,46.9592727915098,14.953208310926));
#57495=CARTESIAN_POINT('Ctrl Pts',(1.501447273049,46.9609822794534,14.9620776692662));
#57496=CARTESIAN_POINT('Ctrl Pts',(1.49093680841019,46.9626912884685,14.9708487102848));
#57497=CARTESIAN_POINT('Ctrl Pts',(1.38006322227004,46.9807194123196,15.063373332681));
#57498=CARTESIAN_POINT('Ctrl Pts',(1.26055089980399,46.9986943927912,15.1450935129852));
#57499=CARTESIAN_POINT('Ctrl Pts',(1.13468374163679,47.0166184141626,15.2144752016254));
#57500=CARTESIAN_POINT('Ctrl Pts',(1.07265992579405,47.0254508706738,15.2486645576237));
#57501=CARTESIAN_POINT('Ctrl Pts',(1.00909365887041,47.0342709560681,15.2798583357467));
#57502=CARTESIAN_POINT('Ctrl Pts',(0.944261256667278,47.0430789466427,15.3078764650197));
#57503=CARTESIAN_POINT('Ctrl Pts',(0.812475281708041,47.0609831054559,15.3648294138124));
#57504=CARTESIAN_POINT('Ctrl Pts',(0.675457283418255,47.078837283571,15.4086575150184));
#57505=CARTESIAN_POINT('Ctrl Pts',(0.536001779571398,47.0966439332634,15.4389983175078));
#57506=CARTESIAN_POINT('Ctrl Pts',(0.40699792754375,47.1131160432818,15.4670651939434));
#57507=CARTESIAN_POINT('Ctrl Pts',(0.275909476634552,47.1295474859783,15.4835910086528));
#57508=CARTESIAN_POINT('Ctrl Pts',(0.144946080722838,47.1459402512969,15.4883285461524));
#57509=CARTESIAN_POINT('Ctrl Pts',(0.052400211512539,47.1575242721954,15.4916763482063));
#57510=CARTESIAN_POINT('Ctrl Pts',(-0.0401751944031819,47.16907224139,15.4891450692736));
#57511=CARTESIAN_POINT('Ctrl Pts',(-0.132013920397452,47.1805906345695,
15.4806224156613));
#57512=CARTESIAN_POINT('Ctrl Pts',(-0.302049520997157,47.2019164628736,
15.4648430751927));
#57513=CARTESIAN_POINT('Ctrl Pts',(-0.469560729760759,47.2231409413218,
15.4285225448653));
#57514=CARTESIAN_POINT('Ctrl Pts',(-0.630324528041842,47.2443051016368,
15.3737808941178));
#57515=CARTESIAN_POINT('Ctrl Pts',(-0.798772123195201,47.2664808149916,
15.3164228351411));
#57516=CARTESIAN_POINT('Ctrl Pts',(-0.959810524721762,47.2885903429389,
15.2388406836729));
#57517=CARTESIAN_POINT('Ctrl Pts',(-1.10857004406211,47.3106800499252,15.1435280009256));
#57518=CARTESIAN_POINT('Ctrl Pts',(-1.14179459733405,47.3156136545092,15.1222404805069));
#57519=CARTESIAN_POINT('Ctrl Pts',(-1.17440665457436,47.3205462659255,15.1000687222124));
#57520=CARTESIAN_POINT('Ctrl Pts',(-1.20635200726083,47.3254783924175,15.0770408546523));
#57521=CARTESIAN_POINT('Ctrl Pts',(-1.28232251514563,47.3372076776825,15.0222773711744));
#57522=CARTESIAN_POINT('Ctrl Pts',(-1.3545961616888,47.3488715301593,14.9626333442155));
#57523=CARTESIAN_POINT('Ctrl Pts',(-1.42240277269893,47.3604896246544,14.8984908981873));
#57524=CARTESIAN_POINT('Ctrl Pts',(-1.5073465397739,47.375044027211,14.8181373616534));
#57525=CARTESIAN_POINT('Ctrl Pts',(-1.58527821899684,47.3895266455885,14.7307232409101));
#57526=CARTESIAN_POINT('Ctrl Pts',(-1.6554807059147,47.4039757275965,14.6377529363878));
#57527=CARTESIAN_POINT('Ctrl Pts',(-1.72591693999175,47.4184729194653,14.5444730766698));
#57528=CARTESIAN_POINT('Ctrl Pts',(-1.78857168988701,47.4329363652546,14.4456010916711));
#57529=CARTESIAN_POINT('Ctrl Pts',(-1.84276115801007,47.4474039676963,14.3426893008476));
#57530=CARTESIAN_POINT('Ctrl Pts',(-1.8952760752046,47.4614244954953,14.2429576673655));
#57531=CARTESIAN_POINT('Ctrl Pts',(-1.93984036957768,47.475448934269,14.1394331900176));
#57532=CARTESIAN_POINT('Ctrl Pts',(-1.97587791985858,47.4895109490354,14.0335425918392));
#57533=CARTESIAN_POINT('Ctrl Pts',(-1.98602212383801,47.4934692632116,14.0037354651324));
#57534=CARTESIAN_POINT('Ctrl Pts',(-1.99549100902068,47.4974305492356,13.9737408854396));
#57535=CARTESIAN_POINT('Ctrl Pts',(-2.00427248941019,47.5013955444323,13.9435906943912));
#57536=CARTESIAN_POINT('Ctrl Pts',(-2.03063765510875,47.5132998875177,13.8530689659838));
#57537=CARTESIAN_POINT('Ctrl Pts',(-2.05090427372228,47.5251676359854,13.7609038126534));
#57538=CARTESIAN_POINT('Ctrl Pts',(-2.06467398077651,47.5369983931114,13.6679110418037));
#57539=CARTESIAN_POINT('Ctrl Pts',(-2.08331667921734,47.5530159624438,13.542008858315));
#57540=CARTESIAN_POINT('Ctrl Pts',(-2.09004753037163,47.5689657217592,13.4145893286777));
#57541=CARTESIAN_POINT('Ctrl Pts',(-2.0853251332468,47.5848469350357,13.2877517923853));
#57542=CARTESIAN_POINT('Ctrl Pts',(-2.080469850256,47.6011750376193,13.1573451119905));
#57543=CARTESIAN_POINT('Ctrl Pts',(-2.0635077757518,47.6174306848979,13.0275550939873));
#57544=CARTESIAN_POINT('Ctrl Pts',(-2.03499220175551,47.6336132009398,12.9006765006415));
#57545=CARTESIAN_POINT('Ctrl Pts',(-2.00676774037093,47.6496305113117,12.7750931980263));
#57546=CARTESIAN_POINT('Ctrl Pts',(-1.96722491767763,47.6655761794401,12.6523637092149));
#57547=CARTESIAN_POINT('Ctrl Pts',(-1.91694860837323,47.6814496221164,12.5347033318195));
#57548=CARTESIAN_POINT('Ctrl Pts',(-1.88677704915636,47.6909755105976,12.4640935934918));
#57549=CARTESIAN_POINT('Ctrl Pts',(-1.85274085457809,47.7004753891121,12.3953091388544));
#57550=CARTESIAN_POINT('Ctrl Pts',(-1.81497392706467,47.7099491365865,12.3288235383124));
#57551=CARTESIAN_POINT('Ctrl Pts',(-1.78679056988097,47.7170188673408,12.2792090329497));
#57552=CARTESIAN_POINT('Ctrl Pts',(-1.75652979937312,47.724074046305,12.2308746093299));
#57553=CARTESIAN_POINT('Ctrl Pts',(-1.72434746508382,47.7311146195406,12.1839532034194));
#57554=CARTESIAN_POINT('Ctrl Pts',(-1.65491285062346,47.7463049249984,12.082718479423));
#57555=CARTESIAN_POINT('Ctrl Pts',(-1.57635114487308,47.7616179338749,11.9879144256428));
#57556=CARTESIAN_POINT('Ctrl Pts',(-1.49018644155164,47.7769591100884,11.9009221587838));
#57557=CARTESIAN_POINT('Ctrl Pts',(-1.4559767182022,47.783049972981,11.8663838702727));
#57558=CARTESIAN_POINT('Ctrl Pts',(-1.42056894123929,47.7891453089514,11.8330765223171));
#57559=CARTESIAN_POINT('Ctrl Pts',(-1.38405974379315,47.7952393381944,11.8010846975313));
#57560=CARTESIAN_POINT('Ctrl Pts',(-1.291106066256,47.8107549471034,11.7196324067941));
#57561=CARTESIAN_POINT('Ctrl Pts',(-1.19101258933282,47.826261822322,11.6467114019376));
#57562=CARTESIAN_POINT('Ctrl Pts',(-1.08551772136646,47.8416672343656,11.5835119067454));
#57563=CARTESIAN_POINT('Ctrl Pts',(-1.07937807937506,47.8425638060804,11.5798337915726));
#57564=CARTESIAN_POINT('Ctrl Pts',(-1.0732201420744,47.8434600351941,11.5761885890833));
#57565=CARTESIAN_POINT('Ctrl Pts',(-1.06704425165267,47.8443559038265,11.5725765284172));
#57566=CARTESIAN_POINT('Ctrl Pts',(-0.984182526285751,47.8563757447734,
11.5241136253402));
#57567=CARTESIAN_POINT('Ctrl Pts',(-0.898114350906959,47.8683270587626,
11.4816288003348));
#57568=CARTESIAN_POINT('Ctrl Pts',(-0.809594952477851,47.8801958143893,
11.4456461415384));
#57569=CARTESIAN_POINT('Ctrl Pts',(-0.759797690759056,47.8868726732554,
11.4254038228013));
#57570=CARTESIAN_POINT('Ctrl Pts',(-0.709224300952944,47.8935234177675,
11.4072196096752));
#57571=CARTESIAN_POINT('Ctrl Pts',(-0.65803506781527,47.9001456523423,11.3910910199214));
#57572=CARTESIAN_POINT('Ctrl Pts',(-0.556989608908551,47.9132176733626,
11.3592538414116));
#57573=CARTESIAN_POINT('Ctrl Pts',(-0.453567639932314,47.9262319211411,
11.3354679413944));
#57574=CARTESIAN_POINT('Ctrl Pts',(-0.349152492158056,47.9392851887089,
11.3198053610108));
#57575=CARTESIAN_POINT('Ctrl Pts',(-0.306643092427297,47.944599423096,11.31342882557));
#57576=CARTESIAN_POINT('Ctrl Pts',(-0.263969510184714,47.9499200773217,
11.3083982854292));
#57577=CARTESIAN_POINT('Ctrl Pts',(-0.221226672214552,47.9552534808775,
11.3047166934343));
#57578=CARTESIAN_POINT('Ctrl Pts',(-0.0941688513748754,47.9711076137719,
11.2937727533895));
#57579=CARTESIAN_POINT('Ctrl Pts',(0.0336667007323784,47.987073378859,11.2947215717854));
#57580=CARTESIAN_POINT('Ctrl Pts',(0.159977082598235,48.0030097641556,11.30753003906));
#57581=CARTESIAN_POINT('Ctrl Pts',(0.277107148884844,48.0177878832507,11.3194075791224));
#57582=CARTESIAN_POINT('Ctrl Pts',(0.392926303456317,48.0325407724067,11.3414822374556));
#57583=CARTESIAN_POINT('Ctrl Pts',(0.505635732065545,48.0471617049776,11.3737411872782));
#57584=CARTESIAN_POINT('Ctrl Pts',(0.554022137755661,48.0534385034999,11.3875900254145));
#57585=CARTESIAN_POINT('Ctrl Pts',(0.601835856642591,48.0596910546578,11.4033161257713));
#57586=CARTESIAN_POINT('Ctrl Pts',(0.648968025783451,48.0659112574905,11.4208298094681));
#57587=CARTESIAN_POINT('Ctrl Pts',(0.792745122678298,48.0848860409917,11.4742554557677));
#57588=CARTESIAN_POINT('Ctrl Pts',(0.929914752706283,48.1037959420619,11.5443812200174));
#57589=CARTESIAN_POINT('Ctrl Pts',(1.0572203088745,48.122757211789,11.6287132239111));
#57590=CARTESIAN_POINT('Ctrl Pts',(1.17368682969203,48.1401040832207,11.7058650418106));
#57591=CARTESIAN_POINT('Ctrl Pts',(1.28189670087718,48.1574938913579,11.794909079678));
#57592=CARTESIAN_POINT('Ctrl Pts',(1.37931897278784,48.1750092485061,11.8939281093346));
#57593=CARTESIAN_POINT('Ctrl Pts',(1.44817970563592,48.1873895831634,11.9639174743364));
#57594=CARTESIAN_POINT('Ctrl Pts',(1.51178307075387,48.1997032029502,12.0388925787864));
#57595=CARTESIAN_POINT('Ctrl Pts',(1.56921941560834,48.2119536546085,12.1181775659105));
#57596=CARTESIAN_POINT('Ctrl Pts',(1.64793677992031,48.2287430806872,12.2268388191942));
#57597=CARTESIAN_POINT('Ctrl Pts',(1.71506824146787,48.2454138784686,12.3435963825234));
#57598=CARTESIAN_POINT('Ctrl Pts',(1.76975360272235,48.2619748990657,12.4657448884544));
#57599=CARTESIAN_POINT('Ctrl Pts',(1.79332319336232,48.269112759493,12.5183913411071));
#57600=CARTESIAN_POINT('Ctrl Pts',(1.81458124833026,48.2762302216107,12.5720387813991));
#57601=CARTESIAN_POINT('Ctrl Pts',(1.83346141180619,48.2833279657749,12.6264690528864));
#57602=CARTESIAN_POINT('Ctrl Pts',(1.86759929129462,48.2961616435777,12.7248863177013));
#57603=CARTESIAN_POINT('Ctrl Pts',(1.89399287542128,48.3088998382903,12.8258755189266));
#57604=CARTESIAN_POINT('Ctrl Pts',(1.91217778741452,48.3216474325737,12.9281520763732));
#57605=CARTESIAN_POINT('Ctrl Pts',(1.91764729273875,48.3254815470765,12.9589139615946));
#57606=CARTESIAN_POINT('Ctrl Pts',(1.92237425929101,48.3293164669574,12.9897919553678));
#57607=CARTESIAN_POINT('Ctrl Pts',(1.92634626748762,48.3331549282506,13.020750204952));
#57608=CARTESIAN_POINT('Ctrl Pts',(1.93922945297624,48.3456049551347,13.1211631074573));
#57609=CARTESIAN_POINT('Ctrl Pts',(1.94416821334328,48.3580927182959,13.2224235142376));
#57610=CARTESIAN_POINT('Ctrl Pts',(1.94124327456912,48.3707074724205,13.3232142749551));
#57611=CARTESIAN_POINT('Ctrl Pts',(1.93975556789633,48.3771236935231,13.3744793094918));
#57612=CARTESIAN_POINT('Ctrl Pts',(1.93623392363029,48.3835726662027,13.4256221544924));
#57613=CARTESIAN_POINT('Ctrl Pts',(1.93069244633872,48.3900654906189,13.4764656414149));
#57614=CARTESIAN_POINT('Ctrl Pts',(1.9195958753464,48.4030670934918,13.5782775468776));
#57615=CARTESIAN_POINT('Ctrl Pts',(1.90062231617946,48.4159740217048,13.6792652673937));
#57616=CARTESIAN_POINT('Ctrl Pts',(1.87381672141904,48.428819389061,13.7780564811559));
#57617=CARTESIAN_POINT('Ctrl Pts',(1.85561139991501,48.4375434649357,13.8451516463402));
#57618=CARTESIAN_POINT('Ctrl Pts',(1.83379425904398,48.4462391002347,13.9112327574732));
#57619=CARTESIAN_POINT('Ctrl Pts',(1.80839081469691,48.4549160542697,13.9758624728608));
#57620=CARTESIAN_POINT('Ctrl Pts',(1.77084002294634,48.4677421297241,14.071396643356));
#57621=CARTESIAN_POINT('Ctrl Pts',(1.72545042400657,48.4805275074423,14.1637591733987));
#57622=CARTESIAN_POINT('Ctrl Pts',(1.67309195688153,48.4933016388624,14.2519334979011));
#57623=CARTESIAN_POINT('Ctrl Pts',(1.6205358691939,48.5061239846627,14.3404406254929));
#57624=CARTESIAN_POINT('Ctrl Pts',(1.56095847103348,48.5189350110995,14.4247267175243));
#57625=CARTESIAN_POINT('Ctrl Pts',(1.4952920782572,48.531761794563,14.5037685682419));
#57626=CARTESIAN_POINT('Ctrl Pts',(1.43148393269753,48.5442256018729,14.5805736690349));
#57627=CARTESIAN_POINT('Ctrl Pts',(1.36192713639654,48.5567042823722,14.652426058278));
#57628=CARTESIAN_POINT('Ctrl Pts',(1.2875196963635,48.5692200943733,14.718407959033));
#57629=CARTESIAN_POINT('Ctrl Pts',(1.21831432097887,48.5808608855011,14.7797768518254));
#57630=CARTESIAN_POINT('Ctrl Pts',(1.1449135718977,48.5925337765941,14.8360668230429));
#57631=CARTESIAN_POINT('Ctrl Pts',(1.06806755633897,48.6042546205366,14.8865691212847));
#57632=CARTESIAN_POINT('Ctrl Pts',(0.997855878415097,48.6149635702968,14.9327114108072));
#57633=CARTESIAN_POINT('Ctrl Pts',(0.924597377811292,48.6256213621673,14.9742971533863));
#57634=CARTESIAN_POINT('Ctrl Pts',(0.848780767190351,48.6362346500015,15.0107513008384));
#57635=CARTESIAN_POINT('Ctrl Pts',(0.751475927923849,48.6498559957507,15.0575374197294));
#57636=CARTESIAN_POINT('Ctrl Pts',(0.649955872521592,48.6634040823214,15.0958688731996));
#57637=CARTESIAN_POINT('Ctrl Pts',(0.545925605715438,48.6768917648121,15.1254196313063));
#57638=CARTESIAN_POINT('Ctrl Pts',(0.496346508051243,48.6833197703148,15.1395030319088));
#57639=CARTESIAN_POINT('Ctrl Pts',(0.446197952127165,48.6897340371865,15.151592479276));
#57640=CARTESIAN_POINT('Ctrl Pts',(0.39566769098551,48.6961358496051,15.1616552427937));
#57641=CARTESIAN_POINT('Ctrl Pts',(0.285443684121811,48.710100420538,15.1836056164902));
#57642=CARTESIAN_POINT('Ctrl Pts',(0.173402081440556,48.7240058432638,15.1959092671239));
#57643=CARTESIAN_POINT('Ctrl Pts',(0.0612786825161412,48.7378643888788,
15.1985578236115));
#57644=CARTESIAN_POINT('Ctrl Pts',(-0.0480306448107308,48.7513751128975,
15.201139906663));
#57645=CARTESIAN_POINT('Ctrl Pts',(-0.157416299553511,48.7648412835544,
15.1945452811103));
#57646=CARTESIAN_POINT('Ctrl Pts',(-0.265259931271808,48.7782726460466,
15.1788127927061));
#57647=CARTESIAN_POINT('Ctrl Pts',(-0.361009084575653,48.7901977042614,
15.1648446759052));
#57648=CARTESIAN_POINT('Ctrl Pts',(-0.45554187461286,48.8020953041717,15.1436738368278));
#57649=CARTESIAN_POINT('Ctrl Pts',(-0.547732499780266,48.8139711442149,
15.1153613345604));
#57650=CARTESIAN_POINT('Ctrl Pts',(-0.549470603064334,48.8141950437333,
15.1148275486892));
#57651=CARTESIAN_POINT('Ctrl Pts',(-0.551207874248608,48.8144189354851,
15.1142912253172));
#57652=CARTESIAN_POINT('Ctrl Pts',(-0.552944306625827,48.8146428195046,
15.1137523689517));
#57653=CARTESIAN_POINT('Ctrl Pts',(-0.664401504574121,48.8290133678834,
15.079164543144));
#57654=CARTESIAN_POINT('Ctrl Pts',(-0.772601599312067,48.843484458884,15.0339363505538));
#57655=CARTESIAN_POINT('Ctrl Pts',(-0.87577886749647,48.8580031014277,14.9792130748679));
#57656=CARTESIAN_POINT('Ctrl Pts',(-0.980104126932079,48.8726832841527,
14.9238809262894));
#57657=CARTESIAN_POINT('Ctrl Pts',(-1.07929375723489,48.88741205545,14.8588430427353));
#57658=CARTESIAN_POINT('Ctrl Pts',(-1.17157210490308,48.9021401953873,14.7852989387065));
#57659=CARTESIAN_POINT('Ctrl Pts',(-1.2345600849423,48.912193428977,14.7350987056765));
#57660=CARTESIAN_POINT('Ctrl Pts',(-1.29432902552041,48.9222464846687,14.6809354960996));
#57661=CARTESIAN_POINT('Ctrl Pts',(-1.35032798481397,48.9322852629655,14.6231886578157));
#57662=CARTESIAN_POINT('Ctrl Pts',(-1.423174139881,48.9453441913763,14.5480687772086));
#57663=CARTESIAN_POINT('Ctrl Pts',(-1.48964008048988,48.9583788276777,14.4668858839713));
#57664=CARTESIAN_POINT('Ctrl Pts',(-1.54908346976911,48.9713613939306,14.3809105942702));
#57665=CARTESIAN_POINT('Ctrl Pts',(-1.61918775705424,48.9866723236292,14.2795160324576));
#57666=CARTESIAN_POINT('Ctrl Pts',(-1.67953046460898,49.0019620494912,14.1713370847684));
#57667=CARTESIAN_POINT('Ctrl Pts',(-1.72890459112104,49.0172519579631,14.0584172512926));
#57668=CARTESIAN_POINT('Ctrl Pts',(-1.76437360470154,49.0282358073908,13.9772987507743));
#57669=CARTESIAN_POINT('Ctrl Pts',(-1.7941821594327,49.0392196723324,13.8937348653189));
#57670=CARTESIAN_POINT('Ctrl Pts',(-1.81789005333813,49.0502102248727,13.8084980951964));
#57671=CARTESIAN_POINT('Ctrl Pts',(-1.85030248460895,49.065236044132,13.6919659829656));
#57672=CARTESIAN_POINT('Ctrl Pts',(-1.87130998121406,49.0802745152564,13.5723064933686));
#57673=CARTESIAN_POINT('Ctrl Pts',(-1.88083583906007,49.0953394774193,13.4518206289011));
#57674=CARTESIAN_POINT('Ctrl Pts',(-1.88761187874116,49.1060556546981,13.3661152770219));
#57675=CARTESIAN_POINT('Ctrl Pts',(-1.88857902809562,49.1167851575353,13.2799925802247));
#57676=CARTESIAN_POINT('Ctrl Pts',(-1.88372494476212,49.1275317726247,13.1942859874444));
#57677=CARTESIAN_POINT('Ctrl Pts',(-1.87755267939483,49.1411967543679,13.0853047858414));
#57678=CARTESIAN_POINT('Ctrl Pts',(-1.86203948095439,49.1548733590618,12.9767539644173));
#57679=CARTESIAN_POINT('Ctrl Pts',(-1.83710075861715,49.1685569018034,12.8703323036927));
#57680=CARTESIAN_POINT('Ctrl Pts',(-1.81005128630724,49.1833985847689,12.7549033845196));
#57681=CARTESIAN_POINT('Ctrl Pts',(-1.7719122407144,49.1982484328727,12.6419806903053));
#57682=CARTESIAN_POINT('Ctrl Pts',(-1.72364873600501,49.2131003184208,12.5335051899417));
#57683=CARTESIAN_POINT('Ctrl Pts',(-1.67524198645834,49.2279962839821,12.4247077370907));
#57684=CARTESIAN_POINT('Ctrl Pts',(-1.61665127013422,49.2428943005386,12.3203853663485));
#57685=CARTESIAN_POINT('Ctrl Pts',(-1.54889859525585,49.2577880297835,12.2224801538035));
#57686=CARTESIAN_POINT('Ctrl Pts',(-1.5081735481019,49.2667404117652,12.1636308994432));
#57687=CARTESIAN_POINT('Ctrl Pts',(-1.46413914973447,49.2756912416321,12.1070997655727));
#57688=CARTESIAN_POINT('Ctrl Pts',(-1.41702412181492,49.2846391126802,12.053302361519));
#57689=CARTESIAN_POINT('Ctrl Pts',(-1.4125881924468,49.2854815641382,12.0482372794187));
#57690=CARTESIAN_POINT('Ctrl Pts',(-1.40812459934876,49.2863240574281,12.0431960154616));
#57691=CARTESIAN_POINT('Ctrl Pts',(-1.40363352034152,49.2871665912809,12.0381789214648));
#57692=CARTESIAN_POINT('Ctrl Pts',(-1.3159668703761,49.3036129998704,11.9402443666394));
#57693=CARTESIAN_POINT('Ctrl Pts',(-1.21782338407748,49.3200747933399,11.8515220987113));
#57694=CARTESIAN_POINT('Ctrl Pts',(-1.11158589337901,49.3365428984598,11.7736691031812));
#57695=CARTESIAN_POINT('Ctrl Pts',(-1.00365240246168,49.3532739042723,11.6945732441704));
#57696=CARTESIAN_POINT('Ctrl Pts',(-0.887366003576533,49.3700114222832,
11.6266974114595));
#57697=CARTESIAN_POINT('Ctrl Pts',(-0.765256969791259,49.3867468451802,
11.5717380804842));
#57698=CARTESIAN_POINT('Ctrl Pts',(-0.718831634849412,49.3931095817388,
11.5508427767576));
#57699=CARTESIAN_POINT('Ctrl Pts',(-0.671564840019194,49.399472024888,11.5318140446093));
#57700=CARTESIAN_POINT('Ctrl Pts',(-0.623596072871047,49.405833736296,11.5147431601453));
#57701=CARTESIAN_POINT('Ctrl Pts',(-0.532872850951344,49.4178656268398,
11.4824570345751));
#57702=CARTESIAN_POINT('Ctrl Pts',(-0.439638967352969,49.4298948854296,
11.4571749515759));
#57703=CARTESIAN_POINT('Ctrl Pts',(-0.345025518837569,49.4419189000586,
11.4390557052432));
#57704=CARTESIAN_POINT('Ctrl Pts',(-0.284024353342111,49.4496712747771,
11.4273734849929));
#57705=CARTESIAN_POINT('Ctrl Pts',(-0.222389419767029,49.4574286193781,
11.4186556387847));
#57706=CARTESIAN_POINT('Ctrl Pts',(-0.160426678944839,49.4651909312848,
11.4129638843323));
#57707=CARTESIAN_POINT('Ctrl Pts',(-0.0509246993106248,49.4789086672828,
11.4029052850537));
#57708=CARTESIAN_POINT('Ctrl Pts',(0.0596021490212685,49.4926420138928,
11.4023002259455));
#57709=CARTESIAN_POINT('Ctrl Pts',(0.169418358914458,49.506389161536,11.4112375241642));
#57710=CARTESIAN_POINT('Ctrl Pts',(0.217924371137122,49.5124613007243,11.4151851444386));
#57711=CARTESIAN_POINT('Ctrl Pts',(0.266291423310214,49.5185361101893,11.4209938662932));
#57712=CARTESIAN_POINT('Ctrl Pts',(0.314368958306638,49.5246133272254,11.4286682717846));
#57713=CARTESIAN_POINT('Ctrl Pts',(0.422761076254026,49.538314579293,11.4459704289203));
#57714=CARTESIAN_POINT('Ctrl Pts',(0.529681050610087,49.5520281843259,11.4727590782111));
#57715=CARTESIAN_POINT('Ctrl Pts',(0.633557827194764,49.5657502923738,11.5084987179536));
#57716=CARTESIAN_POINT('Ctrl Pts',(0.680110637362215,49.5718999122605,11.5245155863922));
#57717=CARTESIAN_POINT('Ctrl Pts',(0.726052331747924,49.5780512168516,11.5423295073784));
#57718=CARTESIAN_POINT('Ctrl Pts',(0.771242460898877,49.5842037467633,11.5618889939815));
#57719=CARTESIAN_POINT('Ctrl Pts',(0.809264810044399,49.5893804002676,11.5783460752667));
#57720=CARTESIAN_POINT('Ctrl Pts',(0.846755103796012,49.5945579200084,11.5960388568935));
#57721=CARTESIAN_POINT('Ctrl Pts',(0.883622318728723,49.5997359852152,11.6149284240134));
#57722=CARTESIAN_POINT('Ctrl Pts',(0.974386618590373,49.6124839908345,11.6614331121886));
#57723=CARTESIAN_POINT('Ctrl Pts',(1.06166785697727,49.6252207027794,11.715139708312));
#57724=CARTESIAN_POINT('Ctrl Pts',(1.14410657474425,49.6379612282381,11.775622065151));
#57725=CARTESIAN_POINT('Ctrl Pts',(1.15692341031759,49.6399420113501,11.7850253218208));
#57726=CARTESIAN_POINT('Ctrl Pts',(1.16962312605051,49.6419228773749,11.7945922827835));
#57727=CARTESIAN_POINT('Ctrl Pts',(1.18220054132778,49.6439038728195,11.8043212610649));
#57728=CARTESIAN_POINT('Ctrl Pts',(1.26367653017654,49.6567366814052,11.8673451899483));
#57729=CARTESIAN_POINT('Ctrl Pts',(1.34002165985689,49.6695753222382,11.9371720643496));
#57730=CARTESIAN_POINT('Ctrl Pts',(1.41040025016923,49.6824295639781,12.0127526220316));
#57731=CARTESIAN_POINT('Ctrl Pts',(1.48079841329015,49.695287380578,12.0883541992281));
#57732=CARTESIAN_POINT('Ctrl Pts',(1.54522548452235,49.7081608107212,12.1697127558005));
#57733=CARTESIAN_POINT('Ctrl Pts',(1.60283895157809,49.7210546571543,12.2557268981212));
#57734=CARTESIAN_POINT('Ctrl Pts',(1.65818525223575,49.7334411136165,12.3383562697764));
#57735=CARTESIAN_POINT('Ctrl Pts',(1.70724251943844,49.7458463830365,12.4252815367258));
#57736=CARTESIAN_POINT('Ctrl Pts',(1.74927539554209,49.7582703635106,12.515482559182));
#57737=CARTESIAN_POINT('Ctrl Pts',(1.78916920388077,49.7700620832733,12.6010932200595));
#57738=CARTESIAN_POINT('Ctrl Pts',(1.82277928288667,49.7818855126595,12.6897593564606));
#57739=CARTESIAN_POINT('Ctrl Pts',(1.84959117159127,49.7937196540585,12.78057038105));
#57740=CARTESIAN_POINT('Ctrl Pts',(1.87549737767598,49.8051540483041,12.8683138870632));
#57741=CARTESIAN_POINT('Ctrl Pts',(1.89505805837168,49.8165984759503,12.9580592310516));
#57742=CARTESIAN_POINT('Ctrl Pts',(1.90825323336579,49.8280400743436,13.0488085486734));
#57743=CARTESIAN_POINT('Ctrl Pts',(1.91216170154511,49.8314291255128,13.0756888909483));
#57744=CARTESIAN_POINT('Ctrl Pts',(1.91551184574708,49.8348179682363,13.1026576218624));
#57745=CARTESIAN_POINT('Ctrl Pts',(1.91830350256686,49.8382063687107,13.1296896098372));
#57746=CARTESIAN_POINT('Ctrl Pts',(1.92953580783151,49.8518396878985,13.2384535304924));
#57747=CARTESIAN_POINT('Ctrl Pts',(1.93169044802515,49.8654785041309,13.348306963276));
#57748=CARTESIAN_POINT('Ctrl Pts',(1.9245084160203,49.8791350497271,13.4576550741967));
#57749=CARTESIAN_POINT('Ctrl Pts',(1.92360157678391,49.8808593933908,13.4714619128938));
#57750=CARTESIAN_POINT('Ctrl Pts',(1.92254587695862,49.8825840113469,13.4852606279965));
#57751=CARTESIAN_POINT('Ctrl Pts',(1.92134079226722,49.8843089209617,13.4990479505969));
#57752=CARTESIAN_POINT('Ctrl Pts',(1.91342147776945,49.8956443082728,13.5896524902889));
#57753=CARTESIAN_POINT('Ctrl Pts',(1.89905036197541,49.9069925388944,13.6797669564011));
#57754=CARTESIAN_POINT('Ctrl Pts',(1.87844238405721,49.9183567502638,13.768533416587));
#57755=CARTESIAN_POINT('Ctrl Pts',(1.85806813861979,49.9295920705153,13.8562931013857));
#57756=CARTESIAN_POINT('Ctrl Pts',(1.83147583519971,49.9408551558828,13.9427357798033));
#57757=CARTESIAN_POINT('Ctrl Pts',(1.79901109730714,49.9521347064582,14.0270300623742));
#57758=CARTESIAN_POINT('Ctrl Pts',(1.76649233280349,49.9634330280427,14.1114646243596));
#57759=CARTESIAN_POINT('Ctrl Pts',(1.72808276981835,49.9747478657175,14.1937439181842));
#57760=CARTESIAN_POINT('Ctrl Pts',(1.68411841978781,49.9860745920622,14.2730826788711));
#57761=CARTESIAN_POINT('Ctrl Pts',(1.66732052166656,49.9904023074738,14.3033964312218));
#57762=CARTESIAN_POINT('Ctrl Pts',(1.64971149644335,49.9947318285754,14.3332814061617));
#57763=CARTESIAN_POINT('Ctrl Pts',(1.63130911220971,49.9990631575573,14.3626955469288));
#57764=CARTESIAN_POINT('Ctrl Pts',(1.62163280526315,50.0013406487879,14.378162034913));
#57765=CARTESIAN_POINT('Ctrl Pts',(1.61174083809686,50.0036182017112,14.3934972853071));
#57766=CARTESIAN_POINT('Ctrl Pts',(1.60163402672504,50.0058959343056,14.4086945746061));
#57767=CARTESIAN_POINT('Ctrl Pts',(1.55666321793511,50.016030829794,14.4763157427519));
#57768=CARTESIAN_POINT('Ctrl Pts',(1.50743724227319,50.0261698123625,14.541209282367));
#57769=CARTESIAN_POINT('Ctrl Pts',(1.45431001726312,50.0363191647339,14.6028716824512));
#57770=CARTESIAN_POINT('Ctrl Pts',(1.40127456235842,50.0464509854698,14.664427569068));
#57771=CARTESIAN_POINT('Ctrl Pts',(1.34435038650263,50.0565931378105,14.7227628433547));
#57772=CARTESIAN_POINT('Ctrl Pts',(1.28391790547149,50.0667452221655,14.7773339478466));
#57773=CARTESIAN_POINT('Ctrl Pts',(1.25729144758455,50.0712182148663,14.8013778922752));
#57774=CARTESIAN_POINT('Ctrl Pts',(1.22998438643742,50.0756930490622,14.824690609789));
#57775=CARTESIAN_POINT('Ctrl Pts',(1.20203166275937,50.0801692812514,14.8472235002155));
#57776=CARTESIAN_POINT('Ctrl Pts',(1.12804255291437,50.0920175876617,14.9068666507039));
#57777=CARTESIAN_POINT('Ctrl Pts',(1.04977223436755,50.1038849490447,14.9614104879932));
#57778=CARTESIAN_POINT('Ctrl Pts',(0.96783739781816,50.1157763050814,15.0100683364991));
#57779=CARTESIAN_POINT('Ctrl Pts',(0.938590872010946,50.1200209080593,15.0274366877644));
#57780=CARTESIAN_POINT('Ctrl Pts',(0.908877794999064,50.1242685118152,15.0440547594811));
#57781=CARTESIAN_POINT('Ctrl Pts',(0.878727474825673,50.1285191529968,15.0598858023556));
#57782=CARTESIAN_POINT('Ctrl Pts',(0.793422786706762,50.1405455466871,15.1046767752954));
#57783=CARTESIAN_POINT('Ctrl Pts',(0.704614297266369,50.1525967170587,15.1431686163929));
#57784=CARTESIAN_POINT('Ctrl Pts',(0.613299149750707,50.1646691980739,15.1750659712351));
#57785=CARTESIAN_POINT('Ctrl Pts',(0.522111477449071,50.1767248260025,15.2069187976257));
#57786=CARTESIAN_POINT('Ctrl Pts',(0.428424044611456,50.1888017024246,15.2321943006212));
#57787=CARTESIAN_POINT('Ctrl Pts',(0.333281062570076,50.2008900790611,15.2505937858019));
#57788=CARTESIAN_POINT('Ctrl Pts',(0.238669253175742,50.2129109676404,15.2688905487109));
#57789=CARTESIAN_POINT('Ctrl Pts',(0.142618408570352,50.2249432204352,15.2803866693137));
#57790=CARTESIAN_POINT('Ctrl Pts',(0.046204394392973,50.2369711067171,15.2848019797074));
#57791=CARTESIAN_POINT('Ctrl Pts',(0.0273405857746152,50.2393244134105,
15.2856658538129));
#57792=CARTESIAN_POINT('Ctrl Pts',(0.00846301594625596,50.2416775342161,
15.2862587437213));
#57793=CARTESIAN_POINT('Ctrl Pts',(-0.0104200573975599,50.2440303240055,
15.2865786720814));
#57794=CARTESIAN_POINT('Ctrl Pts',(-0.106807620890628,50.2560400043727,
15.2882117280234));
#57795=CARTESIAN_POINT('Ctrl Pts',(-0.203498122787935,50.2680945843605,
15.2830885050845));
#57796=CARTESIAN_POINT('Ctrl Pts',(-0.299485996380947,50.2801882117298,
15.2708992987964));
#57797=CARTESIAN_POINT('Ctrl Pts',(-0.336200589439534,50.2848139273629,
15.2662370249922));
#57798=CARTESIAN_POINT('Ctrl Pts',(-0.37281186034304,50.2894453019465,15.2605411428792));
#57799=CARTESIAN_POINT('Ctrl Pts',(-0.40926168203733,50.2940818082829,15.2537950599671));
#57800=CARTESIAN_POINT('Ctrl Pts',(-0.505010731284271,50.3062613211832,
15.236073957505));
#57801=CARTESIAN_POINT('Ctrl Pts',(-0.599648307088963,50.3184766205361,
15.2111032485417));
#57802=CARTESIAN_POINT('Ctrl Pts',(-0.692179824458452,50.3307144389555,
15.1792970548347));
#57803=CARTESIAN_POINT('Ctrl Pts',(-0.78483404415089,50.3429684854536,15.1474486842137));
#57804=CARTESIAN_POINT('Ctrl Pts',(-0.87537560604112,50.3552451097819,15.1087460560846));
#57805=CARTESIAN_POINT('Ctrl Pts',(-0.962776741130743,50.3675257196077,
15.0636478012151));
#57806=CARTESIAN_POINT('Ctrl Pts',(-1.0494068711561,50.3796979966028,15.0189473785117));
#57807=CARTESIAN_POINT('Ctrl Pts',(-1.13295050533364,50.3918741775708,14.9679633451565));
#57808=CARTESIAN_POINT('Ctrl Pts',(-1.21239495140534,50.4040310889802,14.9111913742513));
#57809=CARTESIAN_POINT('Ctrl Pts',(-1.2264718097698,50.4061851869508,14.9011318794343));
#57810=CARTESIAN_POINT('Ctrl Pts',(-1.24041996478418,50.408338667228,14.890890793895));
#57811=CARTESIAN_POINT('Ctrl Pts',(-1.25423379087638,50.4104913845365,14.8804710471741));
#57812=CARTESIAN_POINT('Ctrl Pts',(-1.34117925715569,50.4240407812718,14.8148882223206));
#57813=CARTESIAN_POINT('Ctrl Pts',(-1.42318024899639,50.437645038114,14.7423348026361));
#57814=CARTESIAN_POINT('Ctrl Pts',(-1.49891581544433,50.4512937034892,14.6633880757765));
#57815=CARTESIAN_POINT('Ctrl Pts',(-1.51914701857044,50.4549396644895,14.6422990770121));
#57816=CARTESIAN_POINT('Ctrl Pts',(-1.53893094679464,50.4585887653775,14.620754084337));
#57817=CARTESIAN_POINT('Ctrl Pts',(-1.558242059404,50.4622407435146,14.5987646089574));
#57818=CARTESIAN_POINT('Ctrl Pts',(-1.63288880051887,50.4763573960387,14.513764707133));
#57819=CARTESIAN_POINT('Ctrl Pts',(-1.70047167800137,50.4905175015514,14.4221188719292));
#57820=CARTESIAN_POINT('Ctrl Pts',(-1.76009939321026,50.5047025029048,14.3253128965409));
#57821=CARTESIAN_POINT('Ctrl Pts',(-1.8182349901732,50.5185325401403,14.2309293846276));
#57822=CARTESIAN_POINT('Ctrl Pts',(-1.86880721828935,50.5323862156151,14.1316410694346));
#57823=CARTESIAN_POINT('Ctrl Pts',(-1.91113795400556,50.5462404940161,14.0287752659255));
#57824=CARTESIAN_POINT('Ctrl Pts',(-1.94478507797625,50.5572527435081,13.9470110729708));
#57825=CARTESIAN_POINT('Ctrl Pts',(-1.97322493243461,50.5682652694524,13.8629877245061));
#57826=CARTESIAN_POINT('Ctrl Pts',(-1.99612549706287,50.5792641314507,13.7773936504254));
#57827=CARTESIAN_POINT('Ctrl Pts',(-2.02626276085829,50.5937386918325,13.6647513976352));
#57828=CARTESIAN_POINT('Ctrl Pts',(-2.04712883468148,50.6082867669309,13.5493023740913));
#57829=CARTESIAN_POINT('Ctrl Pts',(-2.05795982560911,50.6228939413266,13.432532945082));
#57830=CARTESIAN_POINT('Ctrl Pts',(-2.06039053292552,50.6261721054311,13.406327373743));
#57831=CARTESIAN_POINT('Ctrl Pts',(-2.0623159026598,50.6294532294161,13.3800554921823));
#57832=CARTESIAN_POINT('Ctrl Pts',(-2.06372746576267,50.6327371214468,13.3537344183884));
#57833=CARTESIAN_POINT('Ctrl Pts',(-2.07004524593896,50.6474349468084,13.2359283083419));
#57834=CARTESIAN_POINT('Ctrl Pts',(-2.06606711496515,50.6621885566942,13.1171341445939));
#57835=CARTESIAN_POINT('Ctrl Pts',(-2.05205326534908,50.6769783447938,12.9993851820754));
#57836=CARTESIAN_POINT('Ctrl Pts',(-2.05069601058759,50.6784107499408,12.9879810822444));
#57837=CARTESIAN_POINT('Ctrl Pts',(-2.0492446528101,50.6798434911776,12.9765868092299));
#57838=CARTESIAN_POINT('Ctrl Pts',(-2.04769945043919,50.6812765485945,12.9652042232842));
#57839=CARTESIAN_POINT('Ctrl Pts',(-2.03194857141904,50.6958842882845,12.8491768746707));
#57840=CARTESIAN_POINT('Ctrl Pts',(-2.00644258990089,50.7105252071379,12.7343629603841));
#57841=CARTESIAN_POINT('Ctrl Pts',(-1.971414945706,50.725175952002,12.6222505812766));
#57842=CARTESIAN_POINT('Ctrl Pts',(-1.96749237097443,50.7268166173372,12.609695663711));
#57843=CARTESIAN_POINT('Ctrl Pts',(-1.96345044163711,50.7284574018316,12.5971746326607));
#57844=CARTESIAN_POINT('Ctrl Pts',(-1.95928952687661,50.7300982696216,12.5846895813309));
#57845=CARTESIAN_POINT('Ctrl Pts',(-1.94164973720009,50.7370545675437,12.5317604317967));
#57846=CARTESIAN_POINT('Ctrl Pts',(-1.92187127034554,50.744012377997,12.4794779791356));
#57847=CARTESIAN_POINT('Ctrl Pts',(-1.90002458491759,50.7509688439665,12.4280317948976));
#57848=CARTESIAN_POINT('Ctrl Pts',(-1.85785924507542,50.764395217165,12.328737746419));
#57849=CARTESIAN_POINT('Ctrl Pts',(-1.80806813568785,50.7779138527103,12.2322626922288));
#57850=CARTESIAN_POINT('Ctrl Pts',(-1.75102971121399,50.7915034847982,12.1399629132644));
#57851=CARTESIAN_POINT('Ctrl Pts',(-1.69905782948915,50.8038859928718,12.0558618315844));
#57852=CARTESIAN_POINT('Ctrl Pts',(-1.64106911183378,50.8163273896247,11.9752284416276));
#57853=CARTESIAN_POINT('Ctrl Pts',(-1.5773822155289,50.8288083149998,11.8991079060624));
#57854=CARTESIAN_POINT('Ctrl Pts',(-1.50691721254408,50.842617567685,11.8148859691019));
#57855=CARTESIAN_POINT('Ctrl Pts',(-1.42947566304557,50.8564752768747,11.7361897647438));
#57856=CARTESIAN_POINT('Ctrl Pts',(-1.34620116056982,50.8703507651883,11.6638070823509));
#57857=CARTESIAN_POINT('Ctrl Pts',(-1.2629885637345,50.8842159385678,11.591478208701));
#57858=CARTESIAN_POINT('Ctrl Pts',(-1.17395204342079,50.898098857206,11.5254547521015));
#57859=CARTESIAN_POINT('Ctrl Pts',(-1.08028227234088,50.9119643914035,11.4665101279605));
#57860=CARTESIAN_POINT('Ctrl Pts',(-1.04634056534299,50.9169886366181,11.445151250506));
#57861=CARTESIAN_POINT('Ctrl Pts',(-1.01179094998515,50.9220105568077,11.4247216168608));
#57862=CARTESIAN_POINT('Ctrl Pts',(-0.976691501791933,50.9270283371022,
11.4052571049783));
#57863=CARTESIAN_POINT('Ctrl Pts',(-0.884937477897842,50.9401453961086,
11.3543746159281));
#57864=CARTESIAN_POINT('Ctrl Pts',(-0.789167206110581,50.9532737375235,
11.3099416664974));
#57865=CARTESIAN_POINT('Ctrl Pts',(-0.690438375184751,50.9664180064903,
11.2726169599394));
#57866=CARTESIAN_POINT('Ctrl Pts',(-0.592043153771279,50.9795178603341,
11.2354183753768));
#57867=CARTESIAN_POINT('Ctrl Pts',(-0.490710572213136,50.992633538247,11.2052802004869));
#57868=CARTESIAN_POINT('Ctrl Pts',(-0.387495446867673,51.005772276969,11.1828042558989));
#57869=CARTESIAN_POINT('Ctrl Pts',(-0.325448366228293,51.0136705416686,
11.1692929924902));
#57870=CARTESIAN_POINT('Ctrl Pts',(-0.262721040796763,51.0215771905168,
11.1585496764105));
#57871=CARTESIAN_POINT('Ctrl Pts',(-0.19954130283245,51.0294942462609,11.1506960304855));
#57872=CARTESIAN_POINT('Ctrl Pts',(-0.0949346514238878,51.0426025103515,
11.1376927539915));
#57873=CARTESIAN_POINT('Ctrl Pts',(0.0109104768394059,51.0557391746088,
11.1326131283539));
#57874=CARTESIAN_POINT('Ctrl Pts',(0.116743595274185,51.0689153793944,11.1352504856376));
#57875=CARTESIAN_POINT('Ctrl Pts',(0.213817704011632,51.0810010890005,11.1376695687329));
#57876=CARTESIAN_POINT('Ctrl Pts',(0.310881342433441,51.0931200967982,11.1465802513686));
#57877=CARTESIAN_POINT('Ctrl Pts',(0.406995758654726,51.1052827788823,11.1617947627978));
#57878=CARTESIAN_POINT('Ctrl Pts',(0.475225197012527,51.1139167903049,11.1725951984714));
#57879=CARTESIAN_POINT('Ctrl Pts',(0.543114902989226,51.122550766893,11.1866681096965));
#57880=CARTESIAN_POINT('Ctrl Pts',(0.610317925577959,51.1311896951867,11.2039733231974));
#57881=CARTESIAN_POINT('Ctrl Pts',(0.720705572369544,51.1453799939026,11.2323988570796));
#57882=CARTESIAN_POINT('Ctrl Pts',(0.829238241388482,51.1595834110016,11.2695473147213));
#57883=CARTESIAN_POINT('Ctrl Pts',(0.934470959369924,51.1738257667431,11.3150044503832));
#57884=CARTESIAN_POINT('Ctrl Pts',(1.03984233068126,51.1880868880367,11.3605214798057));
#57885=CARTESIAN_POINT('Ctrl Pts',(1.14190435883492,51.2023870583837,11.4143679537695));
#57886=CARTESIAN_POINT('Ctrl Pts',(1.23924938699954,51.2167567973926,11.4761000902931));
#57887=CARTESIAN_POINT('Ctrl Pts',(1.27788759182712,51.2224604365985,11.5006028202262));
#57888=CARTESIAN_POINT('Ctrl Pts',(1.31578318420242,51.2281750861814,11.5263476861861));
#57889=CARTESIAN_POINT('Ctrl Pts',(1.35285032883315,51.2339028502947,11.5533062962545));
#57890=CARTESIAN_POINT('Ctrl Pts',(1.44658576544506,51.2483872265617,11.6214792594105));
#57891=CARTESIAN_POINT('Ctrl Pts',(1.53501985110568,51.2629551626989,11.6974132567916));
#57892=CARTESIAN_POINT('Ctrl Pts',(1.61730548063149,51.2776437369066,11.7798474230589));
#57893=CARTESIAN_POINT('Ctrl Pts',(1.63586064267326,51.2809559662249,11.7984360796893));
#57894=CARTESIAN_POINT('Ctrl Pts',(1.65410336719204,51.2842743472626,11.8173553037568));
#57895=CARTESIAN_POINT('Ctrl Pts',(1.67202429616646,51.287599335277,11.8365907362258));
#57896=CARTESIAN_POINT('Ctrl Pts',(1.74730869978597,51.3015673466487,11.9173972649422));
#57897=CARTESIAN_POINT('Ctrl Pts',(1.81684091453586,51.3154633698883,12.0041923127625));
#57898=CARTESIAN_POINT('Ctrl Pts',(1.87981515976553,51.3293199286473,12.0958702323521));
#57899=CARTESIAN_POINT('Ctrl Pts',(1.94326560255564,51.3432812676931,12.1882414004514));
#57900=CARTESIAN_POINT('Ctrl Pts',(2.00005877031958,51.357202544524,12.285568209684));
#57901=CARTESIAN_POINT('Ctrl Pts',(2.0494234544693,51.3711221643026,12.3867219798677));
#57902=CARTESIAN_POINT('Ctrl Pts',(2.09864971396905,51.3850027517541,12.4875921024302));
#57903=CARTESIAN_POINT('Ctrl Pts',(2.14048952988282,51.3988817041221,12.592266729379));
#57904=CARTESIAN_POINT('Ctrl Pts',(2.17422535347785,51.4128020754618,12.6996467516589));
#57905=CARTESIAN_POINT('Ctrl Pts',(2.19881412754627,51.4229481110212,12.777912014692));
#57906=CARTESIAN_POINT('Ctrl Pts',(2.2190987512973,51.4331162540573,12.8576149130984));
#57907=CARTESIAN_POINT('Ctrl Pts',(2.23481506548427,51.4433247841335,12.9383406646595));
#57908=CARTESIAN_POINT('Ctrl Pts',(2.25000922374029,51.4531941478846,13.0163843987032));
#57909=CARTESIAN_POINT('Ctrl Pts',(2.26093395368737,51.4631012689016,13.0953840515804));
#57910=CARTESIAN_POINT('Ctrl Pts',(2.26767989392229,51.4730637999864,13.1748713078923));
#57911=CARTESIAN_POINT('Ctrl Pts',(2.27801605302903,51.4883284336492,13.2966620293613));
#57912=CARTESIAN_POINT('Ctrl Pts',(2.27839959800904,51.5036301509547,13.4199225311563));
#57913=CARTESIAN_POINT('Ctrl Pts',(2.26898183281624,51.5189755570549,13.5429175800468));
#57914=CARTESIAN_POINT('Ctrl Pts',(2.25941221926975,51.534568386467,13.6678957528848));
#57915=CARTESIAN_POINT('Ctrl Pts',(2.23972308856393,51.5502063253031,13.7925983831649));
#57916=CARTESIAN_POINT('Ctrl Pts',(2.21012819997815,51.5658978695212,13.915205273457));
#57917=CARTESIAN_POINT('Ctrl Pts',(2.18127044876477,51.5811985751781,14.0347583215058));
#57918=CARTESIAN_POINT('Ctrl Pts',(2.14299489697288,51.5965502601759,14.1523175527705));
#57919=CARTESIAN_POINT('Ctrl Pts',(2.09554325266421,51.6119621762579,14.2662152151626));
#57920=CARTESIAN_POINT('Ctrl Pts',(2.0485582186183,51.6272225410435,14.3789928780488));
#57921=CARTESIAN_POINT('Ctrl Pts',(1.99257709650871,51.6425419658411,14.4881796253961));
#57922=CARTESIAN_POINT('Ctrl Pts',(1.92787003969126,51.6579306647238,14.5921921555573));
#57923=CARTESIAN_POINT('Ctrl Pts',(1.86255948817896,51.6734628873363,14.6971747655405));
#57924=CARTESIAN_POINT('Ctrl Pts',(1.7883614277045,51.6890656867666,14.7968859216486));
#57925=CARTESIAN_POINT('Ctrl Pts',(1.7066345985162,51.7047506996867,14.8902798816078));
#57926=CARTESIAN_POINT('Ctrl Pts',(1.66581357159012,51.7125850711055,14.936928422755));
#57927=CARTESIAN_POINT('Ctrl Pts',(1.62311439888885,51.7204399711188,14.9820017033674));
#57928=CARTESIAN_POINT('Ctrl Pts',(1.57870657579314,51.7283169522183,15.0253743524037));
#57929=CARTESIAN_POINT('Ctrl Pts',(1.50047847559116,51.7421929142401,15.1017789067888));
#57930=CARTESIAN_POINT('Ctrl Pts',(1.41654901118027,51.756100645792,15.1731573813177));
#57931=CARTESIAN_POINT('Ctrl Pts',(1.32777894335815,51.7700336438041,15.2386647004963));
#57932=CARTESIAN_POINT('Ctrl Pts',(1.23747687650584,51.784207098312,15.3053025488264));
#57933=CARTESIAN_POINT('Ctrl Pts',(1.14216653685236,51.7984066987655,15.3658640092509));
#57934=CARTESIAN_POINT('Ctrl Pts',(1.04280039150845,51.8126258034887,15.4194885002371));
#57935=CARTESIAN_POINT('Ctrl Pts',(0.944082085006813,51.8267522037168,15.4727633748821));
#57936=CARTESIAN_POINT('Ctrl Pts',(0.841361704843203,51.8408978556128,15.5191907371094));
#57937=CARTESIAN_POINT('Ctrl Pts',(0.735604232794058,51.8550564392127,15.5579664995614));
#57938=CARTESIAN_POINT('Ctrl Pts',(0.672327759979994,51.8635277577199,15.5811666898752));
#57939=CARTESIAN_POINT('Ctrl Pts',(0.607964582592411,51.8720037091988,15.6016285497847));
#57940=CARTESIAN_POINT('Ctrl Pts',(0.542724481630528,51.8804829711198,15.6191882969655));
#57941=CARTESIAN_POINT('Ctrl Pts',(0.433306805066517,51.8947039966041,15.6486386918797));
#57942=CARTESIAN_POINT('Ctrl Pts',(0.321422964300072,51.9089343250588,15.6699231722959));
#57943=CARTESIAN_POINT('Ctrl Pts',(0.208379630461429,51.9231677789593,15.6831294558649));
#57944=CARTESIAN_POINT('Ctrl Pts',(0.0975655914236256,51.9371205390436,
15.696075302146));
#57945=CARTESIAN_POINT('Ctrl Pts',(-0.0143615258194681,51.9510763040823,
15.7012587366926));
#57946=CARTESIAN_POINT('Ctrl Pts',(-0.126183054695298,51.965029402954,15.6988098364548));
#57947=CARTESIAN_POINT('Ctrl Pts',(-0.198236902745661,51.97402028759,15.6972318515409));
#57948=CARTESIAN_POINT('Ctrl Pts',(-0.270247206108331,51.9830100681522,
15.6924858204689));
#57949=CARTESIAN_POINT('Ctrl Pts',(-0.341893915334161,51.9919972563659,
15.6846164396408));
#57950=CARTESIAN_POINT('Ctrl Pts',(-0.452329377343791,52.0058500109903,
15.67248666122));
#57951=CARTESIAN_POINT('Ctrl Pts',(-0.562480536841933,52.0197557230553,
15.6528594899942));
#57952=CARTESIAN_POINT('Ctrl Pts',(-0.671147032885876,52.0337055294602,
15.6257021304772));
#57953=CARTESIAN_POINT('Ctrl Pts',(-0.782314303434172,52.0479763669231,
15.5979197905406));
#57954=CARTESIAN_POINT('Ctrl Pts',(-0.891926596930965,52.0622933521822,
15.5622565487633));
#57955=CARTESIAN_POINT('Ctrl Pts',(-0.99868441702179,52.076646931506,15.5187296367709));
#57956=CARTESIAN_POINT('Ctrl Pts',(-1.07193701850435,52.0864957371969,15.4888633512357));
#57957=CARTESIAN_POINT('Ctrl Pts',(-1.14384539681097,52.0963617704336,15.4552958631548));
#57958=CARTESIAN_POINT('Ctrl Pts',(-1.21399056123118,52.1062419256841,15.4180469111777));
#57959=CARTESIAN_POINT('Ctrl Pts',(-1.31504572326384,52.120475846126,15.3643839265842));
#57960=CARTESIAN_POINT('Ctrl Pts',(-1.41243978109377,52.1347390801274,15.3030779985422));
#57961=CARTESIAN_POINT('Ctrl Pts',(-1.50527291662462,52.1490222468805,15.235008197586));
#57962=CARTESIAN_POINT('Ctrl Pts',(-1.5984260151893,52.1633546426652,15.166703784065));
#57963=CARTESIAN_POINT('Ctrl Pts',(-1.68698581781993,52.1777071093187,15.0915896966614));
#57964=CARTESIAN_POINT('Ctrl Pts',(-1.77007593847986,52.1920700892426,15.0105950709922));
#57965=CARTESIAN_POINT('Ctrl Pts',(-1.85100589705314,52.2060596629849,14.9317061291059));
#57966=CARTESIAN_POINT('Ctrl Pts',(-1.92674628733797,52.2200592105307,14.8472393949193));
#57967=CARTESIAN_POINT('Ctrl Pts',(-1.99652887804495,52.2340598218168,14.7580781735643));
#57968=CARTESIAN_POINT('Ctrl Pts',(-2.04046443220278,52.2428746939672,14.7019417127374));
#57969=CARTESIAN_POINT('Ctrl Pts',(-2.08203915034671,52.2516899862194,14.6439447809136));
#57970=CARTESIAN_POINT('Ctrl Pts',(-2.12107165008936,52.2605034578968,14.58431058459));
#57971=CARTESIAN_POINT('Ctrl Pts',(-2.17629436357354,52.272972652144,14.49994083735));
#57972=CARTESIAN_POINT('Ctrl Pts',(-2.22650631414255,52.2852457466958,14.4118971504242));
#57973=CARTESIAN_POINT('Ctrl Pts',(-2.2712142963379,52.2975259079814,14.3208300079618));
#57974=CARTESIAN_POINT('Ctrl Pts',(-2.31592227853324,52.309806069267,14.2297628654994));
#57975=CARTESIAN_POINT('Ctrl Pts',(-2.35512731139636,52.3220933259785,14.1356727343629));
#57976=CARTESIAN_POINT('Ctrl Pts',(-2.38836719431143,52.3345987243418,14.039166525391));
#57977=CARTESIAN_POINT('Ctrl Pts',(-1.22475759790445,61.5085174595755,10.2717937103395));
#57978=CARTESIAN_POINT('Ctrl Pts',(-0.558011100714539,61.5982486649959,
10.0030310024535));
#57979=CARTESIAN_POINT('Ctrl Pts',(0.957582776261939,61.7776481271537,9.92475194519782));
#57980=CARTESIAN_POINT('Ctrl Pts',(2.81969758661395,62.0461398867496,11.2283079993549));
#57981=CARTESIAN_POINT('Ctrl Pts',(3.48222140378021,62.3136428581871,13.3935715300134));
#57982=CARTESIAN_POINT('Ctrl Pts',(2.67681707758244,62.579773345974,15.497292108503));
#57983=CARTESIAN_POINT('Ctrl Pts',(0.759902248054433,62.8441604986882,16.6530507103859));
#57984=CARTESIAN_POINT('Ctrl Pts',(-1.44458547024767,63.1064443544619,16.3863495812049));
#57985=CARTESIAN_POINT('Ctrl Pts',(-3.00432898132876,63.3662787322575,14.8364237012945));
#57986=CARTESIAN_POINT('Ctrl Pts',(-3.26685589537852,63.6138139233043,12.7543667878087));
#57987=CARTESIAN_POINT('Ctrl Pts',(-2.47105982748424,63.811474368391,11.3089218924462));
#57988=CARTESIAN_POINT('Ctrl Pts',(-1.00806246152439,64.0353924428549,10.2305976232193));
#57989=CARTESIAN_POINT('Ctrl Pts',(1.2619356887499,64.293423364255,10.1359463299035));
#57990=CARTESIAN_POINT('Ctrl Pts',(3.17140149111836,64.6184082729688,12.2928073226734));
#57991=CARTESIAN_POINT('Ctrl Pts',(2.73437323989231,64.9360819775815,15.0617858882019));
#57992=CARTESIAN_POINT('Ctrl Pts',(0.366119910750528,65.2460149715181,16.4456710631955));
#57993=CARTESIAN_POINT('Ctrl Pts',(-2.13523691433573,65.5478718326797,15.5180124762315));
#57994=CARTESIAN_POINT('Ctrl Pts',(-2.98478079778392,65.841387878141,13.0674399329054));
#57995=CARTESIAN_POINT('Ctrl Pts',(-1.66701189783808,66.1264296862307,10.9156975846686));
#57996=CARTESIAN_POINT('Ctrl Pts',(0.751927388912868,66.4029443584298,10.5875584960911));
#57997=CARTESIAN_POINT('Ctrl Pts',(2.49274638058045,66.6709882204905,12.19252620218));
#57998=CARTESIAN_POINT('Ctrl Pts',(2.35910723949879,66.9307237214747,14.4856574268905));
#57999=CARTESIAN_POINT('Ctrl Pts',(0.71660521689825,67.1614233848501,15.6875003337387));
#58000=CARTESIAN_POINT('Ctrl Pts',(-0.996423457277477,67.3655344712751,
15.4400425861523));
#58001=CARTESIAN_POINT('Ctrl Pts',(-2.05297602182105,67.5450863880253,14.3512624693526));
#58002=CARTESIAN_POINT('Ctrl Pts',(-2.21336612279098,67.7206997564268,12.8715592664714));
#58003=CARTESIAN_POINT('Ctrl Pts',(-1.44710288542824,67.892614429265,11.6346115739884));
#58004=CARTESIAN_POINT('Ctrl Pts',(-0.109789305964637,68.0610877835164,
11.1391611146274));
#58005=CARTESIAN_POINT('Ctrl Pts',(1.22398483030438,68.2264079408537,11.5627232550221));
#58006=CARTESIAN_POINT('Ctrl Pts',(2.00193544971486,68.3888854005119,12.6965891887889));
#58007=CARTESIAN_POINT('Ctrl Pts',(1.91987771499495,68.5488359593493,14.0479937472136));
#58008=CARTESIAN_POINT('Ctrl Pts',(1.03645178894531,68.7066105132279,15.0496273315261));
#58009=CARTESIAN_POINT('Ctrl Pts',(-0.260707618104073,68.8625671064471,
15.2940633739598));
#58010=CARTESIAN_POINT('Ctrl Pts',(-1.4240215170718,69.0170673179846,14.6948442918268));
#58011=CARTESIAN_POINT('Ctrl Pts',(-1.90763689933083,69.1534481987426,13.6471050935586));
#58012=CARTESIAN_POINT('Ctrl Pts',(-1.81977406488792,69.2426201973106,12.9197483588915));
#58013=CARTESIAN_POINT('Ctrl Pts',(-1.69804219571952,69.2850346430207,12.6023842455621));
#58014=CARTESIAN_POINT('Ctrl Pts',(-1.64242831287433,69.3019970791238,12.4783116538297));
#58015=CARTESIAN_POINT('Ctrl Pts',(-1.52735037370308,69.3316743635896,12.2698368113331));
#58016=CARTESIAN_POINT('Ctrl Pts',(-1.23065205270035,69.3909991147362,11.8947040913177));
#58017=CARTESIAN_POINT('Ctrl Pts',(-0.645158799006976,69.4757025248837,
11.5193939124166));
#58018=CARTESIAN_POINT('Ctrl Pts',(0.044810345871984,69.5604396628484,11.4303795861512));
#58019=CARTESIAN_POINT('Ctrl Pts',(0.580700809085593,69.6283146835187,11.5411475348396));
#58020=CARTESIAN_POINT('Ctrl Pts',(0.861510638146726,69.666531265754,11.6677365653311));
#58021=CARTESIAN_POINT('Ctrl Pts',(1.03443845903176,69.69203334437,11.7767096136909));
#58022=CARTESIAN_POINT('Ctrl Pts',(1.14565717774328,69.709040761661,11.8555746554773));
#58023=CARTESIAN_POINT('Ctrl Pts',(1.32809052278142,69.7388195747815,12.0096995333949));
#58024=CARTESIAN_POINT('Ctrl Pts',(1.82067835896352,69.832521589919,12.5831930627474));
#58025=CARTESIAN_POINT('Ctrl Pts',(2.03046072987068,69.9865805680574,13.9254562576328));
#58026=CARTESIAN_POINT('Ctrl Pts',(0.810259096530256,70.1944780346027,15.2994738528175));
#58027=CARTESIAN_POINT('Ctrl Pts',(-1.05830745474474,70.4057338895888,15.2249363050774));
#58028=CARTESIAN_POINT('Ctrl Pts',(-2.07493719267882,70.5972153712582,13.8764528995484));
#58029=CARTESIAN_POINT('Ctrl Pts',(-1.94180353342299,70.7679921684942,12.450736958435));
#58030=CARTESIAN_POINT('Ctrl Pts',(-1.16039001901908,70.9167953919606,11.4835575608119));
#58031=CARTESIAN_POINT('Ctrl Pts',(0.100587899379937,71.0745421465401,11.0884895976554));
#58032=CARTESIAN_POINT('Ctrl Pts',(1.44344797546005,71.2418455914631,11.5364757461608));
#58033=CARTESIAN_POINT('Ctrl Pts',(2.27501583067712,71.4194119422884,12.7892555436196));
#58034=CARTESIAN_POINT('Ctrl Pts',(2.15695780511918,71.6010238110375,14.3220345011878));
#58035=CARTESIAN_POINT('Ctrl Pts',(1.09667342325315,71.7868784116616,15.4844988867453));
#58036=CARTESIAN_POINT('Ctrl Pts',(-0.49121362380328,71.9771479946895,15.7544990355271));
#58037=CARTESIAN_POINT('Ctrl Pts',(-1.94315347613286,72.1719682245206,14.9722576142499));
#58038=CARTESIAN_POINT('Ctrl Pts',(-2.62186916830043,72.3714469815617,13.4254905457947));
#58039=CARTESIAN_POINT('Ctrl Pts',(-2.33801236899026,72.5075907029867,12.3091065046127));
#58040=CARTESIAN_POINT('Ctrl Pts',(-2.03365423424493,72.5764593847717,11.8488939074775));
#58041=CARTESIAN_POINT('Ctrl Pts',(-1.16855233243332,61.7161262168237,10.525919406708));
#58042=CARTESIAN_POINT('Ctrl Pts',(-0.554998030824625,61.7988802657359,
10.2746212855555));
#58043=CARTESIAN_POINT('Ctrl Pts',(0.838410518237986,61.9638525873806,10.196079471243));
#58044=CARTESIAN_POINT('Ctrl Pts',(2.54752277558488,62.2094399693199,11.3802377323902));
#58045=CARTESIAN_POINT('Ctrl Pts',(3.16045683740201,62.4529270793634,13.3481442920267));
#58046=CARTESIAN_POINT('Ctrl Pts',(2.44047887098306,62.6940925191325,15.2583700375192));
#58047=CARTESIAN_POINT('Ctrl Pts',(0.715779595689003,62.9327332534007,16.3109031130561));
#58048=CARTESIAN_POINT('Ctrl Pts',(-1.26860182455947,63.1686623612665,16.0820261164684));
#58049=CARTESIAN_POINT('Ctrl Pts',(-2.67561081487942,63.4017112264679,14.6998608482283));
#58050=CARTESIAN_POINT('Ctrl Pts',(-2.92163267124444,63.6232113919738,12.8381512919378));
#58051=CARTESIAN_POINT('Ctrl Pts',(-2.21872134954113,63.7997944393218,11.5423534614023));
#58052=CARTESIAN_POINT('Ctrl Pts',(-0.918841957931743,63.9996769886031,
10.5713624439231));
#58053=CARTESIAN_POINT('Ctrl Pts',(1.10544430662327,64.2298315981922,10.4739099322025));
#58054=CARTESIAN_POINT('Ctrl Pts',(2.82170825137881,64.51970605799,12.386084982752));
#58055=CARTESIAN_POINT('Ctrl Pts',(2.44933207825223,64.8034347666427,14.861988589747));
#58056=CARTESIAN_POINT('Ctrl Pts',(0.338060403298642,65.0809899103029,16.1176314364466));
#58057=CARTESIAN_POINT('Ctrl Pts',(-1.91793964377472,65.3524085900801,15.3018101953666));
#58058=CARTESIAN_POINT('Ctrl Pts',(-2.70511906831274,65.617817100817,13.0925450247269));
#58059=CARTESIAN_POINT('Ctrl Pts',(-1.52283152014212,65.8773964748908,11.1221290228538));
#58060=CARTESIAN_POINT('Ctrl Pts',(0.696638563926616,66.1314053760008,10.7997873793317));
#58061=CARTESIAN_POINT('Ctrl Pts',(2.32681777167293,66.3801709599473,12.2734845553138));
#58062=CARTESIAN_POINT('Ctrl Pts',(2.22322828832599,66.6240853182049,14.4283580565722));
#58063=CARTESIAN_POINT('Ctrl Pts',(0.671999738656957,66.8436213521831,15.5881093952669));
#58064=CARTESIAN_POINT('Ctrl Pts',(-0.98168785283175,67.0403488125919,15.3648459972412));
#58065=CARTESIAN_POINT('Ctrl Pts',(-2.02163523086829,67.2154312967404,14.3123594021697));
#58066=CARTESIAN_POINT('Ctrl Pts',(-2.19335801564648,67.3887819673487,12.8531399104545));
#58067=CARTESIAN_POINT('Ctrl Pts',(-1.43842230298015,67.5606555223828,11.6093759169369));
#58068=CARTESIAN_POINT('Ctrl Pts',(-0.0881736940427007,67.7313096264736,
11.0953138370229));
#58069=CARTESIAN_POINT('Ctrl Pts',(1.285019963464,67.9010179476805,11.5180318096301));
#58070=CARTESIAN_POINT('Ctrl Pts',(2.10476272204221,68.0700606754811,12.6908480644406));
#58071=CARTESIAN_POINT('Ctrl Pts',(2.03032672148608,68.2387109111275,14.1166691843227));
#58072=CARTESIAN_POINT('Ctrl Pts',(1.09526545073582,68.4072597306901,15.1946230376736));
#58073=CARTESIAN_POINT('Ctrl Pts',(-0.306217453601036,68.5759923130744,
15.4702676537639));
#58074=CARTESIAN_POINT('Ctrl Pts',(-1.5853325914691,68.7451861618208,14.8237290916841));
#58075=CARTESIAN_POINT('Ctrl Pts',(-2.12944594400514,68.8962437383695,13.6669630662597));
#58076=CARTESIAN_POINT('Ctrl Pts',(-2.03617398744539,68.9958751434108,12.8535321776987));
#58077=CARTESIAN_POINT('Ctrl Pts',(-1.90149875738473,69.0434408618903,12.4968846241885));
#58078=CARTESIAN_POINT('Ctrl Pts',(-1.8398000356147,69.0624786705015,12.3572951814658));
#58079=CARTESIAN_POINT('Ctrl Pts',(-1.71169761948827,69.0958262736986,12.1223446655951));
#58080=CARTESIAN_POINT('Ctrl Pts',(-1.37973281194231,69.1626459611235,11.6980269719962));
#58081=CARTESIAN_POINT('Ctrl Pts',(-0.719622242441448,69.2584844300639,
11.2695961091932));
#58082=CARTESIAN_POINT('Ctrl Pts',(0.0649084390206912,69.3548948427999,
11.1640051083998));
#58083=CARTESIAN_POINT('Ctrl Pts',(0.677588055410269,69.4324078644648,11.2874874815619));
#58084=CARTESIAN_POINT('Ctrl Pts',(0.999777033894293,69.4761562418558,11.4308378696215));
#58085=CARTESIAN_POINT('Ctrl Pts',(1.19860894090253,69.5053887889003,11.5548233552111));
#58086=CARTESIAN_POINT('Ctrl Pts',(1.32660386294558,69.5248947079024,11.6446756441626));
#58087=CARTESIAN_POINT('Ctrl Pts',(1.53686134829739,69.5590761839442,11.8206234250448));
#58088=CARTESIAN_POINT('Ctrl Pts',(2.10636022605492,69.6668006528317,12.4771751346531));
#58089=CARTESIAN_POINT('Ctrl Pts',(2.35791538563205,69.8447713562475,14.0265754559266));
#58090=CARTESIAN_POINT('Ctrl Pts',(0.949121047530638,70.0862200241309,15.6301546468009));
#58091=CARTESIAN_POINT('Ctrl Pts',(-1.22826102218047,70.3322944313609,15.5534418241006));
#58092=CARTESIAN_POINT('Ctrl Pts',(-2.41979078179111,70.5554983884945,13.9862112724621));
#58093=CARTESIAN_POINT('Ctrl Pts',(-2.27116036733893,70.7543056449801,12.3257473977465));
#58094=CARTESIAN_POINT('Ctrl Pts',(-1.36738576107812,70.9271998805336,11.1985433894428));
#58095=CARTESIAN_POINT('Ctrl Pts',(0.0921491958576946,71.1099725263237,
10.7355364493605));
#58096=CARTESIAN_POINT('Ctrl Pts',(1.64396370259509,71.3030831353856,11.2475534497753));
#58097=CARTESIAN_POINT('Ctrl Pts',(2.60363156558085,71.5070216091218,12.6835255182203));
#58098=CARTESIAN_POINT('Ctrl Pts',(2.47410443308142,71.7144050735568,14.434342871696));
#58099=CARTESIAN_POINT('Ctrl Pts',(1.27500325606336,71.9252579488303,15.7567695849295));
#58100=CARTESIAN_POINT('Ctrl Pts',(-0.512870675643372,72.1395798951614,
16.0660444961377));
#58101=CARTESIAN_POINT('Ctrl Pts',(-2.13839595577138,72.3573483133845,15.1961519408739));
#58102=CARTESIAN_POINT('Ctrl Pts',(-2.89569133798197,72.5785162363284,13.4832292970027));
#58103=CARTESIAN_POINT('Ctrl Pts',(-2.58704794005515,72.7281825608065,12.2549998685691));
#58104=CARTESIAN_POINT('Ctrl Pts',(-2.25606553638399,72.8035544420155,11.7498921642414));
#58105=CARTESIAN_POINT('Ctrl Pts',(-1.11234706696219,61.9237349740717,10.7800451030764));
#58106=CARTESIAN_POINT('Ctrl Pts',(-0.551984960934711,61.9995118664758,
10.5462115686574));
#58107=CARTESIAN_POINT('Ctrl Pts',(0.719238260214036,62.1500570476074,10.4674069972882));
#58108=CARTESIAN_POINT('Ctrl Pts',(2.27534796455583,62.3727400518901,11.5321674654256));
#58109=CARTESIAN_POINT('Ctrl Pts',(2.83869227102382,62.5922113005396,13.3027170540399));
#58110=CARTESIAN_POINT('Ctrl Pts',(2.2041406643837,62.8084116922911,15.0194479665355));
#58111=CARTESIAN_POINT('Ctrl Pts',(0.671656943323573,63.0213060081133,15.9687555157265));
#58112=CARTESIAN_POINT('Ctrl Pts',(-1.09261817887129,63.230880368071,15.7777026517318));
#58113=CARTESIAN_POINT('Ctrl Pts',(-2.3468926484301,63.4371437206783,14.5632979951621));
#58114=CARTESIAN_POINT('Ctrl Pts',(-2.57640944711034,63.6326088606432,12.9219357960667));
#58115=CARTESIAN_POINT('Ctrl Pts',(-1.96638287159801,63.7881145102524,11.7757850303583));
#58116=CARTESIAN_POINT('Ctrl Pts',(-0.829621454339106,63.9639615343511,
10.9121272646271));
#58117=CARTESIAN_POINT('Ctrl Pts',(0.948952924496643,64.1662398321294,10.8118735345015));
#58118=CARTESIAN_POINT('Ctrl Pts',(2.47201501163925,64.421003843011,12.4793626428307));
#58119=CARTESIAN_POINT('Ctrl Pts',(2.16429091661214,64.6707875557039,14.6621912912922));
#58120=CARTESIAN_POINT('Ctrl Pts',(0.310000895846759,64.9159648490878,15.7895918096977));
#58121=CARTESIAN_POINT('Ctrl Pts',(-1.70064237321371,65.1569453474805,15.0856079145018));
#58122=CARTESIAN_POINT('Ctrl Pts',(-2.42545733884156,65.394246323493,13.1176501165484));
#58123=CARTESIAN_POINT('Ctrl Pts',(-1.37865114244613,65.6283632635507,11.3285604610391));
#58124=CARTESIAN_POINT('Ctrl Pts',(0.641349738940361,65.8598663935718,11.0120162625725));
#58125=CARTESIAN_POINT('Ctrl Pts',(2.16088916276543,66.0893536994043,12.3544429084476));
#58126=CARTESIAN_POINT('Ctrl Pts',(2.0873493371532,66.3174469149352,14.3710586862541));
#58127=CARTESIAN_POINT('Ctrl Pts',(0.627394260415668,66.5258193195164,15.4887184567952));
#58128=CARTESIAN_POINT('Ctrl Pts',(-0.966952248386021,66.7151631539086,
15.2896494083299));
#58129=CARTESIAN_POINT('Ctrl Pts',(-1.99029443991551,66.8857762054556,14.2734563349868));
#58130=CARTESIAN_POINT('Ctrl Pts',(-2.17334990850197,67.0568641782707,12.8347205544376));
#58131=CARTESIAN_POINT('Ctrl Pts',(-1.42974172053206,67.2286966155006,11.5841402598853));
#58132=CARTESIAN_POINT('Ctrl Pts',(-0.0665580821207584,67.4015314694309,
11.0514665594181));
#58133=CARTESIAN_POINT('Ctrl Pts',(1.34605509662363,67.5756279545075,11.4733403642385));
#58134=CARTESIAN_POINT('Ctrl Pts',(2.20758999436957,67.7512359504503,12.6851069400924));
#58135=CARTESIAN_POINT('Ctrl Pts',(2.14077572797721,67.9285858629059,14.1853446214317));
#58136=CARTESIAN_POINT('Ctrl Pts',(1.15407911252636,68.1079089481521,15.339618743821));
#58137=CARTESIAN_POINT('Ctrl Pts',(-0.351727289097983,68.2894175197017,
15.6464719335678));
#58138=CARTESIAN_POINT('Ctrl Pts',(-1.74664366586638,68.473305005657,14.9526138915416));
#58139=CARTESIAN_POINT('Ctrl Pts',(-2.35125498867944,68.6390392779964,13.6868210389609));
#58140=CARTESIAN_POINT('Ctrl Pts',(-2.25257391000286,68.7491300895112,12.7873159965059));
#58141=CARTESIAN_POINT('Ctrl Pts',(-2.10495531904991,68.8018470807597,12.391385002815));
#58142=CARTESIAN_POINT('Ctrl Pts',(-2.03717175835508,68.8229602618792,12.2362787091018));
#58143=CARTESIAN_POINT('Ctrl Pts',(-1.89604486527342,68.8599781838076,11.9748525198571));
#58144=CARTESIAN_POINT('Ctrl Pts',(-1.52881357118424,68.9342928075108,11.5013498526747));
#58145=CARTESIAN_POINT('Ctrl Pts',(-0.794085685875897,69.0412663352442,
11.0197983059699));
#58146=CARTESIAN_POINT('Ctrl Pts',(0.0850065321694228,69.1493500227514,
10.8976306306484));
#58147=CARTESIAN_POINT('Ctrl Pts',(0.774475301734965,69.2365010454107,11.033827428284));
#58148=CARTESIAN_POINT('Ctrl Pts',(1.13804342964187,69.2857812179576,11.1939391739118));
#58149=CARTESIAN_POINT('Ctrl Pts',(1.36277942277332,69.3187442334309,11.3329370967313));
#58150=CARTESIAN_POINT('Ctrl Pts',(1.50755054814791,69.3407486541439,11.4337766328478));
#58151=CARTESIAN_POINT('Ctrl Pts',(1.74563217381336,69.3793327931068,11.6315473166949));
#58152=CARTESIAN_POINT('Ctrl Pts',(2.39204209314634,69.5010797157444,12.371157206559));
#58153=CARTESIAN_POINT('Ctrl Pts',(2.68537004139343,69.7029621444375,14.1276946542204));
#58154=CARTESIAN_POINT('Ctrl Pts',(1.08798299853103,69.9779620136592,15.9608354407845));
#58155=CARTESIAN_POINT('Ctrl Pts',(-1.39821458961621,70.258854973133,15.8819473431239));
#58156=CARTESIAN_POINT('Ctrl Pts',(-2.76464437090339,70.513781405731,14.0959696453757));
#58157=CARTESIAN_POINT('Ctrl Pts',(-2.60051720125486,70.7406191214659,12.2007578370582));
#58158=CARTESIAN_POINT('Ctrl Pts',(-1.57438150313715,70.9376043691068,10.9135292180737));
#58159=CARTESIAN_POINT('Ctrl Pts',(0.083710492335456,71.1454029061075,10.3825833010656));
#58160=CARTESIAN_POINT('Ctrl Pts',(1.84447942973013,71.3643206793081,10.9586311533899));
#58161=CARTESIAN_POINT('Ctrl Pts',(2.9322473004846,71.5946312759554,12.5777954928207));
#58162=CARTESIAN_POINT('Ctrl Pts',(2.79125106104368,71.8277863360761,14.5466512422041));
#58163=CARTESIAN_POINT('Ctrl Pts',(1.45333308887358,72.0636374859992,16.0290402831137));
#58164=CARTESIAN_POINT('Ctrl Pts',(-0.53452772748346,72.3020117956332,16.3775899567483));
#58165=CARTESIAN_POINT('Ctrl Pts',(-2.33363843540989,72.5427284022483,15.4200462674978));
#58166=CARTESIAN_POINT('Ctrl Pts',(-3.16951350766352,72.785585491095,13.5409680482108));
#58167=CARTESIAN_POINT('Ctrl Pts',(-2.83608351112003,72.9487744186263,12.2008932325256));
#58168=CARTESIAN_POINT('Ctrl Pts',(-2.47847683852305,73.0306494992593,11.6508904210054));
#58169=CARTESIAN_POINT('Ctrl Pts',(-1.05614180149106,62.1313437313199,11.0341707994449));
#58170=CARTESIAN_POINT('Ctrl Pts',(-0.548971891044798,62.2001434672158,
10.8178018517592));
#58171=CARTESIAN_POINT('Ctrl Pts',(0.600066002190081,62.3362615078341,10.7387345233335));
#58172=CARTESIAN_POINT('Ctrl Pts',(2.00317315352676,62.5360401344603,11.6840971984608));
#58173=CARTESIAN_POINT('Ctrl Pts',(2.51692770464562,62.7314955217158,13.2572898160531));
#58174=CARTESIAN_POINT('Ctrl Pts',(1.96780245778434,62.9227308654496,14.7805258955518));
#58175=CARTESIAN_POINT('Ctrl Pts',(0.627534290958144,63.1098787628258,15.6266079183967));
#58176=CARTESIAN_POINT('Ctrl Pts',(-0.916634533183098,63.2930983748755,
15.4733791869953));
#58177=CARTESIAN_POINT('Ctrl Pts',(-2.01817448198077,63.4725762148886,14.4267351420959));
#58178=CARTESIAN_POINT('Ctrl Pts',(-2.23118622297626,63.6420063293127,13.0057203001957));
#58179=CARTESIAN_POINT('Ctrl Pts',(-1.71404439365489,63.7764345811831,12.0092165993144));
#58180=CARTESIAN_POINT('Ctrl Pts',(-0.74040095074646,63.9282460800993,11.252892085331));
#58181=CARTESIAN_POINT('Ctrl Pts',(0.79246154237002,64.1026480660666,11.1498371368005));
#58182=CARTESIAN_POINT('Ctrl Pts',(2.12232177189969,64.3223016280321,12.5726403029094));
#58183=CARTESIAN_POINT('Ctrl Pts',(1.87924975497206,64.538140344765,14.4623939928372));
#58184=CARTESIAN_POINT('Ctrl Pts',(0.281941388394872,64.7509397878726,15.4615521829488));
#58185=CARTESIAN_POINT('Ctrl Pts',(-1.48334510265271,64.9614821048809,14.8694056336369));
#58186=CARTESIAN_POINT('Ctrl Pts',(-2.14579560937037,65.170675546169,13.14275520837));
#58187=CARTESIAN_POINT('Ctrl Pts',(-1.23447076475016,65.3793300522108,11.5349918992243));
#58188=CARTESIAN_POINT('Ctrl Pts',(0.586060913954109,65.5883274111427,11.2242451458131));
#58189=CARTESIAN_POINT('Ctrl Pts',(1.99496055385793,65.7985364388612,12.4354012615815));
#58190=CARTESIAN_POINT('Ctrl Pts',(1.9514703859804,66.0108085116655,14.3137593159358));
#58191=CARTESIAN_POINT('Ctrl Pts',(0.582788782174383,66.2080172868495,15.3893275183234));
#58192=CARTESIAN_POINT('Ctrl Pts',(-0.952216643940287,66.3899774952253,
15.2144528194188));
#58193=CARTESIAN_POINT('Ctrl Pts',(-1.95895364896274,66.5561211141707,14.2345532678041));
#58194=CARTESIAN_POINT('Ctrl Pts',(-2.15334180135745,66.7249463891927,12.8163011984208));
#58195=CARTESIAN_POINT('Ctrl Pts',(-1.42106113808395,66.8967377086185,11.5589046028338));
#58196=CARTESIAN_POINT('Ctrl Pts',(-0.0449424701988081,67.0717533123881,
11.0076192818134));
#58197=CARTESIAN_POINT('Ctrl Pts',(1.40709022978329,67.2502379613344,11.4286489188467));
#58198=CARTESIAN_POINT('Ctrl Pts',(2.31041726669693,67.4324112254196,12.6793658157442));
#58199=CARTESIAN_POINT('Ctrl Pts',(2.25122473446836,67.6184608146842,14.2540200585407));
#58200=CARTESIAN_POINT('Ctrl Pts',(1.21289277431689,67.8085581656143,15.4846144499685));
#58201=CARTESIAN_POINT('Ctrl Pts',(-0.397237124594922,68.0028427263292,
15.8226762133719));
#58202=CARTESIAN_POINT('Ctrl Pts',(-1.90795474026366,68.2014238494934,15.0814986913989));
#58203=CARTESIAN_POINT('Ctrl Pts',(-2.57306403335372,68.3818348176235,13.706679011662));
#58204=CARTESIAN_POINT('Ctrl Pts',(-2.4689738325603,68.5023850356115,12.7210998153131));
#58205=CARTESIAN_POINT('Ctrl Pts',(-2.30841188071509,68.5602532996293,12.2858853814415));
#58206=CARTESIAN_POINT('Ctrl Pts',(-2.23454348109542,68.5834418532569,12.1152622367379));
#58207=CARTESIAN_POINT('Ctrl Pts',(-2.08039211105857,68.6241300939167,11.8273603741192));
#58208=CARTESIAN_POINT('Ctrl Pts',(-1.67789433042616,68.705939653898,11.304672733353));
#58209=CARTESIAN_POINT('Ctrl Pts',(-0.868549129310337,68.8240482404245,
10.7700005027465));
#58210=CARTESIAN_POINT('Ctrl Pts',(0.105104625318163,68.943805202703,10.631256152897));
#58211=CARTESIAN_POINT('Ctrl Pts',(0.871362548059674,69.0405942263567,10.7801673750063));
#58212=CARTESIAN_POINT('Ctrl Pts',(1.27630982538946,69.0954061940594,10.9570404782022));
#58213=CARTESIAN_POINT('Ctrl Pts',(1.52694990464411,69.1320996779613,11.1110508382515));
#58214=CARTESIAN_POINT('Ctrl Pts',(1.68849723335025,69.1566026003853,11.222877621533));
#58215=CARTESIAN_POINT('Ctrl Pts',(1.95440299932936,69.1995894022695,11.442471208345));
#58216=CARTESIAN_POINT('Ctrl Pts',(2.67772396023776,69.335358778657,12.2651392784647));
#58217=CARTESIAN_POINT('Ctrl Pts',(3.01282469715482,69.5611529326277,14.2288138525143));
#58218=CARTESIAN_POINT('Ctrl Pts',(1.22684494953145,69.8697040031874,16.2915162347679));
#58219=CARTESIAN_POINT('Ctrl Pts',(-1.56816815705193,70.1854155149051,16.2104528621472));
#58220=CARTESIAN_POINT('Ctrl Pts',(-3.10949796001566,70.4720644229672,14.2057280182894));
#58221=CARTESIAN_POINT('Ctrl Pts',(-2.92987403517079,70.7269325979517,12.0757682763698));
#58222=CARTESIAN_POINT('Ctrl Pts',(-1.78137724519618,70.9480088576798,10.6285150467044));
#58223=CARTESIAN_POINT('Ctrl Pts',(0.0752717888132247,71.1808332858912,
10.0296301527708));
#58224=CARTESIAN_POINT('Ctrl Pts',(2.04499515686519,71.4255582232306,10.6697088570044));
#58225=CARTESIAN_POINT('Ctrl Pts',(3.26086303538833,71.6822409427889,12.4720654674214));
#58226=CARTESIAN_POINT('Ctrl Pts',(3.10839768900593,71.9411675985953,14.6589596127122));
#58227=CARTESIAN_POINT('Ctrl Pts',(1.63166292168379,72.2020170231681,16.3013109812979));
#58228=CARTESIAN_POINT('Ctrl Pts',(-0.55618477932355,72.4644436961051,16.6891354173588));
#58229=CARTESIAN_POINT('Ctrl Pts',(-2.5288809150484,72.7281084911122,15.6439405941217));
#58230=CARTESIAN_POINT('Ctrl Pts',(-3.44333567734506,72.9926547458617,13.5987067994188));
#58231=CARTESIAN_POINT('Ctrl Pts',(-3.08511908218492,73.1693662764461,12.1467865964821));
#58232=CARTESIAN_POINT('Ctrl Pts',(-2.70088814066211,73.2577445565031,11.5518886777693));
#58233=CARTESIAN_POINT('Ctrl Pts',(-1.05593533999082,62.1312800345432,11.0339552088038));
#58234=CARTESIAN_POINT('Ctrl Pts',(-0.548797894764382,62.2000722428305,
10.8176652497803));
#58235=CARTESIAN_POINT('Ctrl Pts',(0.600192035121667,62.3361862873998,10.7386582030159));
#58236=CARTESIAN_POINT('Ctrl Pts',(2.00329796012928,62.5359652527017,11.6840275306112));
#58237=CARTESIAN_POINT('Ctrl Pts',(2.51707525078404,62.7314316525048,13.2573106468538));
#58238=CARTESIAN_POINT('Ctrl Pts',(1.96791083140091,62.9226784440387,14.7806354540074));
#58239=CARTESIAN_POINT('Ctrl Pts',(0.627554523537033,63.1098381475148,15.6267648112371));
#58240=CARTESIAN_POINT('Ctrl Pts',(-0.916715231028849,63.2930698446158,
15.4735187354625));
#58241=CARTESIAN_POINT('Ctrl Pts',(-2.01832521671403,63.4725599672086,14.4267977634151));
#58242=CARTESIAN_POINT('Ctrl Pts',(-2.23134452615484,63.6420020200743,13.0056818805518));
#58243=CARTESIAN_POINT('Ctrl Pts',(-1.71416010424544,63.7764399370507,12.0091095585455));
#58244=CARTESIAN_POINT('Ctrl Pts',(-0.740441863084698,63.9282624575314,
11.2527358265671));
#58245=CARTESIAN_POINT('Ctrl Pts',(0.792533301977947,64.1026772262679,11.149682162544));
#58246=CARTESIAN_POINT('Ctrl Pts',(2.12248212481777,64.3223468882384,12.5725975301495));
#58247=CARTESIAN_POINT('Ctrl Pts',(1.8793804614795,64.5382011705544,14.4624856105072));
#58248=CARTESIAN_POINT('Ctrl Pts',(0.281954255168914,64.7510154606255,15.4617026065356));
#58249=CARTESIAN_POINT('Ctrl Pts',(-1.48344474498909,64.9615717351561,14.8695047738624));
#58250=CARTESIAN_POINT('Ctrl Pts',(-2.14592384912253,65.1707780652413,13.1427436963524));
#58251=CARTESIAN_POINT('Ctrl Pts',(-1.23453687910888,65.3794442471611,11.534897239449));
#58252=CARTESIAN_POINT('Ctrl Pts',(0.586086266816036,65.588451926184,11.2241478276014));
#58253=CARTESIAN_POINT('Ctrl Pts',(1.99503664093542,65.7986697940167,12.4353641378779));
#58254=CARTESIAN_POINT('Ctrl Pts',(1.95153269369428,66.010949121655,14.3137855907395));
#58255=CARTESIAN_POINT('Ctrl Pts',(0.582809236154573,66.2081630159558,15.389373094346));
#58256=CARTESIAN_POINT('Ctrl Pts',(-0.952223400997341,66.3901266101162,
15.2144873010475));
#58257=CARTESIAN_POINT('Ctrl Pts',(-1.95896802037949,66.5562722785337,14.234571106926));
#58258=CARTESIAN_POINT('Ctrl Pts',(-2.15335097613695,66.7250985911228,12.8163096446735));
#58259=CARTESIAN_POINT('Ctrl Pts',(-1.42106511859191,66.8968899294033,11.5589161747225));
#58260=CARTESIAN_POINT('Ctrl Pts',(-0.0449523821045983,67.0719045331833,
11.0076393881183));
#58261=CARTESIAN_POINT('Ctrl Pts',(1.40706224193395,67.2503871699235,11.4286694122474));
#58262=CARTESIAN_POINT('Ctrl Pts',(2.31037011493275,67.4325574234846,12.6793684483545));
#58263=CARTESIAN_POINT('Ctrl Pts',(2.25117408773437,67.6186030234855,14.2539885672063));
#58264=CARTESIAN_POINT('Ctrl Pts',(1.21286580513013,67.8086954338427,15.4845479617384));
#58265=CARTESIAN_POINT('Ctrl Pts',(-0.397216255918911,68.0029741360882,
15.8225954143537));
#58266=CARTESIAN_POINT('Ctrl Pts',(-1.90788077057091,68.2015485214395,15.0814395908748));
#58267=CARTESIAN_POINT('Ctrl Pts',(-2.4982095699917,68.3616759780349,13.8611890279));
#58268=CARTESIAN_POINT('Ctrl Pts',(-2.49283646883181,68.4555325144937,13.1030816010796));
#58269=CARTESIAN_POINT('Ctrl Pts',(-2.46701393303641,68.4808270900767,12.9018894245279));
#58270=CARTESIAN_POINT('Ctrl Pts',(0.247287541580098,77.6548572027072,10.0427241822324));
#58271=CARTESIAN_POINT('Ctrl Pts',(0.964069001324889,77.7445925079294,10.0979779665913));
#58272=CARTESIAN_POINT('Ctrl Pts',(2.35704967373067,77.9240000776253,10.7009273106633));
#58273=CARTESIAN_POINT('Ctrl Pts',(3.4467728248986,78.192503630638,12.6958819746852));
#58274=CARTESIAN_POINT('Ctrl Pts',(3.07923969920137,78.4600209528315,14.9304288566278));
#58275=CARTESIAN_POINT('Ctrl Pts',(1.42315265705318,78.7261651385104,16.4576833059984));
#58276=CARTESIAN_POINT('Ctrl Pts',(-0.806764227344182,78.9905667981157,
16.6425893403264));
#58277=CARTESIAN_POINT('Ctrl Pts',(-2.66532596956275,79.2528650228532,15.4237333446468));
#58278=CARTESIAN_POINT('Ctrl Pts',(-3.37042528836801,79.5127146681829,13.3446071043689));
#58279=CARTESIAN_POINT('Ctrl Pts',(-2.5847048075285,79.7983491753509,11.0520674671235));
#58280=CARTESIAN_POINT('Ctrl Pts',(-0.137666389072941,80.1081393123657,
9.82774503828806));
#58281=CARTESIAN_POINT('Ctrl Pts',(2.53491771752001,80.439918590107,11.0372481405381));
#58282=CARTESIAN_POINT('Ctrl Pts',(3.0843688080165,80.6768938598906,13.0523003042481));
#58283=CARTESIAN_POINT('Ctrl Pts',(2.70076310244372,80.863947802345,14.5066703222784));
#58284=CARTESIAN_POINT('Ctrl Pts',(1.97786813303724,81.0228941830997,15.6027318765835));
#58285=CARTESIAN_POINT('Ctrl Pts',(0.302161778549171,81.2380000656201,16.3168978017426));
#58286=CARTESIAN_POINT('Ctrl Pts',(-1.58085531198438,81.4682050832055,15.8160551896125));
#58287=CARTESIAN_POINT('Ctrl Pts',(-2.73467581966542,81.6938241351438,14.2940760892576));
#58288=CARTESIAN_POINT('Ctrl Pts',(-2.70879358569799,81.914758094417,12.4242532818977));
#58289=CARTESIAN_POINT('Ctrl Pts',(-1.5638821754899,82.1309391180892,10.9962972897096));
#58290=CARTESIAN_POINT('Ctrl Pts',(-0.112332637144442,82.3070995697092,
10.65403698097));
#58291=CARTESIAN_POINT('Ctrl Pts',(0.971767836276392,82.4456316622513,10.9480842940185));
#58292=CARTESIAN_POINT('Ctrl Pts',(2.05531843922359,82.6053950292879,11.669616155466));
#58293=CARTESIAN_POINT('Ctrl Pts',(2.58022303152249,82.772929767339,13.0429223676538));
#58294=CARTESIAN_POINT('Ctrl Pts',(2.10894229679348,82.9692944639935,14.5905689471349));
#58295=CARTESIAN_POINT('Ctrl Pts',(1.03068522636296,83.1404274052572,15.5507677597493));
#58296=CARTESIAN_POINT('Ctrl Pts',(-0.560032659422088,83.3284650308457,
15.6518101151826));
#58297=CARTESIAN_POINT('Ctrl Pts',(-1.8447489750784,83.512170284916,14.772879306662));
#58298=CARTESIAN_POINT('Ctrl Pts',(-2.25261977308136,83.6717741940494,13.489840670357));
#58299=CARTESIAN_POINT('Ctrl Pts',(-1.91138106357061,83.8480453771256,12.0775888075753));
#58300=CARTESIAN_POINT('Ctrl Pts',(-0.72049864066441,84.0205323353866,11.1412811543025));
#58301=CARTESIAN_POINT('Ctrl Pts',(0.862171558101919,84.2077261938883,11.3140639157902));
#58302=CARTESIAN_POINT('Ctrl Pts',(1.8664262479419,84.3730421625329,12.283684323027));
#58303=CARTESIAN_POINT('Ctrl Pts',(2.06128816907136,84.5355159613324,13.6464327914842));
#58304=CARTESIAN_POINT('Ctrl Pts',(1.38720207749988,84.6954633805368,14.8205992727919));
#58305=CARTESIAN_POINT('Ctrl Pts',(0.151211699798348,84.8532298820947,15.326232344394));
#58306=CARTESIAN_POINT('Ctrl Pts',(-1.11958576901327,85.009179694123,14.9693938082164));
#58307=CARTESIAN_POINT('Ctrl Pts',(-1.89575588946321,85.1636728011368,13.9162459886775));
#58308=CARTESIAN_POINT('Ctrl Pts',(-1.86375037275616,85.3000452442271,12.7629372015215));
#58309=CARTESIAN_POINT('Ctrl Pts',(-1.4047981936709,85.4019466736085,12.062882842335));
#58310=CARTESIAN_POINT('Ctrl Pts',(-0.973350991123209,85.4697837447249,
11.7271521694353));
#58311=CARTESIAN_POINT('Ctrl Pts',(-0.479131804993002,85.5375812762284,
11.4936252857917));
#58312=CARTESIAN_POINT('Ctrl Pts',(0.212066650498646,85.6222764554439,11.4174503611125));
#58313=CARTESIAN_POINT('Ctrl Pts',(1.00124737159773,85.723955620617,11.6892758599415));
#58314=CARTESIAN_POINT('Ctrl Pts',(1.50026311536417,85.8088213091389,12.1762090409978));
#58315=CARTESIAN_POINT('Ctrl Pts',(1.74529030119219,85.8768560281014,12.6664088610162));
#58316=CARTESIAN_POINT('Ctrl Pts',(1.94992832551134,85.979067489764,13.4654738216233));
#58317=CARTESIAN_POINT('Ctrl Pts',(1.54155537527295,86.133122989655,14.7611755398965));
#58318=CARTESIAN_POINT('Ctrl Pts',(-0.161706220391905,86.3409986454679,
15.4503179358885));
#58319=CARTESIAN_POINT('Ctrl Pts',(-1.80233989822033,86.552223249788,14.554166040512));
#58320=CARTESIAN_POINT('Ctrl Pts',(-2.11499875684585,86.7436966602518,12.8951618407757));
#58321=CARTESIAN_POINT('Ctrl Pts',(-1.36195053022674,86.9144564975112,11.6765763097194));
#58322=CARTESIAN_POINT('Ctrl Pts',(-0.232848814881847,87.0632468330563,
11.1571740292811));
#58323=CARTESIAN_POINT('Ctrl Pts',(1.07249419248516,87.2209790231122,11.363039966774));
#58324=CARTESIAN_POINT('Ctrl Pts',(2.07652075315406,87.3882686374323,12.3607198540593));
#58325=CARTESIAN_POINT('Ctrl Pts',(2.26531128235019,87.5658187484789,13.8523567274988));
#58326=CARTESIAN_POINT('Ctrl Pts',(1.47889922862541,87.7474173482421,15.1732495990815));
#58327=CARTESIAN_POINT('Ctrl Pts',(0.0127680510151906,87.9332577758032,
15.7439964436861));
#58328=CARTESIAN_POINT('Ctrl Pts',(-1.52981989797465,88.1235131031462,15.2808950263592));
#58329=CARTESIAN_POINT('Ctrl Pts',(-2.48339938369146,88.3183210263946,13.9353972421663));
#58330=CARTESIAN_POINT('Ctrl Pts',(-2.40474239046522,88.5177875734279,12.2482339471135));
#58331=CARTESIAN_POINT('Ctrl Pts',(-1.65476716887248,88.6539234702229,11.3740678808263));
#58332=CARTESIAN_POINT('Ctrl Pts',(-1.17773130173033,88.7227885365479,11.0968781559722));
#58333=CARTESIAN_POINT('Ctrl Pts',(0.184803675495247,77.862472667449,10.2953881670292));
#58334=CARTESIAN_POINT('Ctrl Pts',(0.846167896041115,77.9452305174071,10.3426706699363));
#58335=CARTESIAN_POINT('Ctrl Pts',(2.12976813845044,78.1102104375581,10.8911235114185));
#58336=CARTESIAN_POINT('Ctrl Pts',(3.13541597804943,78.3558092526022,12.7111536714507));
#58337=CARTESIAN_POINT('Ctrl Pts',(2.81105501535664,78.599309525502,14.7468282838804));
#58338=CARTESIAN_POINT('Ctrl Pts',(1.3174660878423,78.8404879419078,16.1386573044603));
#58339=CARTESIAN_POINT('Ctrl Pts',(-0.694485932762879,79.079142259978,16.3163710055547));
#58340=CARTESIAN_POINT('Ctrl Pts',(-2.37242298386509,79.3150850725898,15.229252877698));
#58341=CARTESIAN_POINT('Ctrl Pts',(-3.01564346814379,79.5481480850051,13.3680196060162));
#58342=CARTESIAN_POINT('Ctrl Pts',(-2.32463299882677,79.8037412444127,11.3123399690757));
#58343=CARTESIAN_POINT('Ctrl Pts',(-0.145960813747356,80.0803886369846,
10.2058035594949));
#58344=CARTESIAN_POINT('Ctrl Pts',(2.2448406691886,80.376321418116,11.2692709379055));
#58345=CARTESIAN_POINT('Ctrl Pts',(2.74720689877205,80.5877004008594,13.0633520002669));
#58346=CARTESIAN_POINT('Ctrl Pts',(2.41359112629158,80.754675913076,14.3640425134037));
#58347=CARTESIAN_POINT('Ctrl Pts',(1.77467578964236,80.8966446736528,15.3475444027645));
#58348=CARTESIAN_POINT('Ctrl Pts',(0.280266482960803,81.089066666713,15.9972992631639));
#58349=CARTESIAN_POINT('Ctrl Pts',(-1.41186855660018,81.2955160386158,15.5607616424528));
#58350=CARTESIAN_POINT('Ctrl Pts',(-2.46067898716311,81.498529477346,14.199207170258));
#58351=CARTESIAN_POINT('Ctrl Pts',(-2.45065374611866,81.698160141879,12.5094141597136));
#58352=CARTESIAN_POINT('Ctrl Pts',(-1.42141928360188,81.8944830257032,11.2041161942034));
#58353=CARTESIAN_POINT('Ctrl Pts',(-0.0978562227218405,82.0554116780197,
10.8803746487815));
#58354=CARTESIAN_POINT('Ctrl Pts',(0.89975624661569,82.1826084511176,11.1429047439257));
#58355=CARTESIAN_POINT('Ctrl Pts',(1.90330680638142,82.329832284588,11.8000378769176));
#58356=CARTESIAN_POINT('Ctrl Pts',(2.40255550468052,82.4853171492715,13.0701031156741));
#58357=CARTESIAN_POINT('Ctrl Pts',(1.97314920561762,82.6691658414288,14.5229682427947));
#58358=CARTESIAN_POINT('Ctrl Pts',(0.963543218920492,82.8306537998472,15.4380219300933));
#58359=CARTESIAN_POINT('Ctrl Pts',(-0.551987846154585,83.0099144809128,
15.548159807256));
#58360=CARTESIAN_POINT('Ctrl Pts',(-1.79825228513438,83.1869738653656,14.7122634879005));
#58361=CARTESIAN_POINT('Ctrl Pts',(-2.20715491105176,83.3426053314291,13.4645232622311));
#58362=CARTESIAN_POINT('Ctrl Pts',(-1.88252472097578,83.5162453863774,12.0706692194223));
#58363=CARTESIAN_POINT('Ctrl Pts',(-0.704083095511786,83.6883202304834,
11.1243417314447));
#58364=CARTESIAN_POINT('Ctrl Pts',(0.900949647343497,83.8779374958976,11.2844042859749));
#58365=CARTESIAN_POINT('Ctrl Pts',(1.94079100521003,84.0476417923649,12.2709767567351));
#58366=CARTESIAN_POINT('Ctrl Pts',(2.15586901925411,84.2166812486924,13.6870647569731));
#58367=CARTESIAN_POINT('Ctrl Pts',(1.45555116861922,84.3853283298918,14.9313227792802));
#58368=CARTESIAN_POINT('Ctrl Pts',(0.139421890731178,84.5538699300146,15.482377466424));
#58369=CARTESIAN_POINT('Ctrl Pts',(-1.23870833428518,84.7225961199578,15.1071712083794));
#58370=CARTESIAN_POINT('Ctrl Pts',(-2.09762284605641,84.8917831351255,13.960184736452));
#58371=CARTESIAN_POINT('Ctrl Pts',(-2.0714028319448,85.0428328228877,12.6823062984053));
#58372=CARTESIAN_POINT('Ctrl Pts',(-1.56323576511282,85.1566891462768,11.8968515809312));
#58373=CARTESIAN_POINT('Ctrl Pts',(-1.08076080089141,85.2328581275125,11.5172616832284));
#58374=CARTESIAN_POINT('Ctrl Pts',(-0.525465502422548,85.3092207324986,
11.2512630571995));
#58375=CARTESIAN_POINT('Ctrl Pts',(0.256192788495037,85.4050520677571,11.160632154595));
#58376=CARTESIAN_POINT('Ctrl Pts',(1.15585653050521,85.5207387464336,11.4649965691636));
#58377=CARTESIAN_POINT('Ctrl Pts',(1.72949109010161,85.6177796698734,12.0187932605256));
#58378=CARTESIAN_POINT('Ctrl Pts',(2.01332360175128,85.6958323950965,12.5799038605807));
#58379=CARTESIAN_POINT('Ctrl Pts',(2.25306236695033,85.8133417315253,13.497370825771));
#58380=CARTESIAN_POINT('Ctrl Pts',(1.7900960149886,85.9913056754938,14.9971579306732));
#58381=CARTESIAN_POINT('Ctrl Pts',(-0.184091351432346,86.2327348191477,
15.8082302617226));
#58382=CARTESIAN_POINT('Ctrl Pts',(-2.10043413195707,86.4787852330779,14.7729907970524));
#58383=CARTESIAN_POINT('Ctrl Pts',(-2.47275342454578,86.7019769498762,12.8404470847727));
#58384=CARTESIAN_POINT('Ctrl Pts',(-1.60144586883462,86.9007689105388,11.4183199337594));
#58385=CARTESIAN_POINT('Ctrl Pts',(-0.291719036302049,87.0736507381159,
10.8098947257727));
#58386=CARTESIAN_POINT('Ctrl Pts',(1.22174090202642,87.2564100022132,11.043035987828));
#58387=CARTESIAN_POINT('Ctrl Pts',(2.38453426877103,87.4495072117008,12.1908837927305));
#58388=CARTESIAN_POINT('Ctrl Pts',(2.60676095777434,87.6534314516664,13.9035461000159));
#58389=CARTESIAN_POINT('Ctrl Pts',(1.7132379478211,87.8608015674409,15.4147166578918));
#58390=CARTESIAN_POINT('Ctrl Pts',(0.0516842488560093,88.0716411492593,
16.0671514745576));
#58391=CARTESIAN_POINT('Ctrl Pts',(-1.68754739984842,88.2859506018957,15.5504356901444));
#58392=CARTESIAN_POINT('Ctrl Pts',(-2.75775208799366,88.503706693754,14.0493169297074));
#58393=CARTESIAN_POINT('Ctrl Pts',(-2.67572823382123,88.7248631301323,12.1783780710712));
#58394=CARTESIAN_POINT('Ctrl Pts',(-1.85388558078155,88.8745225725434,11.2150008714402));
#58395=CARTESIAN_POINT('Ctrl Pts',(-1.3330573230966,88.949891053716,10.9094060841414));
#58396=CARTESIAN_POINT('Ctrl Pts',(0.122319809410396,78.0700881321905,10.548052151826));
#58397=CARTESIAN_POINT('Ctrl Pts',(0.728266790757343,78.1458685268846,10.5873633732813));
#58398=CARTESIAN_POINT('Ctrl Pts',(1.90248660317024,78.2964207974908,11.0813197121736));
#58399=CARTESIAN_POINT('Ctrl Pts',(2.82405913120026,78.5191148745665,12.7264253682162));
#58400=CARTESIAN_POINT('Ctrl Pts',(2.54287033151193,78.7385980981725,14.5632277111332));
#58401=CARTESIAN_POINT('Ctrl Pts',(1.21177951863141,78.9548107453053,15.8196313029222));
#58402=CARTESIAN_POINT('Ctrl Pts',(-0.582207638181581,79.16771772184,15.990152670783));
#58403=CARTESIAN_POINT('Ctrl Pts',(-2.07951999816744,79.3773051223264,15.0347724107492));
#58404=CARTESIAN_POINT('Ctrl Pts',(-2.66086164791958,79.5835815018273,13.3914321076634));
#58405=CARTESIAN_POINT('Ctrl Pts',(-2.06456119012503,79.8091333134742,11.5726124710281));
#58406=CARTESIAN_POINT('Ctrl Pts',(-0.154255238421772,80.0526379616033,
10.5838620807018));
#58407=CARTESIAN_POINT('Ctrl Pts',(1.95476362085717,80.312724246125,11.501293735273));
#58408=CARTESIAN_POINT('Ctrl Pts',(2.41004498952759,80.4985069418283,13.074403696286));
#58409=CARTESIAN_POINT('Ctrl Pts',(2.12641915013944,80.6454040238068,14.2214147045289));
#58410=CARTESIAN_POINT('Ctrl Pts',(1.57148344624747,80.7703951642059,15.0923569289456));
#58411=CARTESIAN_POINT('Ctrl Pts',(0.258371187372433,80.9401332678059,15.677700724585));
#58412=CARTESIAN_POINT('Ctrl Pts',(-1.24288180121598,81.1228269940261,15.3054680952933));
#58413=CARTESIAN_POINT('Ctrl Pts',(-2.1866821546608,81.3032348195481,14.1043382512586));
#58414=CARTESIAN_POINT('Ctrl Pts',(-2.19251390653934,81.4815621893412,12.5945750375294));
#58415=CARTESIAN_POINT('Ctrl Pts',(-1.27895639171386,81.6580269333169,11.4119350986974));
#58416=CARTESIAN_POINT('Ctrl Pts',(-0.0833798082992409,81.8037237863302,
11.1067123165931));
#58417=CARTESIAN_POINT('Ctrl Pts',(0.827744656954988,81.9195852399837,11.3377251938329));
#58418=CARTESIAN_POINT('Ctrl Pts',(1.75129517353926,82.0542695398883,11.9304595983692));
#58419=CARTESIAN_POINT('Ctrl Pts',(2.22488797783857,82.197704531204,13.0972838636943));
#58420=CARTESIAN_POINT('Ctrl Pts',(1.83735611444177,82.3690372188642,14.4553675384547));
#58421=CARTESIAN_POINT('Ctrl Pts',(0.896401211478014,82.5208801944373,15.3252761004372));
#58422=CARTESIAN_POINT('Ctrl Pts',(-0.543943032887081,82.6913639309801,
15.4445094993294));
#58423=CARTESIAN_POINT('Ctrl Pts',(-1.75175559519037,82.8617774458153,14.6516476691391));
#58424=CARTESIAN_POINT('Ctrl Pts',(-2.16169004902218,83.0134364688086,13.4392058541051));
#58425=CARTESIAN_POINT('Ctrl Pts',(-1.85366837838093,83.1844453956293,12.0637496312695));
#58426=CARTESIAN_POINT('Ctrl Pts',(-0.687667550359165,83.3561081255805,
11.1074023085868));
#58427=CARTESIAN_POINT('Ctrl Pts',(0.939727736585077,83.5481487979069,11.2547446561599));
#58428=CARTESIAN_POINT('Ctrl Pts',(2.01515576247816,83.7222414221968,12.258269190443));
#58429=CARTESIAN_POINT('Ctrl Pts',(2.25044986943687,83.8978465360525,13.7276967224621));
#58430=CARTESIAN_POINT('Ctrl Pts',(1.52390025973857,84.0751932792468,15.0420462857686));
#58431=CARTESIAN_POINT('Ctrl Pts',(0.127632081664017,84.2545099779345,15.638522588454));
#58432=CARTESIAN_POINT('Ctrl Pts',(-1.35783089955709,84.4360125457928,15.2449486085422));
#58433=CARTESIAN_POINT('Ctrl Pts',(-2.29948980264962,84.619893469114,14.0041234842265));
#58434=CARTESIAN_POINT('Ctrl Pts',(-2.27905529113342,84.7856204015483,12.6016753952892));
#58435=CARTESIAN_POINT('Ctrl Pts',(-1.72167333655474,84.9114316189451,11.7308203195274));
#58436=CARTESIAN_POINT('Ctrl Pts',(-1.18817061065961,84.9959325103001,11.3073711970217));
#58437=CARTESIAN_POINT('Ctrl Pts',(-0.571799199852085,85.0808601887689,
11.0089008286074));
#58438=CARTESIAN_POINT('Ctrl Pts',(0.300318926491433,85.1878276800704,10.9038139480775));
#58439=CARTESIAN_POINT('Ctrl Pts',(1.31046568941269,85.3175218722502,11.2407172783856));
#58440=CARTESIAN_POINT('Ctrl Pts',(1.95871906483905,85.4267380306077,11.8613774800535));
#58441=CARTESIAN_POINT('Ctrl Pts',(2.28135690231037,85.5148087620915,12.4933988601451));
#58442=CARTESIAN_POINT('Ctrl Pts',(2.55619640838934,85.6476159732867,13.5292678299187));
#58443=CARTESIAN_POINT('Ctrl Pts',(2.03863665470422,85.8494883613327,15.2331403214501));
#58444=CARTESIAN_POINT('Ctrl Pts',(-0.206476482472782,86.1244709928276,
16.1661425875569));
#58445=CARTESIAN_POINT('Ctrl Pts',(-2.39852836569383,86.4053472163679,14.9918155535928));
#58446=CARTESIAN_POINT('Ctrl Pts',(-2.8305080922457,86.6602572395007,12.7857323287695));
#58447=CARTESIAN_POINT('Ctrl Pts',(-1.8409412074425,86.8870813235665,11.1600635577994));
#58448=CARTESIAN_POINT('Ctrl Pts',(-0.350589257722249,87.0840546431753,
10.4626154222644));
#58449=CARTESIAN_POINT('Ctrl Pts',(1.37098761156767,87.2918409813142,10.723032008882));
#58450=CARTESIAN_POINT('Ctrl Pts',(2.692547784388,87.5107457859693,12.0210477314016));
#58451=CARTESIAN_POINT('Ctrl Pts',(2.94821063319851,87.741044154854,13.9547354725332));
#58452=CARTESIAN_POINT('Ctrl Pts',(1.94757666701682,87.9741857866397,15.6561837167021));
#58453=CARTESIAN_POINT('Ctrl Pts',(0.0906004466968272,88.2100245227155,
16.3903065054292));
#58454=CARTESIAN_POINT('Ctrl Pts',(-1.84527490172218,88.4483881006452,15.8199763539294));
#58455=CARTESIAN_POINT('Ctrl Pts',(-3.03210479229587,88.6890923611134,14.1632366172487));
#58456=CARTESIAN_POINT('Ctrl Pts',(-2.94671407717725,88.9319386868365,12.1085221950291));
#58457=CARTESIAN_POINT('Ctrl Pts',(-2.05300399269063,89.0951216748638,11.055933862054));
#58458=CARTESIAN_POINT('Ctrl Pts',(-1.48838334446287,89.1769935708843,10.7219340123104));
#58459=CARTESIAN_POINT('Ctrl Pts',(0.0598359433255453,78.2777035969321,
10.8007161366229));
#58460=CARTESIAN_POINT('Ctrl Pts',(0.61036568547357,78.3465065363623,10.8320560766263));
#58461=CARTESIAN_POINT('Ctrl Pts',(1.67520506789003,78.4826311574234,11.2715159129288));
#58462=CARTESIAN_POINT('Ctrl Pts',(2.51270228435107,78.6824204965308,12.7416970649818));
#58463=CARTESIAN_POINT('Ctrl Pts',(2.2746856476672,78.877886670843,14.3796271383859));
#58464=CARTESIAN_POINT('Ctrl Pts',(1.10609294942053,79.0691335487028,15.5006053013841));
#58465=CARTESIAN_POINT('Ctrl Pts',(-0.46992934360028,79.256293183702,15.6639343360112));
#58466=CARTESIAN_POINT('Ctrl Pts',(-1.78661701246979,79.439525172063,14.8402919438003));
#58467=CARTESIAN_POINT('Ctrl Pts',(-2.30607982769537,79.6190149186495,13.4148446093108));
#58468=CARTESIAN_POINT('Ctrl Pts',(-1.80448938142329,79.8145253825358,11.8328849729804));
#58469=CARTESIAN_POINT('Ctrl Pts',(-0.162549663096186,80.024887286222,10.9619206019087));
#58470=CARTESIAN_POINT('Ctrl Pts',(1.66468657252576,80.2491270741339,11.7333165326405));
#58471=CARTESIAN_POINT('Ctrl Pts',(2.07288308028313,80.4093134827971,13.0854553923048));
#58472=CARTESIAN_POINT('Ctrl Pts',(1.83924717398731,80.5361321345376,14.0787868956542));
#58473=CARTESIAN_POINT('Ctrl Pts',(1.36829110285259,80.6441456547589,14.8371694551268));
#58474=CARTESIAN_POINT('Ctrl Pts',(0.236475891784066,80.7911998688987,15.3581021860063));
#58475=CARTESIAN_POINT('Ctrl Pts',(-1.07389504583177,80.9501379494364,15.0501745481337));
#58476=CARTESIAN_POINT('Ctrl Pts',(-1.91268532215848,81.1079401617502,14.009469332259));
#58477=CARTESIAN_POINT('Ctrl Pts',(-1.93437406696,81.2649642368032,12.6797359153453));
#58478=CARTESIAN_POINT('Ctrl Pts',(-1.13649349982583,81.4215708409309,11.6197540031912));
#58479=CARTESIAN_POINT('Ctrl Pts',(-0.0689033938766367,81.5520358946408,
11.3330499844046));
#58480=CARTESIAN_POINT('Ctrl Pts',(0.755733067294288,81.6565620288498,11.53254564374));
#58481=CARTESIAN_POINT('Ctrl Pts',(1.59928354069709,81.7787067951883,12.0608813198208));
#58482=CARTESIAN_POINT('Ctrl Pts',(2.04722045099659,81.9100919131365,13.1244646117146));
#58483=CARTESIAN_POINT('Ctrl Pts',(1.70156302326592,82.0689085962994,14.3877668341146));
#58484=CARTESIAN_POINT('Ctrl Pts',(0.82925920403554,82.2111065890273,15.2125302707812));
#58485=CARTESIAN_POINT('Ctrl Pts',(-0.53589821961958,82.3728133810471,15.3408591914028));
#58486=CARTESIAN_POINT('Ctrl Pts',(-1.70525890524636,82.536581026265,14.5910318503777));
#58487=CARTESIAN_POINT('Ctrl Pts',(-2.11622518699259,82.6842676061882,13.4138884459793));
#58488=CARTESIAN_POINT('Ctrl Pts',(-1.8248120357861,82.8526454048811,12.0568300431165));
#58489=CARTESIAN_POINT('Ctrl Pts',(-0.67125200520654,83.0238960206773,11.0904628857288));
#58490=CARTESIAN_POINT('Ctrl Pts',(0.978505825826656,83.2183600999162,11.2250850263446));
#58491=CARTESIAN_POINT('Ctrl Pts',(2.0895205197463,83.3968410520288,12.245561624151));
#58492=CARTESIAN_POINT('Ctrl Pts',(2.34503071961963,83.5790118234125,13.768328687951));
#58493=CARTESIAN_POINT('Ctrl Pts',(1.59224935085791,83.7650582286018,15.1527697922569));
#58494=CARTESIAN_POINT('Ctrl Pts',(0.115842272596848,83.9551500258546,15.7946677104839));
#58495=CARTESIAN_POINT('Ctrl Pts',(-1.47695346482901,84.1494289716277,15.3827260087051));
#58496=CARTESIAN_POINT('Ctrl Pts',(-2.50135675924282,84.3480038031027,14.0480622320009));
#58497=CARTESIAN_POINT('Ctrl Pts',(-2.48670775032206,84.528407980209,12.5210444921729));
#58498=CARTESIAN_POINT('Ctrl Pts',(-1.88011090799667,84.6661740916134,11.5647890581236));
#58499=CARTESIAN_POINT('Ctrl Pts',(-1.29558042042781,84.7590068930878,11.0974807108149));
#58500=CARTESIAN_POINT('Ctrl Pts',(-0.618132897281633,84.8524996450391,
10.7665386000152));
#58501=CARTESIAN_POINT('Ctrl Pts',(0.344445064487824,84.9706032923835,10.6469957415602));
#58502=CARTESIAN_POINT('Ctrl Pts',(1.46507484832016,85.1143049980667,11.0164379876078));
#58503=CARTESIAN_POINT('Ctrl Pts',(2.18794703957648,85.2356963913422,11.7039616995813));
#58504=CARTESIAN_POINT('Ctrl Pts',(2.54939020286947,85.3337851290867,12.4068938597097));
#58505=CARTESIAN_POINT('Ctrl Pts',(2.85933044982833,85.481890215048,13.5611648340663));
#58506=CARTESIAN_POINT('Ctrl Pts',(2.28717729441986,85.7076710471716,15.4691227122269));
#58507=CARTESIAN_POINT('Ctrl Pts',(-0.228861613513224,86.0162071665075,
16.5240549133912));
#58508=CARTESIAN_POINT('Ctrl Pts',(-2.69662259943057,86.3319091996579,15.2106403101332));
#58509=CARTESIAN_POINT('Ctrl Pts',(-3.18826275994563,86.6185375291251,12.7310175727665));
#58510=CARTESIAN_POINT('Ctrl Pts',(-2.08043654605037,86.8733937365941,10.9018071818394));
#58511=CARTESIAN_POINT('Ctrl Pts',(-0.409459479142451,87.0944585482347,
10.115336118756));
#58512=CARTESIAN_POINT('Ctrl Pts',(1.52023432110892,87.3272719604151,10.403028029936));
#58513=CARTESIAN_POINT('Ctrl Pts',(3.00056130000496,87.5719843602378,11.8512116700728));
#58514=CARTESIAN_POINT('Ctrl Pts',(3.28966030862267,87.8286568580416,14.0059248450504));
#58515=CARTESIAN_POINT('Ctrl Pts',(2.18191538621251,88.0875700058385,15.8976507755124));
#58516=CARTESIAN_POINT('Ctrl Pts',(0.129516644537648,88.3484078961716,16.7134615363008));
#58517=CARTESIAN_POINT('Ctrl Pts',(-2.00300240359594,88.6108255993947,16.0895170177145));
#58518=CARTESIAN_POINT('Ctrl Pts',(-3.30645749659806,88.8744780284728,14.2771563047898));
#58519=CARTESIAN_POINT('Ctrl Pts',(-3.21769992053326,89.1390142435408,12.038666318987));
#58520=CARTESIAN_POINT('Ctrl Pts',(-2.2521224045997,89.3157207771843,10.896866852668));
#58521=CARTESIAN_POINT('Ctrl Pts',(-1.64370936582915,89.4040960880525,10.5344619404795));
#58522=CARTESIAN_POINT('Ctrl Pts',(0.0622069118415443,78.2779999202659,
10.8008522795397));
#58523=CARTESIAN_POINT('Ctrl Pts',(0.611894146152642,78.3467019602469,10.8326872595339));
#58524=CARTESIAN_POINT('Ctrl Pts',(1.67560584825159,78.4827267656738,11.2722194612178));
#58525=CARTESIAN_POINT('Ctrl Pts',(2.51270228435107,78.6824204965308,12.7416970649818));
#58526=CARTESIAN_POINT('Ctrl Pts',(2.2746856476672,78.877886670843,14.3796271383859));
#58527=CARTESIAN_POINT('Ctrl Pts',(1.10609294942053,79.0691335487028,15.5006053013841));
#58528=CARTESIAN_POINT('Ctrl Pts',(-0.46992934360028,79.256293183702,15.6639343360112));
#58529=CARTESIAN_POINT('Ctrl Pts',(-1.78661701246979,79.439525172063,14.8402919438003));
#58530=CARTESIAN_POINT('Ctrl Pts',(-2.30607982769537,79.6190149186495,13.4148446093108));
#58531=CARTESIAN_POINT('Ctrl Pts',(-1.80448938142329,79.8145253825358,11.8328849729804));
#58532=CARTESIAN_POINT('Ctrl Pts',(-0.162549663096186,80.024887286222,10.9619206019087));
#58533=CARTESIAN_POINT('Ctrl Pts',(1.66468657252576,80.2491270741339,11.7333165326405));
#58534=CARTESIAN_POINT('Ctrl Pts',(2.07288308028313,80.4093134827971,13.0854553923048));
#58535=CARTESIAN_POINT('Ctrl Pts',(1.83924717398731,80.5361321345376,14.0787868956542));
#58536=CARTESIAN_POINT('Ctrl Pts',(1.36829110285259,80.6441456547589,14.8371694551268));
#58537=CARTESIAN_POINT('Ctrl Pts',(0.236475891784066,80.7911998688987,15.3581021860063));
#58538=CARTESIAN_POINT('Ctrl Pts',(-1.07389504583177,80.9501379494364,15.0501745481337));
#58539=CARTESIAN_POINT('Ctrl Pts',(-1.91268532215848,81.1079401617502,14.009469332259));
#58540=CARTESIAN_POINT('Ctrl Pts',(-1.93437406696,81.2649642368032,12.6797359153453));
#58541=CARTESIAN_POINT('Ctrl Pts',(-1.13649349982583,81.4215708409309,11.6197540031912));
#58542=CARTESIAN_POINT('Ctrl Pts',(-0.0689033938766367,81.5520358946408,
11.3330499844046));
#58543=CARTESIAN_POINT('Ctrl Pts',(0.755733067294288,81.6565620288498,11.53254564374));
#58544=CARTESIAN_POINT('Ctrl Pts',(1.59928354069709,81.7787067951883,12.0608813198208));
#58545=CARTESIAN_POINT('Ctrl Pts',(2.04722045099659,81.9100919131365,13.1244646117146));
#58546=CARTESIAN_POINT('Ctrl Pts',(1.70156302326592,82.0689085962994,14.3877668341146));
#58547=CARTESIAN_POINT('Ctrl Pts',(0.82925920403554,82.2111065890273,15.2125302707812));
#58548=CARTESIAN_POINT('Ctrl Pts',(-0.53589821961958,82.3728133810471,15.3408591914028));
#58549=CARTESIAN_POINT('Ctrl Pts',(-1.70525890524636,82.536581026265,14.5910318503777));
#58550=CARTESIAN_POINT('Ctrl Pts',(-2.11622518699259,82.6842676061882,13.4138884459793));
#58551=CARTESIAN_POINT('Ctrl Pts',(-1.8248120357861,82.8526454048811,12.0568300431165));
#58552=CARTESIAN_POINT('Ctrl Pts',(-0.67125200520654,83.0238960206773,11.0904628857288));
#58553=CARTESIAN_POINT('Ctrl Pts',(0.978505825826656,83.2183600999162,11.2250850263446));
#58554=CARTESIAN_POINT('Ctrl Pts',(2.0895205197463,83.3968410520288,12.245561624151));
#58555=CARTESIAN_POINT('Ctrl Pts',(2.34503071961963,83.5790118234125,13.768328687951));
#58556=CARTESIAN_POINT('Ctrl Pts',(1.59224935085791,83.7650582286018,15.1527697922569));
#58557=CARTESIAN_POINT('Ctrl Pts',(0.115842272596848,83.9551500258546,15.7946677104839));
#58558=CARTESIAN_POINT('Ctrl Pts',(-1.47695346482901,84.1494289716277,15.3827260087051));
#58559=CARTESIAN_POINT('Ctrl Pts',(-2.50135675924282,84.3480038031027,14.0480622320009));
#58560=CARTESIAN_POINT('Ctrl Pts',(-2.48835484466458,84.5081238298553,12.6927381742385));
#58561=CARTESIAN_POINT('Ctrl Pts',(-2.14702439884612,84.6019727171383,12.01597911337));
#58562=CARTESIAN_POINT('Ctrl Pts',(-2.03459967169508,84.6272597203354,11.8472323735682));
#58563=CARTESIAN_POINT('Ctrl Pts',(1.62567980018093,93.7945759308532,10.4657523090101));
#58564=CARTESIAN_POINT('Ctrl Pts',(2.26361473188923,93.8863901894122,10.832065737273));
#58565=CARTESIAN_POINT('Ctrl Pts',(3.2658443372097,94.0678999317249,12.0003103131008));
#58566=CARTESIAN_POINT('Ctrl Pts',(3.35691835987926,94.338517066757,14.2896228282011));
#58567=CARTESIAN_POINT('Ctrl Pts',(2.03466811379621,94.6061000245314,16.1290171211605));
#58568=CARTESIAN_POINT('Ctrl Pts',(-0.127985735322314,94.8723118052565,
16.7623211593336));
#58569=CARTESIAN_POINT('Ctrl Pts',(-2.20934172455679,95.1367830226765,15.9374225661859));
#58570=CARTESIAN_POINT('Ctrl Pts',(-3.33304091563268,95.3991528151441,14.0199424862732));
#58571=CARTESIAN_POINT('Ctrl Pts',(-3.04384750747191,95.6590737429842,11.8424470121058));
#58572=CARTESIAN_POINT('Ctrl Pts',(-1.3167115394671,95.9447928973861,10.1387096135308));
#58573=CARTESIAN_POINT('Ctrl Pts',(0.914025025367711,96.1983215575206,10.1341696855316));
#58574=CARTESIAN_POINT('Ctrl Pts',(2.35325644232377,96.4206034690197,11.259890544272));
#58575=CARTESIAN_POINT('Ctrl Pts',(3.1822047885405,96.640723635659,12.8669508643349));
#58576=CARTESIAN_POINT('Ctrl Pts',(2.72392992072032,96.911636589393,15.2118032510287));
#58577=CARTESIAN_POINT('Ctrl Pts',(0.249363689211224,97.2294224043132,16.5493006915505));
#58578=CARTESIAN_POINT('Ctrl Pts',(-2.28232071173272,97.5394610680848,15.4944322266632));
#58579=CARTESIAN_POINT('Ctrl Pts',(-2.9911795578159,97.8162518841324,13.1596802537136));
#58580=CARTESIAN_POINT('Ctrl Pts',(-2.03593613645396,98.0617968089958,11.3100136953354));
#58581=CARTESIAN_POINT('Ctrl Pts',(-0.378017756006219,98.278031770538,10.5386546999244));
#58582=CARTESIAN_POINT('Ctrl Pts',(1.36543463028554,98.4894735789785,10.9445531049755));
#58583=CARTESIAN_POINT('Ctrl Pts',(2.46579833874375,98.696118620997,12.3037545886731));
#58584=CARTESIAN_POINT('Ctrl Pts',(2.49752216123743,98.8979956906054,14.0123482012642));
#58585=CARTESIAN_POINT('Ctrl Pts',(1.49556695346512,99.0951648208613,15.3473452032655));
#58586=CARTESIAN_POINT('Ctrl Pts',(-0.077661314976231,99.2877179951242,
15.7740783614512));
#58587=CARTESIAN_POINT('Ctrl Pts',(-1.54584306935538,99.4757795604173,15.1581600696454));
#58588=CARTESIAN_POINT('Ctrl Pts',(-2.30721550472451,99.6595021625455,13.8018948294568));
#58589=CARTESIAN_POINT('Ctrl Pts',(-2.0792914703476,99.8390693946257,12.2989815972528));
#58590=CARTESIAN_POINT('Ctrl Pts',(-1.0000027499426,100.014689084747,11.2767295564262));
#58591=CARTESIAN_POINT('Ctrl Pts',(0.448470956356669,100.18660318479,11.1369560862804));
#58592=CARTESIAN_POINT('Ctrl Pts',(1.6519323745928,100.355071356998,11.9015096877094));
#58593=CARTESIAN_POINT('Ctrl Pts',(2.12414762484912,100.520379107224,13.2186356429174));
#58594=CARTESIAN_POINT('Ctrl Pts',(1.69158115151593,100.682831846705,14.5246426040201));
#58595=CARTESIAN_POINT('Ctrl Pts',(0.567850360925065,100.842758317436,15.2777758714163));
#58596=CARTESIAN_POINT('Ctrl Pts',(-0.766897362161647,101.000495068412,
15.1812500512025));
#58597=CARTESIAN_POINT('Ctrl Pts',(-1.63301226775241,101.139083491954,14.3962551082184));
#58598=CARTESIAN_POINT('Ctrl Pts',(-1.99790763286353,101.29378375243,13.1740789195566));
#58599=CARTESIAN_POINT('Ctrl Pts',(-1.50166663647508,101.447270514397,11.9203648333942));
#58600=CARTESIAN_POINT('Ctrl Pts',(-0.183210996391025,101.616923102518,
11.3342112094097));
#58601=CARTESIAN_POINT('Ctrl Pts',(1.06606422218322,101.769308904291,11.6402003542304));
#58602=CARTESIAN_POINT('Ctrl Pts',(1.86759638968297,101.921786212033,12.6534070722283));
#58603=CARTESIAN_POINT('Ctrl Pts',(1.87476424258217,102.07475394688,13.94808787474));
#58604=CARTESIAN_POINT('Ctrl Pts',(1.08122962577802,102.228598071457,14.9803147482856));
#58605=CARTESIAN_POINT('Ctrl Pts',(-0.191662859422608,102.383699978547,
15.3087123354403));
#58606=CARTESIAN_POINT('Ctrl Pts',(-1.40653911672816,102.54044013001,14.7803154183345));
#58607=CARTESIAN_POINT('Ctrl Pts',(-2.12819221058885,102.71681720939,13.4692876035973));
#58608=CARTESIAN_POINT('Ctrl Pts',(-1.65992697799525,102.914185604843,11.7906537263468));
#58609=CARTESIAN_POINT('Ctrl Pts',(0.125034229719186,103.134459810349,11.0065966617667));
#58610=CARTESIAN_POINT('Ctrl Pts',(1.75438201985768,103.341615287336,11.8326420188669));
#58611=CARTESIAN_POINT('Ctrl Pts',(2.27797020089514,103.534559255831,13.3831006340595));
#58612=CARTESIAN_POINT('Ctrl Pts',(1.78571770818503,103.712037241146,14.8005586192802));
#58613=CARTESIAN_POINT('Ctrl Pts',(0.494270562277235,103.893566032069,15.6353564465742));
#58614=CARTESIAN_POINT('Ctrl Pts',(-1.07234386693872,104.079339269911,15.4951771393443));
#58615=CARTESIAN_POINT('Ctrl Pts',(-2.24884450357346,104.269528147654,14.3956742992569));
#58616=CARTESIAN_POINT('Ctrl Pts',(-2.50597583289488,104.464274125644,12.7669262238946));
#58617=CARTESIAN_POINT('Ctrl Pts',(-1.68681015579904,104.663681949589,11.2904932986803));
#58618=CARTESIAN_POINT('Ctrl Pts',(-0.627211848440459,104.799780780842,
10.840195813604));
#58619=CARTESIAN_POINT('Ctrl Pts',(-0.0768417822340009,104.868628219523,
10.8036689183428));
#58620=CARTESIAN_POINT('Ctrl Pts',(1.46045405682495,94.0029659022257,10.6668376125859));
#58621=CARTESIAN_POINT('Ctrl Pts',(2.0507217959542,94.0876436018886,11.001428431865));
#58622=CARTESIAN_POINT('Ctrl Pts',(2.97733933924797,94.2545490062617,12.0713852943386));
#58623=CARTESIAN_POINT('Ctrl Pts',(3.070789585288,94.5020541295736,14.1648644902778));
#58624=CARTESIAN_POINT('Ctrl Pts',(1.87574246782933,94.7455856884425,15.8450121964185));
#58625=CARTESIAN_POINT('Ctrl Pts',(-0.0808875490336731,94.9867962122503,
16.4290464283818));
#58626=CARTESIAN_POINT('Ctrl Pts',(-1.96339697661919,95.2254836409508,15.6946328486544));
#58627=CARTESIAN_POINT('Ctrl Pts',(-2.98369333070791,95.4614604001256,13.9756265091926));
#58628=CARTESIAN_POINT('Ctrl Pts',(-2.73559538172536,95.6945574625247,12.0212543429719));
#58629=CARTESIAN_POINT('Ctrl Pts',(-1.19933236447556,95.9501904660232,10.4877100732131));
#58630=CARTESIAN_POINT('Ctrl Pts',(0.792576929541223,96.1765696942838,10.4715620063823));
#58631=CARTESIAN_POINT('Ctrl Pts',(2.0830646340336,96.3748674559486,11.4675188239778));
#58632=CARTESIAN_POINT('Ctrl Pts',(2.83180362082271,96.571179582596,12.8959840254328));
#58633=CARTESIAN_POINT('Ctrl Pts',(2.43734837739185,96.8127941299477,14.9900696749655));
#58634=CARTESIAN_POINT('Ctrl Pts',(0.236241808260255,97.0965847023887,16.2004855511167));
#58635=CARTESIAN_POINT('Ctrl Pts',(-2.0380656366222,97.3741979176357,15.2734889467748));
#58636=CARTESIAN_POINT('Ctrl Pts',(-2.69244372297225,97.6230498986325,13.1794400922548));
#58637=CARTESIAN_POINT('Ctrl Pts',(-1.84270351097513,97.8448918272664,11.5013006210743));
#58638=CARTESIAN_POINT('Ctrl Pts',(-0.342863154852027,98.0412412451055,
10.788621893397));
#58639=CARTESIAN_POINT('Ctrl Pts',(1.2528646694032,98.2343783206733,11.1461289618806));
#58640=CARTESIAN_POINT('Ctrl Pts',(2.2755495541587,98.4244231979741,12.3875957155746));
#58641=CARTESIAN_POINT('Ctrl Pts',(2.31869670558774,98.6115172489426,13.9709051527683));
#58642=CARTESIAN_POINT('Ctrl Pts',(1.39309287730542,98.7958183772439,15.2271343783831));
#58643=CARTESIAN_POINT('Ctrl Pts',(-0.0878663793999987,98.9775060287232,
15.6431191081459));
#58644=CARTESIAN_POINT('Ctrl Pts',(-1.4928633284236,99.1567779325714,15.0686219996598));
#58645=CARTESIAN_POINT('Ctrl Pts',(-2.23865523362967,99.33384542954,13.7680710682018));
#58646=CARTESIAN_POINT('Ctrl Pts',(-2.02981918752864,99.5089370971803,12.3004509925281));
#58647=CARTESIAN_POINT('Ctrl Pts',(-0.973603534998877,99.6822906696519,
11.2815431673196));
#58648=CARTESIAN_POINT('Ctrl Pts',(0.473392355753049,99.8541637345571,11.1286001848778));
#58649=CARTESIAN_POINT('Ctrl Pts',(1.6995472292461,100.024815758553,11.8921649619359));
#58650=CARTESIAN_POINT('Ctrl Pts',(2.19633062747038,100.194517842491,13.2400455689458));
#58651=CARTESIAN_POINT('Ctrl Pts',(1.7580296324876,100.363545819897,14.6030409780728));
#58652=CARTESIAN_POINT('Ctrl Pts',(0.579731615323981,100.532184012228,15.4072839311937));
#58653=CARTESIAN_POINT('Ctrl Pts',(-0.847450930810139,100.700711000255,
15.3160247299797));
#58654=CARTESIAN_POINT('Ctrl Pts',(-1.79134987561612,100.850673253478,14.4736763066588));
#58655=CARTESIAN_POINT('Ctrl Pts',(-2.19937715193843,101.019766916766,13.1405706996597));
#58656=CARTESIAN_POINT('Ctrl Pts',(-1.66218454769459,101.189504468116,11.7493907868574));
#58657=CARTESIAN_POINT('Ctrl Pts',(-0.190544567415407,101.379427278415,
11.0823963921818));
#58658=CARTESIAN_POINT('Ctrl Pts',(1.22377517797031,101.551642707134,11.4192058409893));
#58659=CARTESIAN_POINT('Ctrl Pts',(2.14439907420247,101.725403514285,12.5682324039414));
#58660=CARTESIAN_POINT('Ctrl Pts',(2.16126111529323,101.900962890033,14.0542982782834));
#58661=CARTESIAN_POINT('Ctrl Pts',(1.25160786092212,102.078556211253,15.2509714585909));
#58662=CARTESIAN_POINT('Ctrl Pts',(-0.222627569799362,102.258406121726,
15.639321465208));
#58663=CARTESIAN_POINT('Ctrl Pts',(-1.63877585618237,102.440724413414,15.0313321790294));
#58664=CARTESIAN_POINT('Ctrl Pts',(-2.48666797944368,102.646253989519,13.5072005727598));
#58665=CARTESIAN_POINT('Ctrl Pts',(-1.94851042751775,102.876377989224,11.5474888158579));
#58666=CARTESIAN_POINT('Ctrl Pts',(0.126561907913205,103.132819912367,10.6273830725664));
#58667=CARTESIAN_POINT('Ctrl Pts',(2.01968962832455,103.373117655503,11.5798462181864));
#58668=CARTESIAN_POINT('Ctrl Pts',(2.63002557592199,103.595883122873,13.368059706764));
#58669=CARTESIAN_POINT('Ctrl Pts',(2.06965165021159,103.799773192147,14.9983479377696));
#58670=CARTESIAN_POINT('Ctrl Pts',(0.597346362413307,104.007110012382,15.9563763703115));
#58671=CARTESIAN_POINT('Ctrl Pts',(-1.1809445934538,104.217917207411,15.8025070400524));
#58672=CARTESIAN_POINT('Ctrl Pts',(-2.51010932623597,104.432195681752,14.5674651013056));
#58673=CARTESIAN_POINT('Ctrl Pts',(-2.80272521150328,104.649922000431,12.7471845670932));
#58674=CARTESIAN_POINT('Ctrl Pts',(-1.89885716503994,104.871050085879,11.1073396892158));
#58675=CARTESIAN_POINT('Ctrl Pts',(-0.735145083543213,105.020692283243,
10.6089271762419));
#58676=CARTESIAN_POINT('Ctrl Pts',(-0.132850003595063,105.096052450379,
10.566386044137));
#58677=CARTESIAN_POINT('Ctrl Pts',(1.29522831346895,94.2113558735981,10.8679229161619));
#58678=CARTESIAN_POINT('Ctrl Pts',(1.83782886001918,94.2888970143649,11.1707911264571));
#58679=CARTESIAN_POINT('Ctrl Pts',(2.68883434128623,94.4411980807984,12.1424602755765));
#58680=CARTESIAN_POINT('Ctrl Pts',(2.78466081069676,94.6655911923902,14.0401061523546));
#58681=CARTESIAN_POINT('Ctrl Pts',(1.71681682186247,94.8850713523536,15.5610072716766));
#58682=CARTESIAN_POINT('Ctrl Pts',(-0.0337893627450391,95.101280619244,
16.0957716974301));
#58683=CARTESIAN_POINT('Ctrl Pts',(-1.71745222868159,95.3141842592252,15.4518431311229));
#58684=CARTESIAN_POINT('Ctrl Pts',(-2.63434574578315,95.5237679851071,13.931310532112));
#58685=CARTESIAN_POINT('Ctrl Pts',(-2.42734325597883,95.7300411820652,12.2000616738379));
#58686=CARTESIAN_POINT('Ctrl Pts',(-1.08195318948404,95.9555880346603,10.8367105328952));
#58687=CARTESIAN_POINT('Ctrl Pts',(0.671128833714733,96.1548178310472,10.8089543272328));
#58688=CARTESIAN_POINT('Ctrl Pts',(1.81287282574344,96.3291314428775,11.6751471036834));
#58689=CARTESIAN_POINT('Ctrl Pts',(2.48140245310491,96.501635529533,12.9250171865306));
#58690=CARTESIAN_POINT('Ctrl Pts',(2.15076683406338,96.7139516705026,14.7683360989023));
#58691=CARTESIAN_POINT('Ctrl Pts',(0.223119927309282,96.9637470004642,15.8516704106827));
#58692=CARTESIAN_POINT('Ctrl Pts',(-1.7938105615117,97.2089347671866,15.0525456668865));
#58693=CARTESIAN_POINT('Ctrl Pts',(-2.39370788812863,97.4298479131326,13.1991999307961));
#58694=CARTESIAN_POINT('Ctrl Pts',(-1.64947088549632,97.627986845537,11.692587546813));
#58695=CARTESIAN_POINT('Ctrl Pts',(-0.307708553697835,97.8044507196731,
11.0385890868694));
#58696=CARTESIAN_POINT('Ctrl Pts',(1.14029470852087,97.9792830623682,11.3477048187857));
#58697=CARTESIAN_POINT('Ctrl Pts',(2.08530076957367,98.1527277749512,12.4714368424759));
#58698=CARTESIAN_POINT('Ctrl Pts',(2.13987124993805,98.3250388072801,13.9294621042721));
#58699=CARTESIAN_POINT('Ctrl Pts',(1.29061880114571,98.4964719336266,15.1069235535006));
#58700=CARTESIAN_POINT('Ctrl Pts',(-0.0980714438237656,98.6672940623222,
15.5121598548408));
#58701=CARTESIAN_POINT('Ctrl Pts',(-1.43988358749184,98.8377763047257,14.9790839296742));
#58702=CARTESIAN_POINT('Ctrl Pts',(-2.17009496253482,99.0081886965343,13.7342473069468));
#58703=CARTESIAN_POINT('Ctrl Pts',(-1.98034690470969,99.178804799735,12.3019203878032));
#58704=CARTESIAN_POINT('Ctrl Pts',(-0.947204320055155,99.3498922545572,
11.2863567782128));
#58705=CARTESIAN_POINT('Ctrl Pts',(0.498313755149421,99.5217242843239,11.1202442834754));
#58706=CARTESIAN_POINT('Ctrl Pts',(1.74716208389938,99.6945601601093,11.8828202361623));
#58707=CARTESIAN_POINT('Ctrl Pts',(2.26851363009162,99.8686565777578,13.261455494974));
#58708=CARTESIAN_POINT('Ctrl Pts',(1.82447811345925,100.04425979309,14.6814393521253));
#58709=CARTESIAN_POINT('Ctrl Pts',(0.591612869722885,100.221609707021,15.5367919909709));
#58710=CARTESIAN_POINT('Ctrl Pts',(-0.928004499458635,100.400926932099,
15.4507994087571));
#58711=CARTESIAN_POINT('Ctrl Pts',(-1.94968748347984,100.562263015001,14.5510975050992));
#58712=CARTESIAN_POINT('Ctrl Pts',(-2.40084667101332,100.745750081104,13.1070624797628));
#58713=CARTESIAN_POINT('Ctrl Pts',(-1.82270245891412,100.931738421836,11.5784167403206));
#58714=CARTESIAN_POINT('Ctrl Pts',(-0.197878138439787,101.141931454312,
10.830581574954));
#58715=CARTESIAN_POINT('Ctrl Pts',(1.38148613375741,101.333976509975,11.1982113277482));
#58716=CARTESIAN_POINT('Ctrl Pts',(2.42120175872198,101.529020816538,12.4830577356546));
#58717=CARTESIAN_POINT('Ctrl Pts',(2.44775798800427,101.727171833185,14.1605086818266));
#58718=CARTESIAN_POINT('Ctrl Pts',(1.42198609606622,101.928514351047,15.5216281688963));
#58719=CARTESIAN_POINT('Ctrl Pts',(-0.253592280176116,102.133112264904,
15.9699305949757));
#58720=CARTESIAN_POINT('Ctrl Pts',(-1.87101259563657,102.34100869682,15.2823489397244));
#58721=CARTESIAN_POINT('Ctrl Pts',(-2.84514374829853,102.575690769647,13.5451135419222));
#58722=CARTESIAN_POINT('Ctrl Pts',(-2.23709387704024,102.838570373607,11.304323905369));
#58723=CARTESIAN_POINT('Ctrl Pts',(0.128089586107228,103.131180014383,10.248169483366));
#58724=CARTESIAN_POINT('Ctrl Pts',(2.28499723679145,103.404620023671,11.3270504175059));
#58725=CARTESIAN_POINT('Ctrl Pts',(2.98208095094885,103.657206989915,13.3530187794686));
#58726=CARTESIAN_POINT('Ctrl Pts',(2.35358559223816,103.887509143148,15.196137256259));
#58727=CARTESIAN_POINT('Ctrl Pts',(0.700422162549388,104.120653992695,16.2773962940487));
#58728=CARTESIAN_POINT('Ctrl Pts',(-1.28954531996889,104.35649514491,16.1098369407604));
#58729=CARTESIAN_POINT('Ctrl Pts',(-2.77137414889849,104.594863215849,14.7392559033545));
#58730=CARTESIAN_POINT('Ctrl Pts',(-3.09947459011168,104.835569875216,12.7274429102918));
#58731=CARTESIAN_POINT('Ctrl Pts',(-2.11090417428086,105.078418222169,10.924186079751));
#58732=CARTESIAN_POINT('Ctrl Pts',(-0.843078318645966,105.241603785644,
10.3776585388797));
#58733=CARTESIAN_POINT('Ctrl Pts',(-0.188858224956125,105.323476681233,
10.3291031699311));
#58734=CARTESIAN_POINT('Ctrl Pts',(1.13000257011297,94.4197458449706,11.0690082197377));
#58735=CARTESIAN_POINT('Ctrl Pts',(1.62493592408414,94.4901504268412,11.3401538210491));
#58736=CARTESIAN_POINT('Ctrl Pts',(2.40032934332449,94.6278471553352,12.2135352568143));
#58737=CARTESIAN_POINT('Ctrl Pts',(2.49853203610551,94.8291282552068,13.9153478144313));
#58738=CARTESIAN_POINT('Ctrl Pts',(1.5578911758956,95.0245570162647,15.2770023469347));
#58739=CARTESIAN_POINT('Ctrl Pts',(0.0133088235436025,95.2157650262378,
15.7624969664783));
#58740=CARTESIAN_POINT('Ctrl Pts',(-1.47150748074399,95.4028848774996,15.2090534135915));
#58741=CARTESIAN_POINT('Ctrl Pts',(-2.28499816085838,95.5860755700886,13.8869945550315));
#58742=CARTESIAN_POINT('Ctrl Pts',(-2.11909113023227,95.7655249016057,12.3788690047039));
#58743=CARTESIAN_POINT('Ctrl Pts',(-0.964574014492501,95.9609856032976,
11.1857109925774));
#58744=CARTESIAN_POINT('Ctrl Pts',(0.549680737888245,96.1330659678105,11.1463466480834));
#58745=CARTESIAN_POINT('Ctrl Pts',(1.54268101745328,96.2833954298063,11.8827753833891));
#58746=CARTESIAN_POINT('Ctrl Pts',(2.13100128538712,96.43209147647,12.9540503476284));
#58747=CARTESIAN_POINT('Ctrl Pts',(1.86418529073491,96.6151092110574,14.5466025228392));
#58748=CARTESIAN_POINT('Ctrl Pts',(0.209998046358312,96.8309092985398,15.5028552702488));
#58749=CARTESIAN_POINT('Ctrl Pts',(-1.54955548640118,97.0436716167375,14.8316023869983));
#58750=CARTESIAN_POINT('Ctrl Pts',(-2.094972053285,97.2366459276328,13.2189597693372));
#58751=CARTESIAN_POINT('Ctrl Pts',(-1.45623826001751,97.4110818638077,11.8838744725519));
#58752=CARTESIAN_POINT('Ctrl Pts',(-0.272553952543648,97.5676601942407,
11.288556280342));
#58753=CARTESIAN_POINT('Ctrl Pts',(1.02772474763855,97.7241878040629,11.5492806756908));
#58754=CARTESIAN_POINT('Ctrl Pts',(1.89505198498861,97.8810323519284,12.5552779693774));
#58755=CARTESIAN_POINT('Ctrl Pts',(1.96104579428837,98.0385603656175,13.8880190557761));
#58756=CARTESIAN_POINT('Ctrl Pts',(1.18814472498599,98.1971254900092,14.9867127286182));
#58757=CARTESIAN_POINT('Ctrl Pts',(-0.108276508247538,98.3570820959213,
15.3812006015355));
#58758=CARTESIAN_POINT('Ctrl Pts',(-1.38690384656006,98.5187746768799,14.8895458596885));
#58759=CARTESIAN_POINT('Ctrl Pts',(-2.10153469143998,98.6825319635287,13.7004235456917));
#58760=CARTESIAN_POINT('Ctrl Pts',(-1.93087462189074,98.8486725022897,12.3033897830785));
#58761=CARTESIAN_POINT('Ctrl Pts',(-0.920805105111431,99.0174938394624,
11.291170389106));
#58762=CARTESIAN_POINT('Ctrl Pts',(0.523235154545799,99.1892848340907,11.1118883820729));
#58763=CARTESIAN_POINT('Ctrl Pts',(1.79477693855267,99.3643045616654,11.8734755103888));
#58764=CARTESIAN_POINT('Ctrl Pts',(2.34069663271289,99.542795313025,13.2828654210023));
#58765=CARTESIAN_POINT('Ctrl Pts',(1.89092659443093,99.7249737662826,14.759837726178));
#58766=CARTESIAN_POINT('Ctrl Pts',(0.603494124121801,99.9110354018131,15.6663000507482));
#58767=CARTESIAN_POINT('Ctrl Pts',(-1.00855806810713,100.101142863942,15.5855740875344));
#58768=CARTESIAN_POINT('Ctrl Pts',(-2.10802509134356,100.273852776525,14.6285187035397));
#58769=CARTESIAN_POINT('Ctrl Pts',(-2.60231619008822,100.47173324544,13.0735542598658));
#58770=CARTESIAN_POINT('Ctrl Pts',(-1.98322037013363,100.673972375556,11.4074426937837));
#58771=CARTESIAN_POINT('Ctrl Pts',(-0.20521170946417,100.904435630209,10.5787667577262));
#58772=CARTESIAN_POINT('Ctrl Pts',(1.5391970895445,101.116310312817,10.9772168145072));
#58773=CARTESIAN_POINT('Ctrl Pts',(2.6980044432415,101.332638118791,12.3978830673678));
#58774=CARTESIAN_POINT('Ctrl Pts',(2.73425486071532,101.553380776338,14.2667190853701));
#58775=CARTESIAN_POINT('Ctrl Pts',(1.59236433121031,101.778472490843,15.7922848792018));
#58776=CARTESIAN_POINT('Ctrl Pts',(-0.284556990552873,102.007818408081,
16.3005397247434));
#58777=CARTESIAN_POINT('Ctrl Pts',(-2.10324933509078,102.241292980224,15.5333657004193));
#58778=CARTESIAN_POINT('Ctrl Pts',(-3.20361951715336,102.505127549775,13.5830265110847));
#58779=CARTESIAN_POINT('Ctrl Pts',(-2.52567732656274,102.800762757988,11.0611589948802));
#58780=CARTESIAN_POINT('Ctrl Pts',(0.129617264301245,103.1295401164,9.86895589416567));
#58781=CARTESIAN_POINT('Ctrl Pts',(2.55030484525832,103.436122391839,11.0742546168255));
#58782=CARTESIAN_POINT('Ctrl Pts',(3.33413632597569,103.718530856956,13.3379778521731));
#58783=CARTESIAN_POINT('Ctrl Pts',(2.63751953426473,103.975245094149,15.3939265747484));
#58784=CARTESIAN_POINT('Ctrl Pts',(0.80349796268546,104.234197973009,16.5984162177859));
#58785=CARTESIAN_POINT('Ctrl Pts',(-1.39814604648398,104.495073082409,16.4171668414684));
#58786=CARTESIAN_POINT('Ctrl Pts',(-3.03263897156099,104.757530749947,14.9110467054031));
#58787=CARTESIAN_POINT('Ctrl Pts',(-3.39622396872007,105.021217750003,12.7077012534903));
#58788=CARTESIAN_POINT('Ctrl Pts',(-2.32295118352176,105.285786358458,10.7410324702864));
#58789=CARTESIAN_POINT('Ctrl Pts',(-0.95101155374872,105.462515288045,10.1463899015177));
#58790=CARTESIAN_POINT('Ctrl Pts',(-0.244866446317187,105.550900912088,
10.0918202957253));
#58791=CARTESIAN_POINT('Ctrl Pts',(1.16384208806484,94.4245814674342,11.0879031093561));
#58792=CARTESIAN_POINT('Ctrl Pts',(1.23813215647139,94.4352463283717,11.1301721956053));
#58793=CARTESIAN_POINT('Ctrl Pts',(1.31008885895312,94.4457986760407,11.1762110026006));
#58794=CARTESIAN_POINT('Ctrl Pts',(1.37937803304691,94.4563120296253,11.2257287620783));
#58795=CARTESIAN_POINT('Ctrl Pts',(1.47675945485785,94.4710878634184,11.295322748237));
#58796=CARTESIAN_POINT('Ctrl Pts',(1.56873439650927,94.4859593709836,11.3719505355548));
#58797=CARTESIAN_POINT('Ctrl Pts',(1.65461838219203,94.5008636490935,11.4545758551863));
#58798=CARTESIAN_POINT('Ctrl Pts',(1.69880566651519,94.5085318956151,11.4970865568244));
#58799=CARTESIAN_POINT('Ctrl Pts',(1.74138093416847,94.516208907082,11.5411856574171));
#58800=CARTESIAN_POINT('Ctrl Pts',(1.78225213749528,94.523886700208,11.5867372413334));
#58801=CARTESIAN_POINT('Ctrl Pts',(1.87499141089662,94.5413080848963,11.6900965860755));
#58802=CARTESIAN_POINT('Ctrl Pts',(1.95901578318207,94.5586789124716,11.800897393771));
#58803=CARTESIAN_POINT('Ctrl Pts',(2.03310732138691,94.5759505358216,11.9175028031254));
#58804=CARTESIAN_POINT('Ctrl Pts',(2.05408670808245,94.5808410816775,11.9505202033969));
#58805=CARTESIAN_POINT('Ctrl Pts',(2.07427003233056,94.5857237047095,11.9840029970195));
#58806=CARTESIAN_POINT('Ctrl Pts',(2.09363039773066,94.5905973746505,12.0179141059386));
#58807=CARTESIAN_POINT('Ctrl Pts',(2.13785525671972,94.6017302929322,12.0953772105399));
#58808=CARTESIAN_POINT('Ctrl Pts',(2.17774383806482,94.6128420071046,12.1750806358068));
#58809=CARTESIAN_POINT('Ctrl Pts',(2.21305797123479,94.6238554462755,12.2565231937073));
#58810=CARTESIAN_POINT('Ctrl Pts',(2.21806675245765,94.6254175377773,12.2680746015471));
#58811=CARTESIAN_POINT('Ctrl Pts',(2.22298357177946,94.626977661633,12.279661053157));
#58812=CARTESIAN_POINT('Ctrl Pts',(2.22780781029263,94.6285356072505,12.291281177885));
#58813=CARTESIAN_POINT('Ctrl Pts',(2.22781672452381,94.6285384860235,12.2913026495593));
#58814=CARTESIAN_POINT('Ctrl Pts',(2.22782563843889,94.628541364789,12.2913241213486));
#58815=CARTESIAN_POINT('Ctrl Pts',(2.22783455203788,94.6285442435471,12.2913455932529));
#58816=CARTESIAN_POINT('Ctrl Pts',(2.25606866780065,94.6376628037731,12.3593585509574));
#58817=CARTESIAN_POINT('Ctrl Pts',(2.28116408671351,94.646702650814,12.4285673202461));
#58818=CARTESIAN_POINT('Ctrl Pts',(2.3029763109095,94.6557602078268,12.498685150674));
#58819=CARTESIAN_POINT('Ctrl Pts',(2.3069888938594,94.657426438584,12.5115840466477));
#58820=CARTESIAN_POINT('Ctrl Pts',(2.31089034671451,94.6590932511501,12.5245135672308));
#58821=CARTESIAN_POINT('Ctrl Pts',(2.31467974696626,94.6607612220338,12.5374717373018));
#58822=CARTESIAN_POINT('Ctrl Pts',(2.34630435602342,94.6746813475441,12.6456147244154));
#58823=CARTESIAN_POINT('Ctrl Pts',(2.37012813215105,94.6886884184708,12.7557741957835));
#58824=CARTESIAN_POINT('Ctrl Pts',(2.38624240054443,94.7027315140537,12.8668639407928));
#58825=CARTESIAN_POINT('Ctrl Pts',(2.39057752180477,94.7065094405929,12.8967497229854));
#58826=CARTESIAN_POINT('Ctrl Pts',(2.39435456023409,94.7102900039376,12.92670309968));
#58827=CARTESIAN_POINT('Ctrl Pts',(2.39757499657033,94.7140722783207,12.9567034872774));
#58828=CARTESIAN_POINT('Ctrl Pts',(2.4093599590983,94.7279132480597,13.0664878167119));
#58829=CARTESIAN_POINT('Ctrl Pts',(2.41369253775473,94.7417753550302,13.1768991709058));
#58830=CARTESIAN_POINT('Ctrl Pts',(2.41066283041136,94.7555907348959,13.2868736416682));
#58831=CARTESIAN_POINT('Ctrl Pts',(2.4097227836513,94.7598773215559,13.3209961271803));
#58832=CARTESIAN_POINT('Ctrl Pts',(2.40807401512869,94.7641594609854,13.3550769239517));
#58833=CARTESIAN_POINT('Ctrl Pts',(2.4057192750869,94.7684352653559,13.3890852664348));
#58834=CARTESIAN_POINT('Ctrl Pts',(2.39877851539224,94.7810384954836,13.4893272161194));
#58835=CARTESIAN_POINT('Ctrl Pts',(2.38570406559735,94.7935850145768,13.5889366944001));
#58836=CARTESIAN_POINT('Ctrl Pts',(2.36658259508796,94.806021906971,13.6870815142501));
#58837=CARTESIAN_POINT('Ctrl Pts',(2.35890433225087,94.811015964757,13.7264917532553));
#58838=CARTESIAN_POINT('Ctrl Pts',(2.35025130319088,94.8159924040279,13.7656663340367));
#58839=CARTESIAN_POINT('Ctrl Pts',(2.3406300562542,94.820948033628,13.804553552828));
#58840=CARTESIAN_POINT('Ctrl Pts',(2.33595811646162,94.8233544164263,13.823436629636));
#58841=CARTESIAN_POINT('Ctrl Pts',(2.33105789241856,94.8257558948871,13.8422516379537));
#58842=CARTESIAN_POINT('Ctrl Pts',(2.32593019905366,94.8281521250499,13.8609924524362));
#58843=CARTESIAN_POINT('Ctrl Pts',(2.32592747042772,94.8281534001682,13.8610024250826));
#58844=CARTESIAN_POINT('Ctrl Pts',(2.32592474173736,94.8281546752851,13.861012397708));
#58845=CARTESIAN_POINT('Ctrl Pts',(2.3259220129826,94.8281559504004,13.8610223703123));
#58846=CARTESIAN_POINT('Ctrl Pts',(2.30640662585915,94.8372752637657,13.9323439991563));
#58847=CARTESIAN_POINT('Ctrl Pts',(2.28357429399887,94.8463285543566,14.0026707706559));
#58848=CARTESIAN_POINT('Ctrl Pts',(2.25750079135267,94.8553907428659,14.0716728262931));
#58849=CARTESIAN_POINT('Ctrl Pts',(2.25238156496514,94.8571699972751,14.0852205704841));
#58850=CARTESIAN_POINT('Ctrl Pts',(2.2471374808347,94.8589495754404,14.09871711323));
#58851=CARTESIAN_POINT('Ctrl Pts',(2.24176924538978,94.8607300161108,14.1121597640997));
#58852=CARTESIAN_POINT('Ctrl Pts',(2.19182633343581,94.8772941911647,14.2372222982799));
#58853=CARTESIAN_POINT('Ctrl Pts',(2.13112338733817,94.8939395864207,14.3576440009253));
#58854=CARTESIAN_POINT('Ctrl Pts',(2.06094545719024,94.9106199561259,14.4718988563154));
#58855=CARTESIAN_POINT('Ctrl Pts',(1.99338878329255,94.9266772877442,14.5818861128581));
#58856=CARTESIAN_POINT('Ctrl Pts',(1.91705169652033,94.9427659024484,14.6861574254224));
#58857=CARTESIAN_POINT('Ctrl Pts',(1.83311890325089,94.9588289800573,14.7833506824778));
#58858=CARTESIAN_POINT('Ctrl Pts',(1.76539333323301,94.9717903154893,14.8617761521847));
#58859=CARTESIAN_POINT('Ctrl Pts',(1.69272515930329,94.9847328008935,14.9355917985685));
#58860=CARTESIAN_POINT('Ctrl Pts',(1.61572928392796,94.9976709245923,15.0039820720135));
#58861=CARTESIAN_POINT('Ctrl Pts',(1.59543876744322,95.0010804736222,15.0220047773074));
#58862=CARTESIAN_POINT('Ctrl Pts',(1.57484796678736,95.0044897018255,15.0396508086428));
#58863=CARTESIAN_POINT('Ctrl Pts',(1.55396868625079,95.0078988357666,15.0569055014235));
#58864=CARTESIAN_POINT('Ctrl Pts',(1.52259624465312,95.0130212754636,15.0828317703195));
#58865=CARTESIAN_POINT('Ctrl Pts',(1.49057165165312,95.0181443089837,15.1078749106348));
#58866=CARTESIAN_POINT('Ctrl Pts',(1.45793587909852,95.0232268143161,15.1321138996865));
#58867=CARTESIAN_POINT('Ctrl Pts',(1.45791763697052,95.0232296552389,15.132127448339));
#58868=CARTESIAN_POINT('Ctrl Pts',(1.45789939464426,95.0232324961502,15.1321409967456));
#58869=CARTESIAN_POINT('Ctrl Pts',(1.4578811521197,95.0232353370497,15.1321545449063));
#58870=CARTESIAN_POINT('Ctrl Pts',(1.43842008557607,95.0262659995519,15.1466076791988));
#58871=CARTESIAN_POINT('Ctrl Pts',(1.41873355562059,95.029283362287,15.1607809782664));
#58872=CARTESIAN_POINT('Ctrl Pts',(1.3988312522153,95.0322806589062,15.1746907112598));
#58873=CARTESIAN_POINT('Ctrl Pts',(1.36186797940274,95.0378473458558,15.2005243670391));
#58874=CARTESIAN_POINT('Ctrl Pts',(1.32416532569594,95.0433419253653,15.2254478281681));
#58875=CARTESIAN_POINT('Ctrl Pts',(1.28580327176107,95.0488344411743,15.249210063907));
#58876=CARTESIAN_POINT('Ctrl Pts',(1.26889124922504,95.0512558326696,15.2596857143246));
#58877=CARTESIAN_POINT('Ctrl Pts',(1.25185174888997,95.0536767561581,15.2699357114748));
#58878=CARTESIAN_POINT('Ctrl Pts',(1.23469481319672,95.0561028952065,15.2799388433483));
#58879=CARTESIAN_POINT('Ctrl Pts',(1.16530620576252,95.0659150442419,15.3203949832498));
#58880=CARTESIAN_POINT('Ctrl Pts',(1.09396469403016,95.0758258588412,15.3568131446592));
#58881=CARTESIAN_POINT('Ctrl Pts',(1.02109112390281,95.0858125894788,15.3892182119301));
#58882=CARTESIAN_POINT('Ctrl Pts',(0.985260328694605,95.090722908812,15.4051512769229));
#58883=CARTESIAN_POINT('Ctrl Pts',(0.94905838480203,95.0956516279515,15.4201138743091));
#58884=CARTESIAN_POINT('Ctrl Pts',(0.91253120638146,95.1005963119219,15.4341069509406));
#58885=CARTESIAN_POINT('Ctrl Pts',(0.847516086524827,95.10939740839,15.4590133793509));
#58886=CARTESIAN_POINT('Ctrl Pts',(0.781473143296777,95.1182480463249,15.4808498490037));
#58887=CARTESIAN_POINT('Ctrl Pts',(0.714696263141219,95.1270909750256,15.4996974571892));
#58888=CARTESIAN_POINT('Ctrl Pts',(0.665033561349754,95.1336675585678,15.5137146311365));
#58889=CARTESIAN_POINT('Ctrl Pts',(0.614963849992617,95.1402400039355,15.5260789052132));
#58890=CARTESIAN_POINT('Ctrl Pts',(0.564589439724732,95.1467869856434,15.5368232958241));
#58891=CARTESIAN_POINT('Ctrl Pts',(0.49587615082234,95.1557174057345,15.5514791977434));
#58892=CARTESIAN_POINT('Ctrl Pts',(0.426601235300059,95.164541336616,15.5632716080919));
#58893=CARTESIAN_POINT('Ctrl Pts',(0.357024047331103,95.1733167866231,15.5719815226317));
#58894=CARTESIAN_POINT('Ctrl Pts',(0.307152376719118,95.1796068705573,15.5782246319276));
#58895=CARTESIAN_POINT('Ctrl Pts',(0.257126476871656,95.1858719188813,15.5828837608138));
#58896=CARTESIAN_POINT('Ctrl Pts',(0.207058237683818,95.1921313301595,15.5858780044571));
#58897=CARTESIAN_POINT('Ctrl Pts',(0.14577073648907,95.1997933466875,15.5895431964799));
#58898=CARTESIAN_POINT('Ctrl Pts',(0.0844266935233488,95.2074460632808,
15.5907123431602));
#58899=CARTESIAN_POINT('Ctrl Pts',(0.0232698315542606,95.2150836664526,
15.5893406044066));
#58900=CARTESIAN_POINT('Ctrl Pts',(0.00373966605249472,95.2175227002614,
15.5889025458794));
#58901=CARTESIAN_POINT('Ctrl Pts',(-0.0157812326790508,95.2199614184581,
15.5882052663386));
#58902=CARTESIAN_POINT('Ctrl Pts',(-0.0352857644478857,95.2223996749869,
15.5872510169546));
#58903=CARTESIAN_POINT('Ctrl Pts',(-0.118858048625808,95.2328470248609,
15.5831622850824));
#58904=CARTESIAN_POINT('Ctrl Pts',(-0.20212757240947,95.2432856423306,15.57435170011));
#58905=CARTESIAN_POINT('Ctrl Pts',(-0.284512201205189,95.2537010724677,
15.5610299742258));
#58906=CARTESIAN_POINT('Ctrl Pts',(-0.294743296444043,95.2549945329013,
15.5593755898065));
#58907=CARTESIAN_POINT('Ctrl Pts',(-0.304960752864069,95.2562876359942,
15.5576516980548));
#58908=CARTESIAN_POINT('Ctrl Pts',(-0.315163464674268,95.2575803542851,
15.5558587571799));
#58909=CARTESIAN_POINT('Ctrl Pts',(-0.412099633719754,95.2698624966316,
15.5388239900537));
#58910=CARTESIAN_POINT('Ctrl Pts',(-0.507699861241456,95.282109358852,15.5155569669214));
#58911=CARTESIAN_POINT('Ctrl Pts',(-0.601229851418452,95.294291541424,15.486505910759));
#58912=CARTESIAN_POINT('Ctrl Pts',(-0.616704290937099,95.29630707085,15.4816994437564));
#58913=CARTESIAN_POINT('Ctrl Pts',(-0.632122174381767,95.2983208418937,
15.4767346275083));
#58914=CARTESIAN_POINT('Ctrl Pts',(-0.647480310265967,95.3003327358378,
15.471613461004));
#58915=CARTESIAN_POINT('Ctrl Pts',(-0.707690042210776,95.3082201250359,
15.4515365412012));
#58916=CARTESIAN_POINT('Ctrl Pts',(-0.767012739212091,95.3160591733945,
15.4291118063293));
#58917=CARTESIAN_POINT('Ctrl Pts',(-0.825210479240838,95.3239049988934,
15.4042811838574));
#58918=CARTESIAN_POINT('Ctrl Pts',(-0.871582749652548,95.3301565945989,
15.3844960111138));
#58919=CARTESIAN_POINT('Ctrl Pts',(-0.917239751485826,95.3364123695739,
15.3631832960744));
#58920=CARTESIAN_POINT('Ctrl Pts',(-0.962038500852752,95.3426972625086,
15.3403201667661));
#58921=CARTESIAN_POINT('Ctrl Pts',(-1.01684562864418,95.3503862479177,15.3123492419653));
#58922=CARTESIAN_POINT('Ctrl Pts',(-1.07039430988932,95.3581096649516,15.2820817073528));
#58923=CARTESIAN_POINT('Ctrl Pts',(-1.12256875438812,95.3658159655874,15.2497401217053));
#58924=CARTESIAN_POINT('Ctrl Pts',(-1.16550523980646,95.3721577957315,15.2231249074198));
#58925=CARTESIAN_POINT('Ctrl Pts',(-1.2075120192865,95.3784881524552,15.1951048624561));
#58926=CARTESIAN_POINT('Ctrl Pts',(-1.2485462574634,95.3847816704486,15.1657891575002));
#58927=CARTESIAN_POINT('Ctrl Pts',(-1.28650442894323,95.3906034048298,15.1386710579519));
#58928=CARTESIAN_POINT('Ctrl Pts',(-1.32356327725076,95.3964204635369,15.1103743642508));
#58929=CARTESIAN_POINT('Ctrl Pts',(-1.35961987671512,95.4022300177208,15.080950862646));
#58930=CARTESIAN_POINT('Ctrl Pts',(-1.37565779232735,95.4048140977819,15.0678633379552));
#58931=CARTESIAN_POINT('Ctrl Pts',(-1.39150515784867,95.4073979316919,15.0545466685588));
#58932=CARTESIAN_POINT('Ctrl Pts',(-1.40715667418759,95.4099813311926,15.041008543745));
#58933=CARTESIAN_POINT('Ctrl Pts',(-1.47136461940602,95.4205793314132,14.9854704631157));
#58934=CARTESIAN_POINT('Ctrl Pts',(-1.53227324531738,95.4311699153715,14.9262027716018));
#58935=CARTESIAN_POINT('Ctrl Pts',(-1.58953095433024,95.4417391135738,14.8637684311561));
#58936=CARTESIAN_POINT('Ctrl Pts',(-1.62864806456368,95.4489597393775,14.8211147689738));
#58937=CARTESIAN_POINT('Ctrl Pts',(-1.66605987183824,95.4561699746208,14.7769867410379));
#58938=CARTESIAN_POINT('Ctrl Pts',(-1.70167250251401,95.463367047025,14.7315625019744));
#58939=CARTESIAN_POINT('Ctrl Pts',(-1.73997683466568,95.4711080941382,14.6827049728393));
#58940=CARTESIAN_POINT('Ctrl Pts',(-1.7762005158223,95.4788340079623,14.6323476481508));
#58941=CARTESIAN_POINT('Ctrl Pts',(-1.81024426484934,95.4865438722681,14.5806983708747));
#58942=CARTESIAN_POINT('Ctrl Pts',(-1.86411551659837,95.4987440574076,14.4989679123232));
#58943=CARTESIAN_POINT('Ctrl Pts',(-1.91254280583083,95.5109064364272,14.4139890410822));
#58944=CARTESIAN_POINT('Ctrl Pts',(-1.95518498824451,95.5230438721566,14.3264537180762));
#58945=CARTESIAN_POINT('Ctrl Pts',(-1.98279957081004,95.5309039347076,14.2697668585458));
#58946=CARTESIAN_POINT('Ctrl Pts',(-2.00798817134963,95.5387538769753,14.2120045961421));
#58947=CARTESIAN_POINT('Ctrl Pts',(-2.03064411381718,95.5465958755964,14.1533593567212));
#58948=CARTESIAN_POINT('Ctrl Pts',(-2.06813035770517,95.55957115011,14.0563256645256));
#58949=CARTESIAN_POINT('Ctrl Pts',(-2.09867778680689,95.5725232965738,13.9568841690516));
#58950=CARTESIAN_POINT('Ctrl Pts',(-2.1217652090683,95.58545200991,13.8559834397369));
#58951=CARTESIAN_POINT('Ctrl Pts',(-2.14227665834112,95.5969382054997,13.7663406824167));
#58952=CARTESIAN_POINT('Ctrl Pts',(-2.15689986373622,95.6084053748756,13.6755505235125));
#58953=CARTESIAN_POINT('Ctrl Pts',(-2.16574516758808,95.6198564696486,13.5842996138752));
#58954=CARTESIAN_POINT('Ctrl Pts',(-2.17211995197266,95.6281092398606,13.5185353525704));
#58955=CARTESIAN_POINT('Ctrl Pts',(-2.17549201090315,95.6363548045513,13.4525225851773));
#58956=CARTESIAN_POINT('Ctrl Pts',(-2.17590326200913,95.6445846214129,13.3865967293626));
#58957=CARTESIAN_POINT('Ctrl Pts',(-2.17606264055466,95.6477740505045,13.3610474557932));
#58958=CARTESIAN_POINT('Ctrl Pts',(-2.1757775959806,95.6509611121884,13.335511268976));
#58959=CARTESIAN_POINT('Ctrl Pts',(-2.17505156918613,95.6541453093621,13.3100076794586));
#58960=CARTESIAN_POINT('Ctrl Pts',(-2.17300309787237,95.6631294634148,13.2380497683699));
#58961=CARTESIAN_POINT('Ctrl Pts',(-2.16752924649556,95.6720775411009,13.1663416718358));
#58962=CARTESIAN_POINT('Ctrl Pts',(-2.15857548450997,95.6810176218596,13.0951743479573));
#58963=CARTESIAN_POINT('Ctrl Pts',(-2.15624659691499,95.6833429509459,13.0766636149252));
#58964=CARTESIAN_POINT('Ctrl Pts',(-2.15368217620392,95.6856677074371,13.0581897171597));
#58965=CARTESIAN_POINT('Ctrl Pts',(-2.15088106624707,95.6879923187851,13.039758314068));
#58966=CARTESIAN_POINT('Ctrl Pts',(-2.13474051480207,95.7013871906862,12.9335529117854));
#58967=CARTESIAN_POINT('Ctrl Pts',(-2.11080268605646,95.7147709892224,12.8287124234999));
#58968=CARTESIAN_POINT('Ctrl Pts',(-2.07934926399926,95.7281262603083,12.7264205178026));
#58969=CARTESIAN_POINT('Ctrl Pts',(-2.05792705046345,95.7372222330298,12.6567518171172));
#58970=CARTESIAN_POINT('Ctrl Pts',(-2.03301888080868,95.7463051150478,12.5882642240548));
#58971=CARTESIAN_POINT('Ctrl Pts',(-2.00471254214963,95.7553712266143,12.5213179818491));
#58972=CARTESIAN_POINT('Ctrl Pts',(-1.99475252620534,95.7585612759118,12.4977619279274));
#58973=CARTESIAN_POINT('Ctrl Pts',(-1.98436872862985,95.7617495293799,12.4743999366367));
#58974=CARTESIAN_POINT('Ctrl Pts',(-1.97356473464234,95.76493578494,12.4512495612729));
#58975=CARTESIAN_POINT('Ctrl Pts',(-1.97355279841807,95.7649393051068,12.4512239847988));
#58976=CARTESIAN_POINT('Ctrl Pts',(-1.97354086168094,95.7649428252711,12.451198408583));
#58977=CARTESIAN_POINT('Ctrl Pts',(-1.97352892443098,95.7649463454331,12.4511728326255));
#58978=CARTESIAN_POINT('Ctrl Pts',(-1.93787473334702,95.7754603688591,12.374782535174));
#58979=CARTESIAN_POINT('Ctrl Pts',(-1.89762639969028,95.7859580587182,12.3006573840691));
#58980=CARTESIAN_POINT('Ctrl Pts',(-1.85331695285095,95.796426158897,12.2291776297439));
#58981=CARTESIAN_POINT('Ctrl Pts',(-1.83727577927542,95.8002158837515,12.2033000973426));
#58982=CARTESIAN_POINT('Ctrl Pts',(-1.82070219758726,95.8040017916461,12.1777688086928));
#58983=CARTESIAN_POINT('Ctrl Pts',(-1.80362085265156,95.8077834618331,12.1526002598606));
#58984=CARTESIAN_POINT('Ctrl Pts',(-1.78202255477625,95.8125651484902,12.1207761958413));
#58985=CARTESIAN_POINT('Ctrl Pts',(-1.75958563591836,95.8173432133199,12.0895511217171));
#58986=CARTESIAN_POINT('Ctrl Pts',(-1.73633811654556,95.8221192234617,12.058977289736));
#58987=CARTESIAN_POINT('Ctrl Pts',(-1.66663457668081,95.8364392379103,11.9673071084087));
#58988=CARTESIAN_POINT('Ctrl Pts',(-1.58964146194808,95.8507411093057,11.8814947342166));
#58989=CARTESIAN_POINT('Ctrl Pts',(-1.50652447525991,95.8650199624051,11.8026109896439));
#58990=CARTESIAN_POINT('Ctrl Pts',(-1.46114538740433,95.8728157374337,11.7595431100446));
#58991=CARTESIAN_POINT('Ctrl Pts',(-1.41394159235836,95.8806045476131,11.7185399399839));
#58992=CARTESIAN_POINT('Ctrl Pts',(-1.36510687148839,95.888385133887,11.6797706355735));
#58993=CARTESIAN_POINT('Ctrl Pts',(-1.28959584252985,95.9004159198723,11.6198233272675));
#58994=CARTESIAN_POINT('Ctrl Pts',(-1.21022638718133,95.9124240035505,11.5651294907366));
#58995=CARTESIAN_POINT('Ctrl Pts',(-1.12774807335125,95.9244009269098,11.5163062222698));
#58996=CARTESIAN_POINT('Ctrl Pts',(-1.11380347968499,95.9264258631853,11.5080516810624));
#58997=CARTESIAN_POINT('Ctrl Pts',(-1.0997699745765,95.9284499214416,11.4999648367301));
#58998=CARTESIAN_POINT('Ctrl Pts',(-1.08565111724086,95.9304730762785,11.4920485383264));
#58999=CARTESIAN_POINT('Ctrl Pts',(-1.06139616484,95.9339486779579,11.4784490354481));
#59000=CARTESIAN_POINT('Ctrl Pts',(-1.0369000705869,95.937420739775,11.465333119402));
#59001=CARTESIAN_POINT('Ctrl Pts',(-1.01218504280194,95.9408889018017,11.4527035840313));
#59002=CARTESIAN_POINT('Ctrl Pts',(-1.0121643460679,95.9408918060925,11.4526930078694));
#59003=CARTESIAN_POINT('Ctrl Pts',(-1.01214364918012,95.9408947103805,11.4526824320485));
#59004=CARTESIAN_POINT('Ctrl Pts',(-1.01212295213882,95.9408976146659,11.4526718565687));
#59005=CARTESIAN_POINT('Ctrl Pts',(-0.980130078477351,95.9453869729441,
11.4363245929073));
#59006=CARTESIAN_POINT('Ctrl Pts',(-0.94772828265125,95.9498750213854,11.4207975708423));
#59007=CARTESIAN_POINT('Ctrl Pts',(-0.914959759593808,95.9543615825662,
11.4061156705712));
#59008=CARTESIAN_POINT('Ctrl Pts',(-0.848326045309448,95.9634848572195,
11.3762605090768));
#59009=CARTESIAN_POINT('Ctrl Pts',(-0.780182134957265,95.9726011635176,
11.3499002941302));
#59010=CARTESIAN_POINT('Ctrl Pts',(-0.710906234045462,95.9817091443279,
11.3271548907497));
#59011=CARTESIAN_POINT('Ctrl Pts',(-0.666439205165701,95.9875554031336,
11.3125550010956));
#59012=CARTESIAN_POINT('Ctrl Pts',(-0.62150684637548,95.9933981145678,11.2994445172896));
#59013=CARTESIAN_POINT('Ctrl Pts',(-0.576220351855335,95.9992356586606,
11.2878537721618));
#59014=CARTESIAN_POINT('Ctrl Pts',(-0.522826054268815,96.0061183191484,
11.2741878944833));
#59015=CARTESIAN_POINT('Ctrl Pts',(-0.468934391840693,96.0129944243556,
11.262634800864));
#59016=CARTESIAN_POINT('Ctrl Pts',(-0.414718625558492,96.0198624171801,
11.2532427688084));
#59017=CARTESIAN_POINT('Ctrl Pts',(-0.29434694244602,96.0351109677878,11.232390260693));
#59018=CARTESIAN_POINT('Ctrl Pts',(-0.172377141413166,96.0503195515522,
11.2221941161788));
#59019=CARTESIAN_POINT('Ctrl Pts',(-0.0507252149178954,96.0654809749851,
11.2226095713006));
#59020=CARTESIAN_POINT('Ctrl Pts',(0.00101769105191436,96.0719296694666,
11.2227862791911));
#59021=CARTESIAN_POINT('Ctrl Pts',(0.0527029832957061,96.0783698243123,
11.2248820915687));
#59022=CARTESIAN_POINT('Ctrl Pts',(0.104183178719241,96.0848009594534,11.2288907196644));
#59023=CARTESIAN_POINT('Ctrl Pts',(0.186272301341844,96.0950558980149,11.2352827848187));
#59024=CARTESIAN_POINT('Ctrl Pts',(0.267844000106881,96.1052884101216,11.2465398472509));
#59025=CARTESIAN_POINT('Ctrl Pts',(0.348285412315078,96.1154971448446,11.2625358784358));
#59026=CARTESIAN_POINT('Ctrl Pts',(0.384748555108407,96.1201246438121,11.2697866905885));
#59027=CARTESIAN_POINT('Ctrl Pts',(0.420980163909315,96.1247473462816,11.278011142707));
#59028=CARTESIAN_POINT('Ctrl Pts',(0.456926658271324,96.1293655697248,11.2871975023484));
#59029=CARTESIAN_POINT('Ctrl Pts',(0.508494969858789,96.1359908050843,11.3003761186433));
#59030=CARTESIAN_POINT('Ctrl Pts',(0.559473311276387,96.1426064281092,11.3155337689461));
#59031=CARTESIAN_POINT('Ctrl Pts',(0.609698270949521,96.1492125649547,11.3326328559732));
#59032=CARTESIAN_POINT('Ctrl Pts',(0.663633514182684,96.1563067189353,11.350995109002));
#59033=CARTESIAN_POINT('Ctrl Pts',(0.716698856128576,96.1633897928817,11.3715956364018));
#59034=CARTESIAN_POINT('Ctrl Pts',(0.768756448063106,96.1704729822069,11.3942719800529));
#59035=CARTESIAN_POINT('Ctrl Pts',(0.768768862494322,96.17047467137,11.3942773877927));
#59036=CARTESIAN_POINT('Ctrl Pts',(0.768781276868443,96.1704763605332,11.3942827956505));
#59037=CARTESIAN_POINT('Ctrl Pts',(0.768793691185528,96.1704780496965,11.3942882036265));
#59038=CARTESIAN_POINT('Ctrl Pts',(0.853814957640094,96.1820465312246,11.4313255181957));
#59039=CARTESIAN_POINT('Ctrl Pts',(0.936198354852795,96.1936172508596,11.4741798311531));
#59040=CARTESIAN_POINT('Ctrl Pts',(1.01529734550568,96.2051845723368,11.5222962174482));
#59041=CARTESIAN_POINT('Ctrl Pts',(1.06765635561441,96.2128414779074,11.5541465145964));
#59042=CARTESIAN_POINT('Ctrl Pts',(1.11857538549673,96.2204967750912,11.5883017404707));
#59043=CARTESIAN_POINT('Ctrl Pts',(1.16785982437448,96.2281474195521,11.6245906799445));
#59044=CARTESIAN_POINT('Ctrl Pts',(1.2311908069148,96.2379785719768,11.6712223195563));
#59045=CARTESIAN_POINT('Ctrl Pts',(1.29179889313266,96.2477976271712,11.7214177076016));
#59046=CARTESIAN_POINT('Ctrl Pts',(1.34926661736094,96.2575969719615,11.7748834431036));
#59047=CARTESIAN_POINT('Ctrl Pts',(1.38747278965184,96.264111854192,11.810428979832));
#59048=CARTESIAN_POINT('Ctrl Pts',(1.42428988158487,96.2706178953477,11.8474197352934));
#59049=CARTESIAN_POINT('Ctrl Pts',(1.45958400593841,96.2771113254996,11.885763560152));
#59050=CARTESIAN_POINT('Ctrl Pts',(1.47104336648822,96.2792196242229,11.8982131030139));
#59051=CARTESIAN_POINT('Ctrl Pts',(1.48234259526421,96.2813266706931,11.9108054908799));
#59052=CARTESIAN_POINT('Ctrl Pts',(1.4934792669407,96.2834327268134,11.9235360145983));
#59053=CARTESIAN_POINT('Ctrl Pts',(1.49348443358187,96.283433703877,11.9235419206759));
#59054=CARTESIAN_POINT('Ctrl Pts',(1.49348960018741,96.2834346809402,11.9235478267827));
#59055=CARTESIAN_POINT('Ctrl Pts',(1.49349476675733,96.2834356580031,11.9235537329185));
#59056=CARTESIAN_POINT('Ctrl Pts',(1.54955196201186,96.2940367738654,11.9876352052438));
#59057=CARTESIAN_POINT('Ctrl Pts',(1.60141383309193,96.3045981956347,12.0551335272336));
#59058=CARTESIAN_POINT('Ctrl Pts',(1.64880542222686,96.3151357596347,12.1254293339887));
#59059=CARTESIAN_POINT('Ctrl Pts',(1.67777069941973,96.3215762160061,12.168393445666));
#59060=CARTESIAN_POINT('Ctrl Pts',(1.70506650503284,96.3280078759479,12.212403525441));
#59061=CARTESIAN_POINT('Ctrl Pts',(1.73063201875259,96.3344354421685,12.2573274847705));
#59062=CARTESIAN_POINT('Ctrl Pts',(1.77325818609066,96.3451523210194,12.3322305838773));
#59063=CARTESIAN_POINT('Ctrl Pts',(1.81107681615759,96.3558585099647,12.4096730870144));
#59064=CARTESIAN_POINT('Ctrl Pts',(1.84378220907545,96.3665708757059,12.4890056422043));
#59065=CARTESIAN_POINT('Ctrl Pts',(1.86877617329365,96.3747574303423,12.549632800873));
#59066=CARTESIAN_POINT('Ctrl Pts',(1.89078475316923,96.3829477275824,12.6113645024578));
#59067=CARTESIAN_POINT('Ctrl Pts',(1.90968125808506,96.3911518875422,12.6739288632165));
#59068=CARTESIAN_POINT('Ctrl Pts',(1.9125907471821,96.3924150795483,12.6835618787557));
#59069=CARTESIAN_POINT('Ctrl Pts',(1.91542637278672,96.3936785729357,12.6932145054351));
#59070=CARTESIAN_POINT('Ctrl Pts',(1.91818764680601,96.3949423945857,12.7028857148542));
#59071=CARTESIAN_POINT('Ctrl Pts',(1.91818905954012,96.3949430411872,12.7028906628772));
#59072=CARTESIAN_POINT('Ctrl Pts',(1.91819047225476,96.3949436877888,12.7028956109051));
#59073=CARTESIAN_POINT('Ctrl Pts',(1.91819188494994,96.3949443343905,12.7029005589378));
#59074=CARTESIAN_POINT('Ctrl Pts',(1.92429624476701,96.3977383478278,12.7242813724547));
#59075=CARTESIAN_POINT('Ctrl Pts',(1.93004069192381,96.4005353529886,12.7457621690415));
#59076=CARTESIAN_POINT('Ctrl Pts',(1.93541929227345,96.4033337409118,12.7673314485684));
#59077=CARTESIAN_POINT('Ctrl Pts',(1.95478165646614,96.4134076267929,12.8449784605094));
#59078=CARTESIAN_POINT('Ctrl Pts',(1.96940226796508,96.4234994925514,12.9237697227759));
#59079=CARTESIAN_POINT('Ctrl Pts',(1.97928283481565,96.4335865836525,13.0031205781567));
#59080=CARTESIAN_POINT('Ctrl Pts',(1.98288946460194,96.4372685994491,13.0320854303673));
#59081=CARTESIAN_POINT('Ctrl Pts',(1.98586471178355,96.4409499288741,13.0611243771114));
#59082=CARTESIAN_POINT('Ctrl Pts',(1.98820941786643,96.4446292924097,13.0902074416763));
#59083=CARTESIAN_POINT('Ctrl Pts',(1.99492353019111,96.4551652227943,13.173487373289));
#59084=CARTESIAN_POINT('Ctrl Pts',(1.99646481606683,96.4656849900875,13.2571322183715));
#59085=CARTESIAN_POINT('Ctrl Pts',(1.9928596492666,96.4761605018442,13.3404687148225));
#59086=CARTESIAN_POINT('Ctrl Pts',(1.99160969799698,96.4797924778237,13.3693624013887));
#59087=CARTESIAN_POINT('Ctrl Pts',(1.98974119464507,96.4834190748398,13.3982185749907));
#59088=CARTESIAN_POINT('Ctrl Pts',(1.98725566383167,96.4870389346109,13.4270077853693));
#59089=CARTESIAN_POINT('Ctrl Pts',(1.97980151173059,96.4978949598804,13.5133471507374));
#59090=CARTESIAN_POINT('Ctrl Pts',(1.96679594258491,96.5086903725417,13.599088109065));
#59091=CARTESIAN_POINT('Ctrl Pts',(1.94829282052133,96.5193972636432,13.6834765967547));
#59092=CARTESIAN_POINT('Ctrl Pts',(1.94286298122375,96.522539257619,13.7082408460066));
#59093=CARTESIAN_POINT('Ctrl Pts',(1.9369597083664,96.525673584629,13.7328882876823));
#59094=CARTESIAN_POINT('Ctrl Pts',(1.9305844127389,96.5287994301737,13.7573990147299));
#59095=CARTESIAN_POINT('Ctrl Pts',(1.91343077839771,96.5372099596007,13.8233485916246));
#59096=CARTESIAN_POINT('Ctrl Pts',(1.89285663288248,96.5455607072524,13.8883211413174));
#59097=CARTESIAN_POINT('Ctrl Pts',(1.86906225836649,96.5538832067112,13.9519740874812));
#59098=CARTESIAN_POINT('Ctrl Pts',(1.85209719086988,96.5598170363634,13.9973577779539));
#59099=CARTESIAN_POINT('Ctrl Pts',(1.83349497978107,96.5657366456325,14.0420717676147));
#59100=CARTESIAN_POINT('Ctrl Pts',(1.81332225629261,96.5716555337813,14.086006801809));
#59101=CARTESIAN_POINT('Ctrl Pts',(1.78588406002382,96.5797061876661,14.145765618807));
#59102=CARTESIAN_POINT('Ctrl Pts',(1.75554337688148,96.5877560732731,14.2040807186407));
#59103=CARTESIAN_POINT('Ctrl Pts',(1.72249083697302,96.5958337879808,14.2606441922532));
#59104=CARTESIAN_POINT('Ctrl Pts',(1.70141109533706,96.600985468896,14.2967183763578));
#59105=CARTESIAN_POINT('Ctrl Pts',(1.67922835419628,96.6061485879362,14.3320811519021));
#59106=CARTESIAN_POINT('Ctrl Pts',(1.65599074082823,96.6113318017801,14.3666635818558));
#59107=CARTESIAN_POINT('Ctrl Pts',(1.65131304494949,96.6123751747656,14.373624971888));
#59108=CARTESIAN_POINT('Ctrl Pts',(1.64660456825496,96.6134239217114,14.3805635176563));
#59109=CARTESIAN_POINT('Ctrl Pts',(1.64185061560271,96.614472345387,14.3874675456986));
#59110=CARTESIAN_POINT('Ctrl Pts',(1.64184231942404,96.6144741750035,14.3874795939991));
#59111=CARTESIAN_POINT('Ctrl Pts',(1.64183402310706,96.614476004619,14.3874916421943));
#59112=CARTESIAN_POINT('Ctrl Pts',(1.64182572665163,96.6144778342334,14.3875036902841));
#59113=CARTESIAN_POINT('Ctrl Pts',(1.5948408133683,96.6248394007863,14.4557350526163));
#59114=CARTESIAN_POINT('Ctrl Pts',(1.54339801233543,96.6352440080243,14.5208725954583));
#59115=CARTESIAN_POINT('Ctrl Pts',(1.48809123974865,96.6456718247073,14.5825065833522));
#59116=CARTESIAN_POINT('Ctrl Pts',(1.47805984267335,96.6475631946948,14.593685594113));
#59117=CARTESIAN_POINT('Ctrl Pts',(1.46790146364113,96.6494553219179,14.6047493796719));
#59118=CARTESIAN_POINT('Ctrl Pts',(1.45761981942515,96.651348079647,14.6156955475071));
#59119=CARTESIAN_POINT('Ctrl Pts',(1.38766361293164,96.6642263846881,14.6901731661941));
#59120=CARTESIAN_POINT('Ctrl Pts',(1.31183355965818,96.6770701992615,14.7590824059048));
#59121=CARTESIAN_POINT('Ctrl Pts',(1.23121719354291,96.6898422258653,14.8217255310512));
#59122=CARTESIAN_POINT('Ctrl Pts',(1.14962085059773,96.7027695099031,14.8851301493553));
#59123=CARTESIAN_POINT('Ctrl Pts',(1.06312206621914,96.7156229243032,14.942114893507));
#59124=CARTESIAN_POINT('Ctrl Pts',(0.972882099229031,96.7283769835321,14.9919867057191));
#59125=CARTESIAN_POINT('Ctrl Pts',(0.883954667112826,96.7409455357391,15.0411331354324));
#59126=CARTESIAN_POINT('Ctrl Pts',(0.791395048648228,96.7534172449107,15.0833717561073));
#59127=CARTESIAN_POINT('Ctrl Pts',(0.696332474724466,96.765785423087,15.1180743122479));
#59128=CARTESIAN_POINT('Ctrl Pts',(0.677351449785182,96.7682549617154,15.12500332812));
#59129=CARTESIAN_POINT('Ctrl Pts',(0.658287563029822,96.7707416625033,15.1316832108969));
#59130=CARTESIAN_POINT('Ctrl Pts',(0.639152814130027,96.7732587587901,15.1381405055837));
#59131=CARTESIAN_POINT('Ctrl Pts',(0.566661679031735,96.7827946647978,15.1626036759112));
#59132=CARTESIAN_POINT('Ctrl Pts',(0.49282441715406,96.7923303004171,15.1828190378486));
#59133=CARTESIAN_POINT('Ctrl Pts',(0.418181192380986,96.801858035304,15.1984908859961));
#59134=CARTESIAN_POINT('Ctrl Pts',(0.372795814454764,96.8076511913465,15.2080198519959));
#59135=CARTESIAN_POINT('Ctrl Pts',(0.3271081986575,96.8134419946363,15.2158700313298));
#59136=CARTESIAN_POINT('Ctrl Pts',(0.281260566632972,96.8192262850474,15.2219780794927));
#59137=CARTESIAN_POINT('Ctrl Pts',(0.251704726021794,96.8229551486308,15.2259156546733));
#59138=CARTESIAN_POINT('Ctrl Pts',(0.222083460018819,96.8266811747956,15.2291292646824));
#59139=CARTESIAN_POINT('Ctrl Pts',(0.192436998294307,96.830403003659,15.2316043318055));
#59140=CARTESIAN_POINT('Ctrl Pts',(0.177582023084877,96.832267903289,15.2328445155784));
#59141=CARTESIAN_POINT('Ctrl Pts',(0.162710795323073,96.8341329950944,15.2339001422121));
#59142=CARTESIAN_POINT('Ctrl Pts',(0.147827757845089,96.8359981944933,15.2347724717209));
#59143=CARTESIAN_POINT('Ctrl Pts',(0.0772629933168082,96.8448416417115,
15.2389084370082));
#59144=CARTESIAN_POINT('Ctrl Pts',(0.00643537457473485,96.8536871475861,
15.2389194584622));
#59145=CARTESIAN_POINT('Ctrl Pts',(-0.0641387309311826,96.8625207338574,
15.2349692109548));
#59146=CARTESIAN_POINT('Ctrl Pts',(-0.0771742157732686,96.864152353261,
15.2342395751891));
#59147=CARTESIAN_POINT('Ctrl Pts',(-0.0902010511963878,96.8657835662794,
15.233374938362));
#59148=CARTESIAN_POINT('Ctrl Pts',(-0.103215991010027,96.8674142851885,
15.2323765231221));
#59149=CARTESIAN_POINT('Ctrl Pts',(-0.166641676164636,96.8753612650123,
15.227510947747));
#59150=CARTESIAN_POINT('Ctrl Pts',(-0.229785670077932,96.8832966225723,
15.2194689710231));
#59151=CARTESIAN_POINT('Ctrl Pts',(-0.292387832427161,96.8912816072917,
15.2085109581398));
#59152=CARTESIAN_POINT('Ctrl Pts',(-0.302083567934587,96.8925183105775,
15.2068137964026));
#59153=CARTESIAN_POINT('Ctrl Pts',(-0.311766403639732,96.8937562163189,
15.2050466593504));
#59154=CARTESIAN_POINT('Ctrl Pts',(-0.32143547883787,96.8949955652553,15.2032104804451));
#59155=CARTESIAN_POINT('Ctrl Pts',(-0.39298478617292,96.9041665103697,15.1896231076998));
#59156=CARTESIAN_POINT('Ctrl Pts',(-0.463764328797108,96.9133486001417,
15.1721090777386));
#59157=CARTESIAN_POINT('Ctrl Pts',(-0.533342416148416,96.922490239889,15.1507388991162));
#59158=CARTESIAN_POINT('Ctrl Pts',(-0.55868545034734,96.9258199791442,15.1429550523869));
#59159=CARTESIAN_POINT('Ctrl Pts',(-0.583868589780022,96.9291442892171,
15.1346596058387));
#59160=CARTESIAN_POINT('Ctrl Pts',(-0.60886927308371,96.9324604625022,15.1258560932481));
#59161=CARTESIAN_POINT('Ctrl Pts',(-0.703263780070516,96.9449812619751,
15.0926168725179));
#59162=CARTESIAN_POINT('Ctrl Pts',(-0.795054342654565,96.9573861214602,
15.0521385166626));
#59163=CARTESIAN_POINT('Ctrl Pts',(-0.883112879463809,96.9697181932088,
15.0049849995442));
#59164=CARTESIAN_POINT('Ctrl Pts',(-0.955284732212308,96.9798254298105,
14.9663384717077));
#59165=CARTESIAN_POINT('Ctrl Pts',(-1.02494896921815,96.9898840793762,14.9232085161692));
#59166=CARTESIAN_POINT('Ctrl Pts',(-1.09151383210832,96.999950508479,14.8759547770441));
#59167=CARTESIAN_POINT('Ctrl Pts',(-1.10453113864235,97.0019190815015,14.8667139196254));
#59168=CARTESIAN_POINT('Ctrl Pts',(-1.11743004979981,97.0038879731062,14.8573152712551));
#59169=CARTESIAN_POINT('Ctrl Pts',(-1.13020632708847,97.0058576354751,14.8477613871022));
#59170=CARTESIAN_POINT('Ctrl Pts',(-1.1498824989815,97.0088910241896,14.833047878418));
#59171=CARTESIAN_POINT('Ctrl Pts',(-1.16930221410112,97.0119564434176,14.8180095705093));
#59172=CARTESIAN_POINT('Ctrl Pts',(-1.18841205214264,97.0150214916683,14.8026054837613));
#59173=CARTESIAN_POINT('Ctrl Pts',(-1.24398486563493,97.0239348772453,14.7578092673831));
#59174=CARTESIAN_POINT('Ctrl Pts',(-1.29693707810882,97.0328455603298,14.7099147513584));
#59175=CARTESIAN_POINT('Ctrl Pts',(-1.34676854624776,97.0417400145777,14.6591832773238));
#59176=CARTESIAN_POINT('Ctrl Pts',(-1.34967742339086,97.0422592221313,14.6562218629653));
#59177=CARTESIAN_POINT('Ctrl Pts',(-1.35257567732859,97.0427783744049,14.6532507915937));
#59178=CARTESIAN_POINT('Ctrl Pts',(-1.3554632127988,97.0432974687158,14.6502701188745));
#59179=CARTESIAN_POINT('Ctrl Pts',(-1.35548420701023,97.0433012428602,14.6502484474963));
#59180=CARTESIAN_POINT('Ctrl Pts',(-1.35550520065501,97.0433050170014,14.6502267756106));
#59181=CARTESIAN_POINT('Ctrl Pts',(-1.35552619373324,97.0433087911397,14.6502051032174));
#59182=CARTESIAN_POINT('Ctrl Pts',(-1.39907127316221,97.0511373309756,14.6052509485129));
#59183=CARTESIAN_POINT('Ctrl Pts',(-1.44029344158329,97.0589822101343,14.5580202340714));
#59184=CARTESIAN_POINT('Ctrl Pts',(-1.47915585153603,97.0669126895379,14.5089162135298));
#59185=CARTESIAN_POINT('Ctrl Pts',(-1.50462635225016,97.0721103414993,14.4767333408826));
#59186=CARTESIAN_POINT('Ctrl Pts',(-1.52908428227552,97.0773448936824,14.44374546445));
#59187=CARTESIAN_POINT('Ctrl Pts',(-1.55252975469165,97.0826373060376,14.4100602107336));
#59188=CARTESIAN_POINT('Ctrl Pts',(-1.59225080221582,97.091603649686,14.3529910444578));
#59189=CARTESIAN_POINT('Ctrl Pts',(-1.62887304268975,97.1005957716121,14.2937832759773));
#59190=CARTESIAN_POINT('Ctrl Pts',(-1.66216995717027,97.1095353395864,14.2327791611904));
#59191=CARTESIAN_POINT('Ctrl Pts',(-1.68031818454648,97.114407782417,14.1995293371959));
#59192=CARTESIAN_POINT('Ctrl Pts',(-1.69747814378383,97.1192644930128,14.1657466882876));
#59193=CARTESIAN_POINT('Ctrl Pts',(-1.7136111324771,97.1240919369856,14.1314927698294));
#59194=CARTESIAN_POINT('Ctrl Pts',(-1.72774890789126,97.1283223570279,14.1014751323398));
#59195=CARTESIAN_POINT('Ctrl Pts',(-1.74109927569005,97.1325306439271,14.0710931895949));
#59196=CARTESIAN_POINT('Ctrl Pts',(-1.75363834435648,97.1367085707454,14.0403842715858));
#59197=CARTESIAN_POINT('Ctrl Pts',(-1.78265192617188,97.1463756859663,13.9693283001399));
#59198=CARTESIAN_POINT('Ctrl Pts',(-1.80732281357069,97.1558789228922,13.8965141110427));
#59199=CARTESIAN_POINT('Ctrl Pts',(-1.82758216206067,97.1652840075554,13.8225054486416));
#59200=CARTESIAN_POINT('Ctrl Pts',(-1.83573227138912,97.1690675679343,13.7927325914286));
#59201=CARTESIAN_POINT('Ctrl Pts',(-1.84316839547632,97.1728353129077,13.7627658324143));
#59202=CARTESIAN_POINT('Ctrl Pts',(-1.84988564919904,97.1765917986113,13.732639556223));
#59203=CARTESIAN_POINT('Ctrl Pts',(-1.86656155082962,97.1859174529121,13.6578496437082));
#59204=CARTESIAN_POINT('Ctrl Pts',(-1.87880762938304,97.1951749596988,13.5820800294758));
#59205=CARTESIAN_POINT('Ctrl Pts',(-1.88655046656516,97.2044368823206,13.5059217582517));
#59206=CARTESIAN_POINT('Ctrl Pts',(-1.88958729765734,97.2080695164481,13.4760515956046));
#59207=CARTESIAN_POINT('Ctrl Pts',(-1.89193160827013,97.21170290457,13.4461211222062));
#59208=CARTESIAN_POINT('Ctrl Pts',(-1.89357959499398,97.2153417120222,13.4161639224355));
#59209=CARTESIAN_POINT('Ctrl Pts',(-1.89753812082994,97.2240822638135,13.3442056065407));
#59210=CARTESIAN_POINT('Ctrl Pts',(-1.8974952294512,97.2328672457064,13.2720967317335));
#59211=CARTESIAN_POINT('Ctrl Pts',(-1.893392867159,97.2417399324394,13.2003539629298));
#59212=CARTESIAN_POINT('Ctrl Pts',(-1.89151844720891,97.2457939724873,13.167573806634));
#59213=CARTESIAN_POINT('Ctrl Pts',(-1.88879707332287,97.2498663790102,13.1348696186156));
#59214=CARTESIAN_POINT('Ctrl Pts',(-1.88522576936773,97.25396155984,13.1022881113543));
#59215=CARTESIAN_POINT('Ctrl Pts',(-1.88522410483544,97.2539634685436,13.1022729255927));
#59216=CARTESIAN_POINT('Ctrl Pts',(-1.88522244011855,97.2539653772521,13.1022577398576));
#59217=CARTESIAN_POINT('Ctrl Pts',(-1.88522077521706,97.2539672859656,13.1022425541492));
#59218=CARTESIAN_POINT('Ctrl Pts',(-1.87687837862261,97.2635313622859,13.0261508439112));
#59219=CARTESIAN_POINT('Ctrl Pts',(-1.8638092727973,97.2731792636298,12.9506111981236));
#59220=CARTESIAN_POINT('Ctrl Pts',(-1.84617669575997,97.2828313555678,12.8761466692974));
#59221=CARTESIAN_POINT('Ctrl Pts',(-1.83968311781548,97.2863859472303,12.8487234956451));
#59222=CARTESIAN_POINT('Ctrl Pts',(-1.83257078535585,97.2899410429422,12.8214466178707));
#59223=CARTESIAN_POINT('Ctrl Pts',(-1.82484856185339,97.2934924422361,12.7943437720108));
#59224=CARTESIAN_POINT('Ctrl Pts',(-1.7984871414283,97.3056158843839,12.7018225552653));
#59225=CARTESIAN_POINT('Ctrl Pts',(-1.76491926855089,97.3176303289924,12.6113148964554));
#59226=CARTESIAN_POINT('Ctrl Pts',(-1.72473579061861,97.3295963747473,12.5237921619917));
#59227=CARTESIAN_POINT('Ctrl Pts',(-1.71762473375568,97.3317139423688,12.5083037280981));
#59228=CARTESIAN_POINT('Ctrl Pts',(-1.71030639118383,97.3338300087006,12.4929086971463));
#59229=CARTESIAN_POINT('Ctrl Pts',(-1.70278389273608,97.3359449280349,12.4776123674558));
#59230=CARTESIAN_POINT('Ctrl Pts',(-1.66031859728433,97.3478838702648,12.3912629764724));
#59231=CARTESIAN_POINT('Ctrl Pts',(-1.61134955003944,97.3597875863096,12.3080614246423));
#59232=CARTESIAN_POINT('Ctrl Pts',(-1.55649372150675,97.3717254570158,12.2290167036105));
#59233=CARTESIAN_POINT('Ctrl Pts',(-1.54588844188208,97.3740334060588,12.2137349843873));
#59234=CARTESIAN_POINT('Ctrl Pts',(-1.53506310234205,97.3763426521225,12.1986084810493));
#59235=CARTESIAN_POINT('Ctrl Pts',(-1.5240220999447,97.3786537257481,12.1836442710473));
#59236=CARTESIAN_POINT('Ctrl Pts',(-1.47226273355685,97.3894878603888,12.1134932104529));
#59237=CARTESIAN_POINT('Ctrl Pts',(-1.41576587561513,97.4003622125247,12.0469156908551));
#59238=CARTESIAN_POINT('Ctrl Pts',(-1.35502721013357,97.4113207002559,11.9846684462004));
#59239=CARTESIAN_POINT('Ctrl Pts',(-1.35501170563695,97.4113234975817,11.9846525566152));
#59240=CARTESIAN_POINT('Ctrl Pts',(-1.35499620086394,97.4113262949131,11.984636667312));
#59241=CARTESIAN_POINT('Ctrl Pts',(-1.35498069581462,97.4113290922499,11.9846207782906));
#59242=CARTESIAN_POINT('Ctrl Pts',(-1.30684848055419,97.4200128451833,11.9352966012336));
#59243=CARTESIAN_POINT('Ctrl Pts',(-1.25605103493076,97.4287735162158,11.8886525756439));
#59244=CARTESIAN_POINT('Ctrl Pts',(-1.20286240990663,97.4375040172174,11.8449521299479));
#59245=CARTESIAN_POINT('Ctrl Pts',(-1.17363121677151,97.4423020912572,11.8209354126959));
#59246=CARTESIAN_POINT('Ctrl Pts',(-1.14367848326735,97.4470909336674,11.7978083966171));
#59247=CARTESIAN_POINT('Ctrl Pts',(-1.11305514292375,97.4518519102943,11.7756186034057));
#59248=CARTESIAN_POINT('Ctrl Pts',(-1.0427806679806,97.4627774046693,11.7246974416535));
#59249=CARTESIAN_POINT('Ctrl Pts',(-0.968948674937127,97.473558584887,11.6786916139904));
#59250=CARTESIAN_POINT('Ctrl Pts',(-0.892307937823509,97.4842721205025,
11.6378968881267));
#59251=CARTESIAN_POINT('Ctrl Pts',(-0.877548503559858,97.486335327755,11.6300406605203));
#59252=CARTESIAN_POINT('Ctrl Pts',(-0.862684747866399,97.4883960428806,
11.6223777104206));
#59253=CARTESIAN_POINT('Ctrl Pts',(-0.847721802037244,97.4904548370641,
11.6149101853474));
#59254=CARTESIAN_POINT('Ctrl Pts',(-0.767217209046669,97.5015316924966,
11.5747329319161));
#59255=CARTESIAN_POINT('Ctrl Pts',(-0.683844767705889,97.5125542163153,
11.5402139510128));
#59256=CARTESIAN_POINT('Ctrl Pts',(-0.598493168821003,97.5236103165967,
11.5117148396435));
#59257=CARTESIAN_POINT('Ctrl Pts',(-0.584963917182092,97.5253628410345,
11.5071973888372));
#59258=CARTESIAN_POINT('Ctrl Pts',(-0.571384857853042,97.5271162232202,
11.5028311238124));
#59259=CARTESIAN_POINT('Ctrl Pts',(-0.557759436969811,97.5288708291123,
11.4986174116286));
#59260=CARTESIAN_POINT('Ctrl Pts',(-0.482749928213787,97.538530136311,11.4754204415196));
#59261=CARTESIAN_POINT('Ctrl Pts',(-0.406348656347312,97.548273372566,11.4568046119093));
#59262=CARTESIAN_POINT('Ctrl Pts',(-0.329170500018915,97.5580590483754,
11.4430879578146));
#59263=CARTESIAN_POINT('Ctrl Pts',(-0.303898273917259,97.5612633981989,
11.438596396988));
#59264=CARTESIAN_POINT('Ctrl Pts',(-0.278542947167168,97.5644722821677,
11.4346297942812));
#59265=CARTESIAN_POINT('Ctrl Pts',(-0.253126614249737,97.5676841957192,
11.4311981944688));
#59266=CARTESIAN_POINT('Ctrl Pts',(-0.253114077490711,97.5676857800149,
11.4311965018116));
#59267=CARTESIAN_POINT('Ctrl Pts',(-0.253101540716823,97.5676873643113,
11.4311948092845));
#59268=CARTESIAN_POINT('Ctrl Pts',(-0.253089003928123,97.5676889486084,
11.4311931168876));
#59269=CARTESIAN_POINT('Ctrl Pts',(-0.18397673825891,97.5764227932723,11.4218633443996));
#59270=CARTESIAN_POINT('Ctrl Pts',(-0.114340807000573,97.5852839143722,
11.4163857723326));
#59271=CARTESIAN_POINT('Ctrl Pts',(-0.0445872863122623,97.5941519362418,
11.4147926072362));
#59272=CARTESIAN_POINT('Ctrl Pts',(-0.00519438737967313,97.5991601005007,
11.4138928764268));
#59273=CARTESIAN_POINT('Ctrl Pts',(0.0342350496797649,97.6041703463226,
11.4142320296684));
#59274=CARTESIAN_POINT('Ctrl Pts',(0.0736206917584265,97.6091600813032,
11.4158147843246));
#59275=CARTESIAN_POINT('Ctrl Pts',(0.177736982277446,97.6223504895189,11.4199988101501));
#59276=CARTESIAN_POINT('Ctrl Pts',(0.281593113412828,97.6354011413811,11.4328737201666));
#59277=CARTESIAN_POINT('Ctrl Pts',(0.383794535932431,97.6483864558369,11.4541011665343));
#59278=CARTESIAN_POINT('Ctrl Pts',(0.393982852748109,97.6496809436666,11.4562173009623));
#59279=CARTESIAN_POINT('Ctrl Pts',(0.404154754370905,97.6509747868019,11.4584164723396));
#59280=CARTESIAN_POINT('Ctrl Pts',(0.414308876944704,97.6522680620147,11.4606983671469));
#59281=CARTESIAN_POINT('Ctrl Pts',(0.51538101755854,97.6651410693294,11.483411899622));
#59282=CARTESIAN_POINT('Ctrl Pts',(0.614688302321226,97.6779592698353,11.5143213288823));
#59283=CARTESIAN_POINT('Ctrl Pts',(0.710802678033256,97.690801715761,11.5530729741079));
#59284=CARTESIAN_POINT('Ctrl Pts',(0.721563481973412,97.6922395344192,11.5574115431674));
#59285=CARTESIAN_POINT('Ctrl Pts',(0.732284315605942,97.6936776633208,11.5618483986565));
#59286=CARTESIAN_POINT('Ctrl Pts',(0.742963214249548,97.695116218159,11.5663830364405));
#59287=CARTESIAN_POINT('Ctrl Pts',(0.816089918146439,97.7049671191933,11.5974352194021));
#59288=CARTESIAN_POINT('Ctrl Pts',(0.887244901022521,97.7148378563862,11.6330726003644));
#59289=CARTESIAN_POINT('Ctrl Pts',(0.955770879025923,97.7247576167201,11.6731072941802));
#59290=CARTESIAN_POINT('Ctrl Pts',(0.955778057190901,97.7247586558249,11.6731114878545));
#59291=CARTESIAN_POINT('Ctrl Pts',(0.95578523532708,97.7247596949303,11.6731156815771));
#59292=CARTESIAN_POINT('Ctrl Pts',(0.955792413434416,97.7247607340362,11.673119875348));
#59293=CARTESIAN_POINT('Ctrl Pts',(0.961320102867578,97.7255609247558,11.676349398341));
#59294=CARTESIAN_POINT('Ctrl Pts',(0.966831261423941,97.7263615109594,11.6796078576718));
#59295=CARTESIAN_POINT('Ctrl Pts',(0.972325610934361,97.7271624022525,11.6828950646503));
#59296=CARTESIAN_POINT('Ctrl Pts',(1.0576495049121,97.7395997551455,11.7339433824157));
#59297=CARTESIAN_POINT('Ctrl Pts',(1.13891370374107,97.7521106981753,11.7919244505447));
#59298=CARTESIAN_POINT('Ctrl Pts',(1.21522114079168,97.7646330653377,11.85591814004));
#59299=CARTESIAN_POINT('Ctrl Pts',(1.22860955846217,97.766830160251,11.8671460658669));
#59300=CARTESIAN_POINT('Ctrl Pts',(1.24184538597427,97.7690275976935,11.8785589546342));
#59301=CARTESIAN_POINT('Ctrl Pts',(1.25492378700352,97.771225030318,11.8901516736471));
#59302=CARTESIAN_POINT('Ctrl Pts',(1.34365338452769,97.7861333751475,11.9688017540295));
#59303=CARTESIAN_POINT('Ctrl Pts',(1.42513893512118,97.8010402883418,12.0557330915253));
#59304=CARTESIAN_POINT('Ctrl Pts',(1.49795370519445,97.8158551547241,12.1494019687695));
#59305=CARTESIAN_POINT('Ctrl Pts',(1.54737741727755,97.8259108850367,12.2129806028214));
#59306=CARTESIAN_POINT('Ctrl Pts',(1.59280836790521,97.8359245255454,12.2796639253639));
#59307=CARTESIAN_POINT('Ctrl Pts',(1.6338115478498,97.8458777775162,12.3489859331239));
#59308=CARTESIAN_POINT('Ctrl Pts',(1.67374319894691,97.8555709229141,12.4164963611191));
#59309=CARTESIAN_POINT('Ctrl Pts',(1.70948069097325,97.8652096736894,12.4865223985512));
#59310=CARTESIAN_POINT('Ctrl Pts',(1.74067678353583,97.8749187713275,12.5585082030784));
#59311=CARTESIAN_POINT('Ctrl Pts',(1.74800334055896,97.8771990010501,12.5754144262109));
#59312=CARTESIAN_POINT('Ctrl Pts',(1.75507959183736,97.879483136023,12.5924288752536));
#59313=CARTESIAN_POINT('Ctrl Pts',(1.7619013630991,97.8817728379105,12.6095446057079));
#59314=CARTESIAN_POINT('Ctrl Pts',(1.76190587693937,97.881774352964,12.6095559308711));
#59315=CARTESIAN_POINT('Ctrl Pts',(1.76191039066822,97.88177586802,12.6095672560787));
#59316=CARTESIAN_POINT('Ctrl Pts',(1.76191490428566,97.8817773830784,12.6095785813307));
#59317=CARTESIAN_POINT('Ctrl Pts',(1.79316542671293,97.8922670550735,12.6879901979561));
#59318=CARTESIAN_POINT('Ctrl Pts',(1.81910715435611,97.9028856558508,12.7686162639768));
#59319=CARTESIAN_POINT('Ctrl Pts',(1.83960776096729,97.9135411552663,12.8506684014478));
#59320=CARTESIAN_POINT('Ctrl Pts',(1.84804109783546,97.9179245092701,12.884422198551));
#59321=CARTESIAN_POINT('Ctrl Pts',(1.85555397315441,97.9223140597097,12.9184167872872));
#59322=CARTESIAN_POINT('Ctrl Pts',(1.86213869323708,97.9267032033215,12.9525952536877));
#59323=CARTESIAN_POINT('Ctrl Pts',(1.88122198474518,97.939423456569,13.0516484601161));
#59324=CARTESIAN_POINT('Ctrl Pts',(1.8925131317968,97.9521388029293,13.1522571128828));
#59325=CARTESIAN_POINT('Ctrl Pts',(1.89585194995449,97.9647097334425,13.2532002880244));
#59326=CARTESIAN_POINT('Ctrl Pts',(1.89908136035533,97.9768687345711,13.3508357159814));
#59327=CARTESIAN_POINT('Ctrl Pts',(1.89487040675864,97.9888961908162,13.4488127390259));
#59328=CARTESIAN_POINT('Ctrl Pts',(1.88321720173359,98.0009377480042,13.5459564284894));
#59329=CARTESIAN_POINT('Ctrl Pts',(1.88062458085643,98.003616769998,13.5675690884268));
#59330=CARTESIAN_POINT('Ctrl Pts',(1.87766353102134,98.0062965178051,13.5891406967765));
#59331=CARTESIAN_POINT('Ctrl Pts',(1.87433391400233,98.0089786424861,13.6106586388472));
#59332=CARTESIAN_POINT('Ctrl Pts',(1.86188033756779,98.0190104402967,13.6911409690258));
#59333=CARTESIAN_POINT('Ctrl Pts',(1.84426925603202,98.0290755093867,13.7708615208926));
#59334=CARTESIAN_POINT('Ctrl Pts',(1.82153079495272,98.0392443933049,13.8490694515221));
#59335=CARTESIAN_POINT('Ctrl Pts',(1.82153060951391,98.0392444762351,13.8490700893307));
#59336=CARTESIAN_POINT('Ctrl Pts',(1.82153042407478,98.0392445591653,13.8490707271391));
#59337=CARTESIAN_POINT('Ctrl Pts',(1.82153023863529,98.0392446420956,13.8490713649475));
#59338=CARTESIAN_POINT('Ctrl Pts',(1.79669839808222,98.0503496690028,13.9344790411315));
#59339=CARTESIAN_POINT('Ctrl Pts',(1.76573754278492,98.061598231716,14.0181644050579));
#59340=CARTESIAN_POINT('Ctrl Pts',(1.72905504094309,98.072828361964,14.0993655503024));
#59341=CARTESIAN_POINT('Ctrl Pts',(1.71735742975068,98.0764095162116,14.1252596245274));
#59342=CARTESIAN_POINT('Ctrl Pts',(1.70507822047769,98.079988746162,14.1509007561787));
#59343=CARTESIAN_POINT('Ctrl Pts',(1.69223134657825,98.0835606620397,14.1762634153602));
#59344=CARTESIAN_POINT('Ctrl Pts',(1.63960277065782,98.0981933927275,14.2801642277076));
#59345=CARTESIAN_POINT('Ctrl Pts',(1.57742320284422,98.112709580116,14.3794469289553));
#59346=CARTESIAN_POINT('Ctrl Pts',(1.50679347614601,98.1271985721253,14.472525352511));
#59347=CARTESIAN_POINT('Ctrl Pts',(1.4994630010331,98.1287023468148,14.4821857193186));
#59348=CARTESIAN_POINT('Ctrl Pts',(1.49204145614255,98.130205832455,14.4917792536687));
#59349=CARTESIAN_POINT('Ctrl Pts',(1.48453004020065,98.1317091316073,14.5013041789783));
#59350=CARTESIAN_POINT('Ctrl Pts',(1.41674058875893,98.1452761908243,14.5872652636464));
#59351=CARTESIAN_POINT('Ctrl Pts',(1.34163048417663,98.1588298766215,14.667634774901));
#59352=CARTESIAN_POINT('Ctrl Pts',(1.26017484902886,98.1724340366167,14.7410255875902));
#59353=CARTESIAN_POINT('Ctrl Pts',(1.24631731984343,98.1747484258401,14.7535110998195));
#59354=CARTESIAN_POINT('Ctrl Pts',(1.23227618425927,98.1770642830045,14.765794746951));
#59355=CARTESIAN_POINT('Ctrl Pts',(1.21805629252046,98.1793819310667,14.7778698418999));
#59356=CARTESIAN_POINT('Ctrl Pts',(1.18028855227559,98.1855375566931,14.8099410459457));
#59357=CARTESIAN_POINT('Ctrl Pts',(1.14126131994144,98.1917053619478,14.8405392166875));
#59358=CARTESIAN_POINT('Ctrl Pts',(1.10107288945578,98.1978892643502,14.8695362388996));
#59359=CARTESIAN_POINT('Ctrl Pts',(1.10107163047069,98.1978894580737,14.8695371472908));
#59360=CARTESIAN_POINT('Ctrl Pts',(1.10107037148441,98.1978896517971,14.8695380556806));
#59361=CARTESIAN_POINT('Ctrl Pts',(1.10106911249695,98.1978898455206,14.8695389640687));
#59362=CARTESIAN_POINT('Ctrl Pts',(1.08999497411366,98.1995938503551,14.877529207575));
#59363=CARTESIAN_POINT('Ctrl Pts',(1.07883106803453,98.2012995077411,14.8853991677259));
#59364=CARTESIAN_POINT('Ctrl Pts',(1.06758025653102,98.2030060995129,14.893147481334));
#59365=CARTESIAN_POINT('Ctrl Pts',(0.966358762533452,98.2183599936496,14.9628576421641));
#59366=CARTESIAN_POINT('Ctrl Pts',(0.8581056922415,98.2337880700468,15.0227161239156));
#59367=CARTESIAN_POINT('Ctrl Pts',(0.745006988691363,98.2492258523374,15.0719571136518));
#59368=CARTESIAN_POINT('Ctrl Pts',(0.631369164669553,98.2647372236631,15.1214328260222));
#59369=CARTESIAN_POINT('Ctrl Pts',(0.512840164194871,98.280257780815,15.1601937414373));
#59370=CARTESIAN_POINT('Ctrl Pts',(0.391584713061079,98.2957470338434,15.1874950289018));
#59371=CARTESIAN_POINT('Ctrl Pts',(0.318389028749424,98.3050970998759,15.2039754130814));
#59372=CARTESIAN_POINT('Ctrl Pts',(0.244198641903657,98.3144362830383,15.2162803197437));
#59373=CARTESIAN_POINT('Ctrl Pts',(0.169480875927792,98.3237613047438,15.2242422448514));
#59374=CARTESIAN_POINT('Ctrl Pts',(0.0861780938318283,98.3341577645554,
15.2331189892728));
#59375=CARTESIAN_POINT('Ctrl Pts',(0.00220769556974054,98.3445394959874,
15.236594405874));
#59376=CARTESIAN_POINT('Ctrl Pts',(-0.0816538360917527,98.3549879395243,
15.2344770340646));
#59377=CARTESIAN_POINT('Ctrl Pts',(-0.0895298655725071,98.355969226745,
15.2342781767046));
#59378=CARTESIAN_POINT('Ctrl Pts',(-0.0974049476914433,98.3569511040135,
15.234030024446));
#59379=CARTESIAN_POINT('Ctrl Pts',(-0.105278447982589,98.3579336397859,
15.2337324409201));
#59380=CARTESIAN_POINT('Ctrl Pts',(-0.105280137831452,98.3579338506625,
15.2337323770513));
#59381=CARTESIAN_POINT('Ctrl Pts',(-0.105281827680237,98.3579340615391,
15.2337323131802));
#59382=CARTESIAN_POINT('Ctrl Pts',(-0.105283517529021,98.3579342724158,
15.2337322493068));
#59383=CARTESIAN_POINT('Ctrl Pts',(-0.196236757805741,98.3692843519231,
15.230294373682));
#59384=CARTESIAN_POINT('Ctrl Pts',(-0.287078604914497,98.380764542737,15.2202640739733));
#59385=CARTESIAN_POINT('Ctrl Pts',(-0.376875246424487,98.3922550241297,
15.2039088174115));
#59386=CARTESIAN_POINT('Ctrl Pts',(-0.387994247358728,98.393677824261,15.2018836401896));
#59387=CARTESIAN_POINT('Ctrl Pts',(-0.399097201379292,98.3951007782829,
15.1997615477108));
#59388=CARTESIAN_POINT('Ctrl Pts',(-0.410182320594743,98.3965236554648,
15.1975431005546));
#59389=CARTESIAN_POINT('Ctrl Pts',(-0.458552898082515,98.4027324647383,
15.1878627743453));
#59390=CARTESIAN_POINT('Ctrl Pts',(-0.50658797540966,98.4089401094051,15.1763470910284));
#59391=CARTESIAN_POINT('Ctrl Pts',(-0.55415873369442,98.4151299300796,15.1630371011503));
#59392=CARTESIAN_POINT('Ctrl Pts',(-0.653347259642252,98.4280361609391,
15.1352847943973));
#59393=CARTESIAN_POINT('Ctrl Pts',(-0.750534462141843,98.4408656260839,
15.0997304289456));
#59394=CARTESIAN_POINT('Ctrl Pts',(-0.844558781017521,98.4536866342342,
15.0567776350573));
#59395=CARTESIAN_POINT('Ctrl Pts',(-0.938273398623484,98.4664654120068,
15.0139663208943));
#59396=CARTESIAN_POINT('Ctrl Pts',(-1.0288433211155,98.4792371418048,14.963798187976));
#59397=CARTESIAN_POINT('Ctrl Pts',(-1.11497562087733,98.4920574584708,14.9067308503489));
#59398=CARTESIAN_POINT('Ctrl Pts',(-1.17676837065842,98.5012549676751,14.865789789627));
#59399=CARTESIAN_POINT('Ctrl Pts',(-1.23627335466819,98.5104772704496,14.8212989097111));
#59400=CARTESIAN_POINT('Ctrl Pts',(-1.29298640342411,98.5197355057998,14.7734746819127));
#59401=CARTESIAN_POINT('Ctrl Pts',(-1.29298818097518,98.5197357959797,14.773473182963));
#59402=CARTESIAN_POINT('Ctrl Pts',(-1.29298995852352,98.5197360861597,14.7734716840101));
#59403=CARTESIAN_POINT('Ctrl Pts',(-1.29299173606918,98.5197363763397,14.7734701850538));
#59404=CARTESIAN_POINT('Ctrl Pts',(-1.38337910074375,98.5344918958645,14.6972489603198));
#59405=CARTESIAN_POINT('Ctrl Pts',(-1.46678149799099,98.5494536768941,14.6125203526301));
#59406=CARTESIAN_POINT('Ctrl Pts',(-1.54211853187568,98.5643546623537,14.5208660303085));
#59407=CARTESIAN_POINT('Ctrl Pts',(-1.5486717060631,98.565650821072,14.5128935006211));
#59408=CARTESIAN_POINT('Ctrl Pts',(-1.55516409110504,98.5669465796977,14.5048682835478));
#59409=CARTESIAN_POINT('Ctrl Pts',(-1.56159508914682,98.5682417993886,14.4967912458765));
#59410=CARTESIAN_POINT('Ctrl Pts',(-1.63616755869191,98.5832608882342,14.4031316549639));
#59411=CARTESIAN_POINT('Ctrl Pts',(-1.70250070767046,98.5982088276308,14.3024918863326));
#59412=CARTESIAN_POINT('Ctrl Pts',(-1.75950459074744,98.6131622539348,14.1964906056999));
#59413=CARTESIAN_POINT('Ctrl Pts',(-1.80886624811544,98.6261109491088,14.1047003869863));
#59414=CARTESIAN_POINT('Ctrl Pts',(-1.85122540847539,98.6390647369957,14.0088871266353));
#59415=CARTESIAN_POINT('Ctrl Pts',(-1.88581619914007,98.6520550379284,13.9102265519788));
#59416=CARTESIAN_POINT('Ctrl Pts',(-1.89079028899205,98.6539230184747,13.8960393491494));
#59417=CARTESIAN_POINT('Ctrl Pts',(-1.89560382633042,98.655791755085,13.8817933042435));
#59418=CARTESIAN_POINT('Ctrl Pts',(-1.90025461792823,98.657661342201,13.8674919433306));
#59419=CARTESIAN_POINT('Ctrl Pts',(-1.92176803375755,98.6663095914743,13.8013373720549));
#59420=CARTESIAN_POINT('Ctrl Pts',(-1.93979592581145,98.6749753880474,13.7340024237611));
#59421=CARTESIAN_POINT('Ctrl Pts',(-1.95412537357618,98.6836614942994,13.6658673102719));
#59422=CARTESIAN_POINT('Ctrl Pts',(-1.95412619333049,98.6836619912113,13.6658634124208));
#59423=CARTESIAN_POINT('Ctrl Pts',(-1.95412701307277,98.6836624881233,13.6658595145669));
#59424=CARTESIAN_POINT('Ctrl Pts',(-1.954127832803,98.6836629850355,13.66585561671));
#59425=CARTESIAN_POINT('Ctrl Pts',(-1.95869657896549,98.6864325124844,13.6441310082917));
#59426=CARTESIAN_POINT('Ctrl Pts',(-1.9628912897172,98.6892056382613,13.6223172263087));
#59427=CARTESIAN_POINT('Ctrl Pts',(-1.96671237321969,98.6919808767534,13.600427835094));
#59428=CARTESIAN_POINT('Ctrl Pts',(-1.98732041921042,98.7069484225933,13.4823729481577));
#59429=CARTESIAN_POINT('Ctrl Pts',(-1.99705812785772,98.7219762330531,13.3621230330987));
#59430=CARTESIAN_POINT('Ctrl Pts',(-1.99607641639472,98.737030524678,13.2416925988717));
#59431=CARTESIAN_POINT('Ctrl Pts',(-1.99508560520575,98.7522243582495,13.1201458652111));
#59432=CARTESIAN_POINT('Ctrl Pts',(-1.98317976262498,98.7674451627657,12.9984139576203));
#59433=CARTESIAN_POINT('Ctrl Pts',(-1.96051531540606,98.7826761714344,12.8784999684021));
#59434=CARTESIAN_POINT('Ctrl Pts',(-1.94328165112652,98.7942575741265,12.7873193888519));
#59435=CARTESIAN_POINT('Ctrl Pts',(-1.91982766407115,98.8058452838051,12.6971879433377));
#59436=CARTESIAN_POINT('Ctrl Pts',(-1.89020449960675,98.817438351822,12.6089713671772));
#59437=CARTESIAN_POINT('Ctrl Pts',(-1.86337948525766,98.8279363597669,12.5290875679911));
#59438=CARTESIAN_POINT('Ctrl Pts',(-1.83148685794366,98.8384408144044,12.4507650277481));
#59439=CARTESIAN_POINT('Ctrl Pts',(-1.79462643332624,98.8489816702695,12.374765893803));
#59440=CARTESIAN_POINT('Ctrl Pts',(-1.79345888505005,98.8493155502565,12.3723586329331));
#59441=CARTESIAN_POINT('Ctrl Pts',(-1.79228636127879,98.8496494649769,12.3699537110507));
#59442=CARTESIAN_POINT('Ctrl Pts',(-1.79110886665425,98.8499834152402,12.3675511530638));
#59443=CARTESIAN_POINT('Ctrl Pts',(-1.79110633219145,98.8499841340413,12.3675459817503));
#59444=CARTESIAN_POINT('Ctrl Pts',(-1.79110379770541,98.8499848528427,12.3675408104473));
#59445=CARTESIAN_POINT('Ctrl Pts',(-1.79110126319609,98.8499855716444,12.3675356391548));
#59446=CARTESIAN_POINT('Ctrl Pts',(-1.74887751576844,98.8619604724573,12.2813843088857));
#59447=CARTESIAN_POINT('Ctrl Pts',(-1.700191678123,98.8739967806476,12.1981396898583));
#59448=CARTESIAN_POINT('Ctrl Pts',(-1.645748687921,98.8860580721743,12.1186180955533));
#59449=CARTESIAN_POINT('Ctrl Pts',(-1.63299796783116,98.888882864707,12.0999938872518));
#59450=CARTESIAN_POINT('Ctrl Pts',(-1.61993166374205,98.8917090258783,12.0815737899685));
#59451=CARTESIAN_POINT('Ctrl Pts',(-1.60655918315871,98.8945360847195,12.0633680814703));
#59452=CARTESIAN_POINT('Ctrl Pts',(-1.53875885600299,98.9088696642773,11.9710626199226));
#59453=CARTESIAN_POINT('Ctrl Pts',(-1.46309077473602,98.9232257701794,11.884264458137));
#59454=CARTESIAN_POINT('Ctrl Pts',(-1.38062901541154,98.9375749952128,11.8041346915348));
#59455=CARTESIAN_POINT('Ctrl Pts',(-1.37606804181495,98.9383686532313,11.7997027008428));
#59456=CARTESIAN_POINT('Ctrl Pts',(-1.37148627429814,98.9391622901798,11.7952911180463));
#59457=CARTESIAN_POINT('Ctrl Pts',(-1.36688389103222,98.9399559010773,11.7909001425279));
#59458=CARTESIAN_POINT('Ctrl Pts',(-1.35817186874008,98.9414581566329,11.7825883018162));
#59459=CARTESIAN_POINT('Ctrl Pts',(-1.34938582819855,98.9429603522622,11.7743501579612));
#59460=CARTESIAN_POINT('Ctrl Pts',(-1.34052686707804,98.9444624762572,11.7661869849063));
#59461=CARTESIAN_POINT('Ctrl Pts',(-1.25172850800733,98.9595191114618,11.6843629016738));
#59462=CARTESIAN_POINT('Ctrl Pts',(-1.1555785484111,98.9745726509216,11.6100489305369));
#59463=CARTESIAN_POINT('Ctrl Pts',(-1.05335786448829,98.9896624341179,11.5447106820709));
#59464=CARTESIAN_POINT('Ctrl Pts',(-0.987469521576181,98.9993888492773,
11.5025956349493));
#59465=CARTESIAN_POINT('Ctrl Pts',(-0.919064266961413,99.0091293501279,
11.4642171790027));
#59466=CARTESIAN_POINT('Ctrl Pts',(-0.848573143922676,99.0188824801348,
11.4299952775465));
#59467=CARTESIAN_POINT('Ctrl Pts',(-0.848567958395836,99.0188831976027,
11.4299927600864));
#59468=CARTESIAN_POINT('Ctrl Pts',(-0.84856277285726,99.0188839150707,11.4299902426485));
#59469=CARTESIAN_POINT('Ctrl Pts',(-0.848557587307047,99.018884632539,11.429987725233));
#59470=CARTESIAN_POINT('Ctrl Pts',(-0.748837726886114,99.0326817855019,
11.3815769847876));
#59471=CARTESIAN_POINT('Ctrl Pts',(-0.644794435651932,99.0465373107453,
11.3414081760795));
#59472=CARTESIAN_POINT('Ctrl Pts',(-0.537965648557116,99.0604173137764,
11.3097658392848));
#59473=CARTESIAN_POINT('Ctrl Pts',(-0.527140572212493,99.0618237894704,
11.3065594871317));
#59474=CARTESIAN_POINT('Ctrl Pts',(-0.516286909372726,99.0632305162845,
11.3034406432814));
#59475=CARTESIAN_POINT('Ctrl Pts',(-0.505406268621373,99.0646374588121,
11.3004095754447));
#59476=CARTESIAN_POINT('Ctrl Pts',(-0.484768089040163,99.0673061189774,
11.2946603072017));
#59477=CARTESIAN_POINT('Ctrl Pts',(-0.464031602062175,99.0699757227276,
11.2892264770465));
#59478=CARTESIAN_POINT('Ctrl Pts',(-0.443206192442698,99.0726462392845,
11.2841096394152));
#59479=CARTESIAN_POINT('Ctrl Pts',(-0.324308376627887,99.0878929302988,
11.25489624917));
#59480=CARTESIAN_POINT('Ctrl Pts',(-0.202497790263523,99.1031711376377,
11.2360127819059));
#59481=CARTESIAN_POINT('Ctrl Pts',(-0.0797155686824385,99.1184889367771,
11.2278125167363));
#59482=CARTESIAN_POINT('Ctrl Pts',(-0.0726784790510279,99.1193668548023,
11.2273425301188));
#59483=CARTESIAN_POINT('Ctrl Pts',(-0.065638240207429,99.1202448976162,
11.2269076377068));
#59484=CARTESIAN_POINT('Ctrl Pts',(-0.0585952329236468,99.1211230648279,
11.2265079049832));
#59485=CARTESIAN_POINT('Ctrl Pts',(0.062732712974499,99.1362510094189,11.2196218194921));
#59486=CARTESIAN_POINT('Ctrl Pts',(0.184890897368926,99.1514171321329,11.2231670003939));
#59487=CARTESIAN_POINT('Ctrl Pts',(0.306055934128646,99.166611611458,11.237487058001));
#59488=CARTESIAN_POINT('Ctrl Pts',(0.314699380078351,99.1676955269529,11.2385085956264));
#59489=CARTESIAN_POINT('Ctrl Pts',(0.32333772377812,99.1687795796955,11.2395849710132));
#59490=CARTESIAN_POINT('Ctrl Pts',(0.33197028002139,99.1698637627013,11.2407163092596));
#59491=CARTESIAN_POINT('Ctrl Pts',(0.386420873240079,99.1767023405413,11.2478523228468));
#59492=CARTESIAN_POINT('Ctrl Pts',(0.440642990526318,99.1835463287813,11.2571762344221));
#59493=CARTESIAN_POINT('Ctrl Pts',(0.494433566894493,99.1903909774577,11.2687102385151));
#59494=CARTESIAN_POINT('Ctrl Pts',(0.494434332164162,99.1903910748354,11.2687104026075));
#59495=CARTESIAN_POINT('Ctrl Pts',(0.494435097433744,99.1903911722131,11.2687105667003));
#59496=CARTESIAN_POINT('Ctrl Pts',(0.494435862703259,99.1903912695907,11.2687107307936));
#59497=CARTESIAN_POINT('Ctrl Pts',(0.583481658251176,99.2017220150766,11.2878044172989));
#59498=CARTESIAN_POINT('Ctrl Pts',(0.671484670266375,99.213075632491,11.3129866647636));
#59499=CARTESIAN_POINT('Ctrl Pts',(0.757644214645959,99.2244520508583,11.3438670371024));
#59500=CARTESIAN_POINT('Ctrl Pts',(0.785045848831569,99.2280701346897,11.3536880345605));
#59501=CARTESIAN_POINT('Ctrl Pts',(0.812261106649497,99.2316905230872,11.364084980821));
#59502=CARTESIAN_POINT('Ctrl Pts',(0.839264541734818,99.2353132089604,11.375044266686));
#59503=CARTESIAN_POINT('Ctrl Pts',(0.920341263355562,99.246190176766,11.4079490792193));
#59504=CARTESIAN_POINT('Ctrl Pts',(0.999515454592334,99.2570889340257,11.445924826957));
#59505=CARTESIAN_POINT('Ctrl Pts',(1.0761967882515,99.2680232652008,11.4886436863882));
#59506=CARTESIAN_POINT('Ctrl Pts',(1.17263218746403,99.2817744161221,11.5423674554799));
#59507=CARTESIAN_POINT('Ctrl Pts',(1.26515178344775,99.2955859302042,11.6036043442725));
#59508=CARTESIAN_POINT('Ctrl Pts',(1.3526095427359,99.3094356944523,11.6717679947235));
#59509=CARTESIAN_POINT('Ctrl Pts',(1.36154320244813,99.3108504240532,11.6787307943976));
#59510=CARTESIAN_POINT('Ctrl Pts',(1.37042401857231,99.3122655531071,11.6857659057565));
#59511=CARTESIAN_POINT('Ctrl Pts',(1.37925074973229,99.313681058288,11.6928727277097));
#59512=CARTESIAN_POINT('Ctrl Pts',(1.45913776652313,99.3264921980074,11.757193572473));
#59513=CARTESIAN_POINT('Ctrl Pts',(1.53459254995152,99.3393338010028,11.8273923622317));
#59514=CARTESIAN_POINT('Ctrl Pts',(1.60458603251227,99.352165974687,11.9029059606615));
#59515=CARTESIAN_POINT('Ctrl Pts',(1.61693751847119,99.3544304199937,11.9162315606544));
#59516=CARTESIAN_POINT('Ctrl Pts',(1.62911902663242,99.3566945718676,11.9297225692549));
#59517=CARTESIAN_POINT('Ctrl Pts',(1.64112502549409,99.3589582113924,11.9433757736953));
#59518=CARTESIAN_POINT('Ctrl Pts',(1.65216477562623,99.3610396720882,11.9559301614861));
#59519=CARTESIAN_POINT('Ctrl Pts',(1.6630558483895,99.3631206503809,11.9686213732987));
#59520=CARTESIAN_POINT('Ctrl Pts',(1.67379374264166,99.365200932442,11.9814465471939));
#59521=CARTESIAN_POINT('Ctrl Pts',(1.67380835861525,99.3652037640351,11.9814640042854));
#59522=CARTESIAN_POINT('Ctrl Pts',(1.67382297430502,99.3652065956269,11.9814814616252));
#59523=CARTESIAN_POINT('Ctrl Pts',(1.67383758971101,99.3652094272175,11.9814989192131));
#59524=CARTESIAN_POINT('Ctrl Pts',(1.67768434523775,99.3659546981063,11.9860937332597));
#59525=CARTESIAN_POINT('Ctrl Pts',(1.68151185425506,99.3666999811197,11.9907062370342));
#59526=CARTESIAN_POINT('Ctrl Pts',(1.68532000044771,99.3674452826907,11.9953362194907));
#59527=CARTESIAN_POINT('Ctrl Pts',(1.74387883110136,99.3789059741336,12.0665326349854));
#59528=CARTESIAN_POINT('Ctrl Pts',(1.79784641496243,99.3903686577716,12.1418534154281));
#59529=CARTESIAN_POINT('Ctrl Pts',(1.84681756557283,99.401863028944,12.2205000922566));
#59530=CARTESIAN_POINT('Ctrl Pts',(1.86205035663532,99.4054384269545,12.24496364643));
#59531=CARTESIAN_POINT('Ctrl Pts',(1.87679999799802,99.4090168869979,12.2697487469405));
#59532=CARTESIAN_POINT('Ctrl Pts',(1.8910551057942,99.4125992916037,12.294830743662));
#59533=CARTESIAN_POINT('Ctrl Pts',(1.95110900255702,99.4276912403589,12.4004961418657));
#59534=CARTESIAN_POINT('Ctrl Pts',(2.00238675861918,99.4428738848819,12.5114282785142));
#59535=CARTESIAN_POINT('Ctrl Pts',(2.04421079468902,99.4580904602187,12.6260585904732));
#59536=CARTESIAN_POINT('Ctrl Pts',(2.05297957054067,99.4612807486484,12.6500918403894));
#59537=CARTESIAN_POINT('Ctrl Pts',(2.06133304005819,99.4644726596183,12.6742887381014));
#59538=CARTESIAN_POINT('Ctrl Pts',(2.06926498832166,99.4676664859055,12.6986365937338));
#59539=CARTESIAN_POINT('Ctrl Pts',(2.10723158690889,99.4829538675894,12.8151786122328));
#59540=CARTESIAN_POINT('Ctrl Pts',(2.13552515695722,99.4984499739216,12.9352164099709));
#59541=CARTESIAN_POINT('Ctrl Pts',(2.15337815930707,99.5139729306774,13.057151698573));
#59542=CARTESIAN_POINT('Ctrl Pts',(2.16485500934828,99.5239519047116,13.1355381231415));
#59543=CARTESIAN_POINT('Ctrl Pts',(2.17201203177395,99.5339359392258,13.2146990788338));
#59544=CARTESIAN_POINT('Ctrl Pts',(2.17465225662852,99.5438758174746,13.2940922511326));
#59545=CARTESIAN_POINT('Ctrl Pts',(2.17465250999375,99.5438767713402,13.2940998699797));
#59546=CARTESIAN_POINT('Ctrl Pts',(2.17465276331743,99.5438777252053,13.2941074888289));
#59547=CARTESIAN_POINT('Ctrl Pts',(2.17465301659955,99.54387867907,13.2941151076802));
#59548=CARTESIAN_POINT('Ctrl Pts',(2.17733544349689,99.5539807441159,13.3748038348931));
#59549=CARTESIAN_POINT('Ctrl Pts',(2.17536218380245,99.5640491175395,13.4559394106849));
#59550=CARTESIAN_POINT('Ctrl Pts',(2.1688311785283,99.5741025981913,13.5369052169983));
#59551=CARTESIAN_POINT('Ctrl Pts',(2.16710917366223,99.5767533604976,13.5582531575687));
#59552=CARTESIAN_POINT('Ctrl Pts',(2.16507059489321,99.5794030846536,13.5795892556402));
#59553=CARTESIAN_POINT('Ctrl Pts',(2.16271783205606,99.5820521090332,13.6009021558878));
#59554=CARTESIAN_POINT('Ctrl Pts',(2.15133149971718,99.5948722163059,13.7040471739456));
#59555=CARTESIAN_POINT('Ctrl Pts',(2.13258283001489,99.607679571714,13.8066505407393));
#59556=CARTESIAN_POINT('Ctrl Pts',(2.10673035469947,99.6206636446915,13.9075658443977));
#59557=CARTESIAN_POINT('Ctrl Pts',(2.08570540303654,99.63122315605,13.9896368784315));
#59558=CARTESIAN_POINT('Ctrl Pts',(2.06000808575108,99.6417930747003,14.0706069478822));
#59559=CARTESIAN_POINT('Ctrl Pts',(2.0297813703537,99.6523784596769,14.1499580976884));
#59560=CARTESIAN_POINT('Ctrl Pts',(2.01097046577524,99.6589660317669,14.199340469791));
#59561=CARTESIAN_POINT('Ctrl Pts',(1.99040590211624,99.6655593707656,14.2480942993227));
#59562=CARTESIAN_POINT('Ctrl Pts',(1.96811302571224,99.6721612472383,14.2961051261221));
#59563=CARTESIAN_POINT('Ctrl Pts',(1.92430869073101,99.6851335888631,14.3904438871565));
#59564=CARTESIAN_POINT('Ctrl Pts',(1.87381620266567,99.6981423334792,14.4819377217618));
#59565=CARTESIAN_POINT('Ctrl Pts',(1.81688138065531,99.7112427268971,14.5695059311583));
#59566=CARTESIAN_POINT('Ctrl Pts',(1.79588465351929,99.7160739598097,14.6017998021772));
#59567=CARTESIAN_POINT('Ctrl Pts',(1.77401026281012,99.7209346584008,14.6335529471061));
#59568=CARTESIAN_POINT('Ctrl Pts',(1.75128585840563,99.7257868596548,14.6647124589427));
#59569=CARTESIAN_POINT('Ctrl Pts',(1.75123939456334,99.7257967807911,14.6647761697718));
#59570=CARTESIAN_POINT('Ctrl Pts',(1.75119292716784,99.725806701892,14.6648398781203));
#59571=CARTESIAN_POINT('Ctrl Pts',(1.75114645621964,99.7258166229571,14.6649035839879));
#59572=CARTESIAN_POINT('Ctrl Pts',(1.69420145669655,99.7379737893328,14.7429680682209));
#59573=CARTESIAN_POINT('Ctrl Pts',(1.63180444131572,99.7500896128888,14.8174668607998));
#59574=CARTESIAN_POINT('Ctrl Pts',(1.56463978125246,99.7621883077862,14.8877746218344));
#59575=CARTESIAN_POINT('Ctrl Pts',(1.52240421213,99.7697964050229,14.9319866866051));
#59576=CARTESIAN_POINT('Ctrl Pts',(1.47828438596298,99.7773977137962,14.97454186018));
#59577=CARTESIAN_POINT('Ctrl Pts',(1.43245938870037,99.784998085906,15.0152901982427));
#59578=CARTESIAN_POINT('Ctrl Pts',(1.31889443393477,99.803833567988,15.1162740159252));
#59579=CARTESIAN_POINT('Ctrl Pts',(1.19483881768242,99.8228290554776,15.2061128570069));
#59580=CARTESIAN_POINT('Ctrl Pts',(1.06279457934823,99.8418819585718,15.2828918450947));
#59581=CARTESIAN_POINT('Ctrl Pts',(1.05466051134674,99.8430556380246,15.2876215138639));
#59582=CARTESIAN_POINT('Ctrl Pts',(1.04649611401815,99.8442295364327,15.2923016312756));
#59583=CARTESIAN_POINT('Ctrl Pts',(1.03830196624621,99.8454036302503,15.2969317521906));
#59584=CARTESIAN_POINT('Ctrl Pts',(0.954433305329069,99.8574207037783,15.3443219203741));
#59585=CARTESIAN_POINT('Ctrl Pts',(0.867441690335356,99.8694593707389,15.3864821264533));
#59586=CARTESIAN_POINT('Ctrl Pts',(0.777865883180836,99.8815301958095,15.4229426509981));
#59587=CARTESIAN_POINT('Ctrl Pts',(0.712348864663079,99.890358968832,15.4496103968734));
#59588=CARTESIAN_POINT('Ctrl Pts',(0.645437412417385,99.899206361356,15.4732296160634));
#59589=CARTESIAN_POINT('Ctrl Pts',(0.577432620505872,99.9080652754043,15.493579863064));
#59590=CARTESIAN_POINT('Ctrl Pts',(0.568105477213835,99.9092803127336,15.4963709850492));
#59591=CARTESIAN_POINT('Ctrl Pts',(0.558757828830809,99.9105007863209,15.4990985496394));
#59592=CARTESIAN_POINT('Ctrl Pts',(0.549390643273964,99.9117205036068,15.5017644278983));
#59593=CARTESIAN_POINT('Ctrl Pts',(0.549303760441458,99.9117318167693,15.5017891545414));
#59594=CARTESIAN_POINT('Ctrl Pts',(0.549216875927361,99.9117431298669,15.5018138758781));
#59595=CARTESIAN_POINT('Ctrl Pts',(0.549129989732626,99.9117544428946,15.5018385919101));
#59596=CARTESIAN_POINT('Ctrl Pts',(0.450557554638052,99.924589078939,15.5298789437017));
#59597=CARTESIAN_POINT('Ctrl Pts',(0.349697811882334,99.937366876107,15.5511163310684));
#59598=CARTESIAN_POINT('Ctrl Pts',(0.247623594733156,99.950198263937,15.5654747265406));
#59599=CARTESIAN_POINT('Ctrl Pts',(0.232582801106788,99.9520889887614,15.5675904583007));
#59600=CARTESIAN_POINT('Ctrl Pts',(0.217515698898134,99.9539808712478,15.5695568993481));
#59601=CARTESIAN_POINT('Ctrl Pts',(0.202425780047518,99.9558742584633,15.5713738805561));
#59602=CARTESIAN_POINT('Ctrl Pts',(0.117124253231252,99.9665773524916,15.5816450604592));
#59603=CARTESIAN_POINT('Ctrl Pts',(0.0310858230689608,99.9772955882342,
15.5871565204135));
#59604=CARTESIAN_POINT('Ctrl Pts',(-0.0551574262171184,99.9880340081795,
15.5879089851066));
#59605=CARTESIAN_POINT('Ctrl Pts',(-0.173253145552197,100.00273847999,15.5889393597729));
#59606=CARTESIAN_POINT('Ctrl Pts',(-0.291755310329019,100.017516805886,
15.5810316528577));
#59607=CARTESIAN_POINT('Ctrl Pts',(-0.409204178600894,100.032500685822,
15.5640881905311));
#59608=CARTESIAN_POINT('Ctrl Pts',(-0.523525503977769,100.047085560403,
15.5475959152274));
#59609=CARTESIAN_POINT('Ctrl Pts',(-0.636861243755178,100.061746925084,
15.5225878453474));
#59610=CARTESIAN_POINT('Ctrl Pts',(-0.747795796437421,100.07638777261,15.4890900970245));
#59611=CARTESIAN_POINT('Ctrl Pts',(-0.799676054300541,100.083234791204,
15.4734243573716));
#59612=CARTESIAN_POINT('Ctrl Pts',(-0.851029851688863,100.090077086273,
15.4559027336504));
#59613=CARTESIAN_POINT('Ctrl Pts',(-0.901706648082814,100.096904017119,
15.4365349514725));
#59614=CARTESIAN_POINT('Ctrl Pts',(-0.916450353441402,100.098890217196,
15.4309001660441));
#59615=CARTESIAN_POINT('Ctrl Pts',(-0.931136742687463,100.100875116686,
15.4251091506041));
#59616=CARTESIAN_POINT('Ctrl Pts',(-0.945762089483852,100.102857986619,
15.4191624762268));
#59617=CARTESIAN_POINT('Ctrl Pts',(-0.945778031059615,100.10286014794,15.4191559943729));
#59618=CARTESIAN_POINT('Ctrl Pts',(-0.945793972562841,100.102862309258,
15.4191495123342));
#59619=CARTESIAN_POINT('Ctrl Pts',(-0.945809913993562,100.102864470575,
15.4191430301105));
#59620=CARTESIAN_POINT('Ctrl Pts',(-1.04799977669469,100.116719225642,15.3775898244658));
#59621=CARTESIAN_POINT('Ctrl Pts',(-1.14738413899489,100.130483380395,15.3283701976069));
#59622=CARTESIAN_POINT('Ctrl Pts',(-1.2430104132479,100.144252397705,15.2721648231545));
#59623=CARTESIAN_POINT('Ctrl Pts',(-1.31364396260535,100.154422767422,15.2306491924186));
#59624=CARTESIAN_POINT('Ctrl Pts',(-1.38222670024172,100.164595719987,15.1853232548914));
#59625=CARTESIAN_POINT('Ctrl Pts',(-1.44837327938249,100.17480840503,15.1364794768139));
#59626=CARTESIAN_POINT('Ctrl Pts',(-1.51548974446611,100.185170835377,15.0869195181815));
#59627=CARTESIAN_POINT('Ctrl Pts',(-1.58011109425372,100.195577744006,15.0337298099532));
#59628=CARTESIAN_POINT('Ctrl Pts',(-1.64187900958763,100.206077098135,14.9771766118642));
#59629=CARTESIAN_POINT('Ctrl Pts',(-1.74258242110682,100.223194735566,14.8849750222672));
#59630=CARTESIAN_POINT('Ctrl Pts',(-1.83573088714695,100.240559926231,14.7838007788656));
#59631=CARTESIAN_POINT('Ctrl Pts',(-1.91975790605777,100.25803654293,14.675008534083));
#59632=CARTESIAN_POINT('Ctrl Pts',(-1.95224816775895,100.264794129448,14.6329424397497));
#59633=CARTESIAN_POINT('Ctrl Pts',(-1.98337523693324,100.271568434829,14.5897373495495));
#59634=CARTESIAN_POINT('Ctrl Pts',(-2.01305060062776,100.278351822717,14.5454711408116));
#59635=CARTESIAN_POINT('Ctrl Pts',(-2.04203376731463,100.284976983705,14.5022374699575));
#59636=CARTESIAN_POINT('Ctrl Pts',(-2.06962877181567,100.291610749388,14.4579956181135));
#59637=CARTESIAN_POINT('Ctrl Pts',(-2.09574884560272,100.298246765759,14.4128279128811));
#59638=CARTESIAN_POINT('Ctrl Pts',(-2.09575697155803,100.298248830224,14.4128138612074));
#59639=CARTESIAN_POINT('Ctrl Pts',(-2.09576509737053,100.298250894689,14.4127998094441));
#59640=CARTESIAN_POINT('Ctrl Pts',(-2.09577322304035,100.298252959155,14.4127857575909));
#59641=CARTESIAN_POINT('Ctrl Pts',(-2.12248343407465,100.305039145696,14.3665953544916));
#59642=CARTESIAN_POINT('Ctrl Pts',(-2.14765135421186,100.311829629413,14.3194351763449));
#59643=CARTESIAN_POINT('Ctrl Pts',(-2.17121629666769,100.31863605248,14.2714235530651));
#59644=CARTESIAN_POINT('Ctrl Pts',(-2.21830681840551,100.332237529079,14.1754805057199));
#59645=CARTESIAN_POINT('Ctrl Pts',(-2.25899867212424,100.345905410451,14.076136946669));
#59646=CARTESIAN_POINT('Ctrl Pts',(-2.2928898276478,100.359606310524,13.9742881567927));
#59647=CARTESIAN_POINT('Ctrl Pts',(-2.30621162432765,100.36499180424,13.9342538513858));
#59648=CARTESIAN_POINT('Ctrl Pts',(-2.3184824575564,100.370382006744,13.893832245958));
#59649=CARTESIAN_POINT('Ctrl Pts',(-2.32967708652519,100.375773321592,13.8530771968934));
#59650=CARTESIAN_POINT('Ctrl Pts',(-2.35437903891379,100.387669741123,13.7631475275495));
#59651=CARTESIAN_POINT('Ctrl Pts',(-2.37384061634741,100.399572478644,13.6715843293427));
#59652=CARTESIAN_POINT('Ctrl Pts',(-2.38782825765813,100.411334417878,13.5790799856954));
#59653=CARTESIAN_POINT('Ctrl Pts',(-2.39001701902716,100.413174905323,13.564605069636));
#59654=CARTESIAN_POINT('Ctrl Pts',(-2.39207182906872,100.415011955553,13.5501070441293));
#59655=CARTESIAN_POINT('Ctrl Pts',(-2.39399187955346,100.416845016453,13.5355884844563));
#59656=CARTESIAN_POINT('Ctrl Pts',(-2.39945831298096,100.42206378828,13.4942537692776));
#59657=CARTESIAN_POINT('Ctrl Pts',(-2.40383189474815,100.427249953131,13.4527549038664));
#59658=CARTESIAN_POINT('Ctrl Pts',(-2.40709471261336,100.432390402776,13.4111586367477));
#59659=CARTESIAN_POINT('Ctrl Pts',(-2.40709787622975,100.432395386937,13.4111183051577));
#59660=CARTESIAN_POINT('Ctrl Pts',(-2.4071010387989,100.43240037107,13.411077973439));
#59661=CARTESIAN_POINT('Ctrl Pts',(-2.40710420032078,100.432405355173,13.4110376415917));
#59662=CARTESIAN_POINT('Ctrl Pts',(-2.41381135753041,100.442979111809,13.3254737737003));
#59663=CARTESIAN_POINT('Ctrl Pts',(-2.41580151253102,100.453422042174,13.2393282676031));
#59664=CARTESIAN_POINT('Ctrl Pts',(-2.41313967918205,100.46382042649,13.1531670804234));
#59665=CARTESIAN_POINT('Ctrl Pts',(-2.41158529906977,100.469892572887,13.1028531733358));
#59666=CARTESIAN_POINT('Ctrl Pts',(-2.40844537421013,100.47594946381,13.0525345450383));
#59667=CARTESIAN_POINT('Ctrl Pts',(-2.40373978080333,100.482007711917,13.002328242712));
#59668=CARTESIAN_POINT('Ctrl Pts',(-2.39438755313016,100.494048300786,12.9025447022761));
#59669=CARTESIAN_POINT('Ctrl Pts',(-2.37885121677452,100.50609867673,12.8032014758413));
#59670=CARTESIAN_POINT('Ctrl Pts',(-2.35727131497552,100.518320450128,12.7050350944655));
#59671=CARTESIAN_POINT('Ctrl Pts',(-2.34872486511952,100.523160730426,12.6661575284882));
#59672=CARTESIAN_POINT('Ctrl Pts',(-2.33923035221702,100.528027818563,12.6274650930927));
#59673=CARTESIAN_POINT('Ctrl Pts',(-2.3287961596825,100.532931452916,12.589005765313));
#59674=CARTESIAN_POINT('Ctrl Pts',(-2.32160408235416,100.536311428639,12.562496530557));
#59675=CARTESIAN_POINT('Ctrl Pts',(-2.31396520449789,100.539708857728,12.536096340056));
#59676=CARTESIAN_POINT('Ctrl Pts',(-2.30588147887959,100.543126929759,12.5098188373672));
#59677=CARTESIAN_POINT('Ctrl Pts',(-2.2760356874277,100.555746737733,12.4128000984639));
#59678=CARTESIAN_POINT('Ctrl Pts',(-2.24012155072084,100.568652301366,12.3174378106301));
#59679=CARTESIAN_POINT('Ctrl Pts',(-2.19841568484051,100.581715205391,12.22440728038));
#59680=CARTESIAN_POINT('Ctrl Pts',(-2.18236550217605,100.586742363833,12.1886051942137));
#59681=CARTESIAN_POINT('Ctrl Pts',(-2.1654570885242,100.591792888321,12.1531481562251));
#59682=CARTESIAN_POINT('Ctrl Pts',(-2.14770437000184,100.59685970141,12.1180737365215));
#59683=CARTESIAN_POINT('Ctrl Pts',(-2.1024118139436,100.609786674572,12.028588280047));
#59684=CARTESIAN_POINT('Ctrl Pts',(-2.05162395767972,100.622816458876,11.9415966638525));
#59685=CARTESIAN_POINT('Ctrl Pts',(-1.99564331342835,100.635812319395,11.8578356081371));
#59686=CARTESIAN_POINT('Ctrl Pts',(-1.97414291619667,100.640803618928,11.8256656323444));
#59687=CARTESIAN_POINT('Ctrl Pts',(-1.95187664614289,100.645789976378,11.7939716615095));
#59688=CARTESIAN_POINT('Ctrl Pts',(-1.92886183642982,100.650763880935,11.76279339908));
#59689=CARTESIAN_POINT('Ctrl Pts',(-1.87960254668455,100.661409678523,11.6960616258473));
#59690=CARTESIAN_POINT('Ctrl Pts',(-1.82691430179624,100.671995963239,11.6316957175191));
#59691=CARTESIAN_POINT('Ctrl Pts',(-1.77102050030755,100.682456431535,11.5701340456267));
#59692=CARTESIAN_POINT('Ctrl Pts',(-1.73631729585265,100.688951101074,11.5319117878921));
#59693=CARTESIAN_POINT('Ctrl Pts',(-1.70037892184861,100.69539731069,11.4947697029924));
#59694=CARTESIAN_POINT('Ctrl Pts',(-1.66326310795707,100.701779597646,11.4588034785056));
#59695=CARTESIAN_POINT('Ctrl Pts',(-1.66323745244004,100.701784009266,11.4587786176178));
#59696=CARTESIAN_POINT('Ctrl Pts',(-1.66321179633677,100.701788420855,11.4587537572618));
#59697=CARTESIAN_POINT('Ctrl Pts',(-1.66318613964721,100.701792832411,11.4587288974377));
#59698=CARTESIAN_POINT('Ctrl Pts',(-1.60430288709543,100.71191755316,11.4016744868032));
#59699=CARTESIAN_POINT('Ctrl Pts',(-1.54232771466886,100.721876200575,11.3474197051733));
#59700=CARTESIAN_POINT('Ctrl Pts',(-1.47759943445463,100.731811060499,11.2962869777295));
#59701=CARTESIAN_POINT('Ctrl Pts',(-1.46304701463237,100.734044647612,11.2847911537411));
#59702=CARTESIAN_POINT('Ctrl Pts',(-1.44835562899329,100.736277008215,11.2734532147885));
#59703=CARTESIAN_POINT('Ctrl Pts',(-1.43352946771426,100.738509716868,11.2622769493372));
#59704=CARTESIAN_POINT('Ctrl Pts',(-1.36685292573567,100.748550703836,11.2120147999848));
#59705=CARTESIAN_POINT('Ctrl Pts',(-1.29744712026998,100.758600719898,11.1650194486941));
#59706=CARTESIAN_POINT('Ctrl Pts',(-1.22562892850108,100.76880321441,11.1215867895098));
#59707=CARTESIAN_POINT('Ctrl Pts',(-1.21074116223448,100.770918170939,11.1125832868826));
#59708=CARTESIAN_POINT('Ctrl Pts',(-1.19574983233038,100.77303965936,11.1037330267289));
#59709=CARTESIAN_POINT('Ctrl Pts',(-1.18065793506841,100.775168925174,11.0950388653619));
#59710=CARTESIAN_POINT('Ctrl Pts',(1.85693809316476,98.5858197253477,11.6266881416021));
#59711=CARTESIAN_POINT('Ctrl Pts',(1.91417673598575,98.5969468569167,11.6949465173591));
#59712=CARTESIAN_POINT('Ctrl Pts',(1.96773903937305,98.6079987826475,11.7661548820132));
#59713=CARTESIAN_POINT('Ctrl Pts',(2.01732925929512,98.6190075301634,11.8398678057961));
#59714=CARTESIAN_POINT('Ctrl Pts',(2.047604010715,98.6257283532412,11.8848694300571));
#59715=CARTESIAN_POINT('Ctrl Pts',(2.07639816329627,98.6324329822682,11.9308035091556));
#59716=CARTESIAN_POINT('Ctrl Pts',(2.10364433161086,98.6391277432176,11.9775591854309));
#59717=CARTESIAN_POINT('Ctrl Pts',(2.14800936196921,98.6500288456896,12.0536916152619));
#59718=CARTESIAN_POINT('Ctrl Pts',(2.1882598999595,98.6609084447206,12.1320088513954));
#59719=CARTESIAN_POINT('Ctrl Pts',(2.22411431958962,98.6718089272195,12.2120820155326));
#59720=CARTESIAN_POINT('Ctrl Pts',(2.24634745585678,98.6785682588522,12.2617349617515));
#59721=CARTESIAN_POINT('Ctrl Pts',(2.26688965691372,98.6853354878269,12.3120622309737));
#59722=CARTESIAN_POINT('Ctrl Pts',(2.2856700677231,98.6921194114877,12.3629522603032));
#59723=CARTESIAN_POINT('Ctrl Pts',(2.31285775264305,98.7019402392045,12.4366238161079));
#59724=CARTESIAN_POINT('Ctrl Pts',(2.33635867160346,98.7117988182997,12.5114924425386));
#59725=CARTESIAN_POINT('Ctrl Pts',(2.35618043222215,98.721649839398,12.5871735365766));
#59726=CARTESIAN_POINT('Ctrl Pts',(2.37113415918653,98.7290815445153,12.6442680822317));
#59727=CARTESIAN_POINT('Ctrl Pts',(2.38399444164648,98.736509079571,12.7018260119645));
#59728=CARTESIAN_POINT('Ctrl Pts',(2.39476779116759,98.7439154465351,12.7597014291137));
#59729=CARTESIAN_POINT('Ctrl Pts',(2.401226103283,98.7483553497799,12.7943960713906));
#59730=CARTESIAN_POINT('Ctrl Pts',(2.40693425238278,98.7527872203904,12.8292022708228));
#59731=CARTESIAN_POINT('Ctrl Pts',(2.41190643219563,98.7572035475463,12.8640867791556));
#59732=CARTESIAN_POINT('Ctrl Pts',(2.41190675506834,98.7572038343243,12.8640890444107));
#59733=CARTESIAN_POINT('Ctrl Pts',(2.41190707793795,98.7572041211021,12.8640913096662));
#59734=CARTESIAN_POINT('Ctrl Pts',(2.41190740080446,98.75720440788,12.864093574922));
#59735=CARTESIAN_POINT('Ctrl Pts',(2.42701541202014,98.7706237078314,12.9700925226681));
#59736=CARTESIAN_POINT('Ctrl Pts',(2.43514073546767,98.783968420195,13.0769193128911));
#59737=CARTESIAN_POINT('Ctrl Pts',(2.43638481590199,98.7972525916792,13.18362664369));
#59738=CARTESIAN_POINT('Ctrl Pts',(2.43700897416945,98.8039172937591,13.2371619786083));
#59739=CARTESIAN_POINT('Ctrl Pts',(2.4359016179274,98.8105666942635,13.2906665995291));
#59740=CARTESIAN_POINT('Ctrl Pts',(2.43307914839644,98.8172021819321,13.3440175316217));
#59741=CARTESIAN_POINT('Ctrl Pts',(2.42789700836977,98.8293851393977,13.4419714679263));
#59742=CARTESIAN_POINT('Ctrl Pts',(2.41690336065044,98.8415293527585,13.5394029421038));
#59743=CARTESIAN_POINT('Ctrl Pts',(2.40014414136372,98.8536652226893,13.6355897984486));
#59744=CARTESIAN_POINT('Ctrl Pts',(2.38876309683304,98.8619065896491,13.7009094816985));
#59745=CARTESIAN_POINT('Ctrl Pts',(2.37472306456667,98.8701439677234,13.7656541013784));
#59746=CARTESIAN_POINT('Ctrl Pts',(2.35804083292173,98.8783850720437,13.8295840832372));
#59747=CARTESIAN_POINT('Ctrl Pts',(2.34750679934094,98.8835889363408,13.8699528174721));
#59748=CARTESIAN_POINT('Ctrl Pts',(2.33591896182167,98.8887945023829,13.9099988567666));
#59749=CARTESIAN_POINT('Ctrl Pts',(2.32328120727427,98.8940038103791,13.9496644746548));
#59750=CARTESIAN_POINT('Ctrl Pts',(2.30140899554917,98.9030195803093,14.018313916247));
#59751=CARTESIAN_POINT('Ctrl Pts',(2.27639112347116,98.9120469498515,14.0858253077428));
#59752=CARTESIAN_POINT('Ctrl Pts',(2.24841602309062,98.9210535394763,14.151975538528));
#59753=CARTESIAN_POINT('Ctrl Pts',(2.24405759988463,98.9224567347711,14.1622815140925));
#59754=CARTESIAN_POINT('Ctrl Pts',(2.23962734738864,98.9238594385837,14.1725545399852));
#59755=CARTESIAN_POINT('Ctrl Pts',(2.23512591934516,98.9252615427703,14.1827938692418));
#59756=CARTESIAN_POINT('Ctrl Pts',(2.23511817777363,98.925263954114,14.1828114788757));
#59757=CARTESIAN_POINT('Ctrl Pts',(2.23511043599147,98.9252663654558,14.1828290884078));
#59758=CARTESIAN_POINT('Ctrl Pts',(2.23510269399866,98.9252687767959,14.1828466978383));
#59759=CARTESIAN_POINT('Ctrl Pts',(2.17794479438478,98.9430713162717,14.312854317855));
#59760=CARTESIAN_POINT('Ctrl Pts',(2.10930175381278,98.9607767910995,14.4373209986211));
#59761=CARTESIAN_POINT('Ctrl Pts',(2.03066171000624,98.9783997225956,14.5545960989096));
#59762=CARTESIAN_POINT('Ctrl Pts',(2.02606260275723,98.9794303648494,14.5614547009367));
#59763=CARTESIAN_POINT('Ctrl Pts',(2.02142931602233,98.9804607232536,14.568288698883));
#59764=CARTESIAN_POINT('Ctrl Pts',(2.01676215236437,98.9814908001412,14.575097760253));
#59765=CARTESIAN_POINT('Ctrl Pts',(1.94416808705626,98.99751283715,14.6810073623154));
#59766=CARTESIAN_POINT('Ctrl Pts',(1.86337509951493,99.0134675800737,14.780885479184));
#59767=CARTESIAN_POINT('Ctrl Pts',(1.77547310145705,99.0293745555827,14.8734835174004));
#59768=CARTESIAN_POINT('Ctrl Pts',(1.76064829300454,99.0320572917001,14.8891003203169));
#59769=CARTESIAN_POINT('Ctrl Pts',(1.74562134434268,99.0347386535236,14.9045099526594));
#59770=CARTESIAN_POINT('Ctrl Pts',(1.73039756958489,99.0374187156741,14.919706308246));
#59771=CARTESIAN_POINT('Ctrl Pts',(1.64769725892055,99.0519776523356,15.0022576693882));
#59772=CARTESIAN_POINT('Ctrl Pts',(1.55918602531543,99.0664990006054,15.0785180605838));
#59773=CARTESIAN_POINT('Ctrl Pts',(1.46568429520091,99.0809991507652,15.1475124088901));
#59774=CARTESIAN_POINT('Ctrl Pts',(1.44599705066954,99.0840522279819,15.1620395048564));
#59775=CARTESIAN_POINT('Ctrl Pts',(1.42608862878947,99.0871043460674,15.1762443027718));
#59776=CARTESIAN_POINT('Ctrl Pts',(1.40596681419401,99.0901556270038,15.1901174339669));
#59777=CARTESIAN_POINT('Ctrl Pts',(1.40594264751216,99.0901592916502,15.1901340958612));
#59778=CARTESIAN_POINT('Ctrl Pts',(1.40591848052765,99.0901629562946,15.1901507572739));
#59779=CARTESIAN_POINT('Ctrl Pts',(1.40589431324056,99.090166620937,15.1901674182049));
#59780=CARTESIAN_POINT('Ctrl Pts',(1.40368185140187,99.0905021108659,15.1916926896963));
#59781=CARTESIAN_POINT('Ctrl Pts',(1.40146685330708,99.0908375839379,15.1932139243866));
#59782=CARTESIAN_POINT('Ctrl Pts',(1.39924932977195,99.0911730415125,15.1947311102363));
#59783=CARTESIAN_POINT('Ctrl Pts',(1.30214891635913,99.1058619810725,15.2611652972421));
#59784=CARTESIAN_POINT('Ctrl Pts',(1.20019985425589,99.1205226743845,15.3198379144593));
#59785=CARTESIAN_POINT('Ctrl Pts',(1.09471441959963,99.1351467647404,15.3704986170229));
#59786=CARTESIAN_POINT('Ctrl Pts',(1.02858782949793,99.1443142979806,15.4022567410103));
#59787=CARTESIAN_POINT('Ctrl Pts',(0.96107047246329,99.1534675576461,15.430866581243));
#59788=CARTESIAN_POINT('Ctrl Pts',(0.892475242895028,99.1626056045417,15.4562660571135));
#59789=CARTESIAN_POINT('Ctrl Pts',(0.781385488346495,99.1774046422166,15.4974004269214));
#59790=CARTESIAN_POINT('Ctrl Pts',(0.667469791677626,99.1921631044739,15.5301183468881));
#59791=CARTESIAN_POINT('Ctrl Pts',(0.552101904503678,99.2068707663012,15.5541397627508));
#59792=CARTESIAN_POINT('Ctrl Pts',(0.466973388836592,99.2177233653299,15.5718648639615));
#59793=CARTESIAN_POINT('Ctrl Pts',(0.381053394821842,99.2285484406278,15.5848557127175));
#59794=CARTESIAN_POINT('Ctrl Pts',(0.294876898577294,99.2393441839979,15.5930062691574));
#59795=CARTESIAN_POINT('Ctrl Pts',(0.261373376392985,99.2435413310538,15.5961750258416));
#59796=CARTESIAN_POINT('Ctrl Pts',(0.22783196433043,99.2477339593837,15.598611776666));
#59797=CARTESIAN_POINT('Ctrl Pts',(0.194284751723588,99.2519219225085,15.6003099778197));
#59798=CARTESIAN_POINT('Ctrl Pts',(0.194274870771869,99.2519231560256,15.6003104780056));
#59799=CARTESIAN_POINT('Ctrl Pts',(0.194264989819291,99.2519243895424,15.6003109781277));
#59800=CARTESIAN_POINT('Ctrl Pts',(0.194255108865836,99.2519256230587,15.600311478186));
#59801=CARTESIAN_POINT('Ctrl Pts',(0.125549408185388,99.2605026907845,15.6037885570454));
#59802=CARTESIAN_POINT('Ctrl Pts',(0.0567974642991696,99.2690620764199,
15.6041793692269));
#59803=CARTESIAN_POINT('Ctrl Pts',(-0.0117206539231109,99.277612972139,
15.6014220862784));
#59804=CARTESIAN_POINT('Ctrl Pts',(-0.0279277522598392,99.2796355788799,
15.6007698857065));
#59805=CARTESIAN_POINT('Ctrl Pts',(-0.0441215422889647,99.2816576821861,
15.599941580274));
#59806=CARTESIAN_POINT('Ctrl Pts',(-0.0602979007831986,99.2836793508579,
15.5989364281172));
#59807=CARTESIAN_POINT('Ctrl Pts',(-0.155189454247767,99.2955385885799,
15.5930401412822));
#59808=CARTESIAN_POINT('Ctrl Pts',(-0.249497472395329,99.3073853048398,
15.5810531959571));
#59809=CARTESIAN_POINT('Ctrl Pts',(-0.342529244294992,99.3192120108426,
15.5633069676301));
#59810=CARTESIAN_POINT('Ctrl Pts',(-0.383655949057396,99.3244402617526,
15.5554618639827));
#59811=CARTESIAN_POINT('Ctrl Pts',(-0.424533895934865,99.3296646860019,
15.546491035537));
#59812=CARTESIAN_POINT('Ctrl Pts',(-0.465106181639773,99.3348850358048,
15.536421804769));
#59813=CARTESIAN_POINT('Ctrl Pts',(-0.552371864455765,99.3461133258105,
15.514764205668));
#59814=CARTESIAN_POINT('Ctrl Pts',(-0.638221444598278,99.3573222854356,
15.4880276545498));
#59815=CARTESIAN_POINT('Ctrl Pts',(-0.72206074077835,99.3685044860839,15.4565129213605));
#59816=CARTESIAN_POINT('Ctrl Pts',(-0.766011985468675,99.3743665538644,
15.4399918887081));
#59817=CARTESIAN_POINT('Ctrl Pts',(-0.809411630058819,99.3802213759304,
15.4221576968483));
#59818=CARTESIAN_POINT('Ctrl Pts',(-0.852179681968102,99.3860685973948,
15.4030527200777));
#59819=CARTESIAN_POINT('Ctrl Pts',(-0.911766896620319,99.3942153243315,
15.3764344314036));
#59820=CARTESIAN_POINT('Ctrl Pts',(-0.970130500379672,99.4023468455704,
15.3473587082573));
#59821=CARTESIAN_POINT('Ctrl Pts',(-1.02701479794973,99.410460877643,15.3159043816065));
#59822=CARTESIAN_POINT('Ctrl Pts',(-1.02702824809226,99.4104627961845,15.3158969443137));
#59823=CARTESIAN_POINT('Ctrl Pts',(-1.02704169815214,99.4104647147251,15.3158895068879));
#59824=CARTESIAN_POINT('Ctrl Pts',(-1.02705514812928,99.4104666332647,15.3158820693293));
#59825=CARTESIAN_POINT('Ctrl Pts',(-1.09439411538887,99.4200720379882,15.278645015782));
#59826=CARTESIAN_POINT('Ctrl Pts',(-1.15975492266891,99.4296619103106,15.2380844448373));
#59827=CARTESIAN_POINT('Ctrl Pts',(-1.22278322196834,99.4392373810056,15.1943637056183));
#59828=CARTESIAN_POINT('Ctrl Pts',(-1.28581152126779,99.4488128517006,15.1506429663993));
#59829=CARTESIAN_POINT('Ctrl Pts',(-1.34650663618581,99.4583739206444,15.1037613526107));
#59830=CARTESIAN_POINT('Ctrl Pts',(-1.40447276324155,99.4679146068899,15.0539221631217));
#59831=CARTESIAN_POINT('Ctrl Pts',(-1.4122049541814,99.4691872537182,15.0472740368971));
#59832=CARTESIAN_POINT('Ctrl Pts',(-1.41988877852004,99.4704595693226,15.0405731177698));
#59833=CARTESIAN_POINT('Ctrl Pts',(-1.42752335664479,99.4717315482021,15.0338198509602));
#59834=CARTESIAN_POINT('Ctrl Pts',(-1.46126734594077,99.4773535538969,15.0039711600158));
#59835=CARTESIAN_POINT('Ctrl Pts',(-1.49404925406796,99.4829689748849,14.9730998278357));
#59836=CARTESIAN_POINT('Ctrl Pts',(-1.52583311760315,99.4885787544094,14.9412808719977));
#59837=CARTESIAN_POINT('Ctrl Pts',(-1.52585068633716,99.488581855251,14.9412632838662));
#59838=CARTESIAN_POINT('Ctrl Pts',(-1.52586825476187,99.4885849560902,14.9412456954474));
#59839=CARTESIAN_POINT('Ctrl Pts',(-1.52588582287745,99.4885880569271,14.9412281067411));
#59840=CARTESIAN_POINT('Ctrl Pts',(-1.58115232099639,99.4983427967564,14.8858968335732));
#59841=CARTESIAN_POINT('Ctrl Pts',(-1.63335593453091,99.508074040194,14.827725076819));
#59842=CARTESIAN_POINT('Ctrl Pts',(-1.68232436251468,99.5177858924878,14.7671431406004));
#59843=CARTESIAN_POINT('Ctrl Pts',(-1.73129279049846,99.5274977447815,14.7065612043818));
#59844=CARTESIAN_POINT('Ctrl Pts',(-1.77702683221379,99.5371902063529,14.6435695394248));
#59845=CARTESIAN_POINT('Ctrl Pts',(-1.81938005116608,99.5468739059855,14.5785523901826));
#59846=CARTESIAN_POINT('Ctrl Pts',(-1.8471358321929,99.5532200268514,14.5359440170295));
#59847=CARTESIAN_POINT('Ctrl Pts',(-1.87339785697294,99.5595593031522,14.4924487952036));
#59848=CARTESIAN_POINT('Ctrl Pts',(-1.89806545832282,99.5658887441428,14.4481683280864));
#59849=CARTESIAN_POINT('Ctrl Pts',(-1.89807927164982,99.5658922884938,14.4481435319758));
#59850=CARTESIAN_POINT('Ctrl Pts',(-1.89809308447688,99.5658958328417,14.4481187356191));
#59851=CARTESIAN_POINT('Ctrl Pts',(-1.89810689680401,99.5658993771865,14.4480939390164));
#59852=CARTESIAN_POINT('Ctrl Pts',(-1.94180310649515,99.5771121462621,14.3696482475861));
#59853=CARTESIAN_POINT('Ctrl Pts',(-1.98072253908252,99.5883221576043,14.2886978400264));
#59854=CARTESIAN_POINT('Ctrl Pts',(-2.01465522212182,99.5995194743399,14.2058796237811));
#59855=CARTESIAN_POINT('Ctrl Pts',(-2.03003793630761,99.60459555756,14.1683356150034));
#59856=CARTESIAN_POINT('Ctrl Pts',(-2.044395998321,99.6096689699237,14.1304084537033));
#59857=CARTESIAN_POINT('Ctrl Pts',(-2.05771101303856,99.6147384764741,14.0921607815144));
#59858=CARTESIAN_POINT('Ctrl Pts',(-2.082980968104,99.6243596601867,14.0195722806323));
#59859=CARTESIAN_POINT('Ctrl Pts',(-2.10442266847298,99.6339607541982,13.9458068879));
#59860=CARTESIAN_POINT('Ctrl Pts',(-2.12184796472555,99.643529007375,13.8712543843034));
#59861=CARTESIAN_POINT('Ctrl Pts',(-2.12915552340198,99.6475415974915,13.8399896765699));
#59862=CARTESIAN_POINT('Ctrl Pts',(-2.1357565710266,99.6515483310469,13.808587147076));
#59863=CARTESIAN_POINT('Ctrl Pts',(-2.14163678817645,99.6555479171719,13.7770782183977));
#59864=CARTESIAN_POINT('Ctrl Pts',(-2.15486319803449,99.664544211697,13.7062049845924));
#59865=CARTESIAN_POINT('Ctrl Pts',(-2.16444389128284,99.6735062092448,13.6347768389589));
#59866=CARTESIAN_POINT('Ctrl Pts',(-2.17045407467893,99.6824452970138,13.5631727727705));
#59867=CARTESIAN_POINT('Ctrl Pts',(-2.17527721457745,99.6896188669423,13.5057108941939));
#59868=CARTESIAN_POINT('Ctrl Pts',(-2.1778013805117,99.6967778078112,13.4481347336066));
#59869=CARTESIAN_POINT('Ctrl Pts',(-2.17806600939497,99.7039310388077,13.3906160471066));
#59870=CARTESIAN_POINT('Ctrl Pts',(-2.17824403641185,99.7087433191592,13.3519207994595));
#59871=CARTESIAN_POINT('Ctrl Pts',(-2.17739989657897,99.7135525531618,13.3132557449292));
#59872=CARTESIAN_POINT('Ctrl Pts',(-2.17559770860353,99.7183686082064,13.2746659401345));
#59873=CARTESIAN_POINT('Ctrl Pts',(-2.17559713642049,99.7183701372728,13.2746536881207));
#59874=CARTESIAN_POINT('Ctrl Pts',(-2.17559656414086,99.7183716663399,13.2746414361144));
#59875=CARTESIAN_POINT('Ctrl Pts',(-2.17559599176465,99.7183731954077,13.2746291841155));
#59876=CARTESIAN_POINT('Ctrl Pts',(-2.17048933018398,99.7320153272009,13.165318540355));
#59877=CARTESIAN_POINT('Ctrl Pts',(-2.15706993053311,99.7456422820892,13.0565812767468));
#59878=CARTESIAN_POINT('Ctrl Pts',(-2.13578190969035,99.7592462060556,12.949678958828));
#59879=CARTESIAN_POINT('Ctrl Pts',(-2.13133578786128,99.7620874614149,12.9273518137737));
#59880=CARTESIAN_POINT('Ctrl Pts',(-2.12654661235941,99.7649277125925,12.9051046916816));
#59881=CARTESIAN_POINT('Ctrl Pts',(-2.12141870851789,99.7677668886852,12.8829490359156));
#59882=CARTESIAN_POINT('Ctrl Pts',(-2.10189348894183,99.7785774534577,12.7985882411245));
#59883=CARTESIAN_POINT('Ctrl Pts',(-2.07746172782855,99.7893739247512,12.7155472879905));
#59884=CARTESIAN_POINT('Ctrl Pts',(-2.04824592303377,99.8001393971766,12.6344516591826));
#59885=CARTESIAN_POINT('Ctrl Pts',(-2.03297415615081,99.8057667549174,12.5920611261446));
#59886=CARTESIAN_POINT('Ctrl Pts',(-2.01639540213309,99.811385530251,12.5502029742387));
#59887=CARTESIAN_POINT('Ctrl Pts',(-1.99852925915575,99.8169925733225,12.5089717602133));
#59888=CARTESIAN_POINT('Ctrl Pts',(-1.97943931953326,99.8229836881272,12.4649162868352));
#59889=CARTESIAN_POINT('Ctrl Pts',(-1.95887915899225,99.828961763856,12.4215742489325));
#59890=CARTESIAN_POINT('Ctrl Pts',(-1.93687541951419,99.8349244125409,12.3790552447253));
#59891=CARTESIAN_POINT('Ctrl Pts',(-1.90744196851941,99.8429003898988,12.3221794110549));
#59892=CARTESIAN_POINT('Ctrl Pts',(-1.87542325629485,99.8508490300377,12.2667734780342));
#59893=CARTESIAN_POINT('Ctrl Pts',(-1.8410372511685,99.8587984234362,12.2130119194893));
#59894=CARTESIAN_POINT('Ctrl Pts',(-1.82781102231123,99.8618560771526,12.1923330801061));
#59895=CARTESIAN_POINT('Ctrl Pts',(-1.81423425731905,99.8649139110618,12.1718970672831));
#59896=CARTESIAN_POINT('Ctrl Pts',(-1.80031811883615,99.8679737811827,12.1517121936808));
#59897=CARTESIAN_POINT('Ctrl Pts',(-1.80030955952059,99.8679756631986,12.151699778692));
#59898=CARTESIAN_POINT('Ctrl Pts',(-1.80030100007656,99.8679775452153,12.1516873637982));
#59899=CARTESIAN_POINT('Ctrl Pts',(-1.80029244050419,99.8679794272327,12.1516749489994));
#59900=CARTESIAN_POINT('Ctrl Pts',(-1.7479410958742,99.8794900658441,12.0757445892562));
#59901=CARTESIAN_POINT('Ctrl Pts',(-1.69066835351395,99.891022885017,12.0033523218074));
#59902=CARTESIAN_POINT('Ctrl Pts',(-1.62911768397407,99.902562860591,11.9349818441119));
#59903=CARTESIAN_POINT('Ctrl Pts',(-1.60195215802481,99.907656054674,11.9048063805485));
#59904=CARTESIAN_POINT('Ctrl Pts',(-1.5739540200414,99.9127506110194,11.875414235167));
#59905=CARTESIAN_POINT('Ctrl Pts',(-1.54518169887168,99.9178450865659,11.8468462498985));
#59906=CARTESIAN_POINT('Ctrl Pts',(-1.4835056390015,99.928765553391,11.7856082024225));
#59907=CARTESIAN_POINT('Ctrl Pts',(-1.41824828233156,99.9396779509967,11.7281826004569));
#59908=CARTESIAN_POINT('Ctrl Pts',(-1.34992072050328,99.9505545328162,11.6749941954782));
#59909=CARTESIAN_POINT('Ctrl Pts',(-1.31243779271239,99.9565211752669,11.6458162606919));
#59910=CARTESIAN_POINT('Ctrl Pts',(-1.27403171113861,99.9624769210925,11.6179139380439));
#59911=CARTESIAN_POINT('Ctrl Pts',(-1.23479297782328,99.968416332379,11.5913598429592));
#59912=CARTESIAN_POINT('Ctrl Pts',(-1.16188419622155,99.9794522452065,11.5420201585306));
#59913=CARTESIAN_POINT('Ctrl Pts',(-1.08609498573667,99.9904318799357,11.4973329907347));
#59914=CARTESIAN_POINT('Ctrl Pts',(-1.00797578322965,100.001327151754,11.4577351239215));
#59915=CARTESIAN_POINT('Ctrl Pts',(-0.984896824454309,100.004545970189,
11.4460366233423));
#59916=CARTESIAN_POINT('Ctrl Pts',(-0.961614757223156,100.007757380463,
11.4347825492624));
#59917=CARTESIAN_POINT('Ctrl Pts',(-0.938144459933422,100.010960545475,
11.4239846976537));
#59918=CARTESIAN_POINT('Ctrl Pts',(-0.87745855544309,100.019242799574,11.3960652647065));
#59919=CARTESIAN_POINT('Ctrl Pts',(-0.815496414881841,100.027472245218,
11.3711882621347));
#59920=CARTESIAN_POINT('Ctrl Pts',(-0.752601331419458,100.035687471341,
11.3493825214119));
#59921=CARTESIAN_POINT('Ctrl Pts',(-0.689706247957076,100.043902697464,
11.3275767806891));
#59922=CARTESIAN_POINT('Ctrl Pts',(-0.625878476001496,100.052103707113,
11.3088414440984));
#59923=CARTESIAN_POINT('Ctrl Pts',(-0.561407853639797,100.060336256543,
11.2931873647555));
#59924=CARTESIAN_POINT('Ctrl Pts',(-0.553617389451351,100.061331056642,
11.2912957660698));
#59925=CARTESIAN_POINT('Ctrl Pts',(-0.545817752823663,100.062326290681,
11.2894492130978));
#59926=CARTESIAN_POINT('Ctrl Pts',(-0.538009509754961,100.063322031072,
11.2876477355394));
#59927=CARTESIAN_POINT('Ctrl Pts',(-0.538006771879202,100.063322380217,
11.2876471038708));
#59928=CARTESIAN_POINT('Ctrl Pts',(-0.538004034002362,100.063322729363,
11.2876464722078));
#59929=CARTESIAN_POINT('Ctrl Pts',(-0.538001296124486,100.063323078509,
11.2876458405503));
#59930=CARTESIAN_POINT('Ctrl Pts',(-0.465603546126105,100.072555543897,
11.270942911166));
#59931=CARTESIAN_POINT('Ctrl Pts',(-0.392351732701438,100.081845544988,
11.258092863964));
#59932=CARTESIAN_POINT('Ctrl Pts',(-0.318688500137045,100.091160594883,
11.2491285684583));
#59933=CARTESIAN_POINT('Ctrl Pts',(-0.2827428207369,100.095706089094,11.2447542329713));
#59934=CARTESIAN_POINT('Ctrl Pts',(-0.246699900062628,100.100257475839,
11.2413048304038));
#59935=CARTESIAN_POINT('Ctrl Pts',(-0.210615032233411,100.104810568345,
11.2387819165222));
#59936=CARTESIAN_POINT('Ctrl Pts',(-0.133382096340926,100.114555614476,
11.2333820894533));
#59937=CARTESIAN_POINT('Ctrl Pts',(-0.0559542955087094,100.124307966008,
11.2322293802618));
#59938=CARTESIAN_POINT('Ctrl Pts',(0.0211658642688437,100.134026105027,
11.2353374696711));
#59939=CARTESIAN_POINT('Ctrl Pts',(0.0555764068329223,100.138362279087,
11.2367242801137));
#59940=CARTESIAN_POINT('Ctrl Pts',(0.0899250234073539,100.142691553371,
11.2389592244015));
#59941=CARTESIAN_POINT('Ctrl Pts',(0.124163920066559,100.147009814598,11.2420424808953));
#59942=CARTESIAN_POINT('Ctrl Pts',(0.20308162759669,100.156963034759,11.249149121528));
#59943=CARTESIAN_POINT('Ctrl Pts',(0.281422458186795,100.166857903795,11.2607641033883));
#59944=CARTESIAN_POINT('Ctrl Pts',(0.358643616091216,100.17665221554,11.2768842354255));
#59945=CARTESIAN_POINT('Ctrl Pts',(0.375094826460005,100.178738797603,11.2803184714628));
#59946=CARTESIAN_POINT('Ctrl Pts',(0.391495032520846,100.180820791012,11.2839571764946));
#59947=CARTESIAN_POINT('Ctrl Pts',(0.407838682318079,100.182897747539,11.2878002992483));
#59948=CARTESIAN_POINT('Ctrl Pts',(0.468585816358258,100.190617513817,11.3020846663235));
#59949=CARTESIAN_POINT('Ctrl Pts',(0.528562118821918,100.198268652909,11.3191960405154));
#59950=CARTESIAN_POINT('Ctrl Pts',(0.587545717563093,100.205904122806,11.3389426777065));
#59951=CARTESIAN_POINT('Ctrl Pts',(0.633794056365937,100.211891004011,11.354425781256));
#59952=CARTESIAN_POINT('Ctrl Pts',(0.679433166441745,100.217868381716,11.3715292065591));
#59953=CARTESIAN_POINT('Ctrl Pts',(0.724375738701851,100.223864581261,11.39017098217));
#59954=CARTESIAN_POINT('Ctrl Pts',(0.779479836473583,100.231216522846,11.4130276673627));
#59955=CARTESIAN_POINT('Ctrl Pts',(0.833582014341551,100.238634172081,11.4381156038251));
#59956=CARTESIAN_POINT('Ctrl Pts',(0.886359497714081,100.246059788204,11.4655029679801));
#59957=CARTESIAN_POINT('Ctrl Pts',(0.905127540089821,100.248700389255,11.4752421063052));
#59958=CARTESIAN_POINT('Ctrl Pts',(0.923727743854149,100.251341943263,11.4852716690271));
#59959=CARTESIAN_POINT('Ctrl Pts',(0.942144614126101,100.253981673654,11.4955934837883));
#59960=CARTESIAN_POINT('Ctrl Pts',(0.942200171877861,100.253989636868,11.495624621371));
#59961=CARTESIAN_POINT('Ctrl Pts',(0.942255727960906,100.253997600066,11.4956557616129));
#59962=CARTESIAN_POINT('Ctrl Pts',(0.942311282374887,100.254005563247,11.4956869045136));
#59963=CARTESIAN_POINT('Ctrl Pts',(1.01163318083879,100.263942178207,11.5345476331031));
#59964=CARTESIAN_POINT('Ctrl Pts',(1.07849560640498,100.273872967035,11.5776313369723));
#59965=CARTESIAN_POINT('Ctrl Pts',(1.14251460414552,100.28380385674,11.6244143374231));
#59966=CARTESIAN_POINT('Ctrl Pts',(1.17092756044083,100.288211391146,11.6451776013617));
#59967=CARTESIAN_POINT('Ctrl Pts',(1.19878098938501,100.29261898177,11.6666691120486));
#59968=CARTESIAN_POINT('Ctrl Pts',(1.22604411207514,100.29702731935,11.6888414174065));
#59969=CARTESIAN_POINT('Ctrl Pts',(1.27456703557271,100.304873281442,11.7283037009047));
#59970=CARTESIAN_POINT('Ctrl Pts',(1.32130430385171,100.3127723134,11.7698414731503));
#59971=CARTESIAN_POINT('Ctrl Pts',(1.36601958771573,100.320664003457,11.8133526078688));
#59972=CARTESIAN_POINT('Ctrl Pts',(1.40490907505444,100.327527513068,11.8511948304045));
#59973=CARTESIAN_POINT('Ctrl Pts',(1.44226820566837,100.334385363039,11.8905294255716));
#59974=CARTESIAN_POINT('Ctrl Pts',(1.47792043455174,100.341193724797,11.9312653626777));
#59975=CARTESIAN_POINT('Ctrl Pts',(1.49582365413962,100.344612630133,11.9517214309228));
#59976=CARTESIAN_POINT('Ctrl Pts',(1.5132973929337,100.348019242088,11.9725317016156));
#59977=CARTESIAN_POINT('Ctrl Pts',(1.53032424456408,100.351410609321,11.9936821046758));
#59978=CARTESIAN_POINT('Ctrl Pts',(1.57351136842727,100.36001251647,12.0473282570325));
#59979=CARTESIAN_POINT('Ctrl Pts',(1.61382641444132,100.368515862212,12.1031700902447));
#59980=CARTESIAN_POINT('Ctrl Pts',(1.65116008545529,100.376979620875,12.160833428752));
#59981=CARTESIAN_POINT('Ctrl Pts',(1.67918990886772,100.383334143596,12.2041266049073));
#59982=CARTESIAN_POINT('Ctrl Pts',(1.70553985327126,100.389666485609,12.2484474471584));
#59983=CARTESIAN_POINT('Ctrl Pts',(1.73017010000186,100.396003992062,12.2936556590329));
#59984=CARTESIAN_POINT('Ctrl Pts',(1.76510427318049,100.404992759018,12.3577764743862));
#59985=CARTESIAN_POINT('Ctrl Pts',(1.79668138150137,100.414047556875,12.423644839922));
#59986=CARTESIAN_POINT('Ctrl Pts',(1.8245316294591,100.423117001667,12.4909006139287));
#59987=CARTESIAN_POINT('Ctrl Pts',(1.84244460797566,100.428950370547,12.5341588009554));
#59988=CARTESIAN_POINT('Ctrl Pts',(1.85881590498794,100.434789699189,12.5779898849672));
#59989=CARTESIAN_POINT('Ctrl Pts',(1.87355074227944,100.440620248091,12.6222872607065));
#59990=CARTESIAN_POINT('Ctrl Pts',(1.87357203853786,100.440628674983,12.6223512836979));
#59991=CARTESIAN_POINT('Ctrl Pts',(1.87359333137863,100.440637101856,12.6224153076619));
#59992=CARTESIAN_POINT('Ctrl Pts',(1.87361462080168,100.44064552871,12.6224793325982));
#59993=CARTESIAN_POINT('Ctrl Pts',(1.90030799893165,100.451211395838,12.7027559013972));
#59994=CARTESIAN_POINT('Ctrl Pts',(1.92167142133264,100.461766833131,12.7847043625893));
#59995=CARTESIAN_POINT('Ctrl Pts',(1.93770069774032,100.47229961058,12.8675332722959));
#59996=CARTESIAN_POINT('Ctrl Pts',(1.94150753778997,100.474801070908,12.8872045539384));
#59997=CARTESIAN_POINT('Ctrl Pts',(1.94501374241068,100.47730125392,12.9069254417717));
#59998=CARTESIAN_POINT('Ctrl Pts',(1.94821967647636,100.479799997206,12.926685261519));
#59999=CARTESIAN_POINT('Ctrl Pts',(1.9590004398596,100.488202652894,12.9931326484044));
#60000=CARTESIAN_POINT('Ctrl Pts',(1.96649001887271,100.496645809469,13.0600178136398));
#60001=CARTESIAN_POINT('Ctrl Pts',(1.97057829127119,100.505060909447,13.1270246813479));
#60002=CARTESIAN_POINT('Ctrl Pts',(1.97240853228865,100.508828188054,13.1570223688249));
#60003=CARTESIAN_POINT('Ctrl Pts',(1.97355695524824,100.512589754712,13.1870437638236));
#60004=CARTESIAN_POINT('Ctrl Pts',(1.97401335744123,100.516339028903,13.2170571680248));
#60005=CARTESIAN_POINT('Ctrl Pts',(1.97499263442704,100.524383639525,13.281455272266));
#60006=CARTESIAN_POINT('Ctrl Pts',(1.97275259966565,100.532353585413,13.345826039755));
#60007=CARTESIAN_POINT('Ctrl Pts',(1.9674374615346,100.54032627025,13.4098672138259));
#60008=CARTESIAN_POINT('Ctrl Pts',(1.96413806745553,100.545275347489,13.4496210387194));
#60009=CARTESIAN_POINT('Ctrl Pts',(1.95965359226287,100.55022560885,13.4892488967257));
#60010=CARTESIAN_POINT('Ctrl Pts',(1.95401557164059,100.555196819791,13.5286880681682));
#60011=CARTESIAN_POINT('Ctrl Pts',(1.94533253058027,100.562852916073,13.5894278149629));
#60012=CARTESIAN_POINT('Ctrl Pts',(1.93382032564991,100.570502383121,13.6496950384495));
#60013=CARTESIAN_POINT('Ctrl Pts',(1.91949667738152,100.578140410089,13.7091766423013));
#60014=CARTESIAN_POINT('Ctrl Pts',(1.91270501795872,100.581762034752,13.7373802666653));
#60015=CARTESIAN_POINT('Ctrl Pts',(1.90527920058936,100.585382323055,13.7654169435566));
#60016=CARTESIAN_POINT('Ctrl Pts',(1.89723411364723,100.589001020792,13.7932606663128));
#60017=CARTESIAN_POINT('Ctrl Pts',(1.86995121684532,100.601272927563,13.8876856762602));
#60018=CARTESIAN_POINT('Ctrl Pts',(1.83554273386024,100.613526474822,13.9798896887639));
#60019=CARTESIAN_POINT('Ctrl Pts',(1.79462375037523,100.625751298097,14.0688641654385));
#60020=CARTESIAN_POINT('Ctrl Pts',(1.77730603659434,100.630925082303,14.1065199034268));
#60021=CARTESIAN_POINT('Ctrl Pts',(1.75882279384373,100.636093723609,14.1435974289194));
#60022=CARTESIAN_POINT('Ctrl Pts',(1.73922308164032,100.641256444873,14.1800216839161));
#60023=CARTESIAN_POINT('Ctrl Pts',(1.70422022775325,100.650476477095,14.2450712551733));
#60024=CARTESIAN_POINT('Ctrl Pts',(1.66570410472337,100.659721350228,14.3080859673018));
#60025=CARTESIAN_POINT('Ctrl Pts',(1.62381459103056,100.668918090935,14.3686340530643));
#60026=CARTESIAN_POINT('Ctrl Pts',(1.60866011209576,100.672245219876,14.3905386924201));
#60027=CARTESIAN_POINT('Ctrl Pts',(1.59306431364288,100.675565986668,14.4121200450159));
#60028=CARTESIAN_POINT('Ctrl Pts',(1.57703457414371,100.678876724653,14.4333561841082));
#60029=CARTESIAN_POINT('Ctrl Pts',(1.52079585687444,100.690492113506,14.5078610269577));
#60030=CARTESIAN_POINT('Ctrl Pts',(1.45935413988508,100.702131699336,14.578282915961));
#60031=CARTESIAN_POINT('Ctrl Pts',(1.39315836180106,100.713758449561,14.643758705858));
#60032=CARTESIAN_POINT('Ctrl Pts',(1.39312957784061,100.713763505229,14.6437871767455));
#60033=CARTESIAN_POINT('Ctrl Pts',(1.39310079298179,100.713768560895,14.6438156466972));
#60034=CARTESIAN_POINT('Ctrl Pts',(1.39307200722447,100.713773616559,14.6438441157133));
#60035=CARTESIAN_POINT('Ctrl Pts',(1.32191845089236,100.726270367787,14.7142147411049));
#60036=CARTESIAN_POINT('Ctrl Pts',(1.24528800902981,100.738749371248,14.7788522261899));
#60037=CARTESIAN_POINT('Ctrl Pts',(1.16430067964347,100.751204384363,14.8371779698929));
#60038=CARTESIAN_POINT('Ctrl Pts',(1.10472621250904,100.760366320867,14.8800825220944));
#60039=CARTESIAN_POINT('Ctrl Pts',(1.04279677413752,100.769515002972,14.9195711277492));
#60040=CARTESIAN_POINT('Ctrl Pts',(0.978957754214814,100.778648905549,14.9554270445908));
#60041=CARTESIAN_POINT('Ctrl Pts',(0.883515326126466,100.792304532483,15.0090333776587));
#60042=CARTESIAN_POINT('Ctrl Pts',(0.783795240018645,100.805928784227,15.0545307252639));
#60043=CARTESIAN_POINT('Ctrl Pts',(0.681176813927582,100.819530429895,15.0912367272569));
#60044=CARTESIAN_POINT('Ctrl Pts',(0.616191545489925,100.828143957003,15.1144815721025));
#60045=CARTESIAN_POINT('Ctrl Pts',(0.550044628400873,100.836748278969,15.1342003360991));
#60046=CARTESIAN_POINT('Ctrl Pts',(0.483067235435529,100.845347664371,15.1502137842078));
#60047=CARTESIAN_POINT('Ctrl Pts',(0.477040302176027,100.846121476543,15.1516547477737));
#60048=CARTESIAN_POINT('Ctrl Pts',(0.471006687997389,100.846895242936,15.1530656880532));
#60049=CARTESIAN_POINT('Ctrl Pts',(0.464966659778986,100.847668963334,15.1544464643299));
#60050=CARTESIAN_POINT('Ctrl Pts',(0.42837216229489,100.852356674741,15.1628121229257));
#60051=CARTESIAN_POINT('Ctrl Pts',(0.3915518982456,100.857041458656,15.1700683324017));
#60052=CARTESIAN_POINT('Ctrl Pts',(0.354569618166892,100.861723385158,15.1762220161701));
#60053=CARTESIAN_POINT('Ctrl Pts',(0.197073679531693,100.881662242566,15.2024286264464));
#60054=CARTESIAN_POINT('Ctrl Pts',(0.0366346791472735,100.901549900725,
15.2086399019479));
#60055=CARTESIAN_POINT('Ctrl Pts',(-0.121807786054843,100.921389366738,
15.1953830408523));
#60056=CARTESIAN_POINT('Ctrl Pts',(-0.141394222126714,100.923841893794,
15.1937442462146));
#60057=CARTESIAN_POINT('Ctrl Pts',(-0.160950110191157,100.92629367905,15.191807954743));
#60058=CARTESIAN_POINT('Ctrl Pts',(-0.180466105457516,100.92874472587,15.1895751716503));
#60059=CARTESIAN_POINT('Ctrl Pts',(-0.285412859949347,100.941925166088,
15.1775684389236));
#60060=CARTESIAN_POINT('Ctrl Pts',(-0.389203408420552,100.955083918522,
15.156988916179));
#60061=CARTESIAN_POINT('Ctrl Pts',(-0.490405259706409,100.968252572555,
15.1280211534391));
#60062=CARTESIAN_POINT('Ctrl Pts',(-0.520850058179763,100.972214130699,
15.1193067110882));
#60063=CARTESIAN_POINT('Ctrl Pts',(-0.551069765750844,100.976200068202,
15.1098567628718));
#60064=CARTESIAN_POINT('Ctrl Pts',(-0.581017382346599,100.980185608747,
15.0996490570147));
#60065=CARTESIAN_POINT('Ctrl Pts',(-0.581025570119883,100.980186698406,
15.0996462661956));
#60066=CARTESIAN_POINT('Ctrl Pts',(-0.581033757872797,100.980187788065,
15.0996434753198));
#60067=CARTESIAN_POINT('Ctrl Pts',(-0.581041945605342,100.980188877725,
15.0996406843875));
#60068=CARTESIAN_POINT('Ctrl Pts',(-0.623812244882491,100.985880936685,
15.0850616769844));
#60069=CARTESIAN_POINT('Ctrl Pts',(-0.666033261975055,100.991572632388,
15.0689345095551));
#60070=CARTESIAN_POINT('Ctrl Pts',(-0.707585192450922,100.997232238504,
15.0512956057487));
#60071=CARTESIAN_POINT('Ctrl Pts',(-0.785530363569268,101.007848808231,
15.018207675542));
#60072=CARTESIAN_POINT('Ctrl Pts',(-0.861125942375691,101.018350906553,
14.9797971836134));
#60073=CARTESIAN_POINT('Ctrl Pts',(-0.933743648892485,101.028803989415,
14.9365513449058));
#60074=CARTESIAN_POINT('Ctrl Pts',(-0.973059126825815,101.034463324697,
14.9131378979798));
#60075=CARTESIAN_POINT('Ctrl Pts',(-1.01150033413506,101.040108544714,14.8883086551989));
#60076=CARTESIAN_POINT('Ctrl Pts',(-1.04899875150532,101.045803082492,14.8621841577998));
#60077=CARTESIAN_POINT('Ctrl Pts',(-1.04901392620711,101.045805386934,14.8621735858481));
#60078=CARTESIAN_POINT('Ctrl Pts',(-1.04902910075475,101.045807691384,14.8621630136841));
#60079=CARTESIAN_POINT('Ctrl Pts',(-1.04904427514814,101.045809995841,14.8621524413079));
#60080=CARTESIAN_POINT('Ctrl Pts',(-1.14780635197162,101.060808489259,14.7933424528808));
#60081=CARTESIAN_POINT('Ctrl Pts',(-1.23983412163089,101.075803762398,14.7152570292142));
#60082=CARTESIAN_POINT('Ctrl Pts',(-1.32352871457936,101.090775856186,14.6293332957179));
#60083=CARTESIAN_POINT('Ctrl Pts',(-1.36158956475337,101.097584547146,14.5902587243294));
#60084=CARTESIAN_POINT('Ctrl Pts',(-1.39792524580788,101.104388121798,14.5495649265683));
#60085=CARTESIAN_POINT('Ctrl Pts',(-1.43240459690608,101.111214025577,14.5074087269095));
#60086=CARTESIAN_POINT('Ctrl Pts',(-1.43241988519781,101.111217052212,14.5073900346702));
#60087=CARTESIAN_POINT('Ctrl Pts',(-1.43243517312469,101.111220078851,14.5073713421434));
#60088=CARTESIAN_POINT('Ctrl Pts',(-1.43245046068667,101.111223105495,14.5073526493289));
#60089=CARTESIAN_POINT('Ctrl Pts',(-1.48051087329716,101.120738144411,14.4485869431873));
#60090=CARTESIAN_POINT('Ctrl Pts',(-1.52502073840214,101.130362355319,14.3870057519655));
#60091=CARTESIAN_POINT('Ctrl Pts',(-1.56565256142995,101.139984095314,14.3230138391529));
#60092=CARTESIAN_POINT('Ctrl Pts',(-1.58484471744172,101.14452885657,14.2927877089262));
#60093=CARTESIAN_POINT('Ctrl Pts',(-1.60317115550466,101.149072972734,14.2620243070821));
#60094=CARTESIAN_POINT('Ctrl Pts',(-1.62059515320848,101.153604182934,14.2307696225186));
#60095=CARTESIAN_POINT('Ctrl Pts',(-1.65094915067705,101.16149791348,14.1763214624438));
#60096=CARTESIAN_POINT('Ctrl Pts',(-1.67856899910062,101.169354671326,14.1203746208637));
#60097=CARTESIAN_POINT('Ctrl Pts',(-1.70332335292387,101.177202871508,14.0632424874143));
#60098=CARTESIAN_POINT('Ctrl Pts',(-1.70334055254959,101.177208324533,14.063202791314));
#60099=CARTESIAN_POINT('Ctrl Pts',(-1.70335775079447,101.177213777555,14.0631630946374));
#60100=CARTESIAN_POINT('Ctrl Pts',(-1.70337494765864,101.177219230573,14.0631233973841));
#60101=CARTESIAN_POINT('Ctrl Pts',(-1.73956596018279,101.188695175205,13.9795800386841));
#60102=CARTESIAN_POINT('Ctrl Pts',(-1.76964128316824,101.200157172918,13.8934831722751));
#60103=CARTESIAN_POINT('Ctrl Pts',(-1.79329485505532,101.211603009127,13.8057429884609));
#60104=CARTESIAN_POINT('Ctrl Pts',(-1.81475047729921,101.221985269326,13.7261558441381));
#60105=CARTESIAN_POINT('Ctrl Pts',(-1.83092241545109,101.23235382455,13.6452166785262));
#60106=CARTESIAN_POINT('Ctrl Pts',(-1.84156944772461,101.242689565247,13.5635931444862));
#60107=CARTESIAN_POINT('Ctrl Pts',(-1.8415803211725,101.242700120783,13.5635097851781));
#60108=CARTESIAN_POINT('Ctrl Pts',(-1.84159118883685,101.242710676261,13.5634264252065));
#60109=CARTESIAN_POINT('Ctrl Pts',(-1.84160205071728,101.242721231681,13.5633430645722));
#60110=CARTESIAN_POINT('Ctrl Pts',(-1.84680043505974,101.247772947181,13.523447521735));
#60111=CARTESIAN_POINT('Ctrl Pts',(-1.85067393068992,101.252811335925,13.4833998267027));
#60112=CARTESIAN_POINT('Ctrl Pts',(-1.85321962496362,101.25781362015,13.4432879472018));
#60113=CARTESIAN_POINT('Ctrl Pts',(-1.85842998682014,101.268051970917,13.3611895549859));
#60114=CARTESIAN_POINT('Ctrl Pts',(-1.85807984797538,101.278136725782,13.2788132899903));
#60115=CARTESIAN_POINT('Ctrl Pts',(-1.85234433187327,101.288149422771,13.1968274547615));
#60116=CARTESIAN_POINT('Ctrl Pts',(-1.8513286980246,101.289922451352,13.1823095651963));
#60117=CARTESIAN_POINT('Ctrl Pts',(-1.85014409132655,101.291693230341,13.1678038394538));
#60118=CARTESIAN_POINT('Ctrl Pts',(-1.84879134307173,101.293462225153,13.1533138959481));
#60119=CARTESIAN_POINT('Ctrl Pts',(-1.84158549322088,101.302885346533,13.0761285387478));
#60120=CARTESIAN_POINT('Ctrl Pts',(-1.82961053303086,101.312258858656,12.9993940513807));
#60121=CARTESIAN_POINT('Ctrl Pts',(-1.81305769334936,101.321733758925,12.9237059904937));
#60122=CARTESIAN_POINT('Ctrl Pts',(-1.80874409929264,101.324202874453,12.903982029174));
#60123=CARTESIAN_POINT('Ctrl Pts',(-1.80411954513465,101.326678912259,12.8843288675909));
#60124=CARTESIAN_POINT('Ctrl Pts',(-1.79918721630898,101.329164621995,12.864756507233));
#60125=CARTESIAN_POINT('Ctrl Pts',(-1.781259516784,101.338199513791,12.7936161984879));
#60126=CARTESIAN_POINT('Ctrl Pts',(-1.75923329448882,101.347322928088,12.7235507049475));
#60127=CARTESIAN_POINT('Ctrl Pts',(-1.73316690681723,101.356455930992,12.6551701085499));
#60128=CARTESIAN_POINT('Ctrl Pts',(-1.72493949639034,101.359338607497,12.633586940261));
#60129=CARTESIAN_POINT('Ctrl Pts',(-1.71630997222543,101.362222217204,12.6121716803674));
#60130=CARTESIAN_POINT('Ctrl Pts',(-1.70728125239787,101.365104217731,12.5909435637318));
#60131=CARTESIAN_POINT('Ctrl Pts',(-1.70175345113774,101.366868712195,12.5779467256274));
#60132=CARTESIAN_POINT('Ctrl Pts',(-1.69607614872213,101.368632562364,12.5650203364091));
#60133=CARTESIAN_POINT('Ctrl Pts',(-1.69025059179796,101.370395644794,12.5521689181993));
#60134=CARTESIAN_POINT('Ctrl Pts',(-1.69023447999782,101.370400520968,12.5521333749054));
#60135=CARTESIAN_POINT('Ctrl Pts',(-1.69021836706369,101.370405397137,12.5520978321849));
#60136=CARTESIAN_POINT('Ctrl Pts',(-1.69020225299568,101.3704102733,12.552062290038));
#60137=CARTESIAN_POINT('Ctrl Pts',(-1.65916228541274,101.379803055533,12.4835986911381));
#60138=CARTESIAN_POINT('Ctrl Pts',(-1.62385625943898,101.38925368914,12.4170512664938));
#60139=CARTESIAN_POINT('Ctrl Pts',(-1.58474965219824,101.398869160746,12.3528580433392));
#60140=CARTESIAN_POINT('Ctrl Pts',(-1.57438738692411,101.401417018373,12.335848457132));
#60141=CARTESIAN_POINT('Ctrl Pts',(-1.56375837782247,101.403976475443,12.3190038975838));
#60142=CARTESIAN_POINT('Ctrl Pts',(-1.5528714606858,101.406549577566,12.3023319367589));
#60143=CARTESIAN_POINT('Ctrl Pts',(-1.50522547062975,101.417810616538,12.2293680233106));
#60144=CARTESIAN_POINT('Ctrl Pts',(-1.45250347161367,101.429092584902,12.1598012467578));
#60145=CARTESIAN_POINT('Ctrl Pts',(-1.39521693588701,101.440235591337,12.0942983431898));
#60146=CARTESIAN_POINT('Ctrl Pts',(-1.39002164922676,101.441246144898,12.0883579183274));
#60147=CARTESIAN_POINT('Ctrl Pts',(-1.38478884617555,101.442255550578,12.082450941634));
#60148=CARTESIAN_POINT('Ctrl Pts',(-1.37951892383719,101.443263686164,12.0765779241854));
#60149=CARTESIAN_POINT('Ctrl Pts',(-1.34495561219293,101.449875644027,12.0380591530657));
#60150=CARTESIAN_POINT('Ctrl Pts',(-1.30879295146384,101.456433750153,12.0009970434627));
#60151=CARTESIAN_POINT('Ctrl Pts',(-1.27112355840083,101.462910739872,11.9655177583786));
#60152=CARTESIAN_POINT('Ctrl Pts',(-1.21153623134443,101.473156365653,11.9093948534913));
#60153=CARTESIAN_POINT('Ctrl Pts',(-1.14816421603574,101.483201663861,11.8572216830367));
#60154=CARTESIAN_POINT('Ctrl Pts',(-1.08158704318588,101.493204938719,11.8094775242596));
#60155=CARTESIAN_POINT('Ctrl Pts',(-1.07093446555862,101.494805497249,11.8018382939371));
#60156=CARTESIAN_POINT('Ctrl Pts',(-1.06019975954228,101.496404994277,11.7943123720928));
#60157=CARTESIAN_POINT('Ctrl Pts',(-1.04938521216415,101.498004094492,11.7869016371136));
#60158=CARTESIAN_POINT('Ctrl Pts',(-1.04408127981267,101.498788363964,11.7832670849099));
#60159=CARTESIAN_POINT('Ctrl Pts',(-1.03875823942205,101.499572522058,11.7796603068044));
#60160=CARTESIAN_POINT('Ctrl Pts',(-1.03341640307116,101.500356639497,11.7760815487043));
#60161=CARTESIAN_POINT('Ctrl Pts',(-1.03336341869387,101.500364416967,11.7760460518719));
#60162=CARTESIAN_POINT('Ctrl Pts',(-1.03331043248073,101.500372194422,11.7760105578119));
#60163=CARTESIAN_POINT('Ctrl Pts',(-1.03325744443199,101.500379971861,11.7759750665246));
#60164=CARTESIAN_POINT('Ctrl Pts',(-0.955872453571939,101.511738326574,
11.7241427568935));
#60165=CARTESIAN_POINT('Ctrl Pts',(-0.874575856573246,101.523063002066,
11.6782231996781));
#60166=CARTESIAN_POINT('Ctrl Pts',(-0.790359710197059,101.534440141483,
11.638646522071));
#60167=CARTESIAN_POINT('Ctrl Pts',(-0.704629111445532,101.546021875109,
11.598358140165));
#60168=CARTESIAN_POINT('Ctrl Pts',(-0.615871254096779,101.557658540445,
11.5646445337412));
#60169=CARTESIAN_POINT('Ctrl Pts',(-0.525157127555539,101.5694273881,11.5379923168064));
#60170=CARTESIAN_POINT('Ctrl Pts',(-0.486104601680084,101.574493889263,
11.5265185096809));
#60171=CARTESIAN_POINT('Ctrl Pts',(-0.44668998168622,101.579584667721,11.5163536479057));
#60172=CARTESIAN_POINT('Ctrl Pts',(-0.407001013407849,101.584704683254,
11.5075368986187));
#60173=CARTESIAN_POINT('Ctrl Pts',(-0.407000476373084,101.584704752534,
11.5075367793186));
#60174=CARTESIAN_POINT('Ctrl Pts',(-0.406999939338346,101.584704821813,
11.5075366600186));
#60175=CARTESIAN_POINT('Ctrl Pts',(-0.406999402303475,101.584704891092,
11.507536540719));
#60176=CARTESIAN_POINT('Ctrl Pts',(-0.329796015306562,101.594664396958,
11.490386184222));
#60177=CARTESIAN_POINT('Ctrl Pts',(-0.251492954156446,101.604714509963,
11.4783421362832));
#60178=CARTESIAN_POINT('Ctrl Pts',(-0.172779497151643,101.614698161061,
11.4713970122687));
#60179=CARTESIAN_POINT('Ctrl Pts',(-0.0732229176585234,101.627325457485,
11.4626128371436));
#60180=CARTESIAN_POINT('Ctrl Pts',(0.0270156898914488,101.639845380572,
11.4619757156826));
#60181=CARTESIAN_POINT('Ctrl Pts',(0.126710271978849,101.652303314665,11.4692731564523));
#60182=CARTESIAN_POINT('Ctrl Pts',(0.144363878509435,101.654509326888,11.4705653645676));
#60183=CARTESIAN_POINT('Ctrl Pts',(0.162000461720921,101.656713399613,11.4721064977722));
#60184=CARTESIAN_POINT('Ctrl Pts',(0.179613246981865,101.658915790235,11.4738955420251));
#60185=CARTESIAN_POINT('Ctrl Pts',(0.299670272934969,101.673928320291,11.4860905088702));
#60186=CARTESIAN_POINT('Ctrl Pts',(0.418621183774718,101.688864860963,11.509803609733));
#60187=CARTESIAN_POINT('Ctrl Pts',(0.534175038594159,101.703818319451,11.5446916778135));
#60188=CARTESIAN_POINT('Ctrl Pts',(0.625510733876132,101.715637782592,11.5722677890575));
#60189=CARTESIAN_POINT('Ctrl Pts',(0.714723094408206,101.727469194262,11.6068287669749));
#60190=CARTESIAN_POINT('Ctrl Pts',(0.800618974009707,101.739347773171,11.6481618141023));
#60191=CARTESIAN_POINT('Ctrl Pts',(0.822690628825449,101.742400072007,11.6587826815166));
#60192=CARTESIAN_POINT('Ctrl Pts',(0.84454346195733,101.745455492811,11.6698504774106));
#60193=CARTESIAN_POINT('Ctrl Pts',(0.866157592691843,101.748514648518,11.6813611589937));
#60194=CARTESIAN_POINT('Ctrl Pts',(0.882327175044809,101.750803210141,11.6899723271264));
#60195=CARTESIAN_POINT('Ctrl Pts',(0.898362881185585,101.753093780665,11.6988312276732));
#60196=CARTESIAN_POINT('Ctrl Pts',(0.914256168507836,101.755386520252,11.7079359260225));
#60197=CARTESIAN_POINT('Ctrl Pts',(0.914257785080811,101.755386753456,11.7079368520996));
#60198=CARTESIAN_POINT('Ctrl Pts',(0.914259401652273,101.75538698666,11.7079377781792));
#60199=CARTESIAN_POINT('Ctrl Pts',(0.914261018222301,101.755387219864,11.7079387042614));
#60200=CARTESIAN_POINT('Ctrl Pts',(0.940937878451754,101.759235587764,11.7232210393108));
#60201=CARTESIAN_POINT('Ctrl Pts',(0.967219185296116,101.763089293198,11.7391999111188));
#60202=CARTESIAN_POINT('Ctrl Pts',(0.993078145908535,101.766939862247,11.7558493116055));
#60203=CARTESIAN_POINT('Ctrl Pts',(1.09706050237409,101.782423517972,11.8227987888986));
#60204=CARTESIAN_POINT('Ctrl Pts',(1.19422509448536,101.797855820889,11.9005944041794));
#60205=CARTESIAN_POINT('Ctrl Pts',(1.28287524634823,101.813292829038,11.9873054502622));
#60206=CARTESIAN_POINT('Ctrl Pts',(1.37094245719128,101.828628327318,12.0734463063953));
#60207=CARTESIAN_POINT('Ctrl Pts',(1.45060397515945,101.843969870604,12.1683902843922));
#60208=CARTESIAN_POINT('Ctrl Pts',(1.52013310260964,101.859376807715,12.2701898116273));
#60209=CARTESIAN_POINT('Ctrl Pts',(1.55646790317967,101.867428224551,12.3233886026356));
#60210=CARTESIAN_POINT('Ctrl Pts',(1.59003475840863,101.875497444833,12.3784582390317));
#60211=CARTESIAN_POINT('Ctrl Pts',(1.6205862173276,101.883591653322,12.4351093933504));
#60212=CARTESIAN_POINT('Ctrl Pts',(1.62059035214418,101.883592748787,12.4351170604845));
#60213=CARTESIAN_POINT('Ctrl Pts',(1.62059448690538,101.883593844252,12.4351247276477));
#60214=CARTESIAN_POINT('Ctrl Pts',(1.62059862161118,101.883594939718,12.4351323948399));
#60215=CARTESIAN_POINT('Ctrl Pts',(1.6664257952741,101.895736572376,12.5201120196885));
#60216=CARTESIAN_POINT('Ctrl Pts',(1.70544966603001,101.907870263664,12.6086609400639));
#60217=CARTESIAN_POINT('Ctrl Pts',(1.73736806302339,101.919867668819,12.6996931149193));
#60218=CARTESIAN_POINT('Ctrl Pts',(1.76962662516437,101.931992934377,12.791695450438));
#60219=CARTESIAN_POINT('Ctrl Pts',(1.79464393036553,101.943983508552,12.8862714787962));
#60220=CARTESIAN_POINT('Ctrl Pts',(1.81216092264036,101.955985694475,12.9823149943274));
#60221=CARTESIAN_POINT('Ctrl Pts',(1.81308726913102,101.956620402913,12.9873940382733));
#60222=CARTESIAN_POINT('Ctrl Pts',(1.8139926307371,101.957255144673,12.9924771935236));
#60223=CARTESIAN_POINT('Ctrl Pts',(1.81487696576785,101.957889941672,12.9975642987641));
#60224=CARTESIAN_POINT('Ctrl Pts',(1.82899891315167,101.968027015858,13.0788002897002));
#60225=CARTESIAN_POINT('Ctrl Pts',(1.83779581543448,101.978310040119,13.1610389512985));
#60226=CARTESIAN_POINT('Ctrl Pts',(1.84103497551246,101.988621501177,13.2435190816003));
#60227=CARTESIAN_POINT('Ctrl Pts',(1.84178424014302,101.991006691435,13.262597930089));
#60228=CARTESIAN_POINT('Ctrl Pts',(1.84223632106058,101.993393393443,13.2816895896245));
#60229=CARTESIAN_POINT('Ctrl Pts',(1.84238869790875,101.995780135486,13.3007844682262));
#60230=CARTESIAN_POINT('Ctrl Pts',(1.84272083135378,102.000982479981,13.3424052780066));
#60231=CARTESIAN_POINT('Ctrl Pts',(1.84162862701176,102.006184700812,13.3840388243844));
#60232=CARTESIAN_POINT('Ctrl Pts',(1.83909409203655,102.011384338421,13.4255758404419));
#60233=CARTESIAN_POINT('Ctrl Pts',(1.83779789651504,102.014043503533,13.4468184331532));
#60234=CARTESIAN_POINT('Ctrl Pts',(1.83612393970882,102.016703302959,13.4680462597766));
#60235=CARTESIAN_POINT('Ctrl Pts',(1.83407633900791,102.019363590456,13.4892456201563));
#60236=CARTESIAN_POINT('Ctrl Pts',(1.82766919708152,102.027687889014,13.5555804825347));
#60237=CARTESIAN_POINT('Ctrl Pts',(1.81760231663384,102.036016924254,13.621636062974));
#60238=CARTESIAN_POINT('Ctrl Pts',(1.8040139429858,102.044345796022,13.6869904507889));
#60239=CARTESIAN_POINT('Ctrl Pts',(1.79101315962279,102.052314509595,13.749518775356));
#60240=CARTESIAN_POINT('Ctrl Pts',(1.77479143474322,102.060282887811,13.8114041897799));
#60241=CARTESIAN_POINT('Ctrl Pts',(1.75545902205749,102.068254622193,13.8723411019657));
#60242=CARTESIAN_POINT('Ctrl Pts',(1.73933737379134,102.074902395539,13.9231574941385));
#60243=CARTESIAN_POINT('Ctrl Pts',(1.72105119034358,102.081552937498,13.9733176567778));
#60244=CARTESIAN_POINT('Ctrl Pts',(1.70065806726025,102.088208317205,14.02264184491));
#60245=CARTESIAN_POINT('Ctrl Pts',(1.6779294041025,102.095625910034,14.0776149283855));
#60246=CARTESIAN_POINT('Ctrl Pts',(1.65258423716673,102.103049168786,14.1315469654491));
#60247=CARTESIAN_POINT('Ctrl Pts',(1.62470540352126,102.110478898782,14.1841714827423));
#60248=CARTESIAN_POINT('Ctrl Pts',(1.587534538446,102.120384962097,14.2543357821828));
#60249=CARTESIAN_POINT('Ctrl Pts',(1.5458600144321,102.130301369684,14.3221648529801));
#60250=CARTESIAN_POINT('Ctrl Pts',(1.49995615465894,102.140215749872,14.3869384221161));
#60251=CARTESIAN_POINT('Ctrl Pts',(1.48734045478903,102.142940506472,14.4047400604044));
#60252=CARTESIAN_POINT('Ctrl Pts',(1.47439954153894,102.145666410903,14.4223195999312));
#60253=CARTESIAN_POINT('Ctrl Pts',(1.46114438841258,102.148393241876,14.4396669702997));
#60254=CARTESIAN_POINT('Ctrl Pts',(1.4160858220106,102.157662625134,14.4986363109174));
#60255=CARTESIAN_POINT('Ctrl Pts',(1.3673941495347,102.166942663326,14.554920683033));
#60256=CARTESIAN_POINT('Ctrl Pts',(1.31552286783466,102.17622408939,14.6081351998545));
#60257=CARTESIAN_POINT('Ctrl Pts',(1.26336195040341,102.185557340521,14.6616468526824));
#60258=CARTESIAN_POINT('Ctrl Pts',(1.20798779172185,102.194892123591,14.712057171807));
#60259=CARTESIAN_POINT('Ctrl Pts',(1.14981223697842,102.204229756255,14.759048787269));
#60260=CARTESIAN_POINT('Ctrl Pts',(1.10365938611782,102.211637650681,14.7963289993731));
#60261=CARTESIAN_POINT('Ctrl Pts',(1.05574721904259,102.219046787273,14.8314554930974));
#60262=CARTESIAN_POINT('Ctrl Pts',(1.00625472402403,102.22646140787,14.8642839688946));
#60263=CARTESIAN_POINT('Ctrl Pts',(0.957401217845584,102.233780299613,14.8966886020533));
#60264=CARTESIAN_POINT('Ctrl Pts',(0.906999077813325,102.24110575819,14.9268587964748));
#60265=CARTESIAN_POINT('Ctrl Pts',(0.855243661351061,102.248437734779,14.9546304809421));
#60266=CARTESIAN_POINT('Ctrl Pts',(0.811904162093474,102.254577463056,14.9778862284681));
#60267=CARTESIAN_POINT('Ctrl Pts',(0.767613285959494,102.260722091471,14.9994610717527));
#60268=CARTESIAN_POINT('Ctrl Pts',(0.722496403019601,102.266870227603,15.0192545554209));
#60269=CARTESIAN_POINT('Ctrl Pts',(0.715359425450396,102.267842792789,15.0223856593392));
#60270=CARTESIAN_POINT('Ctrl Pts',(0.708201875033396,102.26881543306,15.0254721527729));
#60271=CARTESIAN_POINT('Ctrl Pts',(0.701024298372724,102.269788136874,15.0285136309998));
#60272=CARTESIAN_POINT('Ctrl Pts',(0.615939180428338,102.281318855751,15.0645682140294));
#60273=CARTESIAN_POINT('Ctrl Pts',(0.528030250094319,102.292859831511,15.094301342847));
#60274=CARTESIAN_POINT('Ctrl Pts',(0.438327753451193,102.304412015396,15.1174064003212));
#60275=CARTESIAN_POINT('Ctrl Pts',(0.326028892076433,102.318874233787,15.1463317005464));
#60276=CARTESIAN_POINT('Ctrl Pts',(0.2109168522982,102.333354294598,15.1648692645029));
#60277=CARTESIAN_POINT('Ctrl Pts',(0.0950175608262004,102.347853139992,
15.1724149891679));
#60278=CARTESIAN_POINT('Ctrl Pts',(0.0714651087958735,102.350799520046,
15.1739483921417));
#60279=CARTESIAN_POINT('Ctrl Pts',(0.0478803795012013,102.353746645807,
15.1750278648192));
#60280=CARTESIAN_POINT('Ctrl Pts',(0.0242805671923874,102.356694499776,
15.1756483834939));
#60281=CARTESIAN_POINT('Ctrl Pts',(-0.0380995050157335,102.36448639833,
15.1772885660185));
#60282=CARTESIAN_POINT('Ctrl Pts',(-0.100574621710386,102.372282104824,
15.175721745767));
#60283=CARTESIAN_POINT('Ctrl Pts',(-0.162848598268233,102.380081104816,
15.1710433231385));
#60284=CARTESIAN_POINT('Ctrl Pts',(-0.16935289488909,102.380895682784,15.1705546784401));
#60285=CARTESIAN_POINT('Ctrl Pts',(-0.175854998454186,102.381710296692,
15.170032090788));
#60286=CARTESIAN_POINT('Ctrl Pts',(-0.182354572319706,102.382524945955,
15.1694756700676));
#60287=CARTESIAN_POINT('Ctrl Pts',(-0.282839184518071,102.395119574,15.1608733029789));
#60288=CARTESIAN_POINT('Ctrl Pts',(-0.382747780320032,102.407726159361,
15.1441862030543));
#60289=CARTESIAN_POINT('Ctrl Pts',(-0.480937897916016,102.420370641684,
15.119773069128));
#60290=CARTESIAN_POINT('Ctrl Pts',(-0.501012570839243,102.422955767897,
15.1147818776456));
#60291=CARTESIAN_POINT('Ctrl Pts',(-0.521015380460676,102.425542478708,
15.1094675780936));
#60292=CARTESIAN_POINT('Ctrl Pts',(-0.540936493039643,102.428130996603,
15.1038329779157));
#60293=CARTESIAN_POINT('Ctrl Pts',(-0.658381045798903,102.443391556239,
15.0706142962156));
#60294=CARTESIAN_POINT('Ctrl Pts',(-0.772985749299366,102.458653750469,
15.0262582844338));
#60295=CARTESIAN_POINT('Ctrl Pts',(-0.88256931461987,102.473947768897,14.9713889903129));
#60296=CARTESIAN_POINT('Ctrl Pts',(-0.969660333172714,102.486102617472,
14.9277818791709));
#60297=CARTESIAN_POINT('Ctrl Pts',(-1.05357673346733,102.498277424713,14.8775317112844));
#60298=CARTESIAN_POINT('Ctrl Pts',(-1.13316354042019,102.510478295086,14.8210130851769));
#60299=CARTESIAN_POINT('Ctrl Pts',(-1.151776491269,102.513331710234,14.8077950852337));
#60300=CARTESIAN_POINT('Ctrl Pts',(-1.17015275037832,102.51618655043,14.794234422748));
#60301=CARTESIAN_POINT('Ctrl Pts',(-1.18827778456024,102.519042892776,14.7803362314562));
#60302=CARTESIAN_POINT('Ctrl Pts',(-1.21584666837573,102.523387500872,14.7591965405114));
#60303=CARTESIAN_POINT('Ctrl Pts',(-1.24283357738955,102.527735467329,14.7372764277728));
#60304=CARTESIAN_POINT('Ctrl Pts',(-1.26918653405338,102.532086809549,14.7145960189609));
#60305=CARTESIAN_POINT('Ctrl Pts',(-1.26919696311563,102.532088531573,14.7145870432927));
#60306=CARTESIAN_POINT('Ctrl Pts',(-1.26920739207869,102.532090253597,14.7145780675054));
#60307=CARTESIAN_POINT('Ctrl Pts',(-1.26921782094239,102.532091975622,14.714569091599));
#60308=CARTESIAN_POINT('Ctrl Pts',(-1.28456090482882,102.534625441661,14.7013636180524));
#60309=CARTESIAN_POINT('Ctrl Pts',(-1.29969240282331,102.537159012642,14.6878976203342));
#60310=CARTESIAN_POINT('Ctrl Pts',(-1.31460648803677,102.539692695173,14.6741800832161));
#60311=CARTESIAN_POINT('Ctrl Pts',(-1.39473833968511,102.553305911791,14.6004771618771));
#60312=CARTESIAN_POINT('Ctrl Pts',(-1.46859534561534,102.566922618664,14.5195113086034));
#60313=CARTESIAN_POINT('Ctrl Pts',(-1.53520819985887,102.580549113367,14.4327271126073));
#60314=CARTESIAN_POINT('Ctrl Pts',(-1.56437067294813,102.586514662953,14.3947338182342));
#60315=CARTESIAN_POINT('Ctrl Pts',(-1.5921446874049,102.592482079263,14.3556253967641));
#60316=CARTESIAN_POINT('Ctrl Pts',(-1.61844847607299,102.598453269443,14.3155236653087));
#60317=CARTESIAN_POINT('Ctrl Pts',(-1.61845152457497,102.598453961479,14.3155190176814));
#60318=CARTESIAN_POINT('Ctrl Pts',(-1.61845457305721,102.598454653516,14.3155143700407));
#60319=CARTESIAN_POINT('Ctrl Pts',(-1.61845762151969,102.598455345553,14.3155097223866));
#60320=CARTESIAN_POINT('Ctrl Pts',(-1.67094957347155,102.610371634069,14.2354810411373));
#60321=CARTESIAN_POINT('Ctrl Pts',(-1.71758551027082,102.622325341605,14.1514964047542));
#60322=CARTESIAN_POINT('Ctrl Pts',(-1.7577644917214,102.634297942855,14.0644150502798));
#60323=CARTESIAN_POINT('Ctrl Pts',(-1.7795209022467,102.640780955077,14.0172615976874));
#60324=CARTESIAN_POINT('Ctrl Pts',(-1.79938391606633,102.647269470249,13.9692004169408));
#60325=CARTESIAN_POINT('Ctrl Pts',(-1.81725750356379,102.653763399263,13.9203696200825));
#60326=CARTESIAN_POINT('Ctrl Pts',(-1.82773260126707,102.657569268729,13.8917515618392));
#60327=CARTESIAN_POINT('Ctrl Pts',(-1.83752439343444,102.661376997973,13.86286916227));
#60328=CARTESIAN_POINT('Ctrl Pts',(-1.84661362179659,102.665186567981,13.8337502505934));
#60329=CARTESIAN_POINT('Ctrl Pts',(-1.86607209132476,102.673342200006,13.7714116853185));
#60330=CARTESIAN_POINT('Ctrl Pts',(-1.88230101863283,102.681502005255,13.7080220587029));
#60331=CARTESIAN_POINT('Ctrl Pts',(-1.89528967154877,102.689668313321,13.6439064532373));
#60332=CARTESIAN_POINT('Ctrl Pts',(-1.90747059011716,102.697326777536,13.5837780492995));
#60333=CARTESIAN_POINT('Ctrl Pts',(-1.91680197140128,102.704990534476,13.5230145044515));
#60334=CARTESIAN_POINT('Ctrl Pts',(-1.92327094072407,102.712665487171,13.461849798818));
#60335=CARTESIAN_POINT('Ctrl Pts',(-1.93042148727562,102.721149080737,13.3942407171976));
#60336=CARTESIAN_POINT('Ctrl Pts',(-1.93407349653831,102.729645648482,13.3261467485587));
#60337=CARTESIAN_POINT('Ctrl Pts',(-1.93418979043081,102.738159614938,13.257911754622));
#60338=CARTESIAN_POINT('Ctrl Pts',(-1.93434417440255,102.749462185765,13.1673275532573));
#60339=CARTESIAN_POINT('Ctrl Pts',(-1.92825964438706,102.760808710744,13.0764949618271));
#60340=CARTESIAN_POINT('Ctrl Pts',(-1.91585938591349,102.772173558771,12.9863960700822));
#60341=CARTESIAN_POINT('Ctrl Pts',(-1.9138656038006,102.774000861868,12.9719094721507));
#60342=CARTESIAN_POINT('Ctrl Pts',(-1.91170865694649,102.775828638566,12.9574418448425));
#60343=CARTESIAN_POINT('Ctrl Pts',(-1.90938835218873,102.777656782239,12.942997266508));
#60344=CARTESIAN_POINT('Ctrl Pts',(-1.89995256426744,102.785091140129,12.8842567164484));
#60345=CARTESIAN_POINT('Ctrl Pts',(-1.8878157775183,102.792517866429,12.8259022336328));
#60346=CARTESIAN_POINT('Ctrl Pts',(-1.87298374690933,102.799937257785,12.7682421088022));
#60347=CARTESIAN_POINT('Ctrl Pts',(-1.8729798057892,102.799939229242,12.7682267875367));
#60348=CARTESIAN_POINT('Ctrl Pts',(-1.87297586447891,102.799941200699,12.7682114663202));
#60349=CARTESIAN_POINT('Ctrl Pts',(-1.87297192297847,102.799943172155,12.7681961451527));
#60350=CARTESIAN_POINT('Ctrl Pts',(-1.85503528338224,102.808914704184,12.6984739003073));
#60351=CARTESIAN_POINT('Ctrl Pts',(-1.83312581629033,102.817917013102,12.6296507484991));
#60352=CARTESIAN_POINT('Ctrl Pts',(-1.80744518956224,102.826929347774,12.5621627833291));
#60353=CARTESIAN_POINT('Ctrl Pts',(-1.77925088720554,102.836823829377,12.4880689492654));
#60354=CARTESIAN_POINT('Ctrl Pts',(-1.74651361060821,102.846730296013,12.4155844666192));
#60355=CARTESIAN_POINT('Ctrl Pts',(-1.70947907627453,102.856651617251,12.3452247196208));
#60356=CARTESIAN_POINT('Ctrl Pts',(-1.69542614491709,102.860416310094,12.3185263767718));
#60357=CARTESIAN_POINT('Ctrl Pts',(-1.68075401715658,102.864183244747,12.2921332498829));
#60358=CARTESIAN_POINT('Ctrl Pts',(-1.66547438252735,102.86795287411,12.2660717160896));
#60359=CARTESIAN_POINT('Ctrl Pts',(-1.63366447046097,102.875800678163,12.2118155039226));
#60360=CARTESIAN_POINT('Ctrl Pts',(-1.59922589293084,102.883658946406,12.1590052148897));
#60361=CARTESIAN_POINT('Ctrl Pts',(-1.56231253061641,102.89152602577,12.1079052427554));
#60362=CARTESIAN_POINT('Ctrl Pts',(-1.5265805530251,102.899141325106,12.0584406872466));
#60363=CARTESIAN_POINT('Ctrl Pts',(-1.48853265842265,102.906764399259,12.010581333861));
#60364=CARTESIAN_POINT('Ctrl Pts',(-1.44829244275389,102.91439729182,11.9645434850451));
#60365=CARTESIAN_POINT('Ctrl Pts',(-1.40956940665713,102.921742400916,11.9202414043558));
#60366=CARTESIAN_POINT('Ctrl Pts',(-1.36881158033374,102.929097353996,11.8776221213014));
#60367=CARTESIAN_POINT('Ctrl Pts',(-1.32614769321825,102.936461761375,11.8369019475121));
#60368=CARTESIAN_POINT('Ctrl Pts',(-1.32614712479651,102.936461859493,11.8369014049869));
#60369=CARTESIAN_POINT('Ctrl Pts',(-1.32614655637446,102.936461957611,11.8369008624621));
#60370=CARTESIAN_POINT('Ctrl Pts',(-1.32614598795205,102.936462055729,11.8369003199376));
#60371=CARTESIAN_POINT('Ctrl Pts',(-1.26598108840654,102.946847380366,11.7794765976501));
#60372=CARTESIAN_POINT('Ctrl Pts',(-1.20204608060229,102.957302316582,11.725860928667));
#60373=CARTESIAN_POINT('Ctrl Pts',(-1.13488521307142,102.967748055726,11.676348725627));
#60374=CARTESIAN_POINT('Ctrl Pts',(-1.06602794478382,102.978457641369,11.6255859053483));
#60375=CARTESIAN_POINT('Ctrl Pts',(-0.993778276255049,102.989157524831,
11.5791364441837));
#60376=CARTESIAN_POINT('Ctrl Pts',(-0.91872494735699,102.999860013816,11.5373700252457));
#60377=CARTESIAN_POINT('Ctrl Pts',(-0.843891976344137,103.010531080106,
11.4957262332436));
#60378=CARTESIAN_POINT('Ctrl Pts',(-0.766271104913007,103.021204517336,
11.4587392283868));
#60379=CARTESIAN_POINT('Ctrl Pts',(-0.686476193102858,103.031898548805,
11.4267986738155));
#60380=CARTESIAN_POINT('Ctrl Pts',(-0.607735369721644,103.042451312433,
11.395280053027));
#60381=CARTESIAN_POINT('Ctrl Pts',(-0.526875037269166,103.053059105642,
11.3686857904221));
#60382=CARTESIAN_POINT('Ctrl Pts',(-0.444524447119211,103.063682235268,
11.3473774222192));
#60383=CARTESIAN_POINT('Ctrl Pts',(-0.415305104344762,103.067451496245,
11.3398168629889));
#60384=CARTESIAN_POINT('Ctrl Pts',(-0.385898388663963,103.071222664651,
11.3329216111304));
#60385=CARTESIAN_POINT('Ctrl Pts',(-0.356333030015614,103.074995438591,
11.3267075705126));
#60386=CARTESIAN_POINT('Ctrl Pts',(-0.327472646434759,103.078678252128,
11.3206417014004));
#60387=CARTESIAN_POINT('Ctrl Pts',(-0.298451485147569,103.082363820692,
11.3152229434911));
#60388=CARTESIAN_POINT('Ctrl Pts',(-0.26930238812307,103.086051687325,11.3104518308713));
#60389=CARTESIAN_POINT('Ctrl Pts',(-0.20458121217553,103.094240039269,11.2998582945064));
#60390=CARTESIAN_POINT('Ctrl Pts',(-0.139230056703358,103.102439623834,
11.2924587532058));
#60391=CARTESIAN_POINT('Ctrl Pts',(-0.0736083162059315,103.110645640778,
11.2882471963228));
#60392=CARTESIAN_POINT('Ctrl Pts',(-0.00798657570850504,103.118851657722,
11.2840356394398));
#60393=CARTESIAN_POINT('Ctrl Pts',(0.0579131368202692,103.127065048991,
11.2830092363397));
#60394=CARTESIAN_POINT('Ctrl Pts',(0.123805004717542,103.135290075073,11.2851582785366));
#60395=CARTESIAN_POINT('Ctrl Pts',(0.214244652810041,103.146579305265,11.2881079387334));
#60396=CARTESIAN_POINT('Ctrl Pts',(0.304695613052521,103.157893607708,11.2970399445611));
#60397=CARTESIAN_POINT('Ctrl Pts',(0.394391122754232,103.169243831579,11.3119717209192));
#60398=CARTESIAN_POINT('Ctrl Pts',(0.471293148687995,103.178975146039,11.3247737425203));
#60399=CARTESIAN_POINT('Ctrl Pts',(0.547630135722643,103.188856484811,11.3420316864373));
#60400=CARTESIAN_POINT('Ctrl Pts',(0.6228077283068,103.198711670681,11.3636742783697));
#60401=CARTESIAN_POINT('Ctrl Pts',(0.636214023632117,103.200469129622,11.3675337658722));
#60402=CARTESIAN_POINT('Ctrl Pts',(0.649583533381155,103.202225764564,11.371532585887));
#60403=CARTESIAN_POINT('Ctrl Pts',(0.662913004719139,103.2039805866,11.3756702041141));
#60404=CARTESIAN_POINT('Ctrl Pts',(0.693468921848236,103.208003266522,11.3851551053867));
#60405=CARTESIAN_POINT('Ctrl Pts',(0.723812672012547,103.212016229393,11.3953690133007));
#60406=CARTESIAN_POINT('Ctrl Pts',(0.753899777174038,103.216013772683,11.4063046363991));
#60407=CARTESIAN_POINT('Ctrl Pts',(0.753902936989191,103.216014192514,11.4063057848827));
#60408=CARTESIAN_POINT('Ctrl Pts',(0.753906096801517,103.216014612345,11.4063069333743));
#60409=CARTESIAN_POINT('Ctrl Pts',(0.753909256611011,103.216015032176,11.4063080818738));
#60410=CARTESIAN_POINT('Ctrl Pts',(0.831077829019071,103.226268096064,11.4343566304229));
#60411=CARTESIAN_POINT('Ctrl Pts',(0.906727440592672,103.236537191423,11.4672517312917));
#60412=CARTESIAN_POINT('Ctrl Pts',(0.980272721481336,103.246808793055,11.5046490674096));
#60413=CARTESIAN_POINT('Ctrl Pts',(1.05449406478093,103.257174816025,11.542390177226));
#60414=CARTESIAN_POINT('Ctrl Pts',(1.12657224304582,103.267543619923,11.5847147858458));
#60415=CARTESIAN_POINT('Ctrl Pts',(1.195954914188,103.277912779759,11.6312655663058));
#60416=CARTESIAN_POINT('Ctrl Pts',(1.26536731042619,103.288286381977,11.6778362901666));
#60417=CARTESIAN_POINT('Ctrl Pts',(1.33208389772585,103.298660751963,11.7286358289529));
#60418=CARTESIAN_POINT('Ctrl Pts',(1.39557045685016,103.309115263228,11.7833497909187));
#60419=CARTESIAN_POINT('Ctrl Pts',(1.45852793730277,103.319482649611,11.8376077825071));
#60420=CARTESIAN_POINT('Ctrl Pts',(1.51832441931271,103.32987163696,11.8956962147245));
#60421=CARTESIAN_POINT('Ctrl Pts',(1.57448689960039,103.340282729759,11.9573233898565));
#60422=CARTESIAN_POINT('Ctrl Pts',(1.6076778484669,103.346435485958,11.9937438685839));
#60423=CARTESIAN_POINT('Ctrl Pts',(1.63960000505281,103.352596068282,12.031401157824));
#60424=CARTESIAN_POINT('Ctrl Pts',(1.67015586494958,103.358766683304,12.0702437448549));
#60425=CARTESIAN_POINT('Ctrl Pts',(1.68429678126935,103.361622376155,12.088219667467));
#60426=CARTESIAN_POINT('Ctrl Pts',(1.69813887463945,103.364478977697,12.106441678321));
#60427=CARTESIAN_POINT('Ctrl Pts',(1.71167812354762,103.36733676856,12.1248998638413));
#60428=CARTESIAN_POINT('Ctrl Pts',(1.76588854289307,103.378779208398,12.1988054389729));
#60429=CARTESIAN_POINT('Ctrl Pts',(1.81524252832232,103.390240048391,12.2764916368507));
#60430=CARTESIAN_POINT('Ctrl Pts',(1.85941492971959,103.401726965554,12.3572704625853));
#60431=CARTESIAN_POINT('Ctrl Pts',(1.89162372670102,103.410102778757,12.4161712403602));
#60432=CARTESIAN_POINT('Ctrl Pts',(1.92107843238021,103.418492896569,12.4767200850574));
#60433=CARTESIAN_POINT('Ctrl Pts',(1.94763876734934,103.426898617052,12.5386425155357));
#60434=CARTESIAN_POINT('Ctrl Pts',(1.9916465790334,103.440826053001,12.6412417735148));
#60435=CARTESIAN_POINT('Ctrl Pts',(2.02770239861494,103.4547950446,12.7476036022882));
#60436=CARTESIAN_POINT('Ctrl Pts',(2.05514361094351,103.468802788122,12.8564086888768));
#60437=CARTESIAN_POINT('Ctrl Pts',(2.07383108038386,103.478342063424,12.9305049680876));
#60438=CARTESIAN_POINT('Ctrl Pts',(2.08852214736075,103.487899095292,13.0057325280781));
#60439=CARTESIAN_POINT('Ctrl Pts',(2.09901135869357,103.497469170066,13.0816417223927));
#60440=CARTESIAN_POINT('Ctrl Pts',(2.10151813830666,103.499756288476,13.0997829929532));
#60441=CARTESIAN_POINT('Ctrl Pts',(2.10378500003126,103.50204413754,13.1179630708559));
#60442=CARTESIAN_POINT('Ctrl Pts',(2.10580936422368,103.504332751059,13.1361765897923));
#60443=CARTESIAN_POINT('Ctrl Pts',(2.1141529711838,103.51376548641,13.2112453170178));
#60444=CARTESIAN_POINT('Ctrl Pts',(2.11837768012527,103.523211823801,13.2868869077833));
#60445=CARTESIAN_POINT('Ctrl Pts',(2.11854006212329,103.532671927025,13.3626648484844));
#60446=CARTESIAN_POINT('Ctrl Pts',(2.11870409170741,103.542228015856,13.4392116594046));
#60447=CARTESIAN_POINT('Ctrl Pts',(2.11472397092425,103.551799338126,13.5159072693305));
#60448=CARTESIAN_POINT('Ctrl Pts',(2.10664856791811,103.561389659365,13.5923313907327));
#60449=CARTESIAN_POINT('Ctrl Pts',(2.09854131514464,103.57101780528,13.6690569324458));
#60450=CARTESIAN_POINT('Ctrl Pts',(2.08630637981466,103.580664825254,13.7455068118658));
#60451=CARTESIAN_POINT('Ctrl Pts',(2.06998377103888,103.590333688978,13.8212470882111));
#60452=CARTESIAN_POINT('Ctrl Pts',(2.05180076205487,103.601104579733,13.90562000581));
#60453=CARTESIAN_POINT('Ctrl Pts',(2.02854198299513,103.611902775125,13.9891132148051));
#60454=CARTESIAN_POINT('Ctrl Pts',(2.00028426875198,103.622722405094,14.0710475380929));
#60455=CARTESIAN_POINT('Ctrl Pts',(1.98078817873922,103.630187286293,14.1275771967981));
#60456=CARTESIAN_POINT('Ctrl Pts',(1.95891301016525,103.637662366928,14.1833647902223));
#60457=CARTESIAN_POINT('Ctrl Pts',(1.93469031992368,103.645145688019,14.238189090484));
#60458=CARTESIAN_POINT('Ctrl Pts',(1.92670015647016,103.647614156967,14.2562735854739));
#60459=CARTESIAN_POINT('Ctrl Pts',(1.91845496550383,103.65008341462,14.274252500844));
#60460=CARTESIAN_POINT('Ctrl Pts',(1.90995524976028,103.652553614003,14.2921195862409));
#60461=CARTESIAN_POINT('Ctrl Pts',(1.89491267730729,103.656925307634,14.3237402821224));
#60462=CARTESIAN_POINT('Ctrl Pts',(1.87906984952767,103.661300828955,14.3550170548085));
#60463=CARTESIAN_POINT('Ctrl Pts',(1.86245045886573,103.665680166301,14.3859142415477));
#60464=CARTESIAN_POINT('Ctrl Pts',(1.82578231744815,103.675342503772,14.4540841543806));
#60465=CARTESIAN_POINT('Ctrl Pts',(1.78533663347209,103.685022518145,14.5203994452426));
#60466=CARTESIAN_POINT('Ctrl Pts',(1.741384462713,103.69471746067,14.5844623370871));
#60467=CARTESIAN_POINT('Ctrl Pts',(1.69810640721786,103.704263707268,14.6475426660116));
#60468=CARTESIAN_POINT('Ctrl Pts',(1.65142912045016,103.713824666201,14.7084418930771));
#60469=CARTESIAN_POINT('Ctrl Pts',(1.60157737672231,103.723404640978,14.766824779694));
#60470=CARTESIAN_POINT('Ctrl Pts',(1.55049795325477,103.733220538113,14.8266454392288));
#60471=CARTESIAN_POINT('Ctrl Pts',(1.49608623762861,103.743056026327,14.8838207915626));
#60472=CARTESIAN_POINT('Ctrl Pts',(1.43861834771889,103.752908804079,14.9379465120586));
#60473=CARTESIAN_POINT('Ctrl Pts',(1.37072344167981,103.764549277058,15.0018928430121));
#60474=CARTESIAN_POINT('Ctrl Pts',(1.29855742573973,103.776214953096,15.0615893537912));
#60475=CARTESIAN_POINT('Ctrl Pts',(1.22272263305689,103.787907076375,15.1165784625959));
#60476=CARTESIAN_POINT('Ctrl Pts',(1.09926103729112,103.806942246735,15.2061025831557));
#60477=CARTESIAN_POINT('Ctrl Pts',(0.966078309936567,103.826046911828,15.2831457798114));
#60478=CARTESIAN_POINT('Ctrl Pts',(0.825808902011507,103.845220872878,15.3457040765431));
#60479=CARTESIAN_POINT('Ctrl Pts',(0.803092666440182,103.848326041871,15.3558352165152));
#60480=CARTESIAN_POINT('Ctrl Pts',(0.780190517107452,103.85143303692,15.3655865045497));
#60481=CARTESIAN_POINT('Ctrl Pts',(0.757113321523855,103.854541900927,15.3749495554873));
#60482=CARTESIAN_POINT('Ctrl Pts',(0.682328192372906,103.864616643131,15.4052919327091));
#60483=CARTESIAN_POINT('Ctrl Pts',(0.605703386872605,103.874711165779,15.4315568903168));
#60484=CARTESIAN_POINT('Ctrl Pts',(0.527732548759711,103.884823374306,15.4535997137354));
#60485=CARTESIAN_POINT('Ctrl Pts',(0.473764907657852,103.891822555714,15.4688566894447));
#60486=CARTESIAN_POINT('Ctrl Pts',(0.419152414187769,103.89883022874,15.4820914790451));
#60487=CARTESIAN_POINT('Ctrl Pts',(0.364045913284344,103.905847363209,15.4932599819668));
#60488=CARTESIAN_POINT('Ctrl Pts',(0.364027306121928,103.905849732602,15.4932637531035));
#60489=CARTESIAN_POINT('Ctrl Pts',(0.36400869890318,103.905852101996,15.4932675240046));
#60490=CARTESIAN_POINT('Ctrl Pts',(0.363990091628161,103.905854471391,15.49327129467));
#60491=CARTESIAN_POINT('Ctrl Pts',(0.246306748264742,103.920839919279,15.5171191993108));
#60492=CARTESIAN_POINT('Ctrl Pts',(0.126383243509028,103.935866907769,15.531541288314));
#60493=CARTESIAN_POINT('Ctrl Pts',(0.00574208375256261,103.951031871898,
15.5360830723919));
#60494=CARTESIAN_POINT('Ctrl Pts',(-0.0117271028536529,103.953227802281,
15.5367407357776));
#60495=CARTESIAN_POINT('Ctrl Pts',(-0.0292112542072715,103.955426615217,
15.5371911983692));
#60496=CARTESIAN_POINT('Ctrl Pts',(-0.0467056605022778,103.957628592728,
15.5374330531079));
#60497=CARTESIAN_POINT('Ctrl Pts',(-0.046708228653569,103.957628915975,
15.5374330886118));
#60498=CARTESIAN_POINT('Ctrl Pts',(-0.0467107968050665,103.957629239221,
15.5374331241112));
#60499=CARTESIAN_POINT('Ctrl Pts',(-0.0467133649567995,103.957629562468,
15.5374331596061));
#60500=CARTESIAN_POINT('Ctrl Pts',(-0.185025688623094,103.9750385958,15.5393448000133));
#60501=CARTESIAN_POINT('Ctrl Pts',(-0.324007003002818,103.992370846683,
15.5284412546859));
#60502=CARTESIAN_POINT('Ctrl Pts',(-0.46124508751448,104.00969676724,15.5048857075416));
#60503=CARTESIAN_POINT('Ctrl Pts',(-0.589157278613788,104.025845320094,
15.4829308569001));
#60504=CARTESIAN_POINT('Ctrl Pts',(-0.71555758177041,104.041990045687,15.4499886266189));
#60505=CARTESIAN_POINT('Ctrl Pts',(-0.838547870354058,104.058221754719,
15.4061513096145));
#60506=CARTESIAN_POINT('Ctrl Pts',(-0.847508384789385,104.059404323398,
15.4029575215817));
#60507=CARTESIAN_POINT('Ctrl Pts',(-0.856450830115381,104.060587360047,
15.3997058739288));
#60508=CARTESIAN_POINT('Ctrl Pts',(-0.865373302888538,104.06177483061,15.3963930849294));
#60509=CARTESIAN_POINT('Ctrl Pts',(-0.865379805326339,104.061775696004,
15.3963906706654));
#60510=CARTESIAN_POINT('Ctrl Pts',(-0.865386307753549,104.0617765614,15.396388256369));
#60511=CARTESIAN_POINT('Ctrl Pts',(-0.865392810170118,104.061777426799,
15.3963858420401));
#60512=CARTESIAN_POINT('Ctrl Pts',(-0.913587803696001,104.068191639078,
15.3784911771197));
#60513=CARTESIAN_POINT('Ctrl Pts',(-0.961214152223209,104.074614481611,
15.3589195478217));
#60514=CARTESIAN_POINT('Ctrl Pts',(-1.00817362924042,104.081044261839,15.3377268451394));
#60515=CARTESIAN_POINT('Ctrl Pts',(-1.10307424807729,104.094038233693,15.2948984167341));
#60516=CARTESIAN_POINT('Ctrl Pts',(-1.1952221055417,104.107191365773,15.2453345790668));
#60517=CARTESIAN_POINT('Ctrl Pts',(-1.28377358272751,104.120396167781,15.1895659707695));
#60518=CARTESIAN_POINT('Ctrl Pts',(-1.30872560007234,104.124117014222,15.1738515035946));
#60519=CARTESIAN_POINT('Ctrl Pts',(-1.33339232672395,104.12784200427,15.1576442027968));
#60520=CARTESIAN_POINT('Ctrl Pts',(-1.35775547083743,104.13156883061,15.1409554752094));
#60521=CARTESIAN_POINT('Ctrl Pts',(-1.43743384378368,104.143757218843,15.0863758751989));
#60522=CARTESIAN_POINT('Ctrl Pts',(-1.51385936633913,104.155955491083,15.0266568408663));
#60523=CARTESIAN_POINT('Ctrl Pts',(-1.58634113998981,104.168074490316,14.9622567875904));
#60524=CARTESIAN_POINT('Ctrl Pts',(-1.58635458946933,104.168076739078,14.9622448377283));
#60525=CARTESIAN_POINT('Ctrl Pts',(-1.58636803881416,104.168078987838,14.9622328877027));
#60526=CARTESIAN_POINT('Ctrl Pts',(-1.58638148802423,104.168081236597,14.9622209375136));
#60527=CARTESIAN_POINT('Ctrl Pts',(-1.65297955240087,104.179216686535,14.9030457548682));
#60528=CARTESIAN_POINT('Ctrl Pts',(-1.71627492265425,104.190321643138,14.8398596493715));
#60529=CARTESIAN_POINT('Ctrl Pts',(-1.77586158642476,104.201440127394,14.7731028926433));
#60530=CARTESIAN_POINT('Ctrl Pts',(-1.81119809134838,104.20803368959,14.7335143284656));
#60531=CARTESIAN_POINT('Ctrl Pts',(-1.84523090896447,104.21463233714,14.692669492739));
#60532=CARTESIAN_POINT('Ctrl Pts',(-1.87787879786267,104.221247238861,14.650653947854));
#60533=CARTESIAN_POINT('Ctrl Pts',(-1.87788445285372,104.221248384638,14.6506466702768));
#60534=CARTESIAN_POINT('Ctrl Pts',(-1.8778901078031,104.221249530416,14.6506393926647));
#60535=CARTESIAN_POINT('Ctrl Pts',(-1.87789576271087,104.221250676194,14.6506321150175));
#60536=CARTESIAN_POINT('Ctrl Pts',(-1.94309068071361,104.23446024942,14.5667287817711));
#60537=CARTESIAN_POINT('Ctrl Pts',(-2.00274975442905,104.247731816801,14.4781733383104));
#60538=CARTESIAN_POINT('Ctrl Pts',(-2.05600639711968,104.261043873617,14.3856565465746));
#60539=CARTESIAN_POINT('Ctrl Pts',(-2.07052185168252,104.264672163838,14.3604404755102));
#60540=CARTESIAN_POINT('Ctrl Pts',(-2.08456176106021,104.268303308782,14.3349302817011));
#60541=CARTESIAN_POINT('Ctrl Pts',(-2.09810878331213,104.271936536213,14.3091403214694));
#60542=CARTESIAN_POINT('Ctrl Pts',(-2.101723072737,104.272905866243,14.3022596669019));
#60543=CARTESIAN_POINT('Ctrl Pts',(-2.10530227924626,104.273875343736,14.2953590991255));
#60544=CARTESIAN_POINT('Ctrl Pts',(-2.10884618910972,104.274844823265,14.2884389695789));
#60545=CARTESIAN_POINT('Ctrl Pts',(-2.10884833437069,104.274845410127,14.2884347805661));
#60546=CARTESIAN_POINT('Ctrl Pts',(-2.10885047961875,104.27484599699,14.2884305915461));
#60547=CARTESIAN_POINT('Ctrl Pts',(-2.10885262485392,104.274846583852,14.2884264025188));
#60548=CARTESIAN_POINT('Ctrl Pts',(-2.16974195938393,104.291503801379,14.1695270438694));
#60549=CARTESIAN_POINT('Ctrl Pts',(-2.22023732229178,104.308178181703,14.0447781897744));
#60550=CARTESIAN_POINT('Ctrl Pts',(-2.25989936296388,104.324896771998,13.9161976968558));
#60551=CARTESIAN_POINT('Ctrl Pts',(-2.27625468960672,104.331790971102,13.8631753125824));
#60552=CARTESIAN_POINT('Ctrl Pts',(-2.29076816705059,104.338692649523,13.8095019061632));
#60553=CARTESIAN_POINT('Ctrl Pts',(-2.30341055969347,104.345603539293,13.7553209891809));
#60554=CARTESIAN_POINT('Ctrl Pts',(-2.34492074316024,104.368294837562,13.5774227172425));
#60555=CARTESIAN_POINT('Ctrl Pts',(-2.36619407616884,104.39114322775,13.3940410050713));
#60556=CARTESIAN_POINT('Ctrl Pts',(-2.36638569117636,104.414108494208,13.2101467996555));
#60557=CARTESIAN_POINT('Ctrl Pts',(-2.36653130410778,104.431560361956,13.0704010946139));
#60558=CARTESIAN_POINT('Ctrl Pts',(-2.35442107477345,104.449151659613,12.9303487498688));
#60559=CARTESIAN_POINT('Ctrl Pts',(-2.32963645208776,104.466892315332,12.7921344291781));
#60560=CARTESIAN_POINT('Ctrl Pts',(-2.31730459512665,104.475719370377,12.7233643996985));
#60561=CARTESIAN_POINT('Ctrl Pts',(-2.30183392522366,104.484582955546,12.6550465613128));
#60562=CARTESIAN_POINT('Ctrl Pts',(-2.28328232913452,104.493398049182,12.5874422945741));
#60563=CARTESIAN_POINT('Ctrl Pts',(-2.28327721304368,104.493400480176,12.5874236509184));
#60564=CARTESIAN_POINT('Ctrl Pts',(-2.28327209671646,104.493402911168,12.5874050073124));
#60565=CARTESIAN_POINT('Ctrl Pts',(-2.28326698015286,104.493405342157,12.5873863637562));
#60566=CARTESIAN_POINT('Ctrl Pts',(-2.2575264836489,104.505635204904,12.4935940388947));
#60567=CARTESIAN_POINT('Ctrl Pts',(-2.22579953848601,104.517804679907,12.4010580314143));
#60568=CARTESIAN_POINT('Ctrl Pts',(-2.18843650510388,104.529954291053,12.3105092748478));
#60569=CARTESIAN_POINT('Ctrl Pts',(-2.17837609430193,104.533225708498,12.2861280186648));
#60570=CARTESIAN_POINT('Ctrl Pts',(-2.16790732621083,104.536495663971,12.2618909596933));
#60571=CARTESIAN_POINT('Ctrl Pts',(-2.15703763802858,104.539764899956,12.2378125948701));
#60572=CARTESIAN_POINT('Ctrl Pts',(-2.11792783245846,104.551527811789,12.1511771596219));
#60573=CARTESIAN_POINT('Ctrl Pts',(-2.07362431716633,104.563282862789,12.0665933270532));
#60574=CARTESIAN_POINT('Ctrl Pts',(-2.02442105756846,104.575107823939,11.9847268004912));
#60575=CARTESIAN_POINT('Ctrl Pts',(-2.0082166354671,104.579002213526,11.9577651771511));
#60576=CARTESIAN_POINT('Ctrl Pts',(-1.99148103306734,104.582904132789,11.9310986069685));
#60577=CARTESIAN_POINT('Ctrl Pts',(-1.97422558590797,104.586816202795,11.9047517760302));
#60578=CARTESIAN_POINT('Ctrl Pts',(-1.90537055124895,104.602426677178,11.7996190639854));
#60579=CARTESIAN_POINT('Ctrl Pts',(-1.8283375168013,104.618118484337,11.6995233412364));
#60580=CARTESIAN_POINT('Ctrl Pts',(-1.74402731031377,104.633846836001,11.6057135876507));
#60581=CARTESIAN_POINT('Ctrl Pts',(-1.69274105295165,104.643414459245,11.5486487153664));
#60582=CARTESIAN_POINT('Ctrl Pts',(-1.63875720934119,104.652996539739,11.4939035602363));
#60583=CARTESIAN_POINT('Ctrl Pts',(-1.5821558071339,104.662685002477,11.4418579253114));
#60584=CARTESIAN_POINT('Ctrl Pts',(-1.5749876441991,104.663911977018,11.4352667177328));
#60585=CARTESIAN_POINT('Ctrl Pts',(-1.56777753282949,104.665140649707,11.4287188657917));
#60586=CARTESIAN_POINT('Ctrl Pts',(-1.560525666171,104.666371200229,11.4222151919796));
#60587=CARTESIAN_POINT('Ctrl Pts',(-1.5055804555543,104.675694711097,11.3729388133293));
#60588=CARTESIAN_POINT('Ctrl Pts',(-1.44825119977244,104.685105532953,11.3261676546078));
#60589=CARTESIAN_POINT('Ctrl Pts',(-1.38881768833724,104.694505635279,11.2820824080902));
#60590=CARTESIAN_POINT('Ctrl Pts',(-1.34605129191711,104.701269639168,11.2503601173602));
#60591=CARTESIAN_POINT('Ctrl Pts',(-1.30219489123442,104.708028222326,11.2200275463276));
#60592=CARTESIAN_POINT('Ctrl Pts',(-1.25734215753611,104.714746897393,11.1911392063596));
#60593=CARTESIAN_POINT('Ctrl Pts',(-1.25035757338188,104.715793146919,11.1866406390495));
#60594=CARTESIAN_POINT('Ctrl Pts',(-1.24334895990707,104.716838419881,11.1821771946694));
#60595=CARTESIAN_POINT('Ctrl Pts',(-1.23631670261522,104.717882600176,11.177749122534));
#60596=CARTESIAN_POINT('Ctrl Pts',(-1.23628269719713,104.71788764945,11.1777277100006));
#60597=CARTESIAN_POINT('Ctrl Pts',(-1.23624869119803,104.717892698706,11.1777062982871));
#60598=CARTESIAN_POINT('Ctrl Pts',(-1.23621468461808,104.717897747947,11.1776848873937));
#60599=CARTESIAN_POINT('Ctrl Pts',(-1.15935205338826,104.729310183284,11.1292913822398));
#60600=CARTESIAN_POINT('Ctrl Pts',(-1.07951740542718,104.740639255472,11.0850877874245));
#60601=CARTESIAN_POINT('Ctrl Pts',(-0.997264676478942,104.751932187046,
11.045326783786));
#60602=CARTESIAN_POINT('Ctrl Pts',(-0.969483553245763,104.755746410935,
11.0318973771745));
#60603=CARTESIAN_POINT('Ctrl Pts',(-0.941427015877044,104.75955647207,11.0189746984554));
#60604=CARTESIAN_POINT('Ctrl Pts',(-0.913117709667293,104.763364066709,
11.0065681929864));
#60605=CARTESIAN_POINT('Ctrl Pts',(-0.842634762476249,104.772844005563,
10.9756791608313));
#60606=CARTESIAN_POINT('Ctrl Pts',(-0.770581015164748,104.782310004766,
10.9479894287309));
#60607=CARTESIAN_POINT('Ctrl Pts',(-0.69725070595239,104.791845872049,10.9237153410963));
#60608=CARTESIAN_POINT('Ctrl Pts',(-0.652537084713335,104.79766042762,10.9089140621699));
#60609=CARTESIAN_POINT('Ctrl Pts',(-0.607349743046027,104.803500833865,
10.8953831642764));
#60610=CARTESIAN_POINT('Ctrl Pts',(-0.561764445978303,104.809384893613,
10.8831744227458));
#60611=CARTESIAN_POINT('Ctrl Pts',(-0.454886573630109,104.823180477433,
10.854550186363));
#60612=CARTESIAN_POINT('Ctrl Pts',(-0.34593646565383,104.837005124755,10.83285266738));
#60613=CARTESIAN_POINT('Ctrl Pts',(-0.235792247083463,104.850865137857,
10.8182859260231));
#60614=CARTESIAN_POINT('Ctrl Pts',(-0.220693775708796,104.852765056108,
10.8162891300927));
#60615=CARTESIAN_POINT('Ctrl Pts',(-0.20557283729048,104.854665640299,10.8144264009999));
#60616=CARTESIAN_POINT('Ctrl Pts',(-0.190431669900425,104.856566907995,
10.812698336862));
#60617=CARTESIAN_POINT('Ctrl Pts',(-0.152853269521076,104.861285606155,
10.8084095073165));
#60618=CARTESIAN_POINT('Ctrl Pts',(-0.115148932112492,104.866008682015,
10.8049499169657));
#60619=CARTESIAN_POINT('Ctrl Pts',(-0.0773493836361189,104.870737059702,
10.8023297075166));
#60620=CARTESIAN_POINT('Ctrl Pts',(-1.07958803427197,23.125761603439,10.3785207772594));
#60621=CARTESIAN_POINT('Ctrl Pts',(-0.34554065930921,23.2239632414138,10.0948431126673));
#60622=CARTESIAN_POINT('Ctrl Pts',(1.34243986332755,23.420102020386,10.1127125594068));
#60623=CARTESIAN_POINT('Ctrl Pts',(3.18017348682762,23.7162461148519,11.8764837958139));
#60624=CARTESIAN_POINT('Ctrl Pts',(3.32060625935821,24.0131814407576,14.4260813171523));
#60625=CARTESIAN_POINT('Ctrl Pts',(1.67691747945551,24.3117154001464,16.3981628554893));
#60626=CARTESIAN_POINT('Ctrl Pts',(-0.880376510953372,24.6113532051016,
16.7210498975078));
#60627=CARTESIAN_POINT('Ctrl Pts',(-2.97471211665326,24.9115581886552,15.2128811643004));
#60628=CARTESIAN_POINT('Ctrl Pts',(-3.48144100827184,25.211804507667,12.6778104888403));
#60629=CARTESIAN_POINT('Ctrl Pts',(-2.17274142682733,25.5004550944448,10.5709222508267));
#60630=CARTESIAN_POINT('Ctrl Pts',(0.0600344106941335,25.7771166135459,
9.85725397170378));
#60631=CARTESIAN_POINT('Ctrl Pts',(2.15934368744129,26.0415422132396,10.6413269741514));
#60632=CARTESIAN_POINT('Ctrl Pts',(3.22061067469158,26.2825345572412,12.3845222667272));
#60633=CARTESIAN_POINT('Ctrl Pts',(3.15347935583999,26.5002557872507,14.1840957311028));
#60634=CARTESIAN_POINT('Ctrl Pts',(2.33420364046461,26.6950126881386,15.5694145660939));
#60635=CARTESIAN_POINT('Ctrl Pts',(0.958566958400896,26.8884387445348,16.3854549505474));
#60636=CARTESIAN_POINT('Ctrl Pts',(-0.627537293809016,27.0804033115453,
16.4434136719425));
#60637=CARTESIAN_POINT('Ctrl Pts',(-2.03552350511545,27.2707817161207,15.7397540217649));
#60638=CARTESIAN_POINT('Ctrl Pts',(-2.92642873709077,27.4594521092887,14.4589186698802));
#60639=CARTESIAN_POINT('Ctrl Pts',(-3.06476918820841,27.6151620870074,13.1791852448839));
#60640=CARTESIAN_POINT('Ctrl Pts',(-2.80163706893976,27.7387642717718,12.2162436591921));
#60641=CARTESIAN_POINT('Ctrl Pts',(-2.31305221628185,27.8617107211686,11.3516558461287));
#60642=CARTESIAN_POINT('Ctrl Pts',(-1.33339394747703,28.0141249041079,10.5593435278253));
#60643=CARTESIAN_POINT('Ctrl Pts',(0.137466061428836,28.1949063678745,10.2916382306392));
#60644=CARTESIAN_POINT('Ctrl Pts',(1.42221496642251,28.3586060455309,10.7168492274562));
#60645=CARTESIAN_POINT('Ctrl Pts',(2.12004744313203,28.4763323007467,11.3762841986774));
#60646=CARTESIAN_POINT('Ctrl Pts',(2.62396197101089,28.5932856628549,12.168670878928));
#60647=CARTESIAN_POINT('Ctrl Pts',(2.89307483334103,28.7237599241023,13.2130931079621));
#60648=CARTESIAN_POINT('Ctrl Pts',(2.54652333624131,28.8953280039873,14.5887900128546));
#60649=CARTESIAN_POINT('Ctrl Pts',(1.59579795643967,29.0644499469633,15.6142705384307));
#60650=CARTESIAN_POINT('Ctrl Pts',(0.617102208219719,29.1894288450293,15.9444046726897));
#60651=CARTESIAN_POINT('Ctrl Pts',(-0.0456556529442235,29.2719631152849,
15.9535087705334));
#60652=CARTESIAN_POINT('Ctrl Pts',(-0.483011850539022,29.3267759193272,
15.9050013907027));
#60653=CARTESIAN_POINT('Ctrl Pts',(-1.2198054873934,29.4221461631643,15.6794201744828));
#60654=CARTESIAN_POINT('Ctrl Pts',(-2.09014382104258,29.5568075472996,14.9852905198769));
#60655=CARTESIAN_POINT('Ctrl Pts',(-2.59788149289038,29.7158584966411,13.7719095212622));
#60656=CARTESIAN_POINT('Ctrl Pts',(-2.46711739291308,29.8723680883128,12.4845544452712));
#60657=CARTESIAN_POINT('Ctrl Pts',(-1.74601398001167,30.0263461962339,11.4352049138197));
#60658=CARTESIAN_POINT('Ctrl Pts',(-0.629844515312964,30.1778111542655,
10.8670301468742));
#60659=CARTESIAN_POINT('Ctrl Pts',(0.601496364936027,30.3267943685925,10.9037055374241));
#60660=CARTESIAN_POINT('Ctrl Pts',(1.64825284718227,30.4733320948358,11.5144435828851));
#60661=CARTESIAN_POINT('Ctrl Pts',(2.2635440376844,30.6174743670642,12.5350177559086));
#60662=CARTESIAN_POINT('Ctrl Pts',(2.31580800504618,30.7592767886105,13.7065846562522));
#60663=CARTESIAN_POINT('Ctrl Pts',(1.807753632511,30.8988065252971,14.7424093963853));
#60664=CARTESIAN_POINT('Ctrl Pts',(0.881013187737084,31.0361391305485,15.3991007570354));
#60665=CARTESIAN_POINT('Ctrl Pts',(-0.229384030457491,31.1713551305116,
15.5289368437615));
#60666=CARTESIAN_POINT('Ctrl Pts',(-1.25180204175459,31.3045516305373,15.1187939179942));
#60667=CARTESIAN_POINT('Ctrl Pts',(-1.9415893920128,31.4358200365546,14.2806703731829));
#60668=CARTESIAN_POINT('Ctrl Pts',(-2.14468763692602,31.5652759046523,13.2295435090225));
#60669=CARTESIAN_POINT('Ctrl Pts',(-1.82320966062737,31.6930248645021,12.2230522342915));
#60670=CARTESIAN_POINT('Ctrl Pts',(-1.06864419389326,31.8191908990757,11.5022587818521));
#60671=CARTESIAN_POINT('Ctrl Pts',(-0.0727669233574973,31.9438975626322,
11.2346252743258));
#60672=CARTESIAN_POINT('Ctrl Pts',(0.919693554917522,32.0672810695473,11.4726566241412));
#60673=CARTESIAN_POINT('Ctrl Pts',(1.66887056249793,32.1894739538329,12.1506666424005));
#60674=CARTESIAN_POINT('Ctrl Pts',(2.00013058191407,32.3106196673884,13.0969596993241));
#60675=CARTESIAN_POINT('Ctrl Pts',(1.83781539368687,32.4308629546113,14.0774584579158));
#60676=CARTESIAN_POINT('Ctrl Pts',(1.1632926479292,32.5636275136061,14.9453606036313));
#60677=CARTESIAN_POINT('Ctrl Pts',(-0.00197077022069799,32.708812342,15.3383648007732));
#60678=CARTESIAN_POINT('Ctrl Pts',(-1.26239853292309,32.8664892999126,14.8907072077442));
#60679=CARTESIAN_POINT('Ctrl Pts',(-1.8258439893124,32.9910569449221,13.9989784067232));
#60680=CARTESIAN_POINT('Ctrl Pts',(-1.90256425845217,33.0828535369837,13.260933206721));
#60681=CARTESIAN_POINT('Ctrl Pts',(-1.81251203490417,33.1615760274655,12.63147976504));
#60682=CARTESIAN_POINT('Ctrl Pts',(-1.40892388448975,33.2600857890204,11.9236479231083));
#60683=CARTESIAN_POINT('Ctrl Pts',(-0.57432734621905,33.3786362635983,11.4089625889543));
#60684=CARTESIAN_POINT('Ctrl Pts',(0.408902180381898,33.4976766157179,11.3569408514114));
#60685=CARTESIAN_POINT('Ctrl Pts',(1.3016420224292,33.6173620208606,11.7849288978517));
#60686=CARTESIAN_POINT('Ctrl Pts',(1.88421901808678,33.7378433732163,12.5934241275751));
#60687=CARTESIAN_POINT('Ctrl Pts',(2.00841783454731,33.859267715344,13.590321732198));
#60688=CARTESIAN_POINT('Ctrl Pts',(1.67741798856941,33.9681678843717,14.4284141902102));
#60689=CARTESIAN_POINT('Ctrl Pts',(1.12015075491802,34.0642516399516,14.9752972742767));
#60690=CARTESIAN_POINT('Ctrl Pts',(0.30883305425423,34.1748415606842,15.3636707172977));
#60691=CARTESIAN_POINT('Ctrl Pts',(-0.63683898934766,34.2866861183453,15.3112234175934));
#60692=CARTESIAN_POINT('Ctrl Pts',(-1.41733709088844,34.3999293831788,14.8225486779453));
#60693=CARTESIAN_POINT('Ctrl Pts',(-2.04209650955594,34.5212951308744,14.0586970846731));
#60694=CARTESIAN_POINT('Ctrl Pts',(-2.23763665747699,34.6806558523311,12.7030451058781));
#60695=CARTESIAN_POINT('Ctrl Pts',(-1.2527133198986,34.8805161631469,11.2917435621959));
#60696=CARTESIAN_POINT('Ctrl Pts',(0.464977883462776,35.0849872890747,10.9202321885198));
#60697=CARTESIAN_POINT('Ctrl Pts',(2.0130473474812,35.2943670661089,11.8427459642946));
#60698=CARTESIAN_POINT('Ctrl Pts',(2.52660114584721,35.50890654089,13.6144619963185));
#60699=CARTESIAN_POINT('Ctrl Pts',(1.67665102832899,35.7288118669548,15.3040875688965));
#60700=CARTESIAN_POINT('Ctrl Pts',(-0.192116355100357,35.9600384371841,
15.9901518801674));
#60701=CARTESIAN_POINT('Ctrl Pts',(-1.45964153582199,36.120174190932,15.41955795021));
#60702=CARTESIAN_POINT('Ctrl Pts',(-1.91091130723325,36.2043175118729,14.9174925473367));
#60703=CARTESIAN_POINT('Ctrl Pts',(-1.00595942234827,23.4703156359905,10.5694791067139));
#60704=CARTESIAN_POINT('Ctrl Pts',(-0.315877847047438,23.5621480601222,
10.3142801806992));
#60705=CARTESIAN_POINT('Ctrl Pts',(1.25363167841598,23.7446337943067,10.3564313620877));
#60706=CARTESIAN_POINT('Ctrl Pts',(2.92084555199283,24.0175788900516,12.0084073813003));
#60707=CARTESIAN_POINT('Ctrl Pts',(3.01267803575596,24.2888665683142,14.3388519167426));
#60708=CARTESIAN_POINT('Ctrl Pts',(1.49612998604492,24.5594335621326,16.1026512075001));
#60709=CARTESIAN_POINT('Ctrl Pts',(-0.808179728832318,24.8290174145929,
16.3582951621009));
#60710=CARTESIAN_POINT('Ctrl Pts',(-2.65944370200479,25.0973445240907,14.9829489444263));
#60711=CARTESIAN_POINT('Ctrl Pts',(-3.07651190721737,25.3641623643543,12.724296780867));
#60712=CARTESIAN_POINT('Ctrl Pts',(-1.8928067719465,25.6194082319424,10.8786418964801));
#60713=CARTESIAN_POINT('Ctrl Pts',(0.0822095539269653,25.8631059996756,
10.2780969229765));
#60714=CARTESIAN_POINT('Ctrl Pts',(1.91564198504364,26.0953415910853,10.992459371924));
#60715=CARTESIAN_POINT('Ctrl Pts',(2.8239435354046,26.3065275168311,12.5326018159647));
#60716=CARTESIAN_POINT('Ctrl Pts',(2.7433255831973,26.4970749742018,14.1062282815387));
#60717=CARTESIAN_POINT('Ctrl Pts',(2.01014712384195,26.6674096336721,15.3074755501791));
#60718=CARTESIAN_POINT('Ctrl Pts',(0.797707037023478,26.8365425712707,16.0040071039835));
#60719=CARTESIAN_POINT('Ctrl Pts',(-0.589761995396185,27.004435551555,16.0352476373376));
#60720=CARTESIAN_POINT('Ctrl Pts',(-1.81296648289921,27.1710551901992,15.4022578695728));
#60721=CARTESIAN_POINT('Ctrl Pts',(-2.57745246520028,27.336372182225,14.2692880697337));
#60722=CARTESIAN_POINT('Ctrl Pts',(-2.68282409359319,27.473031356267,13.1447629858075));
#60723=CARTESIAN_POINT('Ctrl Pts',(-2.43928761960126,27.5816857231595,12.3019245827255));
#60724=CARTESIAN_POINT('Ctrl Pts',(-1.9983164528988,27.6898899233007,11.5475832051832));
#60725=CARTESIAN_POINT('Ctrl Pts',(-1.12459065098004,27.8242955054052,10.8616462820568));
#60726=CARTESIAN_POINT('Ctrl Pts',(0.17954106387617,27.9842153349351,10.6439457189669));
#60727=CARTESIAN_POINT('Ctrl Pts',(1.31419007004281,28.129552146691,11.0381880889183));
#60728=CARTESIAN_POINT('Ctrl Pts',(1.92687082167423,28.2344536276736,11.6350157508958));
#60729=CARTESIAN_POINT('Ctrl Pts',(2.3656901722259,28.3389005281905,12.3493840235856));
#60730=CARTESIAN_POINT('Ctrl Pts',(2.59246433293698,28.455765405854,13.2881757380847));
#60731=CARTESIAN_POINT('Ctrl Pts',(2.26154052562728,28.6102370497776,14.5214959902665));
#60732=CARTESIAN_POINT('Ctrl Pts',(1.38650323158265,28.7633774443539,15.436319994476));
#60733=CARTESIAN_POINT('Ctrl Pts',(0.490367493818371,28.8772522456174,15.7228478889474));
#60734=CARTESIAN_POINT('Ctrl Pts',(-0.115902755902976,28.9527679590394,
15.720994514257));
#60735=CARTESIAN_POINT('Ctrl Pts',(-0.515823678956967,29.0030064433406,
15.6697851525537));
#60736=CARTESIAN_POINT('Ctrl Pts',(-1.18906392073067,29.0906466047621,15.4512023590902));
#60737=CARTESIAN_POINT('Ctrl Pts',(-1.98232267801215,29.2150670210491,14.7969700130926));
#60738=CARTESIAN_POINT('Ctrl Pts',(-2.43605903789984,29.3631627820738,13.6597517681805));
#60739=CARTESIAN_POINT('Ctrl Pts',(-2.29279814786244,29.5100883241477,12.4539148456178));
#60740=CARTESIAN_POINT('Ctrl Pts',(-1.5930426178182,29.6558949765442,11.4725425950399));
#60741=CARTESIAN_POINT('Ctrl Pts',(-0.517432252664176,29.8006287421963,
10.94878973249));
#60742=CARTESIAN_POINT('Ctrl Pts',(0.669193813981328,29.9443493199384,11.0056188986052));
#60743=CARTESIAN_POINT('Ctrl Pts',(1.67744591647376,30.0871116323955,11.6191187333393));
#60744=CARTESIAN_POINT('Ctrl Pts',(2.26375300252859,30.2289807478686,12.6345032307524));
#60745=CARTESIAN_POINT('Ctrl Pts',(2.293238531032,30.370021008209,13.8000545156108));
#60746=CARTESIAN_POINT('Ctrl Pts',(1.76220071904141,30.510302264146,14.8307970020976));
#60747=CARTESIAN_POINT('Ctrl Pts',(0.80734479632738,30.6498973070903,15.4789104494946));
#60748=CARTESIAN_POINT('Ctrl Pts',(-0.336016774735876,30.7888783301199,
15.5887400642292));
#60749=CARTESIAN_POINT('Ctrl Pts',(-1.3890059475663,30.9273270494787,15.1403607710382));
#60750=CARTESIAN_POINT('Ctrl Pts',(-2.09465588475557,31.065316325783,14.2442944012222));
#60751=CARTESIAN_POINT('Ctrl Pts',(-2.28581823124681,31.202933769985,13.1230263682163));
#60752=CARTESIAN_POINT('Ctrl Pts',(-1.91623167317492,31.3402558750362,12.0496946881804));
#60753=CARTESIAN_POINT('Ctrl Pts',(-1.07890358209417,31.4773688229052,11.2857618737474));
#60754=CARTESIAN_POINT('Ctrl Pts',(0.0210509156088651,31.6143552012013,
11.0175686839098));
#60755=CARTESIAN_POINT('Ctrl Pts',(1.11536038725298,31.7513022871471,11.3077307424644));
#60756=CARTESIAN_POINT('Ctrl Pts',(1.93612871033968,31.8882925319881,12.0875194085925));
#60757=CARTESIAN_POINT('Ctrl Pts',(2.28442129393533,32.0254116397918,13.1668223690244));
#60758=CARTESIAN_POINT('Ctrl Pts',(2.07119455170064,32.1627436409057,14.2810268476482));
#60759=CARTESIAN_POINT('Ctrl Pts',(1.26984743031617,32.3156626735956,15.2600648520212));
#60760=CARTESIAN_POINT('Ctrl Pts',(-0.0947238237671589,32.4844144762023,
15.6826089699051));
#60761=CARTESIAN_POINT('Ctrl Pts',(-1.55853578518989,32.6693698596506,15.1204857695937));
#60762=CARTESIAN_POINT('Ctrl Pts',(-2.19675809292368,32.816625001231,14.0501554524693));
#60763=CARTESIAN_POINT('Ctrl Pts',(-2.26420720501918,32.9256178774175,13.1722540887062));
#60764=CARTESIAN_POINT('Ctrl Pts',(-2.13704607973914,33.0192849787917,12.4269900391733));
#60765=CARTESIAN_POINT('Ctrl Pts',(-1.63346515637257,33.1368424073631,11.5959647067977));
#60766=CARTESIAN_POINT('Ctrl Pts',(-0.619082947445776,33.2787432000681,
11.0071612785401));
#60767=CARTESIAN_POINT('Ctrl Pts',(0.560814397369453,33.4215398351124,10.9762790753619));
#60768=CARTESIAN_POINT('Ctrl Pts',(1.61829684472986,33.5652955286783,11.5183922685832));
#60769=CARTESIAN_POINT('Ctrl Pts',(2.29179274561511,33.7100689358281,12.5075111711697));
#60770=CARTESIAN_POINT('Ctrl Pts',(2.40911494050403,33.8559145947988,13.7076478489104));
#60771=CARTESIAN_POINT('Ctrl Pts',(1.98595485145375,33.9865536897804,14.7015680988501));
#60772=CARTESIAN_POINT('Ctrl Pts',(1.30221394563286,34.1016210722776,15.3384786563256));
#60773=CARTESIAN_POINT('Ctrl Pts',(0.321129855928317,34.2338358770118,15.7772973775983));
#60774=CARTESIAN_POINT('Ctrl Pts',(-0.803167037301693,34.3671404111073,
15.6853838858228));
#60775=CARTESIAN_POINT('Ctrl Pts',(-1.71413544543102,34.5015739164706,15.0824384631522));
#60776=CARTESIAN_POINT('Ctrl Pts',(-2.43039140986002,34.6452224333733,14.1605266697859));
#60777=CARTESIAN_POINT('Ctrl Pts',(-2.61917840501806,34.8328540037758,12.5599786999848));
#60778=CARTESIAN_POINT('Ctrl Pts',(-1.42858408684654,35.0661480293711,10.9435773618336));
#60779=CARTESIAN_POINT('Ctrl Pts',(0.565898564707986,35.3025057604142,10.5642067088703));
#60780=CARTESIAN_POINT('Ctrl Pts',(2.30872173182878,35.5419477791935,11.6617907113252));
#60781=CARTESIAN_POINT('Ctrl Pts',(2.840613788849,35.784466262583,13.6767542672384));
#60782=CARTESIAN_POINT('Ctrl Pts',(1.8478141234025,36.0300290070386,15.5397950856984));
#60783=CARTESIAN_POINT('Ctrl Pts',(-0.228189814937037,36.2849569348317,
16.2481689080808));
#60784=CARTESIAN_POINT('Ctrl Pts',(-1.5918854708806,36.4591229948481,15.5967610939565));
#60785=CARTESIAN_POINT('Ctrl Pts',(-2.0681370687829,36.5499727686619,15.0455429908956));
#60786=CARTESIAN_POINT('Ctrl Pts',(-0.932330810424575,23.8148696685421,
10.7604374361683));
#60787=CARTESIAN_POINT('Ctrl Pts',(-0.286215034785667,23.9003328788305,
10.5337172487311));
#60788=CARTESIAN_POINT('Ctrl Pts',(1.16482349350439,24.0691655682275,10.6001501647687));
#60789=CARTESIAN_POINT('Ctrl Pts',(2.66151761715804,24.3189116652514,12.1403309667867));
#60790=CARTESIAN_POINT('Ctrl Pts',(2.70474981215371,24.5645516958709,14.2516225163327));
#60791=CARTESIAN_POINT('Ctrl Pts',(1.31534249263431,24.8071517241187,15.8071395595109));
#60792=CARTESIAN_POINT('Ctrl Pts',(-0.735982946711268,25.0466816240843,
15.9955404266939));
#60793=CARTESIAN_POINT('Ctrl Pts',(-2.3441752873563,25.2831308595262,14.7530167245522));
#60794=CARTESIAN_POINT('Ctrl Pts',(-2.67158280616291,25.5165202210414,12.7707830728936));
#60795=CARTESIAN_POINT('Ctrl Pts',(-1.61287211706566,25.7383613694401,11.1863615421335));
#60796=CARTESIAN_POINT('Ctrl Pts',(0.1043846971598,25.9490953858052,10.6989398742492));
#60797=CARTESIAN_POINT('Ctrl Pts',(1.67194028264597,26.1491409689308,11.3435917696966));
#60798=CARTESIAN_POINT('Ctrl Pts',(2.42727639611763,26.3305204764211,12.6806813652021));
#60799=CARTESIAN_POINT('Ctrl Pts',(2.33317181055461,26.493894161153,14.0283608319746));
#60800=CARTESIAN_POINT('Ctrl Pts',(1.6860906072193,26.6398065792055,15.0455365342643));
#60801=CARTESIAN_POINT('Ctrl Pts',(0.636847115646059,26.7846463980065,15.6225592574197));
#60802=CARTESIAN_POINT('Ctrl Pts',(-0.551986696983355,26.9284677915647,
15.6270816027327));
#60803=CARTESIAN_POINT('Ctrl Pts',(-1.59040946068298,27.0713286642777,15.0647617173808));
#60804=CARTESIAN_POINT('Ctrl Pts',(-2.22847619330979,27.2132922551612,14.0796574695873));
#60805=CARTESIAN_POINT('Ctrl Pts',(-2.30087899897796,27.3309006255265,13.1103407267311));
#60806=CARTESIAN_POINT('Ctrl Pts',(-2.07693817026276,27.4246071745472,12.3876055062589));
#60807=CARTESIAN_POINT('Ctrl Pts',(-1.68358068951573,27.5180691254328,11.7435105642378));
#60808=CARTESIAN_POINT('Ctrl Pts',(-0.915787354483041,27.6344661067026,
11.1639490362885));
#60809=CARTESIAN_POINT('Ctrl Pts',(0.221616066323505,27.7735243019958,10.9962532072946));
#60810=CARTESIAN_POINT('Ctrl Pts',(1.2061651736631,27.9004982478512,11.3595269503803));
#60811=CARTESIAN_POINT('Ctrl Pts',(1.73369420021643,27.9925749546004,11.8937473031143));
#60812=CARTESIAN_POINT('Ctrl Pts',(2.10741837344092,28.0845153935261,12.5300971682432));
#60813=CARTESIAN_POINT('Ctrl Pts',(2.29185383253292,28.1877708876058,13.3632583682073));
#60814=CARTESIAN_POINT('Ctrl Pts',(1.97655771501325,28.3251460955679,14.4542019676785));
#60815=CARTESIAN_POINT('Ctrl Pts',(1.17720850672562,28.4623049417444,15.2583694505214));
#60816=CARTESIAN_POINT('Ctrl Pts',(0.363632779417019,28.5650756462056,15.501291105205));
#60817=CARTESIAN_POINT('Ctrl Pts',(-0.186149858861731,28.633572802794,15.4884802579808));
#60818=CARTESIAN_POINT('Ctrl Pts',(-0.548635507374914,28.679236967354,15.4345689144049));
#60819=CARTESIAN_POINT('Ctrl Pts',(-1.15832235406793,28.7591470463601,15.2229845436976));
#60820=CARTESIAN_POINT('Ctrl Pts',(-1.8745015349817,28.8733264947987,14.6086495063083));
#60821=CARTESIAN_POINT('Ctrl Pts',(-2.27423658290929,29.0104670675064,13.547594015099));
#60822=CARTESIAN_POINT('Ctrl Pts',(-2.11847890281181,29.1478085599825,12.4232752459646));
#60823=CARTESIAN_POINT('Ctrl Pts',(-1.44007125562472,29.2854437568545,11.50988027626));
#60824=CARTESIAN_POINT('Ctrl Pts',(-0.405019990015385,29.4234463301271,
11.0305493181059));
#60825=CARTESIAN_POINT('Ctrl Pts',(0.736891263026629,29.5619042712843,11.1075322597862));
#60826=CARTESIAN_POINT('Ctrl Pts',(1.70663898576526,29.7008911699554,11.7237938837935));
#60827=CARTESIAN_POINT('Ctrl Pts',(2.26396196737277,29.8404871286729,12.7339887055961));
#60828=CARTESIAN_POINT('Ctrl Pts',(2.27066905701781,29.9807652278076,13.8935243749694));
#60829=CARTESIAN_POINT('Ctrl Pts',(1.71664780557182,30.1217980029948,14.9191846078098));
#60830=CARTESIAN_POINT('Ctrl Pts',(0.733676404917682,30.2636554836321,15.5587201419538));
#60831=CARTESIAN_POINT('Ctrl Pts',(-0.442649519014257,30.4064015297281,
15.6485432846969));
#60832=CARTESIAN_POINT('Ctrl Pts',(-1.52620985337802,30.5501024684201,15.161927624082));
#60833=CARTESIAN_POINT('Ctrl Pts',(-2.24772237749834,30.6948126150113,14.2079184292616));
#60834=CARTESIAN_POINT('Ctrl Pts',(-2.42694882556761,30.8405916353176,13.0165092274103));
#60835=CARTESIAN_POINT('Ctrl Pts',(-2.00925368572246,30.9874868855705,11.8763371420694));
#60836=CARTESIAN_POINT('Ctrl Pts',(-1.08916297029509,31.1355467467346,11.0692649656428));
#60837=CARTESIAN_POINT('Ctrl Pts',(0.114868754575229,31.2848128397704,10.800512093494));
#60838=CARTESIAN_POINT('Ctrl Pts',(1.31102721958845,31.435323504747,11.1428048607877));
#60839=CARTESIAN_POINT('Ctrl Pts',(2.20338685818143,31.5871111101434,12.0243721747846));
#60840=CARTESIAN_POINT('Ctrl Pts',(2.56871200595661,31.7402036121951,13.2366850387248));
#60841=CARTESIAN_POINT('Ctrl Pts',(2.30457370971442,31.8946243272,14.4845952373805));
#60842=CARTESIAN_POINT('Ctrl Pts',(1.37640221270315,32.0676978335851,15.5747691004112));
#60843=CARTESIAN_POINT('Ctrl Pts',(-0.187476877313618,32.2600166104046,
16.0268531390372));
#60844=CARTESIAN_POINT('Ctrl Pts',(-1.85467303745672,32.4722504193886,15.3502643314434));
#60845=CARTESIAN_POINT('Ctrl Pts',(-2.56767219653497,32.6421930575399,14.1013324982155));
#60846=CARTESIAN_POINT('Ctrl Pts',(-2.6258501515862,32.7683822178512,13.0835749706912));
#60847=CARTESIAN_POINT('Ctrl Pts',(-2.46158012457412,32.8769939301179,12.2225003133065));
#60848=CARTESIAN_POINT('Ctrl Pts',(-1.85800642825539,33.0135990257057,11.2682814904871));
#60849=CARTESIAN_POINT('Ctrl Pts',(-0.663838548672504,33.178850136538,10.6053599681259));
#60850=CARTESIAN_POINT('Ctrl Pts',(0.712726614357012,33.3454030545069,10.5956172993124));
#60851=CARTESIAN_POINT('Ctrl Pts',(1.93495166703052,33.5132290364961,11.2518556393147));
#60852=CARTESIAN_POINT('Ctrl Pts',(2.69936647314346,33.6822944984401,12.4215982147645));
#60853=CARTESIAN_POINT('Ctrl Pts',(2.80981204646077,33.8525614742537,13.8249739656226));
#60854=CARTESIAN_POINT('Ctrl Pts',(2.2944917143381,34.004939495189,14.97472200749));
#60855=CARTESIAN_POINT('Ctrl Pts',(1.48427713634769,34.1389905046036,15.7016600383746));
#60856=CARTESIAN_POINT('Ctrl Pts',(0.333426657602405,34.2928301933393,16.1909240378989));
#60857=CARTESIAN_POINT('Ctrl Pts',(-0.969495085255728,34.4475947038694,
16.0595443540521));
#60858=CARTESIAN_POINT('Ctrl Pts',(-2.0109337999736,34.6032184497623,15.3423282483589));
#60859=CARTESIAN_POINT('Ctrl Pts',(-2.81868631016408,34.7691497358721,14.2623562548988));
#60860=CARTESIAN_POINT('Ctrl Pts',(-3.00072015255915,34.9850521552204,12.4169122940916));
#60861=CARTESIAN_POINT('Ctrl Pts',(-1.60445485379447,35.2517798955955,10.5954111614711));
#60862=CARTESIAN_POINT('Ctrl Pts',(0.666819245953194,35.5200242317538,10.2081812292208));
#60863=CARTESIAN_POINT('Ctrl Pts',(2.60439611617634,35.7895284922781,11.4808354583559));
#60864=CARTESIAN_POINT('Ctrl Pts',(3.1546264318508,36.0600259842761,13.7390465381583));
#60865=CARTESIAN_POINT('Ctrl Pts',(2.01897721847602,36.3312461471225,15.7755026025001));
#60866=CARTESIAN_POINT('Ctrl Pts',(-0.264263274773716,36.6098754324793,
16.5061859359941));
#60867=CARTESIAN_POINT('Ctrl Pts',(-1.7241294059392,36.7980717987643,15.7739642377031));
#60868=CARTESIAN_POINT('Ctrl Pts',(-2.22536283033256,36.895628025451,15.1735934344545));
#60869=CARTESIAN_POINT('Ctrl Pts',(-0.858702198500876,24.1594237010936,
10.9513957656227));
#60870=CARTESIAN_POINT('Ctrl Pts',(-0.256552222523894,24.2385176975388,
10.7531543167631));
#60871=CARTESIAN_POINT('Ctrl Pts',(1.07601530859282,24.3936973421483,10.8438689674496));
#60872=CARTESIAN_POINT('Ctrl Pts',(2.40218968232325,24.620244440451,12.2722545522732));
#60873=CARTESIAN_POINT('Ctrl Pts',(2.39682158855147,24.8402368234276,14.1643931159229));
#60874=CARTESIAN_POINT('Ctrl Pts',(1.13455499922372,25.0548698861049,15.5116279115216));
#60875=CARTESIAN_POINT('Ctrl Pts',(-0.66378616459021,25.2643458335756,15.632785691287));
#60876=CARTESIAN_POINT('Ctrl Pts',(-2.02890687270782,25.4689171949617,14.5230845046781));
#60877=CARTESIAN_POINT('Ctrl Pts',(-2.26665370510843,25.6688780777285,12.8172693649202));
#60878=CARTESIAN_POINT('Ctrl Pts',(-1.33293746218483,25.8573145069377,11.4940811877868));
#60879=CARTESIAN_POINT('Ctrl Pts',(0.126559840392635,26.0350847719349,11.1197828255219));
#60880=CARTESIAN_POINT('Ctrl Pts',(1.42823858024832,26.2029403467764,11.6947241674692));
#60881=CARTESIAN_POINT('Ctrl Pts',(2.03060925683066,26.3545134360111,12.8287609144396));
#60882=CARTESIAN_POINT('Ctrl Pts',(1.92301803791192,26.490713348104,13.9504933824104));
#60883=CARTESIAN_POINT('Ctrl Pts',(1.36203409059664,26.612203524739,14.7835975183494));
#60884=CARTESIAN_POINT('Ctrl Pts',(0.475987194268644,26.7327502247424,15.2411114108558));
#60885=CARTESIAN_POINT('Ctrl Pts',(-0.514211398570525,26.8525000315743,
15.2189155681279));
#60886=CARTESIAN_POINT('Ctrl Pts',(-1.36785243846674,26.9716021383562,14.7272655651888));
#60887=CARTESIAN_POINT('Ctrl Pts',(-1.87949992141931,27.0902123280975,13.8900268694409));
#60888=CARTESIAN_POINT('Ctrl Pts',(-1.91893390436274,27.1887698947861,13.0759184676546));
#60889=CARTESIAN_POINT('Ctrl Pts',(-1.71458872092426,27.267528625935,12.4732864297923));
#60890=CARTESIAN_POINT('Ctrl Pts',(-1.36884492613267,27.3462483275648,11.9394379232924));
#60891=CARTESIAN_POINT('Ctrl Pts',(-0.70698405798605,27.4446367079999,11.4662517905201));
#60892=CARTESIAN_POINT('Ctrl Pts',(0.26369106877084,27.5628332690564,11.3485606956223));
#60893=CARTESIAN_POINT('Ctrl Pts',(1.0981402772834,27.6714443490113,11.6808658118425));
#60894=CARTESIAN_POINT('Ctrl Pts',(1.54051757875863,27.7506962815273,12.1524788553328));
#60895=CARTESIAN_POINT('Ctrl Pts',(1.84914657465594,27.8301302588617,12.7108103129009));
#60896=CARTESIAN_POINT('Ctrl Pts',(1.99124333212888,27.9197763693575,13.4383409983297));
#60897=CARTESIAN_POINT('Ctrl Pts',(1.69157490439921,28.0400551413582,14.3869079450905));
#60898=CARTESIAN_POINT('Ctrl Pts',(0.967913781868604,28.161232439135,15.0804189065668));
#60899=CARTESIAN_POINT('Ctrl Pts',(0.236898065015672,28.2528990467938,15.2797343214628));
#60900=CARTESIAN_POINT('Ctrl Pts',(-0.256396961820482,28.3143776465486,
15.2559660017045));
#60901=CARTESIAN_POINT('Ctrl Pts',(-0.581447335792858,28.3554674913674,
15.199352676256));
#60902=CARTESIAN_POINT('Ctrl Pts',(-1.12758078740518,28.427647487958,14.9947667283049));
#60903=CARTESIAN_POINT('Ctrl Pts',(-1.76668039195127,28.5315859685482,14.4203289995239));
#60904=CARTESIAN_POINT('Ctrl Pts',(-2.11241412791876,28.6577713529391,13.4354362620173));
#60905=CARTESIAN_POINT('Ctrl Pts',(-1.94415965776118,28.7855287958173,12.3926356463114));
#60906=CARTESIAN_POINT('Ctrl Pts',(-1.28709989343125,28.9149925371647,11.5472179574802));
#60907=CARTESIAN_POINT('Ctrl Pts',(-0.292607727366596,29.0462639180579,
11.1123089037218));
#60908=CARTESIAN_POINT('Ctrl Pts',(0.804588712071932,29.1794592226303,11.2094456209673));
#60909=CARTESIAN_POINT('Ctrl Pts',(1.73583205505676,29.3146707075153,11.8284690342478));
#60910=CARTESIAN_POINT('Ctrl Pts',(2.26417093221696,29.4519935094771,12.8334741804398));
#60911=CARTESIAN_POINT('Ctrl Pts',(2.24809958300362,29.5915094474061,13.986994234328));
#60912=CARTESIAN_POINT('Ctrl Pts',(1.67109489210224,29.7332937418437,15.0075722135221));
#60913=CARTESIAN_POINT('Ctrl Pts',(0.66000801350798,29.8774136601739,15.638529834413));
#60914=CARTESIAN_POINT('Ctrl Pts',(-0.549282263292639,30.0239247293364,
15.7083465051647));
#60915=CARTESIAN_POINT('Ctrl Pts',(-1.66341375918974,30.1728778873614,15.183494477126));
#60916=CARTESIAN_POINT('Ctrl Pts',(-2.40078887024112,30.3243089042397,14.171542457301));
#60917=CARTESIAN_POINT('Ctrl Pts',(-2.5680794198884,30.4782495006503,12.9099920866041));
#60918=CARTESIAN_POINT('Ctrl Pts',(-2.10227569826999,30.6347178961047,11.7029795959583));
#60919=CARTESIAN_POINT('Ctrl Pts',(-1.099422358496,30.7937246705641,10.8527680575381));
#60920=CARTESIAN_POINT('Ctrl Pts',(0.208686593541593,30.9552704783395,10.583455503078));
#60921=CARTESIAN_POINT('Ctrl Pts',(1.50669405192392,31.1193447223469,10.9778789791109));
#60922=CARTESIAN_POINT('Ctrl Pts',(2.47064500602316,31.2859296882988,11.9612249409767));
#60923=CARTESIAN_POINT('Ctrl Pts',(2.85300271797787,31.4549955845984,13.3065477084251));
#60924=CARTESIAN_POINT('Ctrl Pts',(2.53795286772821,31.6265050134944,14.6881636271129));
#60925=CARTESIAN_POINT('Ctrl Pts',(1.48295699509012,31.8197329935747,15.8894733488012));
#60926=CARTESIAN_POINT('Ctrl Pts',(-0.280229930860079,32.035618744607,16.3710973081691));
#60927=CARTESIAN_POINT('Ctrl Pts',(-2.15081028972353,32.2751309791266,15.580042893293));
#60928=CARTESIAN_POINT('Ctrl Pts',(-2.93858630014624,32.4677611138487,14.1525095439616));
#60929=CARTESIAN_POINT('Ctrl Pts',(-2.98749309815322,32.6111465582849,12.9948958526763));
#60930=CARTESIAN_POINT('Ctrl Pts',(-2.7861141694091,32.734702881444,12.0180105874398));
#60931=CARTESIAN_POINT('Ctrl Pts',(-2.0825477001382,32.8903556440484,10.9405982741765));
#60932=CARTESIAN_POINT('Ctrl Pts',(-0.70859414989923,33.0789570730078,10.2035586577117));
#60933=CARTESIAN_POINT('Ctrl Pts',(0.864638831344568,33.2692662739014,10.2149555232629));
#60934=CARTESIAN_POINT('Ctrl Pts',(2.25160648933118,33.4611625443139,10.9853190100463));
#60935=CARTESIAN_POINT('Ctrl Pts',(3.10694020067178,33.654520061052,12.3356852583592));
#60936=CARTESIAN_POINT('Ctrl Pts',(3.21050915241751,33.8492083537085,13.942300082335));
#60937=CARTESIAN_POINT('Ctrl Pts',(2.60302857722243,34.0233253005977,15.2478759161299));
#60938=CARTESIAN_POINT('Ctrl Pts',(1.66634032706253,34.1763599369296,16.0648414204235));
#60939=CARTESIAN_POINT('Ctrl Pts',(0.345723459276493,34.351824509667,16.6045506981994));
#60940=CARTESIAN_POINT('Ctrl Pts',(-1.13582313320976,34.5280489966315,16.4337048222816));
#60941=CARTESIAN_POINT('Ctrl Pts',(-2.30773215451618,34.7048629830541,15.6022180335656));
#60942=CARTESIAN_POINT('Ctrl Pts',(-3.20698121046816,34.893077038371,14.3641858400115));
#60943=CARTESIAN_POINT('Ctrl Pts',(-3.38226190010022,35.137250306665,12.2738458881984));
#60944=CARTESIAN_POINT('Ctrl Pts',(-1.78032562074241,35.4374117618199,10.2472449611088));
#60945=CARTESIAN_POINT('Ctrl Pts',(0.767739927198404,35.7375427030933,9.85215574957131));
#60946=CARTESIAN_POINT('Ctrl Pts',(2.90007050052391,36.0371092053627,11.2998802053865));
#60947=CARTESIAN_POINT('Ctrl Pts',(3.46863907485259,36.3355857059691,13.8013388090782));
#60948=CARTESIAN_POINT('Ctrl Pts',(2.19014031354954,36.6324632872062,16.011210119302));
#60949=CARTESIAN_POINT('Ctrl Pts',(-0.300336734610397,36.934793930127,16.7642029639074));
#60950=CARTESIAN_POINT('Ctrl Pts',(-1.85637334099781,37.1370206026804,15.9511673814496));
#60951=CARTESIAN_POINT('Ctrl Pts',(-2.38258859188221,37.2412832822401,15.3016438780132));
#60952=CARTESIAN_POINT('Ctrl Pts',(-0.790532179204624,24.1655288633479,
10.9282793432527));
#60953=CARTESIAN_POINT('Ctrl Pts',(-0.705496619700135,24.1767170952653,
10.9031561171223));
#60954=CARTESIAN_POINT('Ctrl Pts',(-0.619144472715279,24.1877826920262,
10.8826943635782));
#60955=CARTESIAN_POINT('Ctrl Pts',(-0.532069686028644,24.1987800959838,
10.8669106881475));
#60956=CARTESIAN_POINT('Ctrl Pts',(-0.483596225465598,24.2049022152254,
10.858124110567));
#60957=CARTESIAN_POINT('Ctrl Pts',(-0.434899379414604,24.2110031686845,
10.8507864916071));
#60958=CARTESIAN_POINT('Ctrl Pts',(-0.386085050814084,24.2170920918391,
10.8448946532159));
#60959=CARTESIAN_POINT('Ctrl Pts',(-0.27235985485341,24.231277762293,10.8311681410461));
#60960=CARTESIAN_POINT('Ctrl Pts',(-0.157995879763926,24.245402739549,10.8252904681307));
#60961=CARTESIAN_POINT('Ctrl Pts',(-0.044133356191355,24.2596412506791,
10.8271840731439));
#60962=CARTESIAN_POINT('Ctrl Pts',(-0.00672289068076599,24.2643194302315,
10.8278062325938));
#60963=CARTESIAN_POINT('Ctrl Pts',(0.0306330371977953,24.2690098023138,
10.8292672357684));
#60964=CARTESIAN_POINT('Ctrl Pts',(0.0678928039773157,24.2737183571399,
10.8315639981628));
#60965=CARTESIAN_POINT('Ctrl Pts',(0.166869893362189,24.2862261931297,10.8376651328842));
#60966=CARTESIAN_POINT('Ctrl Pts',(0.26520479343476,24.2988712150022,10.8496654424747));
#60967=CARTESIAN_POINT('Ctrl Pts',(0.362271568845702,24.3115482937811,10.867392080451));
#60968=CARTESIAN_POINT('Ctrl Pts',(0.410662303838928,24.3178682024943,10.8762293477549));
#60969=CARTESIAN_POINT('Ctrl Pts',(0.458738358994614,24.3241961434368,10.8864904394408));
#60970=CARTESIAN_POINT('Ctrl Pts',(0.506424551980968,24.3305194888752,10.8981581464292));
#60971=CARTESIAN_POINT('Ctrl Pts',(0.603301083544006,24.3433656343858,10.9218615899954));
#60972=CARTESIAN_POINT('Ctrl Pts',(0.698567758984909,24.3561892987608,10.951371162955));
#60973=CARTESIAN_POINT('Ctrl Pts',(0.7914604069988,24.368854727582,10.9864979260627));
#60974=CARTESIAN_POINT('Ctrl Pts',(0.83358748498768,24.3745985352904,11.0024280122491));
#60975=CARTESIAN_POINT('Ctrl Pts',(0.875226967343351,24.3803098774156,11.0195131178887));
#60976=CARTESIAN_POINT('Ctrl Pts',(0.916311035982236,24.3859764877482,11.0377348653186));
#60977=CARTESIAN_POINT('Ctrl Pts',(0.93496960169188,24.3885500113729,11.0460103765576));
#60978=CARTESIAN_POINT('Ctrl Pts',(0.953512771719649,24.3911142427904,11.0545199877682));
#60979=CARTESIAN_POINT('Ctrl Pts',(0.971933515321555,24.3936680138793,11.0632615340076));
#60980=CARTESIAN_POINT('Ctrl Pts',(0.971942242388927,24.3936692237617,11.063265675429));
#60981=CARTESIAN_POINT('Ctrl Pts',(0.971950969430421,24.3936704336419,11.0632698169033));
#60982=CARTESIAN_POINT('Ctrl Pts',(0.971959696446036,24.39367164352,11.0632739584305));
#60983=CARTESIAN_POINT('Ctrl Pts',(1.04914245071372,24.4043719481958,11.0999021122559));
#60984=CARTESIAN_POINT('Ctrl Pts',(1.12430172397661,24.4149077656456,11.1406668535456));
#60985=CARTESIAN_POINT('Ctrl Pts',(1.1970061235826,24.4253721436316,11.1852297915425));
#60986=CARTESIAN_POINT('Ctrl Pts',(1.22895635016355,24.4299707545753,11.2048131451474));
#60987=CARTESIAN_POINT('Ctrl Pts',(1.26043238448574,24.4345555211935,11.2251293302296));
#60988=CARTESIAN_POINT('Ctrl Pts',(1.29139731547581,24.4391341100558,11.2461464799215));
#60989=CARTESIAN_POINT('Ctrl Pts',(1.37098541213915,24.4509022994658,11.3001661366033));
#60990=CARTESIAN_POINT('Ctrl Pts',(1.44720127556825,24.4626330806121,11.3588201391346));
#60991=CARTESIAN_POINT('Ctrl Pts',(1.51953449180492,24.4744791334325,11.4216421310785));
#60992=CARTESIAN_POINT('Ctrl Pts',(1.53478362557048,24.4769764929231,11.4348861289043));
#60993=CARTESIAN_POINT('Ctrl Pts',(1.54986003924515,24.4794789505739,11.4483152792074));
#60994=CARTESIAN_POINT('Ctrl Pts',(1.56475870316925,24.4819878965692,11.4619250513116));
#60995=CARTESIAN_POINT('Ctrl Pts',(1.63920471899428,24.4945246605517,11.5299307003153));
#60996=CARTESIAN_POINT('Ctrl Pts',(1.70923359743602,24.507228457478,11.6024629594918));
#60997=CARTESIAN_POINT('Ctrl Pts',(1.77443543912681,24.520000136623,11.6788891281613));
#60998=CARTESIAN_POINT('Ctrl Pts',(1.78842496438163,24.5227403924703,11.6952869136993));
#60999=CARTESIAN_POINT('Ctrl Pts',(1.8021922749423,24.5254837910698,11.7118641446668));
#61000=CARTESIAN_POINT('Ctrl Pts',(1.8157332990014,24.5282293825457,11.7286148816749));
#61001=CARTESIAN_POINT('Ctrl Pts',(1.86939917563113,24.5391107289475,11.795001514016));
#61002=CARTESIAN_POINT('Ctrl Pts',(1.91952345758861,24.550000412573,11.8640972412425));
#61003=CARTESIAN_POINT('Ctrl Pts',(1.96588294352946,24.5607466336136,11.9354502051949));
#61004=CARTESIAN_POINT('Ctrl Pts',(1.98539079095622,24.5652685914442,11.9654751872667));
#61005=CARTESIAN_POINT('Ctrl Pts',(2.00423247487847,24.5697652275476,11.9959002729666));
#61006=CARTESIAN_POINT('Ctrl Pts',(2.02239321040764,24.5742255895454,12.0266938375357));
#61007=CARTESIAN_POINT('Ctrl Pts',(2.06903817571315,24.5856818122464,12.1057856093777));
#61008=CARTESIAN_POINT('Ctrl Pts',(2.11103045397057,24.5971236620765,12.1874184618897));
#61009=CARTESIAN_POINT('Ctrl Pts',(2.14791722509451,24.6085374701448,12.2710079526033));
#61010=CARTESIAN_POINT('Ctrl Pts',(2.15952133018242,24.6121281077702,12.2973041342676));
#61011=CARTESIAN_POINT('Ctrl Pts',(2.17062051788247,24.6157159717933,12.3237937961603));
#61012=CARTESIAN_POINT('Ctrl Pts',(2.18120170250727,24.6193006409265,12.3504583663367));
#61013=CARTESIAN_POINT('Ctrl Pts',(2.18122393174747,24.6193081716968,12.3505143839904));
#61014=CARTESIAN_POINT('Ctrl Pts',(2.18124615873495,24.6193157024643,12.3505704024998));
#61015=CARTESIAN_POINT('Ctrl Pts',(2.18126838346963,24.6193232332289,12.3506264218648));
#61016=CARTESIAN_POINT('Ctrl Pts',(2.20973609341923,24.6289694056803,12.4223817457815));
#61017=CARTESIAN_POINT('Ctrl Pts',(2.23450332313288,24.6386105247647,12.4955396730197));
#61018=CARTESIAN_POINT('Ctrl Pts',(2.2556350856279,24.6481441236829,12.5696228019282));
#61019=CARTESIAN_POINT('Ctrl Pts',(2.26875201254688,24.654061827912,12.6156077493765));
#61020=CARTESIAN_POINT('Ctrl Pts',(2.28046925525904,24.6599381860582,12.6619494053648));
#61021=CARTESIAN_POINT('Ctrl Pts',(2.29081156324566,24.6657495006055,12.7085376385827));
#61022=CARTESIAN_POINT('Ctrl Pts',(2.30207900199876,24.6720806435982,12.7592932402412));
#61023=CARTESIAN_POINT('Ctrl Pts',(2.3116601899614,24.6783999723304,12.8103653611132));
#61024=CARTESIAN_POINT('Ctrl Pts',(2.31952197262884,24.6847548600815,12.8616437840524));
#61025=CARTESIAN_POINT('Ctrl Pts',(2.33615474600301,24.6981995725917,12.9701309330633));
#61026=CARTESIAN_POINT('Ctrl Pts',(2.34509270969781,24.7118071130983,13.0795481055681));
#61027=CARTESIAN_POINT('Ctrl Pts',(2.34648323516451,24.7255126943041,13.1888535873786));
#61028=CARTESIAN_POINT('Ctrl Pts',(2.34666482489125,24.7273025160697,13.2031278693303));
#61029=CARTESIAN_POINT('Ctrl Pts',(2.34671764919802,24.7290940155374,13.2174002971286));
#61030=CARTESIAN_POINT('Ctrl Pts',(2.34664198787484,24.7308870536076,13.2316685936994));
#61031=CARTESIAN_POINT('Ctrl Pts',(2.3460443552167,24.7450498789838,13.3443708257972));
#61032=CARTESIAN_POINT('Ctrl Pts',(2.33743141035916,24.7593068482667,13.4568121330953));
#61033=CARTESIAN_POINT('Ctrl Pts',(2.3209700712763,24.7735505590859,13.5677977657174));
#61034=CARTESIAN_POINT('Ctrl Pts',(2.31920339452561,24.7750792337958,13.579709052875));
#61035=CARTESIAN_POINT('Ctrl Pts',(2.31734631797717,24.776607762684,13.5916036223843));
#61036=CARTESIAN_POINT('Ctrl Pts',(2.31539904563125,24.7781360179876,13.6034800327375));
#61037=CARTESIAN_POINT('Ctrl Pts',(2.30072012589076,24.7896563053219,13.6930067364601));
#61038=CARTESIAN_POINT('Ctrl Pts',(2.28107548322618,24.8010011828669,13.78152064807));
#61039=CARTESIAN_POINT('Ctrl Pts',(2.25639523308752,24.8122854609448,13.8683633433921));
#61040=CARTESIAN_POINT('Ctrl Pts',(2.24802818244187,24.8161110350637,13.8978045859193));
#61041=CARTESIAN_POINT('Ctrl Pts',(2.23908248514902,24.8199295887774,13.9270533262758));
#61042=CARTESIAN_POINT('Ctrl Pts',(2.22955587438,24.8237454230163,13.9560826342555));
#61043=CARTESIAN_POINT('Ctrl Pts',(2.22060788506496,24.8273294934508,13.9833487778949));
#61044=CARTESIAN_POINT('Ctrl Pts',(2.21114760051682,24.8309110769025,14.0104206574023));
#61045=CARTESIAN_POINT('Ctrl Pts',(2.20117766020254,24.8344898520955,14.0372755869749));
#61046=CARTESIAN_POINT('Ctrl Pts',(2.19666877540559,24.8361083457425,14.0494206730893));
#61047=CARTESIAN_POINT('Ctrl Pts',(2.19205566739131,24.837726261712,14.0615213648026));
#61048=CARTESIAN_POINT('Ctrl Pts',(2.18733850595882,24.8393436033777,14.0735758212477));
#61049=CARTESIAN_POINT('Ctrl Pts',(2.15412366891343,24.8507317529334,14.1584545798452));
#61050=CARTESIAN_POINT('Ctrl Pts',(2.11568162245519,24.8621133654551,14.241203190023));
#61051=CARTESIAN_POINT('Ctrl Pts',(2.07250095223306,24.8734753982924,14.3212727372763));
#61052=CARTESIAN_POINT('Ctrl Pts',(2.05683229597124,24.8775982566466,14.3503269924905));
#61053=CARTESIAN_POINT('Ctrl Pts',(2.04054018211963,24.8817185388973,14.3790286750262));
#61054=CARTESIAN_POINT('Ctrl Pts',(2.02364947288061,24.8858356285032,14.4073522635993));
#61055=CARTESIAN_POINT('Ctrl Pts',(1.97234923286759,24.8983399989205,14.4933762944002));
#61056=CARTESIAN_POINT('Ctrl Pts',(1.91552827492433,24.9108143979704,14.5759077643999));
#61057=CARTESIAN_POINT('Ctrl Pts',(1.85391371717396,24.9231899294079,14.6543719309755));
#61058=CARTESIAN_POINT('Ctrl Pts',(1.83723589444989,24.926539737099,14.6756106042391));
#61059=CARTESIAN_POINT('Ctrl Pts',(1.82020684408341,24.9298823279963,14.696551569122));
#61060=CARTESIAN_POINT('Ctrl Pts',(1.80284091122112,24.9332163962459,14.7171840815965));
#61061=CARTESIAN_POINT('Ctrl Pts',(1.72900519018026,24.9473920431954,14.8049085043222));
#61062=CARTESIAN_POINT('Ctrl Pts',(1.64890821977102,24.9615971674717,14.8869397613431));
#61063=CARTESIAN_POINT('Ctrl Pts',(1.56345082456623,24.9759033631905,14.9623497514021));
#61064=CARTESIAN_POINT('Ctrl Pts',(1.55458349057646,24.9773878200389,14.9701745343412));
#61065=CARTESIAN_POINT('Ctrl Pts',(1.54565845157056,24.9788733594118,14.9779279823833));
#61066=CARTESIAN_POINT('Ctrl Pts',(1.53667672267686,24.9803600573206,14.985609027744));
#61067=CARTESIAN_POINT('Ctrl Pts',(1.46649583481387,24.9919767271689,15.0456267135936));
#61068=CARTESIAN_POINT('Ctrl Pts',(1.39298361824446,25.0034897132474,15.1013960053529));
#61069=CARTESIAN_POINT('Ctrl Pts',(1.31653655629669,25.0149663173393,15.1524299601093));
#61070=CARTESIAN_POINT('Ctrl Pts',(1.28900030227362,25.0191001934825,15.1708124055058));
#61071=CARTESIAN_POINT('Ctrl Pts',(1.2610833151214,25.0232293098059,15.1885799835318));
#61072=CARTESIAN_POINT('Ctrl Pts',(1.2328044127504,25.0273566770993,15.2057083009526));
#61073=CARTESIAN_POINT('Ctrl Pts',(1.19862197354779,25.0323456784304,15.2264123460107));
#61074=CARTESIAN_POINT('Ctrl Pts',(1.1639127149925,25.0373318212796,15.2461809395287));
#61075=CARTESIAN_POINT('Ctrl Pts',(1.12872391769523,25.042314251943,15.2649699507994));
#61076=CARTESIAN_POINT('Ctrl Pts',(1.10539121064818,25.0456179623276,15.2774284185321));
#61077=CARTESIAN_POINT('Ctrl Pts',(1.08184768478996,25.0489200407177,15.2894562228361));
#61078=CARTESIAN_POINT('Ctrl Pts',(1.05810730004401,25.0522202396665,15.3010408104736));
#61079=CARTESIAN_POINT('Ctrl Pts',(1.05381435491867,25.0528170106599,15.3031356374766));
#61080=CARTESIAN_POINT('Ctrl Pts',(1.04951498853502,25.0534137180518,15.3052159649668));
#61081=CARTESIAN_POINT('Ctrl Pts',(1.04520923680936,25.0540103669038,15.3072817422161));
#61082=CARTESIAN_POINT('Ctrl Pts',(0.969805629592131,25.0644590593851,15.3434582489506));
#61083=CARTESIAN_POINT('Ctrl Pts',(0.892341956280082,25.0749036058817,15.3752162655216));
#61084=CARTESIAN_POINT('Ctrl Pts',(0.813439179742434,25.085329857511,15.402490680532));
#61085=CARTESIAN_POINT('Ctrl Pts',(0.76493533764984,25.0917391790183,15.4192570603336));
#61086=CARTESIAN_POINT('Ctrl Pts',(0.715888201301439,25.0981415910813,15.4343300757289));
#61087=CARTESIAN_POINT('Ctrl Pts',(0.666445302518113,25.1045338451292,15.4477037384638));
#61088=CARTESIAN_POINT('Ctrl Pts',(0.614869246181018,25.1112018856974,15.4616543926451));
#61089=CARTESIAN_POINT('Ctrl Pts',(0.562857337859564,25.1178595682796,15.4737578028836));
#61090=CARTESIAN_POINT('Ctrl Pts',(0.510559142633728,25.1244846159198,15.4840465880969));
#61091=CARTESIAN_POINT('Ctrl Pts',(0.400691370382397,25.1384024810037,15.5056612137196));
#61092=CARTESIAN_POINT('Ctrl Pts',(0.289494973989037,25.1523103392757,15.5191035287391));
#61093=CARTESIAN_POINT('Ctrl Pts',(0.178168006039007,25.1662170317109,15.5243958968317));
#61094=CARTESIAN_POINT('Ctrl Pts',(0.154206513136954,25.1692102427739,15.5255350012447));
#61095=CARTESIAN_POINT('Ctrl Pts',(0.130238937104567,25.1722033992284,15.52629636005));
#61096=CARTESIAN_POINT('Ctrl Pts',(0.106277191373282,25.1751965882398,15.5266798849848));
#61097=CARTESIAN_POINT('Ctrl Pts',(-0.0157005557933355,25.1904334769267,
15.528632226357));
#61098=CARTESIAN_POINT('Ctrl Pts',(-0.137518646175449,25.2055947319702,
15.5209039553958));
#61099=CARTESIAN_POINT('Ctrl Pts',(-0.257535222984943,25.2207227529219,
15.5034159658435));
#61100=CARTESIAN_POINT('Ctrl Pts',(-0.32788569056501,25.2295903891752,15.4931649798986));
#61101=CARTESIAN_POINT('Ctrl Pts',(-0.39761384151569,25.2384462211708,15.4795598380239));
#61102=CARTESIAN_POINT('Ctrl Pts',(-0.466367579709816,25.2472885820012,
15.4625996730074));
#61103=CARTESIAN_POINT('Ctrl Pts',(-0.508500016991226,25.2527071995613,
15.4522064477428));
#61104=CARTESIAN_POINT('Ctrl Pts',(-0.55026502310578,25.2581205625057,15.4405538196307));
#61105=CARTESIAN_POINT('Ctrl Pts',(-0.591582755307492,25.2635284025615,
15.4276425302246));
#61106=CARTESIAN_POINT('Ctrl Pts',(-0.64233587687555,25.2701711864015,15.4117827962579));
#61107=CARTESIAN_POINT('Ctrl Pts',(-0.692434795980019,25.276808341162,15.3940173763629));
#61108=CARTESIAN_POINT('Ctrl Pts',(-0.741770597672253,25.2834392934233,
15.3744395748014));
#61109=CARTESIAN_POINT('Ctrl Pts',(-0.857544245502194,25.2989997891597,
15.3284974105817));
#61110=CARTESIAN_POINT('Ctrl Pts',(-0.969110719126935,25.3145257007673,
15.2725724022707));
#61111=CARTESIAN_POINT('Ctrl Pts',(-1.07505557528344,25.3300070899883,15.2079177932711));
#61112=CARTESIAN_POINT('Ctrl Pts',(-1.18911110385875,25.3466736663067,15.1383135116495));
#61113=CARTESIAN_POINT('Ctrl Pts',(-1.29665566949087,25.3632890992371,15.0585942988193));
#61114=CARTESIAN_POINT('Ctrl Pts',(-1.39601903951251,25.3798514631867,14.9703134442671));
#61115=CARTESIAN_POINT('Ctrl Pts',(-1.47922852439741,25.3937212199434,14.8963847476972));
#61116=CARTESIAN_POINT('Ctrl Pts',(-1.55669744124286,25.4075529445037,14.8164578973725));
#61117=CARTESIAN_POINT('Ctrl Pts',(-1.62747830354971,25.4213506382061,14.731414023057));
#61118=CARTESIAN_POINT('Ctrl Pts',(-1.66759405307742,25.429170616751,14.6832145712601));
#61119=CARTESIAN_POINT('Ctrl Pts',(-1.70556177787918,25.4369797441687,14.6333706895916));
#61120=CARTESIAN_POINT('Ctrl Pts',(-1.74120779536032,25.4447788901693,14.5820398672115));
#61121=CARTESIAN_POINT('Ctrl Pts',(-1.76668649433977,25.4503534846762,14.5453501424061));
#61122=CARTESIAN_POINT('Ctrl Pts',(-1.79097852609347,25.4559228466412,14.5079016655005));
#61123=CARTESIAN_POINT('Ctrl Pts',(-1.81402318205396,25.4614881423788,14.4697456290445));
#61124=CARTESIAN_POINT('Ctrl Pts',(-1.82321919151665,25.4637089831826,14.4545193972921));
#61125=CARTESIAN_POINT('Ctrl Pts',(-1.83221652257459,25.4659291714859,14.4391805132043));
#61126=CARTESIAN_POINT('Ctrl Pts',(-1.84101122675499,25.4681487818585,14.4237321791533));
#61127=CARTESIAN_POINT('Ctrl Pts',(-1.88684654114243,25.4797167137817,14.3432201763085));
#61128=CARTESIAN_POINT('Ctrl Pts',(-1.92720831415073,25.4912775260564,14.2596729273911));
#61129=CARTESIAN_POINT('Ctrl Pts',(-1.96195986740268,25.5028194777214,14.1739469541749));
#61130=CARTESIAN_POINT('Ctrl Pts',(-1.97652305852491,25.5076563161441,14.138022121606));
#61131=CARTESIAN_POINT('Ctrl Pts',(-1.99010154975033,25.5124898446114,14.1017150196534));
#61132=CARTESIAN_POINT('Ctrl Pts',(-2.00268767175644,25.5173192087944,14.0650899071979));
#61133=CARTESIAN_POINT('Ctrl Pts',(-2.03305155914572,25.5289699992557,13.9767322073694));
#61134=CARTESIAN_POINT('Ctrl Pts',(-2.05764605012002,25.5405910885114,13.8865324065618));
#61135=CARTESIAN_POINT('Ctrl Pts',(-2.07648640744474,25.5521405012169,13.7953550858352));
#61136=CARTESIAN_POINT('Ctrl Pts',(-2.08463482010811,25.5571355965393,13.7559210972959));
#61137=CARTESIAN_POINT('Ctrl Pts',(-2.09170733081712,25.5621173521082,13.7163037678985));
#61138=CARTESIAN_POINT('Ctrl Pts',(-2.09770689659465,25.5670826828953,13.6765705608211));
#61139=CARTESIAN_POINT('Ctrl Pts',(-2.1132466639355,25.5799436278473,13.5736556472115));
#61140=CARTESIAN_POINT('Ctrl Pts',(-2.1213613048407,25.5928052311059,13.4698990160121));
#61141=CARTESIAN_POINT('Ctrl Pts',(-2.12187461644586,25.6057095945976,13.3664402375084));
#61142=CARTESIAN_POINT('Ctrl Pts',(-2.12200261201119,25.6089273307325,13.3406425257282));
#61143=CARTESIAN_POINT('Ctrl Pts',(-2.12165791636404,25.6121476908188,13.3148635757551));
#61144=CARTESIAN_POINT('Ctrl Pts',(-2.12083770945619,25.6153712581238,13.2891215522233));
#61145=CARTESIAN_POINT('Ctrl Pts',(-2.11938579728351,25.6210775458481,13.243553590094));
#61146=CARTESIAN_POINT('Ctrl Pts',(-2.11644439600435,25.6267938637586,13.1980997598415));
#61147=CARTESIAN_POINT('Ctrl Pts',(-2.11199908667531,25.6325229244125,13.1528573978578));
#61148=CARTESIAN_POINT('Ctrl Pts',(-2.10483338533847,25.641757993234,13.0799281077339));
#61149=CARTESIAN_POINT('Ctrl Pts',(-2.09402822430077,25.6509132713589,13.0075333641132));
#61150=CARTESIAN_POINT('Ctrl Pts',(-2.07943293734265,25.6600407951577,12.9360188309056));
#61151=CARTESIAN_POINT('Ctrl Pts',(-2.0751099749949,25.6627442666156,12.9148370182245));
#61152=CARTESIAN_POINT('Ctrl Pts',(-2.07045436364957,25.665445268338,12.893732736597));
#61153=CARTESIAN_POINT('Ctrl Pts',(-2.06546185421087,25.6681450640045,12.8727157771258));
#61154=CARTESIAN_POINT('Ctrl Pts',(-2.06544940448432,25.668151796434,12.8726633675306));
#61155=CARTESIAN_POINT('Ctrl Pts',(-2.06543695264387,25.6681585288649,12.8726109584431));
#61156=CARTESIAN_POINT('Ctrl Pts',(-2.06542449868951,25.6681652612972,12.8725585498632));
#61157=CARTESIAN_POINT('Ctrl Pts',(-2.04706670352818,25.6780892267127,12.7953054986337));
#61158=CARTESIAN_POINT('Ctrl Pts',(-2.02411173197653,25.6880159792777,12.719157839309));
#61159=CARTESIAN_POINT('Ctrl Pts',(-1.99691841665238,25.6979165175409,12.6446076271924));
#61160=CARTESIAN_POINT('Ctrl Pts',(-1.97815704130777,25.7047471563305,12.5931734973385));
#61161=CARTESIAN_POINT('Ctrl Pts',(-1.95737933574469,25.711565369604,12.5424992703761));
#61162=CARTESIAN_POINT('Ctrl Pts',(-1.93471454859936,25.7183623386049,12.4927378129865));
#61163=CARTESIAN_POINT('Ctrl Pts',(-1.90381859825576,25.727627760574,12.4249045036916));
#61164=CARTESIAN_POINT('Ctrl Pts',(-1.86951402923737,25.736814826264,12.3587326941799));
#61165=CARTESIAN_POINT('Ctrl Pts',(-1.83195605601144,25.7459738178074,12.2945925865526));
#61166=CARTESIAN_POINT('Ctrl Pts',(-1.799712190562,25.7538368962861,12.2395277142336));
#61167=CARTESIAN_POINT('Ctrl Pts',(-1.76507040226176,25.7616791745314,12.1859612746389));
#61168=CARTESIAN_POINT('Ctrl Pts',(-1.72814447768616,25.7695284244644,12.1341536739523));
#61169=CARTESIAN_POINT('Ctrl Pts',(-1.67904171679383,25.7799660735435,12.0652617976308));
#61170=CARTESIAN_POINT('Ctrl Pts',(-1.62589626718616,25.7904174914076,11.9994767187561));
#61171=CARTESIAN_POINT('Ctrl Pts',(-1.56903195918004,25.8009195175335,11.9373505639572));
#61172=CARTESIAN_POINT('Ctrl Pts',(-1.55282802297368,25.8039121532895,11.9196472227155));
#61173=CARTESIAN_POINT('Ctrl Pts',(-1.53632224392474,25.8069088566848,11.902241282607));
#61174=CARTESIAN_POINT('Ctrl Pts',(-1.51952248701259,25.8099103799305,11.8851461970513));
#61175=CARTESIAN_POINT('Ctrl Pts',(-1.47307690973132,25.8182085642789,11.8378841371619));
#61176=CARTESIAN_POINT('Ctrl Pts',(-1.42436848087704,25.8265465474126,11.7929833373008));
#61177=CARTESIAN_POINT('Ctrl Pts',(-1.3736949908021,25.8348777561905,11.7505909960002));
#61178=CARTESIAN_POINT('Ctrl Pts',(-1.32316410291418,25.8431855197984,11.7083179525923));
#61179=CARTESIAN_POINT('Ctrl Pts',(-1.27067975251719,25.8514865453385,11.6685385981701));
#61180=CARTESIAN_POINT('Ctrl Pts',(-1.21649750600729,25.8597412413196,11.6313665775228));
#61181=CARTESIAN_POINT('Ctrl Pts',(-1.20785701892122,25.8610576244269,11.6254387250424));
#61182=CARTESIAN_POINT('Ctrl Pts',(-1.19917326060815,25.862372843015,11.6195771253524));
#61183=CARTESIAN_POINT('Ctrl Pts',(-1.19044715961659,25.8636867521325,11.6137821819781));
#61184=CARTESIAN_POINT('Ctrl Pts',(-1.19043009629525,25.863689321396,11.6137708503443));
#61185=CARTESIAN_POINT('Ctrl Pts',(-1.19041303281199,25.8636918906546,11.6137595189654));
#61186=CARTESIAN_POINT('Ctrl Pts',(-1.19039596916682,25.8636944599082,11.6137481878413));
#61187=CARTESIAN_POINT('Ctrl Pts',(-1.1264798774272,25.8733182328611,11.5713046678307));
#61188=CARTESIAN_POINT('Ctrl Pts',(-1.0602419068925,25.88287799545,11.5324007693119));
#61189=CARTESIAN_POINT('Ctrl Pts',(-0.992127910317745,25.8923960439564,
11.497249014445));
#61190=CARTESIAN_POINT('Ctrl Pts',(-0.954893728848248,25.8975990383944,
11.4780334804064));
#61191=CARTESIAN_POINT('Ctrl Pts',(-0.917099873275302,25.9027894827606,
11.4599391294038));
#61192=CARTESIAN_POINT('Ctrl Pts',(-0.878825649101653,25.9079703957492,
11.4429997173555));
#61193=CARTESIAN_POINT('Ctrl Pts',(-0.806452006496361,25.917767107586,11.4109685794291));
#61194=CARTESIAN_POINT('Ctrl Pts',(-0.732357649991044,25.9275309240989,
11.383069151588));
#61195=CARTESIAN_POINT('Ctrl Pts',(-0.657042265930863,25.9372912720487,
11.3595166165103));
#61196=CARTESIAN_POINT('Ctrl Pts',(-0.617950712547168,25.9423572644442,
11.3472919535971));
#61197=CARTESIAN_POINT('Ctrl Pts',(-0.578531040024393,25.9474222116115,
11.3362385664458));
#61198=CARTESIAN_POINT('Ctrl Pts',(-0.538858577138134,25.9524895090482,
11.3263872119904));
#61199=CARTESIAN_POINT('Ctrl Pts',(-0.461125338555252,25.9624182458083,
11.3070847127117));
#61200=CARTESIAN_POINT('Ctrl Pts',(-0.382413447933152,25.972357367322,11.2923951419602));
#61201=CARTESIAN_POINT('Ctrl Pts',(-0.303259288052649,25.9823332138581,
11.2825335805622));
#61202=CARTESIAN_POINT('Ctrl Pts',(-0.297711178831835,25.9830324454113,
11.2818423595347));
#61203=CARTESIAN_POINT('Ctrl Pts',(-0.292160916532026,25.983731854668,11.2811748657093));
#61204=CARTESIAN_POINT('Ctrl Pts',(-0.286608694963468,25.9844314494653,
11.2805311761697));
#61205=CARTESIAN_POINT('Ctrl Pts',(-0.222577255127463,25.9924995824858,
11.2731077750104));
#61206=CARTESIAN_POINT('Ctrl Pts',(-0.158271073497767,26.0005943248532,
11.2688495367221));
#61207=CARTESIAN_POINT('Ctrl Pts',(-0.094001194438398,26.0086819927456,
11.2676757735204));
#61208=CARTESIAN_POINT('Ctrl Pts',(-0.0387229759484104,26.0156381575833,
11.2666662253515));
#61209=CARTESIAN_POINT('Ctrl Pts',(0.0165292080911561,26.0225891930742,
11.2679379464167));
#61210=CARTESIAN_POINT('Ctrl Pts',(0.0715880859921679,26.0295175830648,
11.2714396645856));
#61211=CARTESIAN_POINT('Ctrl Pts',(0.084378900806373,26.0311271282772,11.2722531542595));
#61212=CARTESIAN_POINT('Ctrl Pts',(0.0971588050985991,26.0327353844242,
11.2731869421992));
#61213=CARTESIAN_POINT('Ctrl Pts',(0.109925490074801,26.0343421056677,11.2742403467456));
#61214=CARTESIAN_POINT('Ctrl Pts',(0.109972769734755,26.0343480559386,11.2742442478843));
#61215=CARTESIAN_POINT('Ctrl Pts',(0.110020049213505,26.0343540061884,11.2742481506635));
#61216=CARTESIAN_POINT('Ctrl Pts',(0.11006732851095,26.0343599564172,11.2742520550831));
#61217=CARTESIAN_POINT('Ctrl Pts',(0.188020361137296,26.0441705586301,11.2806895735294));
#61218=CARTESIAN_POINT('Ctrl Pts',(0.265575905387572,26.0539352675481,11.2915938245673));
#61219=CARTESIAN_POINT('Ctrl Pts',(0.342214902082606,26.063668281761,11.3068339293819));
#61220=CARTESIAN_POINT('Ctrl Pts',(0.390739736116091,26.0698308480744,11.3164833714241));
#61221=CARTESIAN_POINT('Ctrl Pts',(0.438896281133394,26.0759806095347,11.3278703749953));
#61222=CARTESIAN_POINT('Ctrl Pts',(0.486545379588903,26.0821201325041,11.3409539337011));
#61223=CARTESIAN_POINT('Ctrl Pts',(0.563970580707379,26.0920962667036,11.362213457952));
#61224=CARTESIAN_POINT('Ctrl Pts',(0.640056503626392,26.1020463490841,11.3879562301718));
#61225=CARTESIAN_POINT('Ctrl Pts',(0.71424317795541,26.1119894619148,11.4180218755906));
#61226=CARTESIAN_POINT('Ctrl Pts',(0.759084224907484,26.1179994305961,11.4361946138898));
#61227=CARTESIAN_POINT('Ctrl Pts',(0.803230433542023,26.1240067201267,11.4559463527347));
#61228=CARTESIAN_POINT('Ctrl Pts',(0.846550212966073,26.1300143244821,11.4772370783737));
#61229=CARTESIAN_POINT('Ctrl Pts',(0.909556373290494,26.138752044023,11.5082032303457));
#61230=CARTESIAN_POINT('Ctrl Pts',(0.970821095358348,26.1474914138024,11.5424279026674));
#61231=CARTESIAN_POINT('Ctrl Pts',(1.02995902501875,26.156242665362,11.5797922673297));
#61232=CARTESIAN_POINT('Ctrl Pts',(1.08330906414026,26.1641374228509,11.6134997428524));
#61233=CARTESIAN_POINT('Ctrl Pts',(1.13493737523878,26.1720434998679,11.649770328516));
#61234=CARTESIAN_POINT('Ctrl Pts',(1.18465916249167,26.1799398318734,11.6883537635916));
#61235=CARTESIAN_POINT('Ctrl Pts',(1.2319428817391,26.1874489735649,11.7250452908378));
#61236=CARTESIAN_POINT('Ctrl Pts',(1.2775032029302,26.1949493480024,11.7638280765745));
#61237=CARTESIAN_POINT('Ctrl Pts',(1.32121473384328,26.2024283816673,11.8045145043413));
#61238=CARTESIAN_POINT('Ctrl Pts',(1.32122793493449,26.2024306403712,11.8045267918369));
#61239=CARTESIAN_POINT('Ctrl Pts',(1.32124113585729,26.2024328990732,11.8045390795064));
#61240=CARTESIAN_POINT('Ctrl Pts',(1.32125433661169,26.2024351577733,11.8045513673497));
#61241=CARTESIAN_POINT('Ctrl Pts',(1.37801297437162,26.2121467800477,11.8573848060531));
#61242=CARTESIAN_POINT('Ctrl Pts',(1.43169948115193,26.2218308038756,11.9134760130508));
#61243=CARTESIAN_POINT('Ctrl Pts',(1.48198939395346,26.2314938796934,11.9724026782956));
#61244=CARTESIAN_POINT('Ctrl Pts',(1.51313722648761,26.2374788546232,12.0088998165603));
#61245=CARTESIAN_POINT('Ctrl Pts',(1.54298181658575,26.2434556952527,12.0464836545084));
#61246=CARTESIAN_POINT('Ctrl Pts',(1.57144506963523,26.2494250094457,12.0850439326772));
#61247=CARTESIAN_POINT('Ctrl Pts',(1.61873444276281,26.2593425380465,12.1491086894025));
#61248=CARTESIAN_POINT('Ctrl Pts',(1.66220900579363,26.2692399343127,12.2158722020372));
#61249=CARTESIAN_POINT('Ctrl Pts',(1.70152968323113,26.2791263300845,12.2848631692563));
#61250=CARTESIAN_POINT('Ctrl Pts',(1.72475382543219,26.2849655748846,12.3256116033551));
#61251=CARTESIAN_POINT('Ctrl Pts',(1.74652835507116,26.2908008517139,12.367136242237));
#61252=CARTESIAN_POINT('Ctrl Pts',(1.76678028680931,26.2966329134192,12.4093320909615));
#61253=CARTESIAN_POINT('Ctrl Pts',(1.80005920530197,26.3062164291375,12.4786702769966));
#61254=CARTESIAN_POINT('Ctrl Pts',(1.82923081452741,26.3157924156678,12.5498286696334));
#61255=CARTESIAN_POINT('Ctrl Pts',(1.85398895827861,26.3253663094589,12.6223615583329));
#61256=CARTESIAN_POINT('Ctrl Pts',(1.87236010055433,26.33247037052,12.676182718407));
#61257=CARTESIAN_POINT('Ctrl Pts',(1.88830247173791,26.3395741832107,12.7307678714192));
#61258=CARTESIAN_POINT('Ctrl Pts',(1.90188226208757,26.3466673663647,12.7858629420231));
#61259=CARTESIAN_POINT('Ctrl Pts',(1.91546205243723,26.3537605495187,12.840958012627));
#61260=CARTESIAN_POINT('Ctrl Pts',(1.92668008312622,26.3608431015405,12.8965627720862));
#61261=CARTESIAN_POINT('Ctrl Pts',(1.93561630538568,26.367911785215,12.9524780880961));
#61262=CARTESIAN_POINT('Ctrl Pts',(1.93562275162362,26.3679168842843,12.9525184231976));
#61263=CARTESIAN_POINT('Ctrl Pts',(1.93562919656829,26.3679219833525,12.9525587584958));
#61264=CARTESIAN_POINT('Ctrl Pts',(1.93563564021965,26.3679270824197,12.9525990939906));
#61265=CARTESIAN_POINT('Ctrl Pts',(1.95062575478464,26.3797892388983,13.0464331104734));
#61266=CARTESIAN_POINT('Ctrl Pts',(1.95861245256558,26.3916455404621,13.1413327981437));
#61267=CARTESIAN_POINT('Ctrl Pts',(1.95972135279568,26.4034863493552,13.2362255096162));
#61268=CARTESIAN_POINT('Ctrl Pts',(1.96011599306144,26.4077003082321,13.2699963429669));
#61269=CARTESIAN_POINT('Ctrl Pts',(1.95964000198191,26.4119122991106,13.3037661489313));
#61270=CARTESIAN_POINT('Ctrl Pts',(1.95830058261461,26.4161218682396,13.3374862584528));
#61271=CARTESIAN_POINT('Ctrl Pts',(1.95434162975595,26.4285641892513,13.4371535674707));
#61272=CARTESIAN_POINT('Ctrl Pts',(1.94284017687827,26.4409852182778,13.5363853582024));
#61273=CARTESIAN_POINT('Ctrl Pts',(1.92400116712185,26.4533856195568,13.6340279456407));
#61274=CARTESIAN_POINT('Ctrl Pts',(1.91445570397717,26.4596687297053,13.683502081054));
#61275=CARTESIAN_POINT('Ctrl Pts',(1.90302703138298,26.4659463059117,13.7325664537329));
#61276=CARTESIAN_POINT('Ctrl Pts',(1.88973927860849,26.472219504861,13.7810795599549));
#61277=CARTESIAN_POINT('Ctrl Pts',(1.88062909918911,26.476520455438,13.8143404965012));
#61278=CARTESIAN_POINT('Ctrl Pts',(1.87064488666174,26.4808194051564,13.847342746645));
#61279=CARTESIAN_POINT('Ctrl Pts',(1.85979331324087,26.4851168427575,13.8800413709616));
#61280=CARTESIAN_POINT('Ctrl Pts',(1.85523491647467,26.4869220579926,13.8937770107222));
#61281=CARTESIAN_POINT('Ctrl Pts',(1.85052345568052,26.4887270075576,13.9074590790529));
#61282=CARTESIAN_POINT('Ctrl Pts',(1.84565939619719,26.4905317240626,13.9210842015379));
#61283=CARTESIAN_POINT('Ctrl Pts',(1.81614650041742,26.5014819211777,14.0037552340909));
#61284=CARTESIAN_POINT('Ctrl Pts',(1.78105506079411,26.5124100594858,14.0842289057742));
#61285=CARTESIAN_POINT('Ctrl Pts',(1.74082207812923,26.5233253660463,14.1619289386771));
#61286=CARTESIAN_POINT('Ctrl Pts',(1.70864272274104,26.5320557038368,14.2240753868607));
#61287=CARTESIAN_POINT('Ctrl Pts',(1.67317232189177,26.5407780438814,14.2844488396059));
#61288=CARTESIAN_POINT('Ctrl Pts',(1.6346238651926,26.5494960544694,14.3427400123217));
#61289=CARTESIAN_POINT('Ctrl Pts',(1.58845574675654,26.559937306333,14.4125532810273));
#61290=CARTESIAN_POINT('Ctrl Pts',(1.53787552728397,26.5703712878131,14.4793717093387));
#61291=CARTESIAN_POINT('Ctrl Pts',(1.4832791576902,26.5807970301582,14.5426113180809));
#61292=CARTESIAN_POINT('Ctrl Pts',(1.45068725105528,26.5870207923541,14.5803629019149));
#61293=CARTESIAN_POINT('Ctrl Pts',(1.41666303948595,26.5932418291801,14.6168403129119));
#61294=CARTESIAN_POINT('Ctrl Pts',(1.38129613268988,26.5994591668962,14.6519153510326));
#61295=CARTESIAN_POINT('Ctrl Pts',(1.35961950282918,26.6032698176033,14.6734130924969));
#61296=CARTESIAN_POINT('Ctrl Pts',(1.33743898344636,26.6070789961626,14.6943835775831));
#61297=CARTESIAN_POINT('Ctrl Pts',(1.31477635765406,26.6108863604908,14.7147970998005));
#61298=CARTESIAN_POINT('Ctrl Pts',(1.31247484687325,26.6112730186886,14.7168702020918));
#61299=CARTESIAN_POINT('Ctrl Pts',(1.31016836889469,26.611659657391,14.7189375563384));
#61300=CARTESIAN_POINT('Ctrl Pts',(1.30785693242784,26.6120462786337,14.720999144444));
#61301=CARTESIAN_POINT('Ctrl Pts',(1.24754470925209,26.6221343719074,14.7747920839022));
#61302=CARTESIAN_POINT('Ctrl Pts',(1.18380547269851,26.6322186925159,14.8246994538605));
#61303=CARTESIAN_POINT('Ctrl Pts',(1.11728747194782,26.642288086747,14.870392029666));
#61304=CARTESIAN_POINT('Ctrl Pts',(1.08014341960182,26.647910897147,14.8959070392632));
#61305=CARTESIAN_POINT('Ctrl Pts',(1.04213727426503,26.6535285142367,14.9201063881285));
#61306=CARTESIAN_POINT('Ctrl Pts',(1.00336745358979,26.6591415297132,14.9429479129451));
#61307=CARTESIAN_POINT('Ctrl Pts',(0.924298984036139,26.6705889012921,14.9895316829514));
#61308=CARTESIAN_POINT('Ctrl Pts',(0.842044189226941,26.682018815034,15.0304781036758));
#61309=CARTESIAN_POINT('Ctrl Pts',(0.757372202484891,26.6934429055962,15.0654266189583));
#61310=CARTESIAN_POINT('Ctrl Pts',(0.708942119160386,26.6999771760099,15.0854162232221));
#61311=CARTESIAN_POINT('Ctrl Pts',(0.659718569616521,26.7065098058046,15.1034428713422));
#61312=CARTESIAN_POINT('Ctrl Pts',(0.609871030073124,26.7130393843689,15.1194250206855));
#61313=CARTESIAN_POINT('Ctrl Pts',(0.577391561902696,26.7172939020661,15.1298386081092));
#61314=CARTESIAN_POINT('Ctrl Pts',(0.544647299040207,26.7215471137913,15.1393842404181));
#61315=CARTESIAN_POINT('Ctrl Pts',(0.511685614043769,26.72579860937,15.1480401775463));
#61316=CARTESIAN_POINT('Ctrl Pts',(0.494059682036892,26.7280720541895,15.1526688535164));
#61317=CARTESIAN_POINT('Ctrl Pts',(0.476371647943156,26.7303449999217,15.1570431209779));
#61318=CARTESIAN_POINT('Ctrl Pts',(0.45862857818344,26.7326174092138,15.1611597883168));
#61319=CARTESIAN_POINT('Ctrl Pts',(0.38046746716195,26.7426277421139,15.1792943781745));
#61320=CARTESIAN_POINT('Ctrl Pts',(0.301129619201349,26.7526414469723,15.192451208845));
#61321=CARTESIAN_POINT('Ctrl Pts',(0.221333754180482,26.7626470419077,15.2006242822204));
#61322=CARTESIAN_POINT('Ctrl Pts',(0.166144292991359,26.7695672425123,15.2062770502646));
#61323=CARTESIAN_POINT('Ctrl Pts',(0.110738439382832,26.7764832785875,15.2095467921131));
#61324=CARTESIAN_POINT('Ctrl Pts',(0.0553475638220142,26.7833923674015,
15.2104447558368));
#61325=CARTESIAN_POINT('Ctrl Pts',(-0.0390703674654303,26.795169431156,
15.2119754028308));
#61326=CARTESIAN_POINT('Ctrl Pts',(-0.133458536060384,26.8069280922523,
15.2066172944852));
#61327=CARTESIAN_POINT('Ctrl Pts',(-0.22680115270891,26.8186701463211,15.1944388640106));
#61328=CARTESIAN_POINT('Ctrl Pts',(-0.281207451622415,26.8255141981215,
15.1873404629534));
#61329=CARTESIAN_POINT('Ctrl Pts',(-0.335267285992045,26.832353670009,15.1779243281533));
#61330=CARTESIAN_POINT('Ctrl Pts',(-0.388799278321244,26.8391914212386,
15.1661949873908));
#61331=CARTESIAN_POINT('Ctrl Pts',(-0.423252557289703,26.8435922092604,
15.1586459642399));
#61332=CARTESIAN_POINT('Ctrl Pts',(-0.4574866653146,26.847992220101,15.1501386986599));
#61333=CARTESIAN_POINT('Ctrl Pts',(-0.49145180641335,26.852392081566,15.1406732080927));
#61334=CARTESIAN_POINT('Ctrl Pts',(-0.599371058044128,26.8663719957137,
15.1105980008277));
#61335=CARTESIAN_POINT('Ctrl Pts',(-0.704548142392309,26.8803470920764,
15.0708508825517));
#61336=CARTESIAN_POINT('Ctrl Pts',(-0.805424879994097,26.8943094435373,
15.0223366624272));
#61337=CARTESIAN_POINT('Ctrl Pts',(-0.813762095815551,26.8954633977617,
15.018327080702));
#61338=CARTESIAN_POINT('Ctrl Pts',(-0.822069946174581,26.8966172649693,
15.0142576422613));
#61339=CARTESIAN_POINT('Ctrl Pts',(-0.830347556806284,26.8977710407052,
15.0101288725927));
#61340=CARTESIAN_POINT('Ctrl Pts',(-0.91080387239077,26.9089854537587,14.9699982587943));
#61341=CARTESIAN_POINT('Ctrl Pts',(-0.988407123994427,26.9201971235708,
14.9242936222472));
#61342=CARTESIAN_POINT('Ctrl Pts',(-1.06244749711786,26.9314310570154,14.8735557043439));
#61343=CARTESIAN_POINT('Ctrl Pts',(-1.08585840943374,26.9349831275918,14.8575128226428));
#61344=CARTESIAN_POINT('Ctrl Pts',(-1.10891344923103,26.9385374708552,14.8409665277642));
#61345=CARTESIAN_POINT('Ctrl Pts',(-1.13159104930669,26.9420950068572,14.8239332758962));
#61346=CARTESIAN_POINT('Ctrl Pts',(-1.1946640178834,26.9519895440091,14.7765588731266));
#61347=CARTESIAN_POINT('Ctrl Pts',(-1.25476955099053,26.9618813400662,14.7253122557269));
#61348=CARTESIAN_POINT('Ctrl Pts',(-1.31137381328732,26.9717637864018,14.670461066501));
#61349=CARTESIAN_POINT('Ctrl Pts',(-1.31139052214061,26.9717667035734,14.6704448751324));
#61350=CARTESIAN_POINT('Ctrl Pts',(-1.31140723068865,26.9717696207442,14.6704286834497));
#61351=CARTESIAN_POINT('Ctrl Pts',(-1.31142393893143,26.9717725379141,14.6704124914531));
#61352=CARTESIAN_POINT('Ctrl Pts',(-1.33082736807509,26.9751602729854,14.6516085834398));
#61353=CARTESIAN_POINT('Ctrl Pts',(-1.34981315569576,26.9785457490261,14.6323860978909));
#61354=CARTESIAN_POINT('Ctrl Pts',(-1.36836037779142,26.9819253610666,14.6127570761749));
#61355=CARTESIAN_POINT('Ctrl Pts',(-1.42590474410372,26.9924109007471,14.5518563326483));
#61356=CARTESIAN_POINT('Ctrl Pts',(-1.47923450728921,27.0028405712445,14.4870294015218));
#61357=CARTESIAN_POINT('Ctrl Pts',(-1.52804058251419,27.0132426074834,14.4189863742454));
#61358=CARTESIAN_POINT('Ctrl Pts',(-1.57616415976755,27.0234991829656,14.3518948520406));
#61359=CARTESIAN_POINT('Ctrl Pts',(-1.61989074263381,27.0337289117467,14.2816768217104));
#61360=CARTESIAN_POINT('Ctrl Pts',(-1.65894551313848,27.0439651116435,14.2089685605005));
#61361=CARTESIAN_POINT('Ctrl Pts',(-1.6979841396017,27.0541970802099,14.1362903546504));
#61362=CARTESIAN_POINT('Ctrl Pts',(-1.73235238482967,27.0644360409672,14.0611322062671));
#61363=CARTESIAN_POINT('Ctrl Pts',(-1.76175618743411,27.0747075582735,13.9841704423163));
#61364=CARTESIAN_POINT('Ctrl Pts',(-1.77653058095541,27.0798686403549,13.9454998185878));
#61365=CARTESIAN_POINT('Ctrl Pts',(-1.79005226973994,27.0850380317582,13.9063733688481));
#61366=CARTESIAN_POINT('Ctrl Pts',(-1.80228759725112,27.0902195146341,13.8668735420617));
#61367=CARTESIAN_POINT('Ctrl Pts',(-1.80229046233201,27.0902207279541,13.8668642925995));
#61368=CARTESIAN_POINT('Ctrl Pts',(-1.80229332734293,27.0902219412749,13.8668550431156));
#61369=CARTESIAN_POINT('Ctrl Pts',(-1.80229619228388,27.0902231545967,13.8668457936099));
#61370=CARTESIAN_POINT('Ctrl Pts',(-1.82161493453645,27.0984047720284,13.8044749386984));
#61371=CARTESIAN_POINT('Ctrl Pts',(-1.8377521095277,27.106627436244,13.7411106197772));
#61372=CARTESIAN_POINT('Ctrl Pts',(-1.85056980592683,27.114845167761,13.6770854800078));
#61373=CARTESIAN_POINT('Ctrl Pts',(-1.8574351557973,27.1192467076516,13.642792657699));
#61374=CARTESIAN_POINT('Ctrl Pts',(-1.86334817017396,27.1236467259484,13.6083111509094));
#61375=CARTESIAN_POINT('Ctrl Pts',(-1.86828817979346,27.1280374245996,13.5736981560504));
#61376=CARTESIAN_POINT('Ctrl Pts',(-1.87384907442427,27.1329799681239,13.5347348276173));
#61377=CARTESIAN_POINT('Ctrl Pts',(-1.87817738865227,27.1379110306736,13.4956014988121));
#61378=CARTESIAN_POINT('Ctrl Pts',(-1.88124534124361,27.1428204812618,13.4563732323631));
#61379=CARTESIAN_POINT('Ctrl Pts',(-1.88670842728362,27.1515627124969,13.3865196774493));
#61380=CARTESIAN_POINT('Ctrl Pts',(-1.88817352459399,27.160236350819,13.3163590539875));
#61381=CARTESIAN_POINT('Ctrl Pts',(-1.88574467811591,27.168885879747,13.2463477102035));
#61382=CARTESIAN_POINT('Ctrl Pts',(-1.88469445278418,27.1726259079743,13.2160750324473));
#61383=CARTESIAN_POINT('Ctrl Pts',(-1.88291621065804,27.1763615122148,13.1858296027228));
#61384=CARTESIAN_POINT('Ctrl Pts',(-1.88041816319571,27.1800966692258,13.1556453328878));
#61385=CARTESIAN_POINT('Ctrl Pts',(-1.87412761009965,27.1895024967189,13.0796356673686));
#61386=CARTESIAN_POINT('Ctrl Pts',(-1.86336477392588,27.1989397763323,13.004033176327));
#61387=CARTESIAN_POINT('Ctrl Pts',(-1.84820671069898,27.208441770839,12.9293977240039));
#61388=CARTESIAN_POINT('Ctrl Pts',(-1.84820111143111,27.2084452808001,12.929370154262));
#61389=CARTESIAN_POINT('Ctrl Pts',(-1.84819551153823,27.2084487907615,12.929342584645));
#61390=CARTESIAN_POINT('Ctrl Pts',(-1.84818991102035,27.2084523007232,12.9293150151529));
#61391=CARTESIAN_POINT('Ctrl Pts',(-1.83030520988397,27.2196610168163,12.8412745629681));
#61392=CARTESIAN_POINT('Ctrl Pts',(-1.8060448615243,27.2308723673325,12.7545081592047));
#61393=CARTESIAN_POINT('Ctrl Pts',(-1.77577747562567,27.2420816866914,12.6698953588806));
#61394=CARTESIAN_POINT('Ctrl Pts',(-1.75287738960566,27.2505625769276,12.6058779239986));
#61395=CARTESIAN_POINT('Ctrl Pts',(-1.72668954665041,27.2591051415846,12.5430686690698));
#61396=CARTESIAN_POINT('Ctrl Pts',(-1.69724790405521,27.2676669113444,12.4818153629211));
#61397=CARTESIAN_POINT('Ctrl Pts',(-1.69724652292347,27.2676673129841,12.481812489478));
#61398=CARTESIAN_POINT('Ctrl Pts',(-1.69724514178453,27.2676677146238,12.4818096160383));
#61399=CARTESIAN_POINT('Ctrl Pts',(-1.69724376063839,27.2676681162635,12.4818067426021));
#61400=CARTESIAN_POINT('Ctrl Pts',(-1.66430207130025,27.2772476172591,12.4132724725238));
#61401=CARTESIAN_POINT('Ctrl Pts',(-1.62726066159056,27.2868384375968,12.3466995858302));
#61402=CARTESIAN_POINT('Ctrl Pts',(-1.58629098297827,27.2963888487984,12.2826368596186));
#61403=CARTESIAN_POINT('Ctrl Pts',(-1.57662795109612,27.298641390948,12.2675271446585));
#61404=CARTESIAN_POINT('Ctrl Pts',(-1.56674652444052,27.3008916571568,12.2525572529114));
#61405=CARTESIAN_POINT('Ctrl Pts',(-1.55664921499818,27.3031389170245,12.2377347113786));
#61406=CARTESIAN_POINT('Ctrl Pts',(-1.52072433105668,27.3111343687233,12.1849980801679));
#61407=CARTESIAN_POINT('Ctrl Pts',(-1.48206375949998,27.3190928728718,12.134121665641));
#61408=CARTESIAN_POINT('Ctrl Pts',(-1.44091793592416,27.3270608041123,12.0853539206243));
#61409=CARTESIAN_POINT('Ctrl Pts',(-1.44089965093364,27.3270643450196,12.0853322484914));
#61410=CARTESIAN_POINT('Ctrl Pts',(-1.44088136545198,27.3270678859289,12.0853105767744));
#61411=CARTESIAN_POINT('Ctrl Pts',(-1.44086307947923,27.3270714268401,12.0852889054732));
#61412=CARTESIAN_POINT('Ctrl Pts',(-1.37290541594973,27.340230806158,12.0047500678301));
#61413=CARTESIAN_POINT('Ctrl Pts',(-1.29814242898036,27.353423300194,11.9299261142695));
#61414=CARTESIAN_POINT('Ctrl Pts',(-1.2177183305258,27.3666107050185,11.8617505225983));
#61415=CARTESIAN_POINT('Ctrl Pts',(-1.171839339842,27.3741336345224,11.8228588546126));
#61416=CARTESIAN_POINT('Ctrl Pts',(-1.1241189340707,27.3816547985145,11.7861312188262));
#61417=CARTESIAN_POINT('Ctrl Pts',(-1.07477681256499,27.3891662459853,11.7517428934414));
#61418=CARTESIAN_POINT('Ctrl Pts',(-0.99956793163206,27.4006154407348,11.699327079317));
#61419=CARTESIAN_POINT('Ctrl Pts',(-0.920584331624732,27.4120420994908,
11.6523420033146));
#61420=CARTESIAN_POINT('Ctrl Pts',(-0.838579152359779,27.4234222755877,
11.6113921337498));
#61421=CARTESIAN_POINT('Ctrl Pts',(-0.794850714564251,27.4294906401351,
11.5895560272983));
#61422=CARTESIAN_POINT('Ctrl Pts',(-0.750262542867168,27.4355460182717,
11.5694357671497));
#61423=CARTESIAN_POINT('Ctrl Pts',(-0.704959621222531,27.4416147128761,
11.5510781899004));
#61424=CARTESIAN_POINT('Ctrl Pts',(-0.696050783088503,27.4428081241607,
11.5474681648003));
#61425=CARTESIAN_POINT('Ctrl Pts',(-0.687114326100849,27.4440021923229,
11.5439260602436));
#61426=CARTESIAN_POINT('Ctrl Pts',(-0.678150996518129,27.445196938178,11.5404524767586));
#61427=CARTESIAN_POINT('Ctrl Pts',(-0.652873478156679,27.4485662453099,
11.5306566113371));
#61428=CARTESIAN_POINT('Ctrl Pts',(-0.627382253185017,27.4519409421826,
11.5214056561756));
#61429=CARTESIAN_POINT('Ctrl Pts',(-0.601698775311904,27.455321496039,11.5127018755957));
#61430=CARTESIAN_POINT('Ctrl Pts',(-0.512785748786099,27.4670245557332,
11.4825704628098));
#61431=CARTESIAN_POINT('Ctrl Pts',(-0.421596875476661,27.478791232657,11.4590127255446));
#61432=CARTESIAN_POINT('Ctrl Pts',(-0.329148571622093,27.4905698807564,
11.4422447586241));
#61433=CARTESIAN_POINT('Ctrl Pts',(-0.26164332414904,27.4991705853848,11.4300008805929));
#61434=CARTESIAN_POINT('Ctrl Pts',(-0.193467731801849,27.5077775363492,
11.4213775047135));
#61435=CARTESIAN_POINT('Ctrl Pts',(-0.125034808865138,27.5163684720874,
11.416456530407));
#61436=CARTESIAN_POINT('Ctrl Pts',(-0.0519841159098541,27.5255391136717,
11.4112034947674));
#61437=CARTESIAN_POINT('Ctrl Pts',(0.0213678892687439,27.5346915349819,
11.4101692925342));
#61438=CARTESIAN_POINT('Ctrl Pts',(0.0945403155628665,27.5438002147465,
11.4134558015847));
#61439=CARTESIAN_POINT('Ctrl Pts',(0.144374619553393,27.5500037088676,11.4156940885923));
#61440=CARTESIAN_POINT('Ctrl Pts',(0.194126449213719,27.5561869384646,11.4199365452109));
#61441=CARTESIAN_POINT('Ctrl Pts',(0.243651158933981,27.5623809508564,11.4261604084152));
#61442=CARTESIAN_POINT('Ctrl Pts',(0.246929283648362,27.5627909430646,11.4265723764995));
#61443=CARTESIAN_POINT('Ctrl Pts',(0.250206368205759,27.5632009860023,11.4269930074509));
#61444=CARTESIAN_POINT('Ctrl Pts',(0.253482365585964,27.5636110783592,11.4274223086756));
#61445=CARTESIAN_POINT('Ctrl Pts',(0.295019741136255,27.5688107651305,11.4328655505729));
#61446=CARTESIAN_POINT('Ctrl Pts',(0.336382394805737,27.5740184062628,11.4397027942762));
#61447=CARTESIAN_POINT('Ctrl Pts',(0.377479965674802,27.5792312709867,11.4479033776284));
#61448=CARTESIAN_POINT('Ctrl Pts',(0.489172342174389,27.5933984647422,11.4701904039398));
#61449=CARTESIAN_POINT('Ctrl Pts',(0.59891405835899,27.6076025976756,11.5025514309844));
#61450=CARTESIAN_POINT('Ctrl Pts',(0.70498573918653,27.6218081421299,11.5443691488903));
#61451=CARTESIAN_POINT('Ctrl Pts',(0.80981178530218,27.6358468661932,11.5856957875506));
#61452=CARTESIAN_POINT('Ctrl Pts',(0.911053985636797,27.6498861793188,11.6362575654412));
#61453=CARTESIAN_POINT('Ctrl Pts',(1.00707860992282,27.6639253942448,11.6954416207046));
#61454=CARTESIAN_POINT('Ctrl Pts',(1.04156773713381,27.6689678536465,11.7166987349711));
#61455=CARTESIAN_POINT('Ctrl Pts',(1.07538405831602,27.6740108791178,11.73906822974));
#61456=CARTESIAN_POINT('Ctrl Pts',(1.10844854241686,27.6790679276367,11.7624938816867));
#61457=CARTESIAN_POINT('Ctrl Pts',(1.11475462243416,27.6800324112353,11.766961637336));
#61458=CARTESIAN_POINT('Ctrl Pts',(1.12103345404847,27.6809974777904,11.7714677574257));
#61459=CARTESIAN_POINT('Ctrl Pts',(1.1272846856579,27.6819631475066,11.7760121696997));
#61460=CARTESIAN_POINT('Ctrl Pts',(1.14385067003335,27.6845222063337,11.7880550226016));
#61461=CARTESIAN_POINT('Ctrl Pts',(1.16022285215818,27.6870855012016,11.8003667614323));
#61462=CARTESIAN_POINT('Ctrl Pts',(1.17639727375936,27.6896534044628,11.8129421599516));
#61463=CARTESIAN_POINT('Ctrl Pts',(1.24562276956801,27.7006438671096,11.8667640658569));
#61464=CARTESIAN_POINT('Ctrl Pts',(1.31119539583706,27.7117132341387,11.9253968527617));
#61465=CARTESIAN_POINT('Ctrl Pts',(1.3724868230913,27.7227907181938,11.9882690194109));
#61466=CARTESIAN_POINT('Ctrl Pts',(1.37686796078122,27.7235825415381,11.9927631490354));
#61467=CARTESIAN_POINT('Ctrl Pts',(1.38122721400554,27.724374403745,11.9972789200397));
#61468=CARTESIAN_POINT('Ctrl Pts',(1.38556434912975,27.7251662777597,12.0018161145392));
#61469=CARTESIAN_POINT('Ctrl Pts',(1.44325296611283,27.7356990639016,12.0621657389255));
#61470=CARTESIAN_POINT('Ctrl Pts',(1.49703119317074,27.7462334628006,12.1263084875048));
#61471=CARTESIAN_POINT('Ctrl Pts',(1.54636318879888,27.7566942978174,12.1937888134211));
#61472=CARTESIAN_POINT('Ctrl Pts',(1.55035953962408,27.7575417228226,12.1992553479232));
#61473=CARTESIAN_POINT('Ctrl Pts',(1.55432668879006,27.758388661677,12.2047437694752));
#61474=CARTESIAN_POINT('Ctrl Pts',(1.55826433952585,27.759235072631,12.2102538270502));
#61475=CARTESIAN_POINT('Ctrl Pts',(1.57774734208177,27.7634230079982,12.2375169016651));
#61476=CARTESIAN_POINT('Ctrl Pts',(1.59650875485946,27.7675980087701,12.2653106392325));
#61477=CARTESIAN_POINT('Ctrl Pts',(1.61451335491316,27.7717549888583,12.2936076191409));
#61478=CARTESIAN_POINT('Ctrl Pts',(1.61453750474986,27.7717605646772,12.2936455742991));
#61479=CARTESIAN_POINT('Ctrl Pts',(1.61456165322472,27.7717661404638,12.2936835303626));
#61480=CARTESIAN_POINT('Ctrl Pts',(1.61458580033765,27.7717717162178,12.2937214873314));
#61481=CARTESIAN_POINT('Ctrl Pts',(1.63439184598387,27.776345084453,12.3248547104929));
#61482=CARTESIAN_POINT('Ctrl Pts',(1.65327828751371,27.7808958585312,12.3565921302816));
#61483=CARTESIAN_POINT('Ctrl Pts',(1.67119768818825,27.7854193222409,12.3888748756123));
#61484=CARTESIAN_POINT('Ctrl Pts',(1.69193772409766,27.7906548098266,12.4262391440704));
#61485=CARTESIAN_POINT('Ctrl Pts',(1.71138267339757,27.7958536280428,12.4643344982101));
#61486=CARTESIAN_POINT('Ctrl Pts',(1.72950947559644,27.8010521028769,12.5030547640794));
#61487=CARTESIAN_POINT('Ctrl Pts',(1.72951799205781,27.8010545452609,12.5030729559063));
#61488=CARTESIAN_POINT('Ctrl Pts',(1.72952650822833,27.8010569876447,12.5030911478714));
#61489=CARTESIAN_POINT('Ctrl Pts',(1.729535024108,27.8010594300285,12.5031093399746));
#61490=CARTESIAN_POINT('Ctrl Pts',(1.75621161116458,27.8087103677144,12.5600973721866));
#61491=CARTESIAN_POINT('Ctrl Pts',(1.77999496964844,27.8163359500152,12.6184065650703));
#61492=CARTESIAN_POINT('Ctrl Pts',(1.80095447272991,27.8240478620407,12.6777061742592));
#61493=CARTESIAN_POINT('Ctrl Pts',(1.80661497184171,27.8261306056535,12.6937211238426));
#61494=CARTESIAN_POINT('Ctrl Pts',(1.81206954810936,27.8282196798225,12.7098086011334));
#61495=CARTESIAN_POINT('Ctrl Pts',(1.81731962540062,27.8303173594206,12.7259627345639));
#61496=CARTESIAN_POINT('Ctrl Pts',(1.84046907600862,27.839566771868,12.7971920314329));
#61497=CARTESIAN_POINT('Ctrl Pts',(1.85956826403524,27.8489060776057,12.8697755299982));
#61498=CARTESIAN_POINT('Ctrl Pts',(1.87443315079832,27.8582628805153,12.943311013621));
#61499=CARTESIAN_POINT('Ctrl Pts',(1.87540869087311,27.858876940774,12.9481369374464));
#61500=CARTESIAN_POINT('Ctrl Pts',(1.87636598086617,27.8594910744935,12.9529669484949));
#61501=CARTESIAN_POINT('Ctrl Pts',(1.87730496335598,27.8601052604144,12.9578009274768));
#61502=CARTESIAN_POINT('Ctrl Pts',(1.89250598473335,27.8700482076086,13.0360573578578));
#61503=CARTESIAN_POINT('Ctrl Pts',(1.90290822949596,27.8800048478456,13.1153542584566));
#61504=CARTESIAN_POINT('Ctrl Pts',(1.90835950198352,27.8899729257711,13.1950670158045));
#61505=CARTESIAN_POINT('Ctrl Pts',(1.91108513822731,27.8949569647339,13.2349233944784));
#61506=CARTESIAN_POINT('Ctrl Pts',(1.91257301511765,27.8999438549339,13.2748835851175));
#61507=CARTESIAN_POINT('Ctrl Pts',(1.91280547596267,27.9049323592216,13.3148614673998));
#61508=CARTESIAN_POINT('Ctrl Pts',(1.91295913350828,27.9082297804497,13.3412870070188));
#61509=CARTESIAN_POINT('Ctrl Pts',(1.91256431850402,27.9115279068385,13.3677202694795));
#61510=CARTESIAN_POINT('Ctrl Pts',(1.91161655319156,27.9148263801428,13.3941363756395));
#61511=CARTESIAN_POINT('Ctrl Pts',(1.91113049158358,27.9165180027598,13.4076838803519));
#61512=CARTESIAN_POINT('Ctrl Pts',(1.91049900939872,27.918209704164,13.4212267734741));
#61513=CARTESIAN_POINT('Ctrl Pts',(1.90972153695773,27.9199014734697,13.4347620038057));
#61514=CARTESIAN_POINT('Ctrl Pts',(1.90534923235206,27.9294155479715,13.5108806503292));
#61515=CARTESIAN_POINT('Ctrl Pts',(1.89634539771753,27.9389515961825,13.5869155167899));
#61516=CARTESIAN_POINT('Ctrl Pts',(1.88285252040647,27.9484938268728,13.6622095436909));
#61517=CARTESIAN_POINT('Ctrl Pts',(1.86935964309542,27.958036057563,13.7375035705918));
#61518=CARTESIAN_POINT('Ctrl Pts',(1.85138106885504,27.967584453052,13.8120563319306));
#61519=CARTESIAN_POINT('Ctrl Pts',(1.82908775889807,27.977133039192,13.8852948652974));
#61520=CARTESIAN_POINT('Ctrl Pts',(1.80844629276644,27.985974113837,13.9531067204656));
#61521=CARTESIAN_POINT('Ctrl Pts',(1.7842640395328,27.9949641707816,14.0197929648663));
#61522=CARTESIAN_POINT('Ctrl Pts',(1.75653947367986,28.0039968977633,14.0849877155301));
#61523=CARTESIAN_POINT('Ctrl Pts',(1.75454192988809,28.0046477021005,14.0896849710304));
#61524=CARTESIAN_POINT('Ctrl Pts',(1.75252599432901,28.0052987252934,14.0943744619669));
#61525=CARTESIAN_POINT('Ctrl Pts',(1.75049166532415,28.0059499263501,14.0990560412568));
#61526=CARTESIAN_POINT('Ctrl Pts',(1.72659336103571,28.0135999185435,14.1540529498948));
#61527=CARTESIAN_POINT('Ctrl Pts',(1.70009385182191,28.0212128584894,14.2079551069128));
#61528=CARTESIAN_POINT('Ctrl Pts',(1.67102796759327,28.0287744333106,14.2605321315749));
#61529=CARTESIAN_POINT('Ctrl Pts',(1.65532057049091,28.0328607586225,14.288945105298));
#61530=CARTESIAN_POINT('Ctrl Pts',(1.63886325653744,28.0369324130974,14.3169714922753));
#61531=CARTESIAN_POINT('Ctrl Pts',(1.62168131926052,28.0410046404417,14.3445726722918));
#61532=CARTESIAN_POINT('Ctrl Pts',(1.62166911426219,28.0410075331031,14.3445922784835));
#61533=CARTESIAN_POINT('Ctrl Pts',(1.62165690889821,28.0410104257649,14.3446118844608));
#61534=CARTESIAN_POINT('Ctrl Pts',(1.62164470316857,28.041013318427,14.3446314902236));
#61535=CARTESIAN_POINT('Ctrl Pts',(1.57267741401981,28.0526181814509,14.4232864403415));
#61536=CARTESIAN_POINT('Ctrl Pts',(1.51781046943814,28.0641401287839,14.4983839269083));
#61537=CARTESIAN_POINT('Ctrl Pts',(1.45777148584965,28.0756435782486,14.5692788341777));
#61538=CARTESIAN_POINT('Ctrl Pts',(1.39615710929978,28.0874488724854,14.6420339884272));
#61539=CARTESIAN_POINT('Ctrl Pts',(1.32909482450444,28.0992349137366,14.7103624156715));
#61540=CARTESIAN_POINT('Ctrl Pts',(1.25735647030735,28.1110433153804,14.7735405036232));
#61541=CARTESIAN_POINT('Ctrl Pts',(1.18543183367424,28.1228823798105,14.836882645633));
#61542=CARTESIAN_POINT('Ctrl Pts',(1.10880657100335,28.1347440652443,14.8950469721656));
#61543=CARTESIAN_POINT('Ctrl Pts',(1.02825283032043,28.1466399321335,14.9472888127912));
#61544=CARTESIAN_POINT('Ctrl Pts',(1.01730894768943,28.1482560826676,14.9543862929006));
#61545=CARTESIAN_POINT('Ctrl Pts',(1.0062925477142,28.1498728163086,14.9613744448076));
#61546=CARTESIAN_POINT('Ctrl Pts',(0.995205558188219,28.1514901164888,14.9682513895842));
#61547=CARTESIAN_POINT('Ctrl Pts',(0.972475805446326,28.1548057896136,14.9823500097756));
#61548=CARTESIAN_POINT('Ctrl Pts',(0.949449322592214,28.1581238419525,14.9959812758543));
#61549=CARTESIAN_POINT('Ctrl Pts',(0.926143163075408,28.1614500362462,15.0091338425473));
#61550=CARTESIAN_POINT('Ctrl Pts',(0.926131693837206,28.1614516731059,15.0091403150817));
#61551=CARTESIAN_POINT('Ctrl Pts',(0.926120224530382,28.1614533099669,15.0091467874999));
#61552=CARTESIAN_POINT('Ctrl Pts',(0.926108755154938,28.161454946829,15.0091532598019));
#61553=CARTESIAN_POINT('Ctrl Pts',(0.837659685175365,28.1740780344321,15.0590660989367));
#61554=CARTESIAN_POINT('Ctrl Pts',(0.745127032716431,28.186771118259,15.1020652714529));
#61555=CARTESIAN_POINT('Ctrl Pts',(0.649704821666005,28.1994902401537,15.1377317143075));
#61556=CARTESIAN_POINT('Ctrl Pts',(0.553321727077857,28.2123374411895,15.1737573114659));
#61557=CARTESIAN_POINT('Ctrl Pts',(0.453993920957942,28.225215802371,15.2023068048996));
#61558=CARTESIAN_POINT('Ctrl Pts',(0.352925350219839,28.2380928432519,15.2229791730088));
#61559=CARTESIAN_POINT('Ctrl Pts',(0.254602793423587,28.2506200173688,15.2430898767882));
#61560=CARTESIAN_POINT('Ctrl Pts',(0.154632426084098,28.2631457303804,15.2557469701838));
#61561=CARTESIAN_POINT('Ctrl Pts',(0.0541040691992433,28.2756669717454,
15.2605928269564));
#61562=CARTESIAN_POINT('Ctrl Pts',(0.0327897991787413,28.2783217562034,
15.2616202574539));
#61563=CARTESIAN_POINT('Ctrl Pts',(0.0114516579271045,28.2809803578895,
15.2622993252151));
#61564=CARTESIAN_POINT('Ctrl Pts',(-0.00989862692612825,28.2836444589833,
15.2626278963491));
#61565=CARTESIAN_POINT('Ctrl Pts',(-0.00991502536138304,28.2836465051897,
15.2626281487136));
#61566=CARTESIAN_POINT('Ctrl Pts',(-0.00993142380461405,28.2836485513966,
15.2626284008693));
#61567=CARTESIAN_POINT('Ctrl Pts',(-0.00994782225579749,28.2836505976039,
15.2626286528162));
#61568=CARTESIAN_POINT('Ctrl Pts',(-0.0919646539396332,28.2938847010688,
15.263888765243));
#61569=CARTESIAN_POINT('Ctrl Pts',(-0.174180657339046,28.3041311546817,
15.2599274400423));
#61570=CARTESIAN_POINT('Ctrl Pts',(-0.255920339664015,28.3143906605047,
15.2508700293366));
#61571=CARTESIAN_POINT('Ctrl Pts',(-0.33765847038126,28.3246499715787,15.2418127905616));
#61572=CARTESIAN_POINT('Ctrl Pts',(-0.418920429682987,28.3349223484336,
15.2276597501592));
#61573=CARTESIAN_POINT('Ctrl Pts',(-0.499103565974076,28.3452080191226,
15.2084815967412));
#61574=CARTESIAN_POINT('Ctrl Pts',(-0.600206827742772,28.3581772655781,
15.184299780527));
#61575=CARTESIAN_POINT('Ctrl Pts',(-0.699603445862627,28.3711687987847,
15.1521250292407));
#61576=CARTESIAN_POINT('Ctrl Pts',(-0.795994742605581,28.3841800605095,
15.1122879210286));
#61577=CARTESIAN_POINT('Ctrl Pts',(-0.852489506494473,28.3918059373664,
15.0889394642851));
#61578=CARTESIAN_POINT('Ctrl Pts',(-0.907953474039107,28.3994387680334,
15.0629590072487));
#61579=CARTESIAN_POINT('Ctrl Pts',(-0.962136588998806,28.407079578439,15.0344083837009));
#61580=CARTESIAN_POINT('Ctrl Pts',(-1.12646005194889,28.4302521927586,14.9478216798126));
#61581=CARTESIAN_POINT('Ctrl Pts',(-1.27897078824977,28.4534938027453,14.8376104886566));
#61582=CARTESIAN_POINT('Ctrl Pts',(-1.41393887862166,28.4768086286541,14.7083454242204));
#61583=CARTESIAN_POINT('Ctrl Pts',(-1.50240492763019,28.4920905410364,14.6236174748659));
#61584=CARTESIAN_POINT('Ctrl Pts',(-1.58333431865573,28.5074039430096,14.5307032225104));
#61585=CARTESIAN_POINT('Ctrl Pts',(-1.65511262555103,28.5227498647524,14.4308907336903));
#61586=CARTESIAN_POINT('Ctrl Pts',(-1.66926241111438,28.5257750336554,14.4112145198809));
#61587=CARTESIAN_POINT('Ctrl Pts',(-1.68305657838302,28.5288014662315,14.3912702361043));
#61588=CARTESIAN_POINT('Ctrl Pts',(-1.69648276036997,28.5318291698286,14.3710677556957));
#61589=CARTESIAN_POINT('Ctrl Pts',(-1.77787575643723,28.5501838939946,14.2485950817777));
#61590=CARTESIAN_POINT('Ctrl Pts',(-1.84575323579243,28.5685876070242,14.1166170873232));
#61591=CARTESIAN_POINT('Ctrl Pts',(-1.89879251057137,28.587038324042,13.9785079438035));
#61592=CARTESIAN_POINT('Ctrl Pts',(-1.95222788591733,28.6056268321495,13.8393673927035));
#61593=CARTESIAN_POINT('Ctrl Pts',(-1.99060677787332,28.6242664220067,13.6940061019775));
#61594=CARTESIAN_POINT('Ctrl Pts',(-2.01260790568954,28.6429812057999,13.5458408356626));
#61595=CARTESIAN_POINT('Ctrl Pts',(-2.0180160388561,28.647581517374,13.5094200895271));
#61596=CARTESIAN_POINT('Ctrl Pts',(-2.02243389469254,28.6521848475788,13.4728291848583));
#61597=CARTESIAN_POINT('Ctrl Pts',(-2.02584159212891,28.6567913464262,13.4361185882898));
#61598=CARTESIAN_POINT('Ctrl Pts',(-2.02615949296527,28.6572210823002,13.4326938918282));
#61599=CARTESIAN_POINT('Ctrl Pts',(-2.02646860250647,28.6576508458103,13.4292681536581));
#61600=CARTESIAN_POINT('Ctrl Pts',(-2.02676890775793,28.6580806444262,13.4258414188437));
#61601=CARTESIAN_POINT('Ctrl Pts',(-2.02677007512464,28.6580823151682,13.4258280982103));
#61602=CARTESIAN_POINT('Ctrl Pts',(-2.02677124235842,28.658083985911,13.4258147775617));
#61603=CARTESIAN_POINT('Ctrl Pts',(-2.02677240945925,28.6580856566545,13.425801456898));
#61604=CARTESIAN_POINT('Ctrl Pts',(-2.0405316559978,28.677782473794,13.2687607875455));
#61605=CARTESIAN_POINT('Ctrl Pts',(-2.03580963395929,28.6975830887113,13.1096130060237));
#61606=CARTESIAN_POINT('Ctrl Pts',(-2.01300737612442,28.7174335268602,12.9526738600431));
#61607=CARTESIAN_POINT('Ctrl Pts',(-1.98997249743873,28.7374864724032,12.7941336744667));
#61608=CARTESIAN_POINT('Ctrl Pts',(-1.94849435885256,28.7575884801872,12.6378473421967));
#61609=CARTESIAN_POINT('Ctrl Pts',(-1.8889688971964,28.7776882004441,12.488165435839));
#61610=CARTESIAN_POINT('Ctrl Pts',(-1.88062290443526,28.7805063578359,12.4671787173462));
#61611=CARTESIAN_POINT('Ctrl Pts',(-1.87192198593172,28.7833245038566,12.446321690604));
#61612=CARTESIAN_POINT('Ctrl Pts',(-1.86286706311752,28.7861425377394,12.4256062236929));
#61613=CARTESIAN_POINT('Ctrl Pts',(-1.86286080290841,28.7861444860145,12.425591901853));
#61614=CARTESIAN_POINT('Ctrl Pts',(-1.86285454253086,28.7861464342897,12.4255775800823));
#61615=CARTESIAN_POINT('Ctrl Pts',(-1.86284828198488,28.7861483825649,12.4255632583808));
#61616=CARTESIAN_POINT('Ctrl Pts',(-1.86181575438794,28.786469704041,12.4232012356302));
#61617=CARTESIAN_POINT('Ctrl Pts',(-1.86077864520166,28.7867910253279,12.4208410947962));
#61618=CARTESIAN_POINT('Ctrl Pts',(-1.8597369631722,28.7871123432515,12.4184828489633));
#61619=CARTESIAN_POINT('Ctrl Pts',(-1.81231342527778,28.8017406389244,12.3111215261644));
#61620=CARTESIAN_POINT('Ctrl Pts',(-1.75541341869991,28.8163628134929,12.2076790811907));
#61621=CARTESIAN_POINT('Ctrl Pts',(-1.69002467064595,28.831029030168,12.1094970535507));
#61622=CARTESIAN_POINT('Ctrl Pts',(-1.62433393102225,28.8457629813377,12.0108615817705));
#61623=CARTESIAN_POINT('Ctrl Pts',(-1.55007153298118,28.8605420587782,11.9175376889213));
#61624=CARTESIAN_POINT('Ctrl Pts',(-1.46826629077973,28.8754003434675,11.8309726423896));
#61625=CARTESIAN_POINT('Ctrl Pts',(-1.39497406680941,28.8887124088064,11.7534159405492));
#61626=CARTESIAN_POINT('Ctrl Pts',(-1.31562661124625,28.9020881303713,11.6812880245723));
#61627=CARTESIAN_POINT('Ctrl Pts',(-1.23101598506768,28.9155342832238,11.61565552247));
#61628=CARTESIAN_POINT('Ctrl Pts',(-1.23099796339198,28.9155371471927,11.6156415430478));
#61629=CARTESIAN_POINT('Ctrl Pts',(-1.23097994147602,28.9155400111662,11.6156275639185));
#61630=CARTESIAN_POINT('Ctrl Pts',(-1.23096191931979,28.9155428751441,11.6156135850821));
#61631=CARTESIAN_POINT('Ctrl Pts',(-1.14884577065289,28.9285923035583,11.5519204181195));
#61632=CARTESIAN_POINT('Ctrl Pts',(-1.06173893290582,28.9417352560574,11.4943088010887));
#61633=CARTESIAN_POINT('Ctrl Pts',(-0.970673823222862,28.9548248633794,
11.4433545033137));
#61634=CARTESIAN_POINT('Ctrl Pts',(-0.950609266581978,28.9577089225809,
11.4321276415951));
#61635=CARTESIAN_POINT('Ctrl Pts',(-0.9303517397105,28.9605905530007,11.4212233990956));
#61636=CARTESIAN_POINT('Ctrl Pts',(-0.90991081640154,28.9634684850355,11.4106471890954));
#61637=CARTESIAN_POINT('Ctrl Pts',(-0.818131349886293,28.9763903605709,
11.3631601506239));
#61638=CARTESIAN_POINT('Ctrl Pts',(-0.722640356060095,28.9892385982485,
11.322277457506));
#61639=CARTESIAN_POINT('Ctrl Pts',(-0.624423301925256,29.0021044649047,
11.2885101519301));
#61640=CARTESIAN_POINT('Ctrl Pts',(-0.539660016265759,29.0132079656179,
11.2593682906343));
#61641=CARTESIAN_POINT('Ctrl Pts',(-0.452864400020062,29.0243256761542,
11.2355310152117));
#61642=CARTESIAN_POINT('Ctrl Pts',(-0.364792165622707,29.0355025217288,
11.2173494433471));
#61643=CARTESIAN_POINT('Ctrl Pts',(-0.350519914334075,29.0373137480449,
11.2144030895472));
#61644=CARTESIAN_POINT('Ctrl Pts',(-0.336214152551724,29.0391265288975,
11.2116051485266));
#61645=CARTESIAN_POINT('Ctrl Pts',(-0.321878107417712,29.0409410572737,
11.2089569848025));
#61646=CARTESIAN_POINT('Ctrl Pts',(-0.306478186558829,29.0428902415243,
11.2061123012519));
#61647=CARTESIAN_POINT('Ctrl Pts',(-0.291043687766917,29.0448413775742,
11.2034405256956));
#61648=CARTESIAN_POINT('Ctrl Pts',(-0.275579005610156,29.0467946305441,
11.2009433363203));
#61649=CARTESIAN_POINT('Ctrl Pts',(-0.275570523676965,29.0467957018472,
11.2009419666838));
#61650=CARTESIAN_POINT('Ctrl Pts',(-0.275562041733366,29.0467967731509,
11.2009405970996));
#61651=CARTESIAN_POINT('Ctrl Pts',(-0.27555355977936,29.0467978444553,11.2009392275678));
#61652=CARTESIAN_POINT('Ctrl Pts',(-0.174162714297345,29.0596039102395,
11.1845682365639));
#61653=CARTESIAN_POINT('Ctrl Pts',(-0.0712833547055921,29.0725078447394,
11.1756792523032));
#61654=CARTESIAN_POINT('Ctrl Pts',(0.0319050888017752,29.0854479062699,
11.1742525038087));
#61655=CARTESIAN_POINT('Ctrl Pts',(0.0563634941319289,29.0885150449838,
11.1739143264722));
#61656=CARTESIAN_POINT('Ctrl Pts',(0.0808392051649467,29.0915842082012,
11.1739951662006));
#61657=CARTESIAN_POINT('Ctrl Pts',(0.105316439168227,29.0946545643595,11.1744943403296));
#61658=CARTESIAN_POINT('Ctrl Pts',(0.215803238224659,29.1085137211518,11.1767475422921));
#61659=CARTESIAN_POINT('Ctrl Pts',(0.326326071542987,29.1223966823686,11.187520012059));
#61660=CARTESIAN_POINT('Ctrl Pts',(0.4356269082667,29.1362579642596,11.2067721272977));
#61661=CARTESIAN_POINT('Ctrl Pts',(0.44531767414695,29.1374869250034,11.2084790469067));
#61662=CARTESIAN_POINT('Ctrl Pts',(0.454998828002351,29.1387157148839,11.2102526570044));
#61663=CARTESIAN_POINT('Ctrl Pts',(0.464669488559821,29.1399443019515,11.2120929492527));
#61664=CARTESIAN_POINT('Ctrl Pts',(0.472045000348972,29.1408813070657,11.2134964828678));
#61665=CARTESIAN_POINT('Ctrl Pts',(0.479414478883609,29.1418182095507,11.2149388151259));
#61666=CARTESIAN_POINT('Ctrl Pts',(0.486777559710844,29.1427550015008,11.2164199509909));
#61667=CARTESIAN_POINT('Ctrl Pts',(0.584925682586,29.1552422162397,11.2361631411435));
#61668=CARTESIAN_POINT('Ctrl Pts',(0.681953371103919,29.1677125483654,11.2628089358605));
#61669=CARTESIAN_POINT('Ctrl Pts',(0.776769474478284,29.18024255482,11.2962806128029));
#61670=CARTESIAN_POINT('Ctrl Pts',(0.776795505175567,29.1802459947927,11.2962898020762));
#61671=CARTESIAN_POINT('Ctrl Pts',(0.776821535712201,29.18024943477,11.2962989918659));
#61672=CARTESIAN_POINT('Ctrl Pts',(0.776847566088163,29.1802528747521,11.2963081821719));
#61673=CARTESIAN_POINT('Ctrl Pts',(0.880974325285057,29.1940134976104,11.3330712617267));
#61674=CARTESIAN_POINT('Ctrl Pts',(0.982528966870906,29.2078494488345,11.3781009897652));
#61675=CARTESIAN_POINT('Ctrl Pts',(1.08027920797818,29.221732415313,11.4307123916727));
#61676=CARTESIAN_POINT('Ctrl Pts',(1.10566362016273,29.2253376334633,11.444374859371));
#61677=CARTESIAN_POINT('Ctrl Pts',(1.13079156032285,29.2289460195216,11.4585483521387));
#61678=CARTESIAN_POINT('Ctrl Pts',(1.15564167179722,29.2325570721909,11.4732203485793));
#61679=CARTESIAN_POINT('Ctrl Pts',(1.26785552218459,29.248863241457,11.5394736213333));
#61680=CARTESIAN_POINT('Ctrl Pts',(1.37440664919206,29.2652229399408,11.6158899316168));
#61681=CARTESIAN_POINT('Ctrl Pts',(1.47348562479979,29.2816050850296,11.7014171741355));
#61682=CARTESIAN_POINT('Ctrl Pts',(1.54227988610125,29.2929798248571,11.7608019571748));
#61683=CARTESIAN_POINT('Ctrl Pts',(1.60747602190586,29.3043656634369,11.8245805288282));
#61684=CARTESIAN_POINT('Ctrl Pts',(1.6684943777618,29.3157601683119,11.8924550823692));
#61685=CARTESIAN_POINT('Ctrl Pts',(1.66853645781051,29.3157680262969,11.892501890653));
#61686=CARTESIAN_POINT('Ctrl Pts',(1.66857853581567,29.3157758843017,11.8925487008194));
#61687=CARTESIAN_POINT('Ctrl Pts',(1.66862061177711,29.3157837423264,11.8925955128682));
#61688=CARTESIAN_POINT('Ctrl Pts',(1.68689026181752,29.3191957466442,11.9129216021676));
#61689=CARTESIAN_POINT('Ctrl Pts',(1.70477463383708,29.3226115033997,11.9336025645071));
#61690=CARTESIAN_POINT('Ctrl Pts',(1.7222669118597,29.3260292758585,11.9546242986192));
#61691=CARTESIAN_POINT('Ctrl Pts',(1.77994411232085,29.3372986798196,12.023939156916));
#61692=CARTESIAN_POINT('Ctrl Pts',(1.83336850913228,29.3485911700184,12.0969651193588));
#61693=CARTESIAN_POINT('Ctrl Pts',(1.88224583463627,29.3599118637564,12.1731883821223));
#61694=CARTESIAN_POINT('Ctrl Pts',(1.88636797421079,29.3608666107519,12.1796167806629));
#61695=CARTESIAN_POINT('Ctrl Pts',(1.89045774741834,29.3618215584311,12.1860679385147));
#61696=CARTESIAN_POINT('Ctrl Pts',(1.8945149637451,29.3627767099103,12.1925415568821));
#61697=CARTESIAN_POINT('Ctrl Pts',(1.94704272883048,29.3751428172315,12.2763538748526));
#61698=CARTESIAN_POINT('Ctrl Pts',(1.99411367278242,29.3875433734691,12.363931434955));
#61699=CARTESIAN_POINT('Ctrl Pts',(2.03523714538344,29.3999686153529,12.4545081593452));
#61700=CARTESIAN_POINT('Ctrl Pts',(2.07322751764787,29.4114472073779,12.5381840568421));
#61701=CARTESIAN_POINT('Ctrl Pts',(2.10613781564245,29.4229469985678,12.624420666633));
#61702=CARTESIAN_POINT('Ctrl Pts',(2.13355885314394,29.4344446947496,12.7125039212252));
#61703=CARTESIAN_POINT('Ctrl Pts',(2.13583932206719,29.4354008999563,12.7198293597592));
#61704=CARTESIAN_POINT('Ctrl Pts',(2.13808185278511,29.436357090538,12.7271675592712));
#61705=CARTESIAN_POINT('Ctrl Pts',(2.14028622537885,29.4373132530233,12.7345181035168));
#61706=CARTESIAN_POINT('Ctrl Pts',(2.15252451656922,29.4426216999495,12.7753270398734));
#61707=CARTESIAN_POINT('Ctrl Pts',(2.16358586192327,29.4479290261542,12.8165149793703));
#61708=CARTESIAN_POINT('Ctrl Pts',(2.17343309975439,29.4532317761385,12.8580033371832));
#61709=CARTESIAN_POINT('Ctrl Pts',(2.17343821350038,29.4532345298972,12.858024882405));
#61710=CARTESIAN_POINT('Ctrl Pts',(2.17344332691904,29.4532372836546,12.8580464277078));
#61711=CARTESIAN_POINT('Ctrl Pts',(2.17344844001037,29.4532400374108,12.8580679730916));
#61712=CARTESIAN_POINT('Ctrl Pts',(2.19411109386932,29.4643683172111,12.9451356155083));
#61713=CARTESIAN_POINT('Ctrl Pts',(2.20947493606372,29.475510217651,13.0337400666774));
#61714=CARTESIAN_POINT('Ctrl Pts',(2.21947125049892,29.4866669450407,13.1231108473052));
#61715=CARTESIAN_POINT('Ctrl Pts',(2.22148929070966,29.4889192475907,13.1411528797103));
#61716=CARTESIAN_POINT('Ctrl Pts',(2.22328874345907,29.4911721539522,13.1592261051922));
#61717=CARTESIAN_POINT('Ctrl Pts',(2.22486929541162,29.4934256733204,13.1773241399873));
#61718=CARTESIAN_POINT('Ctrl Pts',(2.23428776598476,29.5068543403262,13.2851698883503));
#61719=CARTESIAN_POINT('Ctrl Pts',(2.23593228547602,29.5203046621321,13.3938963078404));
#61720=CARTESIAN_POINT('Ctrl Pts',(2.22976674229424,29.5338006156728,13.5023174068447));
#61721=CARTESIAN_POINT('Ctrl Pts',(2.22414927678059,29.5460968645763,13.6011005580855));
#61722=CARTESIAN_POINT('Ctrl Pts',(2.21205384164696,29.5584310899797,13.6996317595469));
#61723=CARTESIAN_POINT('Ctrl Pts',(2.19342580677518,29.5708383222901,13.7971348227835));
#61724=CARTESIAN_POINT('Ctrl Pts',(2.19206135353893,29.5717471185424,13.80427665879));
#61725=CARTESIAN_POINT('Ctrl Pts',(2.19066182866396,29.572656306571,13.8114129765725));
#61726=CARTESIAN_POINT('Ctrl Pts',(2.18922719967663,29.5735659001798,13.8185434696397));
#61727=CARTESIAN_POINT('Ctrl Pts',(2.179380513441,29.5798089657715,13.8674841564362));
#61728=CARTESIAN_POINT('Ctrl Pts',(2.16788022758423,29.586071426847,13.9161525834398));
#61729=CARTESIAN_POINT('Ctrl Pts',(2.15471003642721,29.5923592074735,13.964458986641));
#61730=CARTESIAN_POINT('Ctrl Pts',(2.15468671042886,29.592370343892,13.9645445431123));
#61731=CARTESIAN_POINT('Ctrl Pts',(2.15466337925621,29.5923814803489,13.9646300982071));
#61732=CARTESIAN_POINT('Ctrl Pts',(2.15464004290921,29.5923926168443,13.964715651925));
#61733=CARTESIAN_POINT('Ctrl Pts',(2.14403590146766,29.5974530906289,14.0035916476497));
#61734=CARTESIAN_POINT('Ctrl Pts',(2.13236371009766,29.6025215008339,14.0421834073582));
#61735=CARTESIAN_POINT('Ctrl Pts',(2.11964678076267,29.6075987803237,14.0804583158383));
#61736=CARTESIAN_POINT('Ctrl Pts',(2.08780168468648,29.6203130487528,14.1763044203301));
#61737=CARTESIAN_POINT('Ctrl Pts',(2.04939393621146,29.6330888116124,14.2702042051983));
#61738=CARTESIAN_POINT('Ctrl Pts',(2.00478346581371,29.6459139074135,14.3614182861861));
#61739=CARTESIAN_POINT('Ctrl Pts',(1.97944178986073,29.6531994038218,14.413233872575));
#61740=CARTESIAN_POINT('Ctrl Pts',(1.95209761230748,29.6605008231038,14.4641824559238));
#61741=CARTESIAN_POINT('Ctrl Pts',(1.92281048669964,29.6678159670389,14.5141246144164));
#61742=CARTESIAN_POINT('Ctrl Pts',(1.87765301719436,29.6790951001842,14.5911298326601));
#61743=CARTESIAN_POINT('Ctrl Pts',(1.82787363930548,29.6904059116434,14.6657363662634));
#61744=CARTESIAN_POINT('Ctrl Pts',(1.7737969730373,29.7017162772042,14.7372854931457));
#61745=CARTESIAN_POINT('Ctrl Pts',(1.73439595654646,29.7099571679753,14.7894171891755));
#61746=CARTESIAN_POINT('Ctrl Pts',(1.69271464849936,29.7181978182467,14.8399260823175));
#61747=CARTESIAN_POINT('Ctrl Pts',(1.64889283119282,29.7264257544821,14.8885675303056));
#61748=CARTESIAN_POINT('Ctrl Pts',(1.63254870314928,29.7294945099932,14.9067092255388));
#61749=CARTESIAN_POINT('Ctrl Pts',(1.61590806306995,29.7325612921836,14.9245899635758));
#61750=CARTESIAN_POINT('Ctrl Pts',(1.59898001760933,29.7356252411689,14.9421962435881));
#61751=CARTESIAN_POINT('Ctrl Pts',(1.59893601614321,29.7356332053634,14.9422420080052));
#61752=CARTESIAN_POINT('Ctrl Pts',(1.59889201273545,29.7356411695389,14.9422877705682));
#61753=CARTESIAN_POINT('Ctrl Pts',(1.59884800738628,29.7356491336951,14.9423335312769));
#61754=CARTESIAN_POINT('Ctrl Pts',(1.53854824913323,29.7465622773449,15.0050386278986));
#61755=CARTESIAN_POINT('Ctrl Pts',(1.47443051445554,29.7573805351958,15.0644453439063));
#61756=CARTESIAN_POINT('Ctrl Pts',(1.40702016816517,29.7681437325686,15.1201383185971));
#61757=CARTESIAN_POINT('Ctrl Pts',(1.33888074946686,29.7790233386331,15.1764336371919));
#61758=CARTESIAN_POINT('Ctrl Pts',(1.2673791377501,29.7898466507777,15.2289354518161));
#61759=CARTESIAN_POINT('Ctrl Pts',(1.19303629151063,29.8006646111447,15.2772718656253));
#61760=CARTESIAN_POINT('Ctrl Pts',(1.11892238419049,29.8114492575847,15.3254594273673));
#61761=CARTESIAN_POINT('Ctrl Pts',(1.04198600371556,29.8222286282337,15.36950892309));
#61762=CARTESIAN_POINT('Ctrl Pts',(0.962697131488878,29.8330627782369,15.4090874366371));
#61763=CARTESIAN_POINT('Ctrl Pts',(0.885176571317848,29.843655303438,15.4477832643711));
#61764=CARTESIAN_POINT('Ctrl Pts',(0.805407622756845,29.8543003069106,15.4822072937904));
#61765=CARTESIAN_POINT('Ctrl Pts',(0.723775978306456,29.8650757003008,15.512051919412));
#61766=CARTESIAN_POINT('Ctrl Pts',(0.69185218421878,29.8692896475037,15.5237232962338));
#61767=CARTESIAN_POINT('Ctrl Pts',(0.65964519270811,29.873535660542,15.5346917884168));
#61768=CARTESIAN_POINT('Ctrl Pts',(0.627169428730706,29.8777866196656,15.5449446896347));
#61769=CARTESIAN_POINT('Ctrl Pts',(0.627104324720616,29.8777951415432,15.5449652435772));
#61770=CARTESIAN_POINT('Ctrl Pts',(0.627039219745971,29.8778036634256,15.5449857946067));
#61771=CARTESIAN_POINT('Ctrl Pts',(0.626974113806956,29.8778121853127,15.5450063427231));
#61772=CARTESIAN_POINT('Ctrl Pts',(0.573993027685789,29.8847470186868,15.5617277285364));
#61773=CARTESIAN_POINT('Ctrl Pts',(0.520373373533641,29.8916850888289,15.5765205850681));
#61774=CARTESIAN_POINT('Ctrl Pts',(0.46624416580409,29.8986948306155,15.5893696321012));
#61775=CARTESIAN_POINT('Ctrl Pts',(0.373543369291603,29.9106995998375,15.6113747000555));
#61776=CARTESIAN_POINT('Ctrl Pts',(0.279317216943743,29.922860064562,15.6276972133245));
#61777=CARTESIAN_POINT('Ctrl Pts',(0.184173410113904,29.9351243913809,15.6382729149402));
#61778=CARTESIAN_POINT('Ctrl Pts',(0.172193152097602,29.9366686831702,15.6396045794834));
#61779=CARTESIAN_POINT('Ctrl Pts',(0.160198331622726,29.938214622535,15.640845060734));
#61780=CARTESIAN_POINT('Ctrl Pts',(0.148190153236795,29.9397621067286,15.6419941724037));
#61781=CARTESIAN_POINT('Ctrl Pts',(0.0353352487810282,29.9543056265862,
15.6527937194724));
#61782=CARTESIAN_POINT('Ctrl Pts',(-0.0787020464481159,29.9689850838153,
15.6555199105086));
#61783=CARTESIAN_POINT('Ctrl Pts',(-0.192666393973396,29.9836868481843,
15.650006965307));
#61784=CARTESIAN_POINT('Ctrl Pts',(-0.275518477501743,29.9943750312519,
15.6459990540062));
#61785=CARTESIAN_POINT('Ctrl Pts',(-0.358329908898737,30.005074367007,15.6376341430243));
#61786=CARTESIAN_POINT('Ctrl Pts',(-0.440525514520615,30.0157305485564,
15.6248862161416));
#61787=CARTESIAN_POINT('Ctrl Pts',(-0.464990701058588,30.0189023175022,
15.6210918477347));
#61788=CARTESIAN_POINT('Ctrl Pts',(-0.48940139016687,30.0220702645024,15.6169095178364));
#61789=CARTESIAN_POINT('Ctrl Pts',(-0.513742625389251,30.0252329608739,
15.6123394160239));
#61790=CARTESIAN_POINT('Ctrl Pts',(-0.519998017753285,30.0260457342007,
15.6111649571388));
#61791=CARTESIAN_POINT('Ctrl Pts',(-0.526248767278081,30.0268581564716,
15.6099649008537));
#61792=CARTESIAN_POINT('Ctrl Pts',(-0.532494600244034,30.0276702019342,
15.6087392602533));
#61793=CARTESIAN_POINT('Ctrl Pts',(-0.532607167216087,30.0276848372118,
15.6087171708616));
#61794=CARTESIAN_POINT('Ctrl Pts',(-0.532719732591162,30.0276994723669,
15.6086950731596));
#61795=CARTESIAN_POINT('Ctrl Pts',(-0.532832296367725,30.0277141073995,
15.6086729671481));
#61796=CARTESIAN_POINT('Ctrl Pts',(-0.629575186013529,30.0402921799077,
15.5896739650215));
#61797=CARTESIAN_POINT('Ctrl Pts',(-0.725421815311289,30.0527048234065,
15.564499656116));
#61798=CARTESIAN_POINT('Ctrl Pts',(-0.819553158172979,30.0650012028476,
15.533430181105));
#61799=CARTESIAN_POINT('Ctrl Pts',(-0.912430194723611,30.0771337322269,
15.5027747088842));
#61800=CARTESIAN_POINT('Ctrl Pts',(-1.00363754468808,30.0891532520328,15.4663824189752));
#61801=CARTESIAN_POINT('Ctrl Pts',(-1.09244306912936,30.101118142086,15.4245300478977));
#61802=CARTESIAN_POINT('Ctrl Pts',(-1.18304757425361,30.1133254112728,15.3818298511069));
#61803=CARTESIAN_POINT('Ctrl Pts',(-1.27115286095415,30.1254759916691,15.3334481546789));
#61804=CARTESIAN_POINT('Ctrl Pts',(-1.35603062313171,30.1376409804006,15.2796540167812));
#61805=CARTESIAN_POINT('Ctrl Pts',(-1.44090489737409,30.1498054692285,15.2258620894798));
#61806=CARTESIAN_POINT('Ctrl Pts',(-1.52255382815821,30.1619846397928,15.1666596796856));
#61807=CARTESIAN_POINT('Ctrl Pts',(-1.60027633593227,30.1742551659115,15.1022643792663));
#61808=CARTESIAN_POINT('Ctrl Pts',(-1.60027952996336,30.1742556701727,15.102261732921));
#61809=CARTESIAN_POINT('Ctrl Pts',(-1.60028272398781,30.174256174434,15.1022590865669));
#61810=CARTESIAN_POINT('Ctrl Pts',(-1.60028591800562,30.1742566786955,15.1022564402041));
#61811=CARTESIAN_POINT('Ctrl Pts',(-1.6556121130327,30.1829914040227,15.0564166251924));
#61812=CARTESIAN_POINT('Ctrl Pts',(-1.7088727262563,30.1917573173011,15.0080094863337));
#61813=CARTESIAN_POINT('Ctrl Pts',(-1.7599234820375,30.2006017288594,14.9572220375249));
#61814=CARTESIAN_POINT('Ctrl Pts',(-1.8738210369486,30.2203341860134,14.8439119375866));
#61815=CARTESIAN_POINT('Ctrl Pts',(-1.9767798244198,30.2404668949515,14.7186852514332));
#61816=CARTESIAN_POINT('Ctrl Pts',(-2.06678104296929,30.2607837065916,14.583998713918));
#61817=CARTESIAN_POINT('Ctrl Pts',(-2.0791973003519,30.2635865437819,14.5654178242066));
#61818=CARTESIAN_POINT('Ctrl Pts',(-2.0913668989552,30.2663928935877,14.5466568306674));
#61819=CARTESIAN_POINT('Ctrl Pts',(-2.10328448339727,30.2692021972246,14.5277221222004));
#61820=CARTESIAN_POINT('Ctrl Pts',(-2.15511224181361,30.2814194305838,14.4453779608576));
#61821=CARTESIAN_POINT('Ctrl Pts',(-2.20216501934561,30.2936897390157,14.3597551774029));
#61822=CARTESIAN_POINT('Ctrl Pts',(-2.24395841450402,30.3059607202294,14.2714967638777));
#61823=CARTESIAN_POINT('Ctrl Pts',(-2.26596138977105,30.3124210256228,14.2250313431445));
#61824=CARTESIAN_POINT('Ctrl Pts',(-2.28650738014192,30.3188815253586,14.1778357860376));
#61825=CARTESIAN_POINT('Ctrl Pts',(-2.30553125367308,30.3253346297916,14.130005746823));
#61826=CARTESIAN_POINT('Ctrl Pts',(-2.30553533391181,30.3253360138529,14.1299954882403));
#61827=CARTESIAN_POINT('Ctrl Pts',(-2.30553941408055,30.3253373979138,14.1299852296285));
#61828=CARTESIAN_POINT('Ctrl Pts',(-2.30554349417927,30.3253387819744,14.1299749709875));
#61829=CARTESIAN_POINT('Ctrl Pts',(-2.33525917090889,30.335419003064,14.0552604897481));
#61830=CARTESIAN_POINT('Ctrl Pts',(-2.36130148626115,30.3454845543004,13.9789016837452));
#61831=CARTESIAN_POINT('Ctrl Pts',(-2.38355823401219,30.3555699324038,13.9013347181094));
#61832=CARTESIAN_POINT('Ctrl Pts',(-2.42000205154344,30.3720840108957,13.7743244121248));
#61833=CARTESIAN_POINT('Ctrl Pts',(-2.44630586152763,30.3886555642733,13.6440648978829));
#61834=CARTESIAN_POINT('Ctrl Pts',(-2.46214628409733,30.4052617673184,13.5122063580512));
#61835=CARTESIAN_POINT('Ctrl Pts',(-2.47815337947532,30.4220427007082,13.3789604036455));
#61836=CARTESIAN_POINT('Ctrl Pts',(-2.48347301960662,30.4388587794074,13.2440793313919));
#61837=CARTESIAN_POINT('Ctrl Pts',(-2.477753291159,30.4556599230741,13.109316033593));
#61838=CARTESIAN_POINT('Ctrl Pts',(-2.4750610064385,30.4635682464841,13.045882748102));
#61839=CARTESIAN_POINT('Ctrl Pts',(-2.46992283116894,30.471472902046,12.9824764931707));
#61840=CARTESIAN_POINT('Ctrl Pts',(-2.46230396877764,30.4793669670259,12.919285459566));
#61841=CARTESIAN_POINT('Ctrl Pts',(-2.46230212926615,30.4793688729828,12.9192702026121));
#61842=CARTESIAN_POINT('Ctrl Pts',(-2.46230028961007,30.479370778939,12.9192549456707));
#61843=CARTESIAN_POINT('Ctrl Pts',(-2.46229844980938,30.4793726848947,12.9192396887419));
#61844=CARTESIAN_POINT('Ctrl Pts',(-2.45230851230945,30.4897218373576,12.8363960599049));
#61845=CARTESIAN_POINT('Ctrl Pts',(-2.43805598787451,30.5000467733648,12.7539095196764));
#61846=CARTESIAN_POINT('Ctrl Pts',(-2.41964302419575,30.510435508637,12.6722284099323));
#61847=CARTESIAN_POINT('Ctrl Pts',(-2.41850888848298,30.5110753967011,12.6671973098207));
#61848=CARTESIAN_POINT('Ctrl Pts',(-2.41735896832571,30.5117155262703,12.6621692480524));
#61849=CARTESIAN_POINT('Ctrl Pts',(-2.41619328710392,30.5123559175791,12.6571443227054));
#61850=CARTESIAN_POINT('Ctrl Pts',(0.312594521684916,39.2687268985923,10.2006318123981));
#61851=CARTESIAN_POINT('Ctrl Pts',(1.10278451631874,39.367686684378,10.2682228699795));
#61852=CARTESIAN_POINT('Ctrl Pts',(2.61633807062915,39.5646092557192,11.0339471882628));
#61853=CARTESIAN_POINT('Ctrl Pts',(3.48447994224266,39.8615963196975,13.4364945624193));
#61854=CARTESIAN_POINT('Ctrl Pts',(2.4737037416439,40.1586230481117,15.7850298071184));
#61855=CARTESIAN_POINT('Ctrl Pts',(0.519194218473144,40.407493993742,16.6463753640912));
#61856=CARTESIAN_POINT('Ctrl Pts',(-1.09278868638896,40.6071406712818,16.4018153614845));
#61857=CARTESIAN_POINT('Ctrl Pts',(-2.15309749265246,40.7570895673928,15.7935618381816));
#61858=CARTESIAN_POINT('Ctrl Pts',(-2.91471385951109,40.9071784817713,14.8368183188706));
#61859=CARTESIAN_POINT('Ctrl Pts',(-3.4010545907453,41.1074039103802,13.27518106621));
#61860=CARTESIAN_POINT('Ctrl Pts',(-2.95389395785344,41.3076508602556,11.6180538648701));
#61861=CARTESIAN_POINT('Ctrl Pts',(-1.74978220776,41.507656939418,10.5138956535236));
#61862=CARTESIAN_POINT('Ctrl Pts',(-0.485944985235109,41.6741175145073,
10.0214181492683));
#61863=CARTESIAN_POINT('Ctrl Pts',(1.02219499728983,41.8568649670751,10.1224423359238));
#61864=CARTESIAN_POINT('Ctrl Pts',(2.4080714216259,42.055620188501,11.0053265175813));
#61865=CARTESIAN_POINT('Ctrl Pts',(3.19871761650152,42.2536196929027,12.4385646110554));
#61866=CARTESIAN_POINT('Ctrl Pts',(3.20534904741162,42.4507122354209,14.0681869289385));
#61867=CARTESIAN_POINT('Ctrl Pts',(2.43477412422895,42.6467536737798,15.4938098236939));
#61868=CARTESIAN_POINT('Ctrl Pts',(1.0830399884291,42.841601180305,16.371133498718));
#61869=CARTESIAN_POINT('Ctrl Pts',(-0.24597312730138,43.0028674028311,16.4710263452315));
#61870=CARTESIAN_POINT('Ctrl Pts',(-1.17424515823741,43.1231290597125,16.1845758479658));
#61871=CARTESIAN_POINT('Ctrl Pts',(-1.62147454355865,43.1870491201526,15.930571493716));
#61872=CARTESIAN_POINT('Ctrl Pts',(-2.23622373822675,43.2827275887014,15.4716413166819));
#61873=CARTESIAN_POINT('Ctrl Pts',(-2.90863938487666,43.4176422979667,14.5818001747071));
#61874=CARTESIAN_POINT('Ctrl Pts',(-3.13855465666707,43.6064005807676,13.0381770779871));
#61875=CARTESIAN_POINT('Ctrl Pts',(-2.60415871522266,43.7933389117483,11.5873361511012));
#61876=CARTESIAN_POINT('Ctrl Pts',(-1.45426483026413,43.9783463662533,10.5801220890633));
#61877=CARTESIAN_POINT('Ctrl Pts',(0.0244694520634532,44.1613257418401,
10.2498340654442));
#61878=CARTESIAN_POINT('Ctrl Pts',(1.29887252139762,44.3220911833599,10.6192174467748));
#61879=CARTESIAN_POINT('Ctrl Pts',(2.41856206199899,44.5011143240446,11.5510825760216));
#61880=CARTESIAN_POINT('Ctrl Pts',(2.84250102970257,44.6386014173983,12.6326702660212));
#61881=CARTESIAN_POINT('Ctrl Pts',(2.80370202652921,44.7551453055736,13.5697356758772));
#61882=CARTESIAN_POINT('Ctrl Pts',(2.67642885900552,44.8324899718607,14.1780930409513));
#61883=CARTESIAN_POINT('Ctrl Pts',(2.19691057886715,44.9669190865462,15.1608829794906));
#61884=CARTESIAN_POINT('Ctrl Pts',(0.884633708880359,45.1562704903835,16.0821444896688));
#61885=CARTESIAN_POINT('Ctrl Pts',(-0.84304439264534,45.3605213244521,15.9901433791172));
#61886=CARTESIAN_POINT('Ctrl Pts',(-2.05603092570168,45.5429387474247,15.0919397400054));
#61887=CARTESIAN_POINT('Ctrl Pts',(-2.62182065763438,45.704578250735,13.8823526995957));
#61888=CARTESIAN_POINT('Ctrl Pts',(-2.53890823740617,45.8636701656143,12.5686554366777));
#61889=CARTESIAN_POINT('Ctrl Pts',(-1.84908359161403,46.0202157746922,11.4739637874368));
#61890=CARTESIAN_POINT('Ctrl Pts',(-0.737127953307188,46.1742234772143,
10.8524676464036));
#61891=CARTESIAN_POINT('Ctrl Pts',(0.515346184392654,46.3257139419959,10.8400377663191));
#61892=CARTESIAN_POINT('Ctrl Pts',(1.60285677681394,46.4747159390649,11.4192206339482));
#61893=CARTESIAN_POINT('Ctrl Pts',(2.26941428252578,46.621267325306,12.4315435743272));
#61894=CARTESIAN_POINT('Ctrl Pts',(2.36785255272078,46.765417671326,13.6189966756103));
#61895=CARTESIAN_POINT('Ctrl Pts',(1.89419027637734,46.9072227042509,14.6926655000575));
#61896=CARTESIAN_POINT('Ctrl Pts',(0.979655970614668,47.0467488710647,15.3945169326622));
#61897=CARTESIAN_POINT('Ctrl Pts',(-0.267888938204166,47.1993308203444,
15.5934545697946));
#61898=CARTESIAN_POINT('Ctrl Pts',(-1.53802286151021,47.3641460563792,15.0145962937778));
#61899=CARTESIAN_POINT('Ctrl Pts',(-2.22386857489773,47.5403959173155,13.6869883557155));
#61900=CARTESIAN_POINT('Ctrl Pts',(-1.99472867839811,47.6845135743016,12.4883514392389));
#61901=CARTESIAN_POINT('Ctrl Pts',(-1.40787042894492,47.7982904443204,11.7737414854899));
#61902=CARTESIAN_POINT('Ctrl Pts',(-0.628592239028725,47.9110997303948,
11.2898598022948));
#61903=CARTESIAN_POINT('Ctrl Pts',(0.549891817357097,48.0503941761843,11.2289545937645));
#61904=CARTESIAN_POINT('Ctrl Pts',(1.59591722050374,48.2013738551115,11.9659967128779));
#61905=CARTESIAN_POINT('Ctrl Pts',(2.00471040208874,48.3370802711296,13.0108431266425));
#61906=CARTESIAN_POINT('Ctrl Pts',(1.86296813475303,48.4783457746698,14.1718151081312));
#61907=CARTESIAN_POINT('Ctrl Pts',(1.16286679576134,48.5982957390209,14.9262017757273));
#61908=CARTESIAN_POINT('Ctrl Pts',(0.246695609337611,48.717566789975,15.2299109611891));
#61909=CARTESIAN_POINT('Ctrl Pts',(-0.569930120220827,48.8165778583093,
15.1898375551156));
#61910=CARTESIAN_POINT('Ctrl Pts',(-1.40496458666125,48.934940168389,14.6767864237024));
#61911=CARTESIAN_POINT('Ctrl Pts',(-1.89013333564764,49.0530095875852,13.8297344728053));
#61912=CARTESIAN_POINT('Ctrl Pts',(-1.91089170362233,49.1709390025344,12.8543916068453));
#61913=CARTESIAN_POINT('Ctrl Pts',(-1.46115125975772,49.2888886784375,11.9883720090566));
#61914=CARTESIAN_POINT('Ctrl Pts',(-0.785669968721914,49.3873285392625,
11.5338753755548));
#61915=CARTESIAN_POINT('Ctrl Pts',(-0.162780906843137,49.4662449068257,
11.3969697014267));
#61916=CARTESIAN_POINT('Ctrl Pts',(0.31613138970614,49.5255377704516,11.412316051461));
#61917=CARTESIAN_POINT('Ctrl Pts',(0.776867431823825,49.5849509789929,11.5464608590512));
#61918=CARTESIAN_POINT('Ctrl Pts',(1.40001179816061,49.6742843891679,11.9120303973004));
#61919=CARTESIAN_POINT('Ctrl Pts',(1.87317942742205,49.7740147394822,12.6037507980505));
#61920=CARTESIAN_POINT('Ctrl Pts',(1.97191227059097,49.8945205239042,13.5833072938098));
#61921=CARTESIAN_POINT('Ctrl Pts',(1.66936919957167,50.00574156926,14.4507596289108));
#61922=CARTESIAN_POINT('Ctrl Pts',(0.835340557919474,50.1417629552019,15.2072538991447));
#61923=CARTESIAN_POINT('Ctrl Pts',(-0.43261694699927,50.2931364853892,15.4022044191531));
#61924=CARTESIAN_POINT('Ctrl Pts',(-1.35934397586363,50.418870004698,14.8771965133792));
#61925=CARTESIAN_POINT('Ctrl Pts',(-1.89864355168201,50.5317973556908,14.1456434479416));
#61926=CARTESIAN_POINT('Ctrl Pts',(-2.08194393077751,50.604760573542,13.5721200297017));
#61927=CARTESIAN_POINT('Ctrl Pts',(-2.05671808092609,50.6801976316638,12.9645461728789));
#61928=CARTESIAN_POINT('Ctrl Pts',(-1.93870659718733,50.7451915351799,12.4553172529021));
#61929=CARTESIAN_POINT('Ctrl Pts',(-1.48562870557272,50.8598274622143,11.6353297371026));
#61930=CARTESIAN_POINT('Ctrl Pts',(-0.484014005491188,50.992982147934,11.085134484943));
#61931=CARTESIAN_POINT('Ctrl Pts',(0.620094294898221,51.1284453465146,11.1583829405731));
#61932=CARTESIAN_POINT('Ctrl Pts',(1.63397002672975,51.2654986273511,11.6292366243552));
#61933=CARTESIAN_POINT('Ctrl Pts',(2.4487093254446,51.4398837730822,12.887573924851));
#61934=CARTESIAN_POINT('Ctrl Pts',(2.12339578027333,51.6543187474332,14.7042901983831));
#61935=CARTESIAN_POINT('Ctrl Pts',(0.611026275306804,51.8741245979643,15.8381715292352));
#61936=CARTESIAN_POINT('Ctrl Pts',(-1.40546246703902,52.1098521447515,15.6203703325987));
#61937=CARTESIAN_POINT('Ctrl Pts',(-2.29978083208262,52.2747671286668,14.4865823778754));
#61938=CARTESIAN_POINT('Ctrl Pts',(-2.45785835496615,52.3637908706225,13.7890755589211));
#61939=CARTESIAN_POINT('Ctrl Pts',(0.294903861775253,39.6139115644023,10.4045779384392));
#61940=CARTESIAN_POINT('Ctrl Pts',(1.03268206896656,39.7064516885537,10.4785410543229));
#61941=CARTESIAN_POINT('Ctrl Pts',(2.42857112035405,39.8896587319756,11.2135222039816));
#61942=CARTESIAN_POINT('Ctrl Pts',(3.19296975732018,40.1633527535325,13.4396418953121));
#61943=CARTESIAN_POINT('Ctrl Pts',(2.23642221120207,40.4346975246274,15.5696280850306));
#61944=CARTESIAN_POINT('Ctrl Pts',(0.453975309221201,40.6602273892792,16.3228441371572));
#61945=CARTESIAN_POINT('Ctrl Pts',(-0.995070086503688,40.8401590193753,
16.0819104233793));
#61946=CARTESIAN_POINT('Ctrl Pts',(-1.93938070844708,40.9748303090262,15.5223972612286));
#61947=CARTESIAN_POINT('Ctrl Pts',(-2.60894671018738,41.1091870901098,14.6566847282954));
#61948=CARTESIAN_POINT('Ctrl Pts',(-3.02329663478697,41.2878712464816,13.2573491380613));
#61949=CARTESIAN_POINT('Ctrl Pts',(-2.60463724926944,41.4658015589571,11.7911606651713));
#61950=CARTESIAN_POINT('Ctrl Pts',(-1.52552555387745,41.6428577046171,10.8288627721415));
#61951=CARTESIAN_POINT('Ctrl Pts',(-0.403553397693664,41.7898852789765,
10.4094234971742));
#61952=CARTESIAN_POINT('Ctrl Pts',(0.923675528652629,41.9509113858405,10.5169608454263));
#61953=CARTESIAN_POINT('Ctrl Pts',(2.13077972830358,42.1256332856869,11.3097879483148));
#61954=CARTESIAN_POINT('Ctrl Pts',(2.80677821778962,42.299353081632,12.5765216609874));
#61955=CARTESIAN_POINT('Ctrl Pts',(2.79274880982071,42.4720138755312,14.0037583001608));
#61956=CARTESIAN_POINT('Ctrl Pts',(2.10130782698956,42.6435641932168,15.2415086413168));
#61957=CARTESIAN_POINT('Ctrl Pts',(0.908928431243241,42.8139558890705,15.9920026155197));
#61958=CARTESIAN_POINT('Ctrl Pts',(-0.253854780111174,42.9549481130077,
16.0630860323738));
#61959=CARTESIAN_POINT('Ctrl Pts',(-1.06179228515288,43.0601100424265,15.8012973910613));
#61960=CARTESIAN_POINT('Ctrl Pts',(-1.44967403461439,43.1160138685282,15.5737088269141));
#61961=CARTESIAN_POINT('Ctrl Pts',(-1.98157874533087,43.1997094802458,15.1647965689675));
#61962=CARTESIAN_POINT('Ctrl Pts',(-2.5588383120568,43.3177713855586,14.3780726568003));
#61963=CARTESIAN_POINT('Ctrl Pts',(-2.74104930113207,43.483143195421,13.0233004846037));
#61964=CARTESIAN_POINT('Ctrl Pts',(-2.25410072239219,43.647188172129,11.7572301414462));
#61965=CARTESIAN_POINT('Ctrl Pts',(-1.23048329990724,43.8098860070457,10.8863164624582));
#61966=CARTESIAN_POINT('Ctrl Pts',(0.0771158868406177,43.9712239212822,
10.6140519303021));
#61967=CARTESIAN_POINT('Ctrl Pts',(1.19916525789307,44.1134181689073,10.9572039819767));
#61968=CARTESIAN_POINT('Ctrl Pts',(2.1797215331002,44.2722435626865,11.7984904045362));
#61969=CARTESIAN_POINT('Ctrl Pts',(2.54314510409658,44.394707072148,12.7670995874116));
#61970=CARTESIAN_POINT('Ctrl Pts',(2.49539793108867,44.4989185614651,13.604153393425));
#61971=CARTESIAN_POINT('Ctrl Pts',(2.37287581901333,44.568191507612,14.1470080965811));
#61972=CARTESIAN_POINT('Ctrl Pts',(1.92877687281838,44.6888918452501,15.0222703355227));
#61973=CARTESIAN_POINT('Ctrl Pts',(0.732108445051806,44.8598258348619,15.8359448411065));
#61974=CARTESIAN_POINT('Ctrl Pts',(-0.838250425788402,45.0457028640936,
15.7283431435459));
#61975=CARTESIAN_POINT('Ctrl Pts',(-1.93723819221189,45.2130184634799,14.8869161384525));
#61976=CARTESIAN_POINT('Ctrl Pts',(-2.44132651224387,45.3623520315815,13.7613265784781));
#61977=CARTESIAN_POINT('Ctrl Pts',(-2.34379149512239,45.5104721996345,12.5400740554247));
#61978=CARTESIAN_POINT('Ctrl Pts',(-1.67903175903387,45.6574216643582,11.5239844507756));
#61979=CARTESIAN_POINT('Ctrl Pts',(-0.616494263126933,45.8032455001699,
10.9540765507697));
#61980=CARTESIAN_POINT('Ctrl Pts',(0.579876890742993,45.9479958855824,10.9634172020583));
#61981=CARTESIAN_POINT('Ctrl Pts',(1.61826918658412,46.0917277688557,11.5408030474182));
#61982=CARTESIAN_POINT('Ctrl Pts',(2.24906033510871,46.2344985697371,12.5384885873925));
#61983=CARTESIAN_POINT('Ctrl Pts',(2.32378436557046,46.37637271732,13.7083777135971));
#61984=CARTESIAN_POINT('Ctrl Pts',(1.83239123279297,46.5174147356513,14.7665437342237));
#61985=CARTESIAN_POINT('Ctrl Pts',(0.899464032953714,46.657693670538,15.4535636835773));
#61986=CARTESIAN_POINT('Ctrl Pts',(-0.371763906289662,46.8127931156224,
15.630157515452));
#61987=CARTESIAN_POINT('Ctrl Pts',(-1.66726587814456,46.9825231239923,15.0086744544976));
#61988=CARTESIAN_POINT('Ctrl Pts',(-2.35580384867077,47.1667730292082,13.6071446302206));
#61989=CARTESIAN_POINT('Ctrl Pts',(-2.08617697257812,47.3197112981773,12.34100074822));
#61990=CARTESIAN_POINT('Ctrl Pts',(-1.43906379959527,47.4418000516265,11.5892918254582));
#61991=CARTESIAN_POINT('Ctrl Pts',(-0.58526695271636,47.5637444470721,11.0864992112));
#61992=CARTESIAN_POINT('Ctrl Pts',(0.703174222752905,47.7159712607203,11.0485248694669));
#61993=CARTESIAN_POINT('Ctrl Pts',(1.8429732534516,47.8833013930449,11.8911301665703));
#61994=CARTESIAN_POINT('Ctrl Pts',(2.27259405105886,48.0354730745259,13.0729978551617));
#61995=CARTESIAN_POINT('Ctrl Pts',(2.07998644589785,48.1954006594234,14.3821003864233));
#61996=CARTESIAN_POINT('Ctrl Pts',(1.25848223006792,48.3327436550993,15.225877237191));
#61997=CARTESIAN_POINT('Ctrl Pts',(0.192592484505567,48.4704234645487,15.5485749946903));
#61998=CARTESIAN_POINT('Ctrl Pts',(-0.753401380942494,48.5853899109762,
15.4776711893897));
#61999=CARTESIAN_POINT('Ctrl Pts',(-1.71342552510336,48.7238069063804,14.8530008472574));
#62000=CARTESIAN_POINT('Ctrl Pts',(-2.25772039498446,48.8627612021184,13.8421264947207));
#62001=CARTESIAN_POINT('Ctrl Pts',(-2.25181468353777,49.0023278556759,12.6883745865887));
#62002=CARTESIAN_POINT('Ctrl Pts',(-1.69023381425614,49.142582938478,11.6738167015065));
#62003=CARTESIAN_POINT('Ctrl Pts',(-0.870245654444321,49.2600959933723,
11.1533123062566));
#62004=CARTESIAN_POINT('Ctrl Pts',(-0.121299859616587,49.3545201124099,
11.0097786824479));
#62005=CARTESIAN_POINT('Ctrl Pts',(0.451358189684015,49.4255548502409,11.04360042071));
#62006=CARTESIAN_POINT('Ctrl Pts',(0.999038222241836,49.4968126879922,11.2192031733343));
#62007=CARTESIAN_POINT('Ctrl Pts',(1.73449309711661,49.604047323927,11.6776627570674));
#62008=CARTESIAN_POINT('Ctrl Pts',(2.28033102004061,49.723896475789,12.523210973049));
#62009=CARTESIAN_POINT('Ctrl Pts',(2.36751628288518,49.8687455361102,13.7026302524268));
#62010=CARTESIAN_POINT('Ctrl Pts',(1.97671262830022,50.0023841240909,14.7341871695187));
#62011=CARTESIAN_POINT('Ctrl Pts',(0.952834108900274,50.1656178959293,15.614728141144));
#62012=CARTESIAN_POINT('Ctrl Pts',(-0.569770782102248,50.3468428570876,
15.8077195842284));
#62013=CARTESIAN_POINT('Ctrl Pts',(-1.65715677486589,50.496752779469,15.1534589049772));
#62014=CARTESIAN_POINT('Ctrl Pts',(-2.27546471621605,50.6309468937531,14.2688059616163));
#62015=CARTESIAN_POINT('Ctrl Pts',(-2.47523622476083,50.7174027252289,13.5842958454368));
#62016=CARTESIAN_POINT('Ctrl Pts',(-2.42770164858311,50.8064919076948,12.8681568966158));
#62017=CARTESIAN_POINT('Ctrl Pts',(-2.27399740751639,50.8831013712292,12.2718655454637));
#62018=CARTESIAN_POINT('Ctrl Pts',(-1.7181195707613,51.0178208654781,11.3221134951395));
#62019=CARTESIAN_POINT('Ctrl Pts',(-0.533448887883877,51.1732967383133,
10.7100836543821));
#62020=CARTESIAN_POINT('Ctrl Pts',(0.743053321251822,51.3303063206415,10.8254204432482));
#62021=CARTESIAN_POINT('Ctrl Pts',(1.89861213344509,51.4883421473996,11.3954710536808));
#62022=CARTESIAN_POINT('Ctrl Pts',(2.79438771635136,51.6878173191196,12.8565507493252));
#62023=CARTESIAN_POINT('Ctrl Pts',(2.37731698119797,51.9302681611678,14.9000235374981));
#62024=CARTESIAN_POINT('Ctrl Pts',(0.659697208520961,52.1757699545507,16.1255851353615));
#62025=CARTESIAN_POINT('Ctrl Pts',(-1.55650206655295,52.4357027514075,15.8344584184493));
#62026=CARTESIAN_POINT('Ctrl Pts',(-2.50012270616443,52.6150222833368,14.5799293707503));
#62027=CARTESIAN_POINT('Ctrl Pts',(-2.65572307264903,52.7110742858936,13.8247094991072));
#62028=CARTESIAN_POINT('Ctrl Pts',(0.27721320186559,39.9590962302123,10.6085240644802));
#62029=CARTESIAN_POINT('Ctrl Pts',(0.96257962161438,40.0452166927294,10.6888592386662));
#62030=CARTESIAN_POINT('Ctrl Pts',(2.24080417007896,40.2147082082319,11.3930972197004));
#62031=CARTESIAN_POINT('Ctrl Pts',(2.9014595723977,40.4651091873673,13.442789228205));
#62032=CARTESIAN_POINT('Ctrl Pts',(1.99914068076025,40.7107720011432,15.3542263629428));
#62033=CARTESIAN_POINT('Ctrl Pts',(0.388756399969259,40.9129607848164,15.9993129102233));
#62034=CARTESIAN_POINT('Ctrl Pts',(-0.897351486618409,41.0731773674687,
15.7620054852741));
#62035=CARTESIAN_POINT('Ctrl Pts',(-1.7256639242417,41.1925710506597,15.2512326842756));
#62036=CARTESIAN_POINT('Ctrl Pts',(-2.30317956086367,41.3111956984482,14.4765511377203));
#62037=CARTESIAN_POINT('Ctrl Pts',(-2.64553867882863,41.468338582583,13.2395172099127));
#62038=CARTESIAN_POINT('Ctrl Pts',(-2.25538054068543,41.6239522576586,11.9642674654724));
#62039=CARTESIAN_POINT('Ctrl Pts',(-1.30126889999489,41.7780584698162,11.1438298907594));
#62040=CARTESIAN_POINT('Ctrl Pts',(-0.321161810152211,41.9056530434457,
10.7974288450802));
#62041=CARTESIAN_POINT('Ctrl Pts',(0.82515606001542,42.0449578046059,10.9114793549288));
#62042=CARTESIAN_POINT('Ctrl Pts',(1.85348803498126,42.1956463828727,11.6142493790484));
#62043=CARTESIAN_POINT('Ctrl Pts',(2.41483881907772,42.3450864703612,12.7144787109194));
#62044=CARTESIAN_POINT('Ctrl Pts',(2.38014857222981,42.4933155156414,13.9393296713829));
#62045=CARTESIAN_POINT('Ctrl Pts',(1.76784152975018,42.6403747126539,14.9892074589397));
#62046=CARTESIAN_POINT('Ctrl Pts',(0.734816874057389,42.786310597836,15.6128717323214));
#62047=CARTESIAN_POINT('Ctrl Pts',(-0.261736432920961,42.9070288231842,
15.6551457195162));
#62048=CARTESIAN_POINT('Ctrl Pts',(-0.949339412068327,42.9970910251405,
15.4180189341568));
#62049=CARTESIAN_POINT('Ctrl Pts',(-1.27787352567013,43.0449786169039,15.2168461601121));
#62050=CARTESIAN_POINT('Ctrl Pts',(-1.726933752435,43.1166913717903,14.857951821253));
#62051=CARTESIAN_POINT('Ctrl Pts',(-2.20903723923693,43.2179004731506,14.1743451388937));
#62052=CARTESIAN_POINT('Ctrl Pts',(-2.34354394559704,43.3598858100745,13.0084238912205));
#62053=CARTESIAN_POINT('Ctrl Pts',(-1.90404272956172,43.5010374325095,11.9271241317911));
#62054=CARTESIAN_POINT('Ctrl Pts',(-1.00670176955033,43.6414256478381,11.192510835853));
#62055=CARTESIAN_POINT('Ctrl Pts',(0.129762321617784,43.7811221007244,10.9782697951601));
#62056=CARTESIAN_POINT('Ctrl Pts',(1.09945799438853,43.9047451544546,11.2951905171787));
#62057=CARTESIAN_POINT('Ctrl Pts',(1.94088100420141,44.0433728013285,12.0458982330509));
#62058=CARTESIAN_POINT('Ctrl Pts',(2.24378917849061,44.1508127268978,12.9015289088021));
#62059=CARTESIAN_POINT('Ctrl Pts',(2.18709383564812,44.2426918173567,13.6385711109727));
#62060=CARTESIAN_POINT('Ctrl Pts',(2.06932277902114,44.3038930433633,14.115923152211));
#62061=CARTESIAN_POINT('Ctrl Pts',(1.66064316676961,44.410864603954,14.8836576915548));
#62062=CARTESIAN_POINT('Ctrl Pts',(0.579583181223254,44.5633811793401,15.5897451925441));
#62063=CARTESIAN_POINT('Ctrl Pts',(-0.833456458931463,44.7308844037353,
15.4665429079745));
#62064=CARTESIAN_POINT('Ctrl Pts',(-1.81844545872208,44.8830981795351,14.6818925368995));
#62065=CARTESIAN_POINT('Ctrl Pts',(-2.26083236685335,45.020125812428,13.6403004573605));
#62066=CARTESIAN_POINT('Ctrl Pts',(-2.14867475283861,45.1572742336549,12.5114926741716));
#62067=CARTESIAN_POINT('Ctrl Pts',(-1.5089799264537,45.2946275540243,11.5740051141142));
#62068=CARTESIAN_POINT('Ctrl Pts',(-0.495860572946676,45.4322675231254,
11.0556854551358));
#62069=CARTESIAN_POINT('Ctrl Pts',(0.644407597093334,45.5702778291688,11.0867966377975));
#62070=CARTESIAN_POINT('Ctrl Pts',(1.6336815963543,45.7087395986466,11.662385460888));
#62071=CARTESIAN_POINT('Ctrl Pts',(2.22870638769164,45.8477298141681,12.6454336004577));
#62072=CARTESIAN_POINT('Ctrl Pts',(2.27971617842012,45.9873277633141,13.797758751584));
#62073=CARTESIAN_POINT('Ctrl Pts',(1.77059218920859,46.1276067670516,14.84042196839));
#62074=CARTESIAN_POINT('Ctrl Pts',(0.819272095292761,46.2686384700114,15.5126104344925));
#62075=CARTESIAN_POINT('Ctrl Pts',(-0.47563887437516,46.4262554109004,15.6668604611094));
#62076=CARTESIAN_POINT('Ctrl Pts',(-1.79650889477891,46.6009001916055,15.0027526152174));
#62077=CARTESIAN_POINT('Ctrl Pts',(-2.4877391224438,46.7931501411008,13.5273009047258));
#62078=CARTESIAN_POINT('Ctrl Pts',(-2.17762526675814,46.9549090220529,12.1936500572011));
#62079=CARTESIAN_POINT('Ctrl Pts',(-1.47025717024561,47.0853096589328,11.4048421654265));
#62080=CARTESIAN_POINT('Ctrl Pts',(-0.541941666403998,47.2163891637494,
10.8831386201051));
#62081=CARTESIAN_POINT('Ctrl Pts',(0.85645662814871,47.3815483452563,10.8680951451692));
#62082=CARTESIAN_POINT('Ctrl Pts',(2.09002928639948,47.5652289309781,11.8162636202629));
#62083=CARTESIAN_POINT('Ctrl Pts',(2.54047770002897,47.7338658779222,13.1351525836811));
#62084=CARTESIAN_POINT('Ctrl Pts',(2.29700475704268,47.9124555441771,14.5923856647155));
#62085=CARTESIAN_POINT('Ctrl Pts',(1.35409766437449,48.0671915711777,15.5255526986548));
#62086=CARTESIAN_POINT('Ctrl Pts',(0.138489359673523,48.2232801391222,15.8672390281914));
#62087=CARTESIAN_POINT('Ctrl Pts',(-0.936872641664163,48.3542019636433,
15.7655048236637));
#62088=CARTESIAN_POINT('Ctrl Pts',(-2.02188646354548,48.5126736443718,15.0292152708126));
#62089=CARTESIAN_POINT('Ctrl Pts',(-2.62530745432128,48.6725128166516,13.8545185166361));
#62090=CARTESIAN_POINT('Ctrl Pts',(-2.59273766345323,48.8337167088173,12.522357566332));
#62091=CARTESIAN_POINT('Ctrl Pts',(-1.91931636875457,48.9962771985184,11.3592613939564));
#62092=CARTESIAN_POINT('Ctrl Pts',(-0.954821340166725,49.1328634474821,
10.7727492369583));
#62093=CARTESIAN_POINT('Ctrl Pts',(-0.0798188123900331,49.242795317994,
10.6225876634692));
#62094=CARTESIAN_POINT('Ctrl Pts',(0.586584989661894,49.3255719300301,10.6748847899589));
#62095=CARTESIAN_POINT('Ctrl Pts',(1.22120901265984,49.4086743969914,10.8919454876174));
#62096=CARTESIAN_POINT('Ctrl Pts',(2.0689743960726,49.5338102586861,11.4432951168345));
#62097=CARTESIAN_POINT('Ctrl Pts',(2.68748261265918,49.6737782120957,12.4426711480475));
#62098=CARTESIAN_POINT('Ctrl Pts',(2.7631202951794,49.842970548316,13.8219532110439));
#62099=CARTESIAN_POINT('Ctrl Pts',(2.28405605702878,49.999026678922,15.0176147101266));
#62100=CARTESIAN_POINT('Ctrl Pts',(1.07032765988108,50.1894728366565,16.0222023831432));
#62101=CARTESIAN_POINT('Ctrl Pts',(-0.706924617205229,50.400549228786,16.2132347493037));
#62102=CARTESIAN_POINT('Ctrl Pts',(-1.95496957386815,50.5746355542401,15.4297212965753));
#62103=CARTESIAN_POINT('Ctrl Pts',(-2.65228588075009,50.7300964318154,14.3919684752911));
#62104=CARTESIAN_POINT('Ctrl Pts',(-2.86852851874415,50.8300448769158,13.5964716611719));
#62105=CARTESIAN_POINT('Ctrl Pts',(-2.79868521624013,50.9327861837258,12.7717676203526));
#62106=CARTESIAN_POINT('Ctrl Pts',(-2.60928821784544,51.0210112072784,12.0884138380253));
#62107=CARTESIAN_POINT('Ctrl Pts',(-1.9506104359499,51.1758142687417,11.0088972531764));
#62108=CARTESIAN_POINT('Ctrl Pts',(-0.582883770276567,51.3536113286928,
10.3350328238214));
#62109=CARTESIAN_POINT('Ctrl Pts',(0.866012347605427,51.5321672947683,10.4924579459233));
#62110=CARTESIAN_POINT('Ctrl Pts',(2.16325424016043,51.7111856674481,11.1617054830065));
#62111=CARTESIAN_POINT('Ctrl Pts',(3.14006610725811,51.935750865157,12.8255275737996));
#62112=CARTESIAN_POINT('Ctrl Pts',(2.63123818212263,52.2062175749024,15.0957568766131));
#62113=CARTESIAN_POINT('Ctrl Pts',(0.708368141735119,52.4774153111372,16.4129987414879));
#62114=CARTESIAN_POINT('Ctrl Pts',(-1.70754166606687,52.7615533580634,16.0485465042998));
#62115=CARTESIAN_POINT('Ctrl Pts',(-2.70046458024624,52.9552774380068,14.6732763636255));
#62116=CARTESIAN_POINT('Ctrl Pts',(-2.85358779033189,53.0583577011648,13.8603434392933));
#62117=CARTESIAN_POINT('Ctrl Pts',(0.259522541955927,40.3042808960223,10.8124701905213));
#62118=CARTESIAN_POINT('Ctrl Pts',(0.8924771742622,40.3839816969049,10.8991774230097));
#62119=CARTESIAN_POINT('Ctrl Pts',(2.05303721980387,40.5397576844882,11.5726722354191));
#62120=CARTESIAN_POINT('Ctrl Pts',(2.60994938747521,40.7668656212022,13.4459365610979));
#62121=CARTESIAN_POINT('Ctrl Pts',(1.76185915031841,40.9868464776589,15.1388246408551));
#62122=CARTESIAN_POINT('Ctrl Pts',(0.323537490717318,41.1656941803536,15.6757816832893));
#62123=CARTESIAN_POINT('Ctrl Pts',(-0.799632886733132,41.3061957155623,
15.4421005471689));
#62124=CARTESIAN_POINT('Ctrl Pts',(-1.51194714003632,41.4103117922932,14.9800681073227));
#62125=CARTESIAN_POINT('Ctrl Pts',(-1.99741241153996,41.5132043067865,14.2964175471451));
#62126=CARTESIAN_POINT('Ctrl Pts',(-2.2677807228703,41.6488059186844,13.221685281764));
#62127=CARTESIAN_POINT('Ctrl Pts',(-1.90612383210144,41.78210295636,12.1373742657736));
#62128=CARTESIAN_POINT('Ctrl Pts',(-1.07701224611235,41.9132592350153,11.4587970093773));
#62129=CARTESIAN_POINT('Ctrl Pts',(-0.238770222610763,42.0214208079148,
11.185434192986));
#62130=CARTESIAN_POINT('Ctrl Pts',(0.726636591378214,42.1390042233713,11.3059978644313));
#62131=CARTESIAN_POINT('Ctrl Pts',(1.57619634165895,42.2656594800585,11.9187108097819));
#62132=CARTESIAN_POINT('Ctrl Pts',(2.02289942036582,42.3908198590905,12.8524357608515));
#62133=CARTESIAN_POINT('Ctrl Pts',(1.9675483346389,42.5146171557516,13.8749010426051));
#62134=CARTESIAN_POINT('Ctrl Pts',(1.43437523251079,42.637185232091,14.7369062765628));
#62135=CARTESIAN_POINT('Ctrl Pts',(0.56070531687153,42.7586653066015,15.2337408491231));
#62136=CARTESIAN_POINT('Ctrl Pts',(-0.269618085730753,42.8591095333607,
15.2472054066585));
#62137=CARTESIAN_POINT('Ctrl Pts',(-0.83688653898379,42.9340720078546,15.0347404772521));
#62138=CARTESIAN_POINT('Ctrl Pts',(-1.10607301672588,42.9739433652795,14.8599834933103));
#62139=CARTESIAN_POINT('Ctrl Pts',(-1.47228875953913,43.0336732633348,14.5511070735386));
#62140=CARTESIAN_POINT('Ctrl Pts',(-1.85923616641706,43.1180295607426,13.9706176209871));
#62141=CARTESIAN_POINT('Ctrl Pts',(-1.94603859006203,43.2366284247279,12.9935472978372));
#62142=CARTESIAN_POINT('Ctrl Pts',(-1.55398473673125,43.3548866928901,12.097018122136));
#62143=CARTESIAN_POINT('Ctrl Pts',(-0.782920239193443,43.4729652886305,
11.4987052092478));
#62144=CARTESIAN_POINT('Ctrl Pts',(0.182408756394949,43.5910202801664,11.342487660018));
#62145=CARTESIAN_POINT('Ctrl Pts',(0.999750730883996,43.6960721400019,11.6331770523806));
#62146=CARTESIAN_POINT('Ctrl Pts',(1.70204047530261,43.8145020399705,12.2933060615655));
#62147=CARTESIAN_POINT('Ctrl Pts',(1.94443325288464,43.9069183816476,13.0359582301927));
#62148=CARTESIAN_POINT('Ctrl Pts',(1.87878974020758,43.9864650732482,13.6729888285206));
#62149=CARTESIAN_POINT('Ctrl Pts',(1.76576973902895,44.0395945791145,14.0848382078407));
#62150=CARTESIAN_POINT('Ctrl Pts',(1.39250946072084,44.1328373626579,14.7450450475868));
#62151=CARTESIAN_POINT('Ctrl Pts',(0.427057917394702,44.2669365238183,15.3435455439818));
#62152=CARTESIAN_POINT('Ctrl Pts',(-0.828662492074526,44.4160659433769,
15.2047426724031));
#62153=CARTESIAN_POINT('Ctrl Pts',(-1.69965272523227,44.5531778955905,14.4768689353467));
#62154=CARTESIAN_POINT('Ctrl Pts',(-2.08033822146284,44.6778995932745,13.519274336243));
#62155=CARTESIAN_POINT('Ctrl Pts',(-1.95355801055484,44.8040762676752,12.4829112929186));
#62156=CARTESIAN_POINT('Ctrl Pts',(-1.33892809387352,44.9318334436903,11.6240257774529));
#62157=CARTESIAN_POINT('Ctrl Pts',(-0.375226882766422,45.061289546081,11.1572943595019));
#62158=CARTESIAN_POINT('Ctrl Pts',(0.708938303443674,45.1925597727553,11.2101760735367));
#62159=CARTESIAN_POINT('Ctrl Pts',(1.64909400612448,45.3257514284375,11.7839678743579));
#62160=CARTESIAN_POINT('Ctrl Pts',(2.20835244027458,45.4609610585992,12.752378613523));
#62161=CARTESIAN_POINT('Ctrl Pts',(2.2356479912698,45.598282809308,13.8871397895708));
#62162=CARTESIAN_POINT('Ctrl Pts',(1.70879314562423,45.737798798452,14.9143002025562));
#62163=CARTESIAN_POINT('Ctrl Pts',(0.739080157631811,45.8795832694846,15.5716571854076));
#62164=CARTESIAN_POINT('Ctrl Pts',(-0.579513842460654,46.0397177061783,
15.7035634067668));
#62165=CARTESIAN_POINT('Ctrl Pts',(-1.92575191141326,46.2192772592186,14.9968307759372));
#62166=CARTESIAN_POINT('Ctrl Pts',(-2.61967439621684,46.4195272529936,13.447457179231));
#62167=CARTESIAN_POINT('Ctrl Pts',(-2.26907356093815,46.5901067459285,12.0462993661822));
#62168=CARTESIAN_POINT('Ctrl Pts',(-1.50145054089596,46.728819266239,11.2203925053949));
#62169=CARTESIAN_POINT('Ctrl Pts',(-0.498616380091633,46.8690338804268,
10.6797780290102));
#62170=CARTESIAN_POINT('Ctrl Pts',(1.00973903354452,47.0471254297924,10.6876654208715));
#62171=CARTESIAN_POINT('Ctrl Pts',(2.33708531934735,47.2471564689115,11.7413970739553));
#62172=CARTESIAN_POINT('Ctrl Pts',(2.80836134899909,47.4322586813186,13.1973073122003));
#62173=CARTESIAN_POINT('Ctrl Pts',(2.51402306818751,47.6295104289307,14.8026709430076));
#62174=CARTESIAN_POINT('Ctrl Pts',(1.44971309868106,47.8016394872561,15.8252281601187));
#62175=CARTESIAN_POINT('Ctrl Pts',(0.084386234841479,47.9761368136959,16.1859030616927));
#62176=CARTESIAN_POINT('Ctrl Pts',(-1.12034390238583,48.1230140163103,16.0533384579378));
#62177=CARTESIAN_POINT('Ctrl Pts',(-2.3303474019876,48.3015403823632,15.2054296943677));
#62178=CARTESIAN_POINT('Ctrl Pts',(-2.99289451365811,48.4822644311848,13.8669105385515));
#62179=CARTESIAN_POINT('Ctrl Pts',(-2.93366064336868,48.6651055619588,12.3563405460754));
#62180=CARTESIAN_POINT('Ctrl Pts',(-2.14839892325299,48.8499714585589,11.0447060864063));
#62181=CARTESIAN_POINT('Ctrl Pts',(-1.03939702588914,49.005630901592,10.3921861676601));
#62182=CARTESIAN_POINT('Ctrl Pts',(-0.0383377651634865,49.1310705235782,
10.2353966444905));
#62183=CARTESIAN_POINT('Ctrl Pts',(0.721811789639765,49.2255890098193,10.3061691592078));
#62184=CARTESIAN_POINT('Ctrl Pts',(1.44337980307785,49.3205361059907,10.5646878019004));
#62185=CARTESIAN_POINT('Ctrl Pts',(2.4034556950286,49.4635731934453,11.2089274766015));
#62186=CARTESIAN_POINT('Ctrl Pts',(3.09463420527775,49.6236599484025,12.362131323046));
#62187=CARTESIAN_POINT('Ctrl Pts',(3.15872430747361,49.817195560522,13.9412761696611));
#62188=CARTESIAN_POINT('Ctrl Pts',(2.59139948575733,49.995669233753,15.3010422507346));
#62189=CARTESIAN_POINT('Ctrl Pts',(1.18782121086188,50.2133277773838,16.4296766251425));
#62190=CARTESIAN_POINT('Ctrl Pts',(-0.844078452308207,50.4542556004844,
16.6187499143789));
#62191=CARTESIAN_POINT('Ctrl Pts',(-2.25278237287041,50.6525183290112,15.7059836881734));
#62192=CARTESIAN_POINT('Ctrl Pts',(-3.02910704528412,50.8292459698778,14.5151309889659));
#62193=CARTESIAN_POINT('Ctrl Pts',(-3.26182081272746,50.9426870286026,13.608647476907));
#62194=CARTESIAN_POINT('Ctrl Pts',(-3.16966878389714,51.0590804597567,12.6753783440895));
#62195=CARTESIAN_POINT('Ctrl Pts',(-2.94457902817449,51.1589210433276,11.904962130587));
#62196=CARTESIAN_POINT('Ctrl Pts',(-2.18310130113848,51.3338076720054,10.6956810112131));
#62197=CARTESIAN_POINT('Ctrl Pts',(-0.632318652669253,51.5339259190722,
9.95998199326065));
#62198=CARTESIAN_POINT('Ctrl Pts',(0.988971373959032,51.7340282688952,10.1594954485985));
#62199=CARTESIAN_POINT('Ctrl Pts',(2.42789634687579,51.9340291874966,10.9279399123321));
#62200=CARTESIAN_POINT('Ctrl Pts',(3.48574449816487,52.1836844111943,12.7945043982738));
#62201=CARTESIAN_POINT('Ctrl Pts',(2.88515938304727,52.482166988637,15.2914902157282));
#62202=CARTESIAN_POINT('Ctrl Pts',(0.757039074949276,52.7790606677237,16.7004123476143));
#62203=CARTESIAN_POINT('Ctrl Pts',(-1.8585812655808,53.0874039647193,16.2626345901503));
#62204=CARTESIAN_POINT('Ctrl Pts',(-2.90080645432805,53.2955325926767,14.7666233565004));
#62205=CARTESIAN_POINT('Ctrl Pts',(-3.05145250801475,53.4056411164359,13.8959773794795));
#62206=CARTESIAN_POINT('Ctrl Pts',(0.29921364472731,40.3086929042607,10.8178945405685));
#62207=CARTESIAN_POINT('Ctrl Pts',(0.389708924283056,40.3200412428889,10.8317964718351));
#62208=CARTESIAN_POINT('Ctrl Pts',(0.479307970878857,40.3312307169892,10.8507982196188));
#62209=CARTESIAN_POINT('Ctrl Pts',(0.567442862048113,40.3423697335524,10.874654633906));
#62210=CARTESIAN_POINT('Ctrl Pts',(0.61829069060576,40.3487961873324,10.8884181598784));
#62211=CARTESIAN_POINT('Ctrl Pts',(0.668650725446275,40.3552057799045,10.9037966870897));
#62212=CARTESIAN_POINT('Ctrl Pts',(0.71841105546202,40.3616187646839,10.9207358224377));
#62213=CARTESIAN_POINT('Ctrl Pts',(0.768295778232184,40.3680477808852,10.9377173028767));
#62214=CARTESIAN_POINT('Ctrl Pts',(0.817584154307734,40.3744817266285,10.9562693482308));
#62215=CARTESIAN_POINT('Ctrl Pts',(0.866182167778944,40.3809444554227,10.9763435938198));
#62216=CARTESIAN_POINT('Ctrl Pts',(0.992812167616661,40.3977841426384,11.028650293911));
#62217=CARTESIAN_POINT('Ctrl Pts',(1.11477083880608,40.4148213759188,11.0912994771739));
#62218=CARTESIAN_POINT('Ctrl Pts',(1.23052443055251,40.4319181993909,11.1631211590004));
#62219=CARTESIAN_POINT('Ctrl Pts',(1.32825415279444,40.4463528945389,11.2237595626123));
#62220=CARTESIAN_POINT('Ctrl Pts',(1.42155667767204,40.4608333153926,11.2909313605061));
#62221=CARTESIAN_POINT('Ctrl Pts',(1.50958454153687,40.4753200946979,11.3640247833597));
#62222=CARTESIAN_POINT('Ctrl Pts',(1.52586217991162,40.4779989118859,11.3775408253554));
#62223=CARTESIAN_POINT('Ctrl Pts',(1.54195940664155,40.4806779520352,11.3912594810224));
#62224=CARTESIAN_POINT('Ctrl Pts',(1.55787077915975,40.4833569738712,11.4051770599222));
#62225=CARTESIAN_POINT('Ctrl Pts',(1.63095701633537,40.4956626140715,11.4691051384844));
#62226=CARTESIAN_POINT('Ctrl Pts',(1.70012936350538,40.5079651183981,11.5372375066277));
#62227=CARTESIAN_POINT('Ctrl Pts',(1.76480372628695,40.5201590532169,11.6090886428941));
#62228=CARTESIAN_POINT('Ctrl Pts',(1.79231321248755,40.5253457897722,11.6396507969936));
#62229=CARTESIAN_POINT('Ctrl Pts',(1.8190095269056,40.5305129350236,11.6708856794057));
#62230=CARTESIAN_POINT('Ctrl Pts',(1.84485058684559,40.5356526085924,11.7027558137197));
#62231=CARTESIAN_POINT('Ctrl Pts',(1.85147263365616,40.5369697046806,11.7109228750467));
#62232=CARTESIAN_POINT('Ctrl Pts',(1.85803839042547,40.5382849988255,11.7191315174064));
#62233=CARTESIAN_POINT('Ctrl Pts',(1.86454710629466,40.5395983634004,11.7273810383168));
#62234=CARTESIAN_POINT('Ctrl Pts',(1.86456047911591,40.5396010618421,11.7273979877997));
#62235=CARTESIAN_POINT('Ctrl Pts',(1.86457385169639,40.5396037602755,11.7274149374552));
#62236=CARTESIAN_POINT('Ctrl Pts',(1.86458722403605,40.5396064587008,11.7274318872833));
#62237=CARTESIAN_POINT('Ctrl Pts',(1.91920647481157,40.5506281626434,11.7966633704424));
#62238=CARTESIAN_POINT('Ctrl Pts',(1.96988117462805,40.5615262747318,11.868867246658));
#62239=CARTESIAN_POINT('Ctrl Pts',(2.01635880546304,40.5724223878967,11.9435176162419));
#62240=CARTESIAN_POINT('Ctrl Pts',(2.03391176247672,40.5765374643875,11.9717104200664));
#62241=CARTESIAN_POINT('Ctrl Pts',(2.05086612770534,40.580652204766,12.0002516398698));
#62242=CARTESIAN_POINT('Ctrl Pts',(2.06720854888125,40.5847729704798,12.0291110379928));
#62243=CARTESIAN_POINT('Ctrl Pts',(2.1251107751972,40.5993731026384,12.1313617010662));
#62244=CARTESIAN_POINT('Ctrl Pts',(2.17534849306533,40.6140595297461,12.2376372192857));
#62245=CARTESIAN_POINT('Ctrl Pts',(2.21770338471842,40.6287898647364,12.3467457412031));
#62246=CARTESIAN_POINT('Ctrl Pts',(2.22676037647349,40.6319397375693,12.3700770482811));
#62247=CARTESIAN_POINT('Ctrl Pts',(2.23545679903343,40.635091626804,12.3935380428671));
#62248=CARTESIAN_POINT('Ctrl Pts',(2.24379030937884,40.6382451323147,12.4171172937197));
#62249=CARTESIAN_POINT('Ctrl Pts',(2.28177739974992,40.6526199268315,12.5245998665965));
#62250=CARTESIAN_POINT('Ctrl Pts',(2.31222379200685,40.6670266825246,12.6345367851813));
#62251=CARTESIAN_POINT('Ctrl Pts',(2.33494566400176,40.6813420419667,12.7457804166104));
#62252=CARTESIAN_POINT('Ctrl Pts',(2.34093686488405,40.6851166514768,12.7751126363728));
#62253=CARTESIAN_POINT('Ctrl Pts',(2.3463910825083,40.6888849446716,12.8045359763344));
#62254=CARTESIAN_POINT('Ctrl Pts',(2.35130503246029,40.6926447427818,12.8340299954686));
#62255=CARTESIAN_POINT('Ctrl Pts',(2.3708251816471,40.7075801452054,12.951191883409));
#62256=CARTESIAN_POINT('Ctrl Pts',(2.3818237226639,40.7223757699855,13.0694732144141));
#62257=CARTESIAN_POINT('Ctrl Pts',(2.38389473371903,40.7371193386535,13.1875244947628));
#62258=CARTESIAN_POINT('Ctrl Pts',(2.38425800952661,40.7397055063136,13.2082318560773));
#62259=CARTESIAN_POINT('Ctrl Pts',(2.38434665072993,40.7422900586909,13.2289320216384));
#62260=CARTESIAN_POINT('Ctrl Pts',(2.3841585449045,40.7448734517146,13.2496175621632));
#62261=CARTESIAN_POINT('Ctrl Pts',(2.38380342397982,40.7497505836018,13.2886693473047));
#62262=CARTESIAN_POINT('Ctrl Pts',(2.38246187836942,40.7546234616989,13.3276680242106));
#62263=CARTESIAN_POINT('Ctrl Pts',(2.38012342299583,40.7594914216212,13.3665605088907));
#62264=CARTESIAN_POINT('Ctrl Pts',(2.37908962600529,40.7616434756543,13.3837543087259));
#62265=CARTESIAN_POINT('Ctrl Pts',(2.37786100980895,40.7637945658517,13.4009273349506));
#62266=CARTESIAN_POINT('Ctrl Pts',(2.37643673308905,40.7659446431555,13.4180750779064));
#62267=CARTESIAN_POINT('Ctrl Pts',(2.37233988670818,40.7721292112929,13.4673995298806));
#62268=CARTESIAN_POINT('Ctrl Pts',(2.36662142988896,40.778308975065,13.5165432850552));
#62269=CARTESIAN_POINT('Ctrl Pts',(2.35933309034131,40.7844817243333,13.5654036434861));
#62270=CARTESIAN_POINT('Ctrl Pts',(2.33704875590962,40.8033551053219,13.7147957732856));
#62271=CARTESIAN_POINT('Ctrl Pts',(2.30014819488779,40.8221023500989,13.8615581024037));
#62272=CARTESIAN_POINT('Ctrl Pts',(2.25003614297448,40.8407735714396,14.0033046981994));
#62273=CARTESIAN_POINT('Ctrl Pts',(2.19888350058474,40.8598325058027,14.1479947008606));
#62274=CARTESIAN_POINT('Ctrl Pts',(2.13389124211246,40.878890914239,14.287436632662));
#62275=CARTESIAN_POINT('Ctrl Pts',(2.0566055062284,40.8979317948094,14.4190419642919));
#62276=CARTESIAN_POINT('Ctrl Pts',(1.98146478693575,40.9164442078138,14.5469946733954));
#62277=CARTESIAN_POINT('Ctrl Pts',(1.89470320260612,40.9349397372278,14.6675387394565));
#62278=CARTESIAN_POINT('Ctrl Pts',(1.79776587934872,40.9533860059923,14.7783012426381));
#62279=CARTESIAN_POINT('Ctrl Pts',(1.75293375851325,40.961917140569,14.8295273107799));
#62280=CARTESIAN_POINT('Ctrl Pts',(1.70594716370153,40.9704109181371,14.8786784377205));
#62281=CARTESIAN_POINT('Ctrl Pts',(1.65693321099782,40.9788826648687,14.9255125539089));
#62282=CARTESIAN_POINT('Ctrl Pts',(1.64331612303024,40.9812362910123,14.9385240382893));
#62283=CARTESIAN_POINT('Ctrl Pts',(1.62954199423124,40.9835889418671,14.9513561644984));
#62284=CARTESIAN_POINT('Ctrl Pts',(1.61561341902634,40.9859406848803,14.9640042671608));
#62285=CARTESIAN_POINT('Ctrl Pts',(1.61559001021275,40.9859446372956,14.9640255239709));
#62286=CARTESIAN_POINT('Ctrl Pts',(1.61556660095658,40.9859485897094,14.9640467802669));
#62287=CARTESIAN_POINT('Ctrl Pts',(1.61554319125781,40.9859525421217,14.9640680360489));
#62288=CARTESIAN_POINT('Ctrl Pts',(1.53699799424492,40.9992138406697,15.0353863217062));
#62289=CARTESIAN_POINT('Ctrl Pts',(1.45346874200654,41.0124580741077,15.100913361394));
#62290=CARTESIAN_POINT('Ctrl Pts',(1.36598276713797,41.0256372990086,15.1603283697664));
#62291=CARTESIAN_POINT('Ctrl Pts',(1.30906834718812,41.0342111068876,15.1989810880212));
#62292=CARTESIAN_POINT('Ctrl Pts',(1.25047987467762,41.042757462791,15.2350481158454));
#62293=CARTESIAN_POINT('Ctrl Pts',(1.1905023459014,41.0512638657709,15.26845268478));
#62294=CARTESIAN_POINT('Ctrl Pts',(1.08122052341071,41.0667629241591,15.329317349383));
#62295=CARTESIAN_POINT('Ctrl Pts',(0.967285307371829,41.0821959395283,15.3812831031045));
#62296=CARTESIAN_POINT('Ctrl Pts',(0.850290169753213,41.0976389120642,15.4238000634698));
#62297=CARTESIAN_POINT('Ctrl Pts',(0.795820561512864,41.1048287208136,15.4435947508544));
#62298=CARTESIAN_POINT('Ctrl Pts',(0.740688400621284,41.1120205844328,15.4613411633113));
#62299=CARTESIAN_POINT('Ctrl Pts',(0.68505833144481,41.1192216234386,15.4769835331194));
#62300=CARTESIAN_POINT('Ctrl Pts',(0.571552703550573,41.1339143690336,15.5088996718751));
#62301=CARTESIAN_POINT('Ctrl Pts',(0.455966207734481,41.1486479005713,15.5320595644014));
#62302=CARTESIAN_POINT('Ctrl Pts',(0.339637431692946,41.1634826568834,15.5460020514382));
#62303=CARTESIAN_POINT('Ctrl Pts',(0.325257843037984,41.1653164051684,15.5477255048711));
#62304=CARTESIAN_POINT('Ctrl Pts',(0.310866960743178,41.1671516927431,15.5493080740837));
#62305=CARTESIAN_POINT('Ctrl Pts',(0.296467356775281,41.1689886274585,15.5507488532967));
#62306=CARTESIAN_POINT('Ctrl Pts',(0.226273338322151,41.1779431674308,15.5577722466407));
#62307=CARTESIAN_POINT('Ctrl Pts',(0.155897904900614,41.1867591053219,15.5616485894261));
#62308=CARTESIAN_POINT('Ctrl Pts',(0.0855691817809186,41.1955437231765,
15.5621662701891));
#62309=CARTESIAN_POINT('Ctrl Pts',(0.0721177742732594,41.197223911147,15.5622652842846));
#62310=CARTESIAN_POINT('Ctrl Pts',(0.058668207975929,41.1989029364518,15.5622413560316));
#62311=CARTESIAN_POINT('Ctrl Pts',(0.0452222715730123,41.2005815256376,
15.562092905444));
#62312=CARTESIAN_POINT('Ctrl Pts',(0.0451600061366055,41.2005892988477,
15.5620922179991));
#62313=CARTESIAN_POINT('Ctrl Pts',(0.0450977407922936,41.2005970720496,
15.5620915278801));
#62314=CARTESIAN_POINT('Ctrl Pts',(0.0450354755402967,41.2006048452436,
15.5620908350869));
#62315=CARTESIAN_POINT('Ctrl Pts',(-0.081427957730793,41.2163925399532,
15.5606837419627));
#62316=CARTESIAN_POINT('Ctrl Pts',(-0.207510800809204,41.2321468958339,
15.548240943279));
#62317=CARTESIAN_POINT('Ctrl Pts',(-0.331408562526946,41.2478592715305,
15.525416196154));
#62318=CARTESIAN_POINT('Ctrl Pts',(-0.446691773100654,41.2624791733829,
15.5041784426013));
#62319=CARTESIAN_POINT('Ctrl Pts',(-0.560079211735611,41.277062186552,15.4739576326248));
#62320=CARTESIAN_POINT('Ctrl Pts',(-0.670192647273795,41.2916109840416,
15.4352831102998));
#62321=CARTESIAN_POINT('Ctrl Pts',(-0.706446075772782,41.2964009879767,
15.4225500226162));
#62322=CARTESIAN_POINT('Ctrl Pts',(-0.742344255168313,41.3011872392498,
15.4089006313629));
#62323=CARTESIAN_POINT('Ctrl Pts',(-0.777839298886074,41.3059700276314,
15.394352965456));
#62324=CARTESIAN_POINT('Ctrl Pts',(-0.777878076994723,41.3059752527971,
15.3943370722239));
#62325=CARTESIAN_POINT('Ctrl Pts',(-0.777916854633722,41.3059804779314,
15.3943211779562));
#62326=CARTESIAN_POINT('Ctrl Pts',(-0.777955631802971,41.3059857030343,
15.394305282653));
#62327=CARTESIAN_POINT('Ctrl Pts',(-0.845785815731969,41.3151256091237,
15.3665007429917));
#62328=CARTESIAN_POINT('Ctrl Pts',(-0.912182599394111,41.3241697766217,
15.3355258587009));
#62329=CARTESIAN_POINT('Ctrl Pts',(-0.976793529516771,41.3332125956318,
15.3014564402282));
#62330=CARTESIAN_POINT('Ctrl Pts',(-1.00835275007618,41.3376295622205,15.2848152265841));
#62331=CARTESIAN_POINT('Ctrl Pts',(-1.03948518449441,41.3420461083214,15.2674360359707));
#62332=CARTESIAN_POINT('Ctrl Pts',(-1.07014589413268,41.3464726629492,15.2493300025927));
#62333=CARTESIAN_POINT('Ctrl Pts',(-1.09008732209048,41.3493516511152,15.2375540142197));
#62334=CARTESIAN_POINT('Ctrl Pts',(-1.10982934471936,41.3522356210233,15.2254693704854));
#62335=CARTESIAN_POINT('Ctrl Pts',(-1.12936096218729,41.3551260565641,15.213080737006));
#62336=CARTESIAN_POINT('Ctrl Pts',(-1.18740847623011,41.3637163639424,15.1762620056825));
#62337=CARTESIAN_POINT('Ctrl Pts',(-1.24360031778782,41.3723650434639,15.1367548615641));
#62338=CARTESIAN_POINT('Ctrl Pts',(-1.29777160212577,41.3809771605696,15.0948428402832));
#62339=CARTESIAN_POINT('Ctrl Pts',(-1.3297139369798,41.3860553331061,15.0701292335352));
#62340=CARTESIAN_POINT('Ctrl Pts',(-1.36095461147447,41.3911209143976,15.044579025209));
#62341=CARTESIAN_POINT('Ctrl Pts',(-1.39146671510647,41.3961554986744,15.0182454627002));
#62342=CARTESIAN_POINT('Ctrl Pts',(-1.41900663030876,41.4006996633684,14.9944770563257));
#62343=CARTESIAN_POINT('Ctrl Pts',(-1.44593358249322,41.4052387725666,14.9700461351532));
#62344=CARTESIAN_POINT('Ctrl Pts',(-1.47220672066735,41.4097741167282,14.944977687754));
#62345=CARTESIAN_POINT('Ctrl Pts',(-1.47285119576385,41.4098853678603,14.9443627634937));
#62346=CARTESIAN_POINT('Ctrl Pts',(-1.47349528119897,41.4099966173698,14.9437474520967));
#62347=CARTESIAN_POINT('Ctrl Pts',(-1.4741389764032,41.4101078652536,14.943131753934));
#62348=CARTESIAN_POINT('Ctrl Pts',(-1.55503558920578,41.4240889807296,14.8657536788142));
#62349=CARTESIAN_POINT('Ctrl Pts',(-1.62976666435367,41.4380444185006,14.7822644022364));
#62350=CARTESIAN_POINT('Ctrl Pts',(-1.69765987755627,41.45196673785,14.6938022668145));
#62351=CARTESIAN_POINT('Ctrl Pts',(-1.71610060763517,41.4557482311847,14.6697747346862));
#62352=CARTESIAN_POINT('Ctrl Pts',(-1.73403715537414,41.4595273060083,14.6453803408061));
#62353=CARTESIAN_POINT('Ctrl Pts',(-1.75145650730607,41.4633038406332,14.6206420253425));
#62354=CARTESIAN_POINT('Ctrl Pts',(-1.79941698135957,41.4737017240676,14.552530344635));
#62355=CARTESIAN_POINT('Ctrl Pts',(-1.84345465993251,41.4840795024122,14.4818155892012));
#62356=CARTESIAN_POINT('Ctrl Pts',(-1.88341683573492,41.4943720001996,14.4090078495041));
#62357=CARTESIAN_POINT('Ctrl Pts',(-1.89134100977552,41.4964129186967,14.394570667612));
#62358=CARTESIAN_POINT('Ctrl Pts',(-1.89910502357148,41.498450504055,14.3800510525844));
#62359=CARTESIAN_POINT('Ctrl Pts',(-1.90670780596449,41.5004842780006,14.3654527697682));
#62360=CARTESIAN_POINT('Ctrl Pts',(-1.92203075343397,41.5045832262176,14.3360308148611));
#62361=CARTESIAN_POINT('Ctrl Pts',(-1.93667848735068,41.5086818513199,14.3062737320976));
#62362=CARTESIAN_POINT('Ctrl Pts',(-1.95062893794502,41.5127822756707,14.2762114621491));
#62363=CARTESIAN_POINT('Ctrl Pts',(-1.95303105473353,41.5134883244185,14.271035064236));
#62364=CARTESIAN_POINT('Ctrl Pts',(-1.95541249773989,41.5141944262844,14.2658496199283));
#62365=CARTESIAN_POINT('Ctrl Pts',(-1.95777318849794,41.5149005918288,14.2606553125988));
#62366=CARTESIAN_POINT('Ctrl Pts',(-1.98281014357756,41.522390024722,14.2055656576594));
#62367=CARTESIAN_POINT('Ctrl Pts',(-2.00550484535097,41.5298867889419,14.1494891022725));
#62368=CARTESIAN_POINT('Ctrl Pts',(-2.02573738634781,41.5374229399387,14.0926310802962));
#62369=CARTESIAN_POINT('Ctrl Pts',(-2.04854357092303,41.5459177133163,14.0285405370482));
#62370=CARTESIAN_POINT('Ctrl Pts',(-2.06822067624309,41.5544637764423,13.9634546675661));
#62371=CARTESIAN_POINT('Ctrl Pts',(-2.08482135703504,41.5629839304559,13.8977113934608));
#62372=CARTESIAN_POINT('Ctrl Pts',(-2.09159121163654,41.566458499034,13.8709009022348));
#62373=CARTESIAN_POINT('Ctrl Pts',(-2.09784959854094,41.5699288335508,13.8439805042489));
#62374=CARTESIAN_POINT('Ctrl Pts',(-2.10360055620429,41.5733900089782,13.8169706884938));
#62375=CARTESIAN_POINT('Ctrl Pts',(-2.1236059163137,41.5854301012344,13.723013973404));
#62376=CARTESIAN_POINT('Ctrl Pts',(-2.13742420412686,41.5973875232401,13.6279516650221));
#62377=CARTESIAN_POINT('Ctrl Pts',(-2.14468551498309,41.6093217191047,13.5326515650383));
#62378=CARTESIAN_POINT('Ctrl Pts',(-2.1457745351032,41.6111115583873,13.5183588666006));
#62379=CARTESIAN_POINT('Ctrl Pts',(-2.14671605313871,41.6129008236976,13.5040612353341));
#62380=CARTESIAN_POINT('Ctrl Pts',(-2.14750923793178,41.6146894540213,13.4897620970082));
#62381=CARTESIAN_POINT('Ctrl Pts',(-2.14751278765176,41.6146974586337,13.4896981044337));
#62382=CARTESIAN_POINT('Ctrl Pts',(-2.14751633446029,41.6147054632175,13.4896341117367));
#62383=CARTESIAN_POINT('Ctrl Pts',(-2.14751987835732,41.6147134677728,13.4895701189175));
#62384=CARTESIAN_POINT('Ctrl Pts',(-2.15201532684852,41.6248672803339,13.4083949548605));
#62385=CARTESIAN_POINT('Ctrl Pts',(-2.15182151215461,41.6349749615117,13.327024578324));
#62386=CARTESIAN_POINT('Ctrl Pts',(-2.147149080938,41.6450029527301,13.246018671873));
#62387=CARTESIAN_POINT('Ctrl Pts',(-2.14333727732236,41.6531838614287,13.1799334599599));
#62388=CARTESIAN_POINT('Ctrl Pts',(-2.13654599047871,41.6613117860843,13.1140907826608));
#62389=CARTESIAN_POINT('Ctrl Pts',(-2.12691228998368,41.6693699018129,13.0487826967084));
#62390=CARTESIAN_POINT('Ctrl Pts',(-2.11564878821672,41.6787912659911,12.9724259797956));
#62391=CARTESIAN_POINT('Ctrl Pts',(-2.10033681376959,41.6881990268741,12.8967983660334));
#62392=CARTESIAN_POINT('Ctrl Pts',(-2.08102619939381,41.6976521858791,12.8223395356854));
#62393=CARTESIAN_POINT('Ctrl Pts',(-2.06921096952788,41.7034361161275,12.7767817828873));
#62394=CARTESIAN_POINT('Ctrl Pts',(-2.05589880879169,41.7092369106262,12.7316625943557));
#62395=CARTESIAN_POINT('Ctrl Pts',(-2.04110298493506,41.7150668347247,12.6870920669858));
#62396=CARTESIAN_POINT('Ctrl Pts',(-2.01561930883787,41.7251080395158,12.6103257514374));
#62397=CARTESIAN_POINT('Ctrl Pts',(-1.9857256496552,41.7352391333325,12.5351627453933));
#62398=CARTESIAN_POINT('Ctrl Pts',(-1.9517297894167,41.7454027323094,12.4620609055182));
#62399=CARTESIAN_POINT('Ctrl Pts',(-1.92355032332468,41.7538274284557,12.4014661506399));
#62400=CARTESIAN_POINT('Ctrl Pts',(-1.89255229461433,41.7622745755602,12.3422865252118));
#62401=CARTESIAN_POINT('Ctrl Pts',(-1.85889837851605,41.7707149892952,12.2847589717646));
#62402=CARTESIAN_POINT('Ctrl Pts',(-1.81950911849044,41.7805938292602,12.2174274982222));
#62403=CARTESIAN_POINT('Ctrl Pts',(-1.77648736441405,41.7904611540848,12.1523692608652));
#62404=CARTESIAN_POINT('Ctrl Pts',(-1.73011822727339,41.8002681947985,12.0899959420359));
#62405=CARTESIAN_POINT('Ctrl Pts',(-1.72435025841091,41.8014881162582,12.0822371743934));
#62406=CARTESIAN_POINT('Ctrl Pts',(-1.71853048361876,41.8027071123791,12.0745198867226));
#62407=CARTESIAN_POINT('Ctrl Pts',(-1.71265944073235,41.8039250956661,12.0668448162017));
#62408=CARTESIAN_POINT('Ctrl Pts',(-1.69565312410084,41.807453158709,12.0446128751355));
#62409=CARTESIAN_POINT('Ctrl Pts',(-1.6782168963213,41.8109727231298,12.0227358723218));
#62410=CARTESIAN_POINT('Ctrl Pts',(-1.66036526887978,41.8144806926752,12.0012284753065));
#62411=CARTESIAN_POINT('Ctrl Pts',(-1.6603632194742,41.8144810953977,12.0012260062107));
#62412=CARTESIAN_POINT('Ctrl Pts',(-1.66036117006314,41.8144814981201,12.0012235371197));
#62413=CARTESIAN_POINT('Ctrl Pts',(-1.66035912064661,41.8144819008423,12.0012210680335));
#62414=CARTESIAN_POINT('Ctrl Pts',(-1.60821266638108,41.8247289809986,11.9383963154232));
#62415=CARTESIAN_POINT('Ctrl Pts',(-1.55247647132068,41.83488619402,11.8786714244548));
#62416=CARTESIAN_POINT('Ctrl Pts',(-1.49354549202297,41.8450014026924,11.822404207685));
#62417=CARTESIAN_POINT('Ctrl Pts',(-1.4883815886577,41.8458877609495,11.8174737199603));
#62418=CARTESIAN_POINT('Ctrl Pts',(-1.48319317620903,41.8467737926257,11.8125698063066));
#62419=CARTESIAN_POINT('Ctrl Pts',(-1.47798053339602,41.8476595275812,11.8076927213209));
#62420=CARTESIAN_POINT('Ctrl Pts',(-1.42309820539036,41.8569851610647,11.7563433794429));
#62421=CARTESIAN_POINT('Ctrl Pts',(-1.36553232159843,41.8662768706289,11.7079683961237));
#62422=CARTESIAN_POINT('Ctrl Pts',(-1.30561140899485,41.875578475886,11.6629071708844));
#62423=CARTESIAN_POINT('Ctrl Pts',(-1.27274558510597,41.8806802827007,11.6381916879489));
#62424=CARTESIAN_POINT('Ctrl Pts',(-1.23917201965742,41.8857849530133,11.6144736420939));
#62425=CARTESIAN_POINT('Ctrl Pts',(-1.20495077659448,41.890898885685,11.5918121276779));
#62426=CARTESIAN_POINT('Ctrl Pts',(-1.15638684658384,41.8981561518192,11.5596527990992));
#62427=CARTESIAN_POINT('Ctrl Pts',(-1.10651335019658,41.905433193919,11.5296178064519));
#62428=CARTESIAN_POINT('Ctrl Pts',(-1.0555248004714,41.9127118485166,11.5017548784269));
#62429=CARTESIAN_POINT('Ctrl Pts',(-1.05549913535242,41.912715512232,11.5017408536043));
#62430=CARTESIAN_POINT('Ctrl Pts',(-1.0554734699505,41.9127191759479,11.5017268293321));
#62431=CARTESIAN_POINT('Ctrl Pts',(-1.05544780426564,41.9127228396642,11.5017128056101));
#62432=CARTESIAN_POINT('Ctrl Pts',(-0.974974870225346,41.9242101623427,
11.4577424201886));
#62433=CARTESIAN_POINT('Ctrl Pts',(-0.89180778368217,41.9356890569172,11.4192251624486));
#62434=CARTESIAN_POINT('Ctrl Pts',(-0.806686485525665,41.9471334535082,
11.386287900019));
#62435=CARTESIAN_POINT('Ctrl Pts',(-0.789077040580342,41.9495010098786,
11.37947401299));
#62436=CARTESIAN_POINT('Ctrl Pts',(-0.771383784061609,41.9518671099596,
11.372898926669));
#62437=CARTESIAN_POINT('Ctrl Pts',(-0.753612990007207,41.9542315545212,
11.3665637686692));
#62438=CARTESIAN_POINT('Ctrl Pts',(-0.66263533706061,41.9663363381385,11.3341309013419));
#62439=CARTESIAN_POINT('Ctrl Pts',(-0.569629829803022,41.9783966846349,
11.3079860838203));
#62440=CARTESIAN_POINT('Ctrl Pts',(-0.475465072600727,41.9903866688685,
11.2883103668133));
#62441=CARTESIAN_POINT('Ctrl Pts',(-0.459458822915358,41.99242474221,11.2849658624731));
#62442=CARTESIAN_POINT('Ctrl Pts',(-0.443418960303733,41.9944607979775,
11.2818082466664));
#62443=CARTESIAN_POINT('Ctrl Pts',(-0.427349602979368,41.9964947278661,
11.2788383836326));
#62444=CARTESIAN_POINT('Ctrl Pts',(-0.390917916437925,42.0011059574662,
11.2721052506931));
#62445=CARTESIAN_POINT('Ctrl Pts',(-0.354335452180833,42.0057062529319,
11.2663376977822));
#62446=CARTESIAN_POINT('Ctrl Pts',(-0.317651724132881,42.0102945165577,
11.2615471228867));
#62447=CARTESIAN_POINT('Ctrl Pts',(-0.317649527816609,42.0102947912647,
11.2615468360669));
#62448=CARTESIAN_POINT('Ctrl Pts',(-0.317647331499938,42.0102950659717,
11.2615465492507));
#62449=CARTESIAN_POINT('Ctrl Pts',(-0.317645135182867,42.0102953406786,
11.2615462624379));
#62450=CARTESIAN_POINT('Ctrl Pts',(-0.249506701873501,42.0188178357928,
11.252648197594));
#62451=CARTESIAN_POINT('Ctrl Pts',(-0.180978975914568,42.0273035867772,
11.2471157665343));
#62452=CARTESIAN_POINT('Ctrl Pts',(-0.112414609941067,42.0357869027238,
11.2450258022412));
#62453=CARTESIAN_POINT('Ctrl Pts',(-0.0766654418275343,42.0402100674921,
11.2439361037687));
#62454=CARTESIAN_POINT('Ctrl Pts',(-0.040907166826984,42.0446324668788,
11.2437821724988));
#62455=CARTESIAN_POINT('Ctrl Pts',(-0.00519524463400642,42.0490582852264,
11.2445737716325));
#62456=CARTESIAN_POINT('Ctrl Pts',(0.031375385536169,42.0535905242114,11.2453844050956));
#62457=CARTESIAN_POINT('Ctrl Pts',(0.0678999347651532,42.0581266875243,
11.2471866328337));
#62458=CARTESIAN_POINT('Ctrl Pts',(0.104323051734636,42.0626716287559,11.2499903668977));
#62459=CARTESIAN_POINT('Ctrl Pts',(0.178549888398028,42.0719337852793,11.2557041093705));
#62460=CARTESIAN_POINT('Ctrl Pts',(0.252359763212599,42.0812335714815,11.2655798042766));
#62461=CARTESIAN_POINT('Ctrl Pts',(0.325315592533385,42.0905367642454,11.2794198507996));
#62462=CARTESIAN_POINT('Ctrl Pts',(0.354711087375632,42.094285223518,11.2849963074031));
#62463=CARTESIAN_POINT('Ctrl Pts',(0.383968515541066,42.0980343105421,11.2912164383134));
#62464=CARTESIAN_POINT('Ctrl Pts',(0.413061600809365,42.1017820899529,11.2980678380498));
#62465=CARTESIAN_POINT('Ctrl Pts',(0.482481934639655,42.1107248368437,11.3144162745432));
#62466=CARTESIAN_POINT('Ctrl Pts',(0.550962843439977,42.1196590721596,11.3343571753581));
#62467=CARTESIAN_POINT('Ctrl Pts',(0.618117926916335,42.1285530190561,11.3577013517488));
#62468=CARTESIAN_POINT('Ctrl Pts',(0.643243679210771,42.1318806466172,11.3664354633476));
#62469=CARTESIAN_POINT('Ctrl Pts',(0.668184354966428,42.1352026955231,11.3756459489252));
#62470=CARTESIAN_POINT('Ctrl Pts',(0.692921584537619,42.1385177210261,11.3853229296319));
#62471=CARTESIAN_POINT('Ctrl Pts',(0.692939560513565,42.1385201299789,11.3853299616713));
#62472=CARTESIAN_POINT('Ctrl Pts',(0.69295753638213,42.138522538928,11.385336993957));
#62473=CARTESIAN_POINT('Ctrl Pts',(0.692975512143297,42.1385249478734,11.3853440264891));
#62474=CARTESIAN_POINT('Ctrl Pts',(0.763650395731234,42.1479961426866,11.4129936697879));
#62475=CARTESIAN_POINT('Ctrl Pts',(0.83277045242766,42.1574232662154,11.4444904798113));
#62476=CARTESIAN_POINT('Ctrl Pts',(0.899894377043377,42.1668266383785,11.4796363913641));
#62477=CARTESIAN_POINT('Ctrl Pts',(0.947822006023835,42.1735408067585,11.5047311726768));
#62478=CARTESIAN_POINT('Ctrl Pts',(0.994731099116168,42.1802427486524,11.53168562757));
#62479=CARTESIAN_POINT('Ctrl Pts',(1.04045131454124,42.1869380742162,11.5604147064339));
#62480=CARTESIAN_POINT('Ctrl Pts',(1.10548782309154,42.1964621019189,11.601281508259));
#62481=CARTESIAN_POINT('Ctrl Pts',(1.16811995715933,42.2059740216997,11.6457435079751));
#62482=CARTESIAN_POINT('Ctrl Pts',(1.22789007894113,42.2154964115977,11.693577895516));
#62483=CARTESIAN_POINT('Ctrl Pts',(1.26131603094944,42.2208217303062,11.7203288857202));
#62484=CARTESIAN_POINT('Ctrl Pts',(1.29384607028539,42.2261502030454,11.7481341423429));
#62485=CARTESIAN_POINT('Ctrl Pts',(1.3253946185824,42.2314848597499,11.7769503010397));
#62486=CARTESIAN_POINT('Ctrl Pts',(1.37375156243058,42.239661708088,11.8211190962217));
#62487=CARTESIAN_POINT('Ctrl Pts',(1.41981048771004,42.2478544794227,11.8676700248371));
#62488=CARTESIAN_POINT('Ctrl Pts',(1.46342795372799,42.2560397529707,11.9163149769343));
#62489=CARTESIAN_POINT('Ctrl Pts',(1.47943059990831,42.2590428168448,11.934162138357));
#62490=CARTESIAN_POINT('Ctrl Pts',(1.49510493384772,42.2620449351324,11.9522915536643));
#62491=CARTESIAN_POINT('Ctrl Pts',(1.51044488246768,42.2650451729185,11.9706904195566));
#62492=CARTESIAN_POINT('Ctrl Pts',(1.51049483357141,42.2650549425203,11.9707503313387));
#62493=CARTESIAN_POINT('Ctrl Pts',(1.51054478112997,42.2650647121022,11.9708102459786));
#62494=CARTESIAN_POINT('Ctrl Pts',(1.51059472514333,42.2650744816642,11.9708701634757));
#62495=CARTESIAN_POINT('Ctrl Pts',(1.59683622386887,42.2819442047123,12.074333509788));
#62496=CARTESIAN_POINT('Ctrl Pts',(1.67243490577711,42.2987396556532,12.1862255054654));
#62497=CARTESIAN_POINT('Ctrl Pts',(1.73631215842149,42.3154757047293,12.3041221328013));
#62498=CARTESIAN_POINT('Ctrl Pts',(1.79428034222021,42.3306635584449,12.4111125414325));
#62499=CARTESIAN_POINT('Ctrl Pts',(1.84259533597738,42.3458027937175,12.5230481751928));
#62500=CARTESIAN_POINT('Ctrl Pts',(1.88042817925358,42.3609092433609,12.6381457050623));
#62501=CARTESIAN_POINT('Ctrl Pts',(1.88540868050647,42.3628979305665,12.6532977090376));
#62502=CARTESIAN_POINT('Ctrl Pts',(1.89020746677454,42.3648860410024,12.6685044613407));
#62503=CARTESIAN_POINT('Ctrl Pts',(1.89482259963009,42.3668736029749,12.6837618462973));
#62504=CARTESIAN_POINT('Ctrl Pts',(1.91305124808663,42.3747239877019,12.7440247933123));
#62505=CARTESIAN_POINT('Ctrl Pts',(1.92841526796983,42.3825660203068,12.8050790443732));
#62506=CARTESIAN_POINT('Ctrl Pts',(1.94079431330655,42.3904018914181,12.8666749392279));
#62507=CARTESIAN_POINT('Ctrl Pts',(1.94080538279298,42.3904088983452,12.866730018994));
#62508=CARTESIAN_POINT('Ctrl Pts',(1.9408164498923,42.3904159052674,12.866785099193));
#62509=CARTESIAN_POINT('Ctrl Pts',(1.94082751460454,42.3904229121846,12.8668401798248));
#62510=CARTESIAN_POINT('Ctrl Pts',(1.94475934098526,42.3929128081224,12.8864129871634));
#62511=CARTESIAN_POINT('Ctrl Pts',(1.94838922236558,42.39540175289,12.9060378691002));
#62512=CARTESIAN_POINT('Ctrl Pts',(1.95171349888433,42.3978902143845,12.9257067365807));
#62513=CARTESIAN_POINT('Ctrl Pts',(1.96761896503129,42.4097966065981,13.0198151851698));
#62514=CARTESIAN_POINT('Ctrl Pts',(1.97652941610515,42.4216924760102,13.1149342117459));
#62515=CARTESIAN_POINT('Ctrl Pts',(1.97863244733539,42.4335719581307,13.2100822071488));
#62516=CARTESIAN_POINT('Ctrl Pts',(1.97948496302688,42.438387599843,13.2486527989349));
#62517=CARTESIAN_POINT('Ctrl Pts',(1.97921872054168,42.4432006194967,13.2872287404352));
#62518=CARTESIAN_POINT('Ctrl Pts',(1.97784553494189,42.4480109165588,13.3257469651751));
#62519=CARTESIAN_POINT('Ctrl Pts',(1.97429488067168,42.4604489306242,13.4253437707157));
#62520=CARTESIAN_POINT('Ctrl Pts',(1.96334565529604,42.4728680349482,13.5245510557992));
#62521=CARTESIAN_POINT('Ctrl Pts',(1.94519022359318,42.4852628635351,13.622239251103));
#62522=CARTESIAN_POINT('Ctrl Pts',(1.93863348315691,42.4897391918939,13.6575188385442));
#62523=CARTESIAN_POINT('Ctrl Pts',(1.93113692151219,42.4942124162428,13.6926007850153));
#62524=CARTESIAN_POINT('Ctrl Pts',(1.922709587364,42.4986824947968,13.7274335506639));
#62525=CARTESIAN_POINT('Ctrl Pts',(1.91286572512561,42.5039039369167,13.7681212628631));
#62526=CARTESIAN_POINT('Ctrl Pts',(1.90175154041046,42.5091209489411,13.8084675312016));
#62527=CARTESIAN_POINT('Ctrl Pts',(1.88938058275007,42.5143332820113,13.8483877905191));
#62528=CARTESIAN_POINT('Ctrl Pts',(1.88936713991042,42.5143389459671,13.8484311696705));
#62529=CARTESIAN_POINT('Ctrl Pts',(1.88935369558682,42.5143446099174,13.848474548319));
#62530=CARTESIAN_POINT('Ctrl Pts',(1.88934024977934,42.5143502738622,13.8485179264645));
#62531=CARTESIAN_POINT('Ctrl Pts',(1.87077278763808,42.5221716769888,13.9084192805149));
#62532=CARTESIAN_POINT('Ctrl Pts',(1.8493691554294,42.5299879209432,13.9674068716725));
#62533=CARTESIAN_POINT('Ctrl Pts',(1.82517111605764,42.5377988314389,14.0251660285722));
#62534=CARTESIAN_POINT('Ctrl Pts',(1.81388311926842,42.5414424957557,14.0521097477561));
#62535=CARTESIAN_POINT('Ctrl Pts',(1.80198745247787,42.5450849110612,14.0787855396012));
#62536=CARTESIAN_POINT('Ctrl Pts',(1.78949078968044,42.54872559605,14.1051584724611));
#62537=CARTESIAN_POINT('Ctrl Pts',(1.77448006045558,42.5530987104923,14.1368370862194));
#62538=CARTESIAN_POINT('Ctrl Pts',(1.75860107719396,42.5574696300421,14.1680808381114));
#62539=CARTESIAN_POINT('Ctrl Pts',(1.7418644439805,42.5618380058926,14.1988332167171));
#62540=CARTESIAN_POINT('Ctrl Pts',(1.71247101624427,42.5695098917641,14.2528415591798));
#62541=CARTESIAN_POINT('Ctrl Pts',(1.68042916372249,42.5771742446803,14.3053352714451));
#62542=CARTESIAN_POINT('Ctrl Pts',(1.6460207588783,42.5848284344902,14.3561499430919));
#62543=CARTESIAN_POINT('Ctrl Pts',(1.62916427312265,42.5885781794169,14.3810437675127));
#62544=CARTESIAN_POINT('Ctrl Pts',(1.61173942472271,42.592325583695,14.405535313502));
#62545=CARTESIAN_POINT('Ctrl Pts',(1.59377670300584,42.5960709051086,14.4296089222223));
#62546=CARTESIAN_POINT('Ctrl Pts',(1.55914873649875,42.6032910172114,14.4760172633198));
#62547=CARTESIAN_POINT('Ctrl Pts',(1.52271985975815,42.6105013040806,14.5209829604909));
#62548=CARTESIAN_POINT('Ctrl Pts',(1.48447273530543,42.617706601848,14.5642671857303));
#62549=CARTESIAN_POINT('Ctrl Pts',(1.46168436591892,42.6219996562779,14.5900567562531));
#62550=CARTESIAN_POINT('Ctrl Pts',(1.4382509215297,42.626290816224,14.6152484881778));
#62551=CARTESIAN_POINT('Ctrl Pts',(1.41417332299015,42.6305800124311,14.6397844353151));
#62552=CARTESIAN_POINT('Ctrl Pts',(1.40214956548563,42.6327219309865,14.6520370807788));
#62553=CARTESIAN_POINT('Ctrl Pts',(1.38996570285484,42.634863262063,14.6641256142807));
#62554=CARTESIAN_POINT('Ctrl Pts',(1.37762576359211,42.6370038984529,14.6760444996634));
#62555=CARTESIAN_POINT('Ctrl Pts',(1.31200813933492,42.6483867319751,14.7394231700081));
#62556=CARTESIAN_POINT('Ctrl Pts',(1.2418649492262,42.6597688584519,14.7981076923313));
#62557=CARTESIAN_POINT('Ctrl Pts',(1.16804459840713,42.6711396652326,14.8515972801294));
#62558=CARTESIAN_POINT('Ctrl Pts',(1.09738226872308,42.6820240309745,14.902798593124));
#62559=CARTESIAN_POINT('Ctrl Pts',(1.02335923147554,42.6928970547553,14.9492371895748));
#62560=CARTESIAN_POINT('Ctrl Pts',(0.946697171476419,42.7037561622759,14.9905293134562));
#62561=CARTESIAN_POINT('Ctrl Pts',(0.913311298611611,42.7084852392549,15.008511788728));
#62562=CARTESIAN_POINT('Ctrl Pts',(0.879424674105818,42.7132117248894,15.0255185420544));
#62563=CARTESIAN_POINT('Ctrl Pts',(0.84509668278392,42.7179354752911,15.0415187184684));
#62564=CARTESIAN_POINT('Ctrl Pts',(0.774769865368988,42.7276128936084,15.0742978424994));
#62565=CARTESIAN_POINT('Ctrl Pts',(0.702716449912161,42.7372903507808,15.1030452829988));
#62566=CARTESIAN_POINT('Ctrl Pts',(0.629302381291837,42.7469761521853,15.1274709114355));
#62567=CARTESIAN_POINT('Ctrl Pts',(0.608107942487717,42.7497724162937,15.1345225228894));
#62568=CARTESIAN_POINT('Ctrl Pts',(0.586800226012909,42.7525693460874,15.1412136224501));
#62569=CARTESIAN_POINT('Ctrl Pts',(0.565388389919398,42.7553670690054,15.1475365058111));
#62570=CARTESIAN_POINT('Ctrl Pts',(0.55718087964312,42.7564394823892,15.1499601713919));
#62571=CARTESIAN_POINT('Ctrl Pts',(0.548957102893311,42.7575118763432,15.1523278304504));
#62572=CARTESIAN_POINT('Ctrl Pts',(0.540717629607357,42.7585842514268,15.1546390187087));
#62573=CARTESIAN_POINT('Ctrl Pts',(0.540695318249796,42.7585871552707,15.1546452770878));
#62574=CARTESIAN_POINT('Ctrl Pts',(0.540673006777153,42.7585900591144,15.1546515350528));
#62575=CARTESIAN_POINT('Ctrl Pts',(0.54065069518942,42.758592962958,15.1546577926038));
#62576=CARTESIAN_POINT('Ctrl Pts',(0.49246290568457,42.7648645831174,15.1681726330802));
#62577=CARTESIAN_POINT('Ctrl Pts',(0.443780012972278,42.7711302171204,15.1797449878543));
#62578=CARTESIAN_POINT('Ctrl Pts',(0.394732848316695,42.7773801057318,15.1892846520821));
#62579=CARTESIAN_POINT('Ctrl Pts',(0.323682173577829,42.7864338156862,15.20310399485));
#62580=CARTESIAN_POINT('Ctrl Pts',(0.251860925182453,42.7954548674434,15.2126560886557));
#62581=CARTESIAN_POINT('Ctrl Pts',(0.179759012530397,42.8044535753376,15.218064782161));
#62582=CARTESIAN_POINT('Ctrl Pts',(0.142098641767993,42.8091537928937,15.2208898584351));
#62583=CARTESIAN_POINT('Ctrl Pts',(0.104360829440141,42.8138480236583,15.2225845865189));
#62584=CARTESIAN_POINT('Ctrl Pts',(0.0666098022250313,42.8185384501019,
15.2231662273549));
#62585=CARTESIAN_POINT('Ctrl Pts',(0.00168799995770721,42.826604745527,
15.2241664960661));
#62586=CARTESIAN_POINT('Ctrl Pts',(-0.0632696613322676,42.8346597279797,
15.2218763741639));
#62587=CARTESIAN_POINT('Ctrl Pts',(-0.127904922426963,42.8427160306386,
15.2164300042142));
#62588=CARTESIAN_POINT('Ctrl Pts',(-0.172040947023254,42.8482172565373,
15.2127109642663));
#62589=CARTESIAN_POINT('Ctrl Pts',(-0.216027677298764,42.8537192316855,
15.20752059654));
#62590=CARTESIAN_POINT('Ctrl Pts',(-0.259764820855651,42.8592277004498,
15.2009032833102));
#62591=CARTESIAN_POINT('Ctrl Pts',(-0.312212838029759,42.8658332590405,
15.1929680381227));
#62592=CARTESIAN_POINT('Ctrl Pts',(-0.364301538169402,42.8724449833506,
15.182955242973));
#62593=CARTESIAN_POINT('Ctrl Pts',(-0.415828148376253,42.879049848528,15.1707954835916));
#62594=CARTESIAN_POINT('Ctrl Pts',(-0.41587164670824,42.8790554242997,15.1707852184247));
#62595=CARTESIAN_POINT('Ctrl Pts',(-0.415915144672645,42.8790610000708,
15.1707749517203));
#62596=CARTESIAN_POINT('Ctrl Pts',(-0.415958642269399,42.8790665758413,
15.1707646834784));
#62597=CARTESIAN_POINT('Ctrl Pts',(-0.473867314471872,42.8864896402445,
15.157094497067));
#62598=CARTESIAN_POINT('Ctrl Pts',(-0.5311200159653,42.8939109955232,15.1406994155213));
#62599=CARTESIAN_POINT('Ctrl Pts',(-0.587498039973528,42.9013502931383,
15.1218310232062));
#62600=CARTESIAN_POINT('Ctrl Pts',(-0.614661409572605,42.9049346044765,
15.1127400853238));
#62601=CARTESIAN_POINT('Ctrl Pts',(-0.641622503810247,42.9085231761516,
15.1030749623491));
#62602=CARTESIAN_POINT('Ctrl Pts',(-0.668361108099995,42.9121187362383,
15.0928631758522));
#62603=CARTESIAN_POINT('Ctrl Pts',(-0.735732438505744,42.9211782093495,
15.0671332748199));
#62604=CARTESIAN_POINT('Ctrl Pts',(-0.801662743307208,42.930256284252,15.0377558250763));
#62605=CARTESIAN_POINT('Ctrl Pts',(-0.865742422457812,42.9393440302551,
15.0048247434824));
#62606=CARTESIAN_POINT('Ctrl Pts',(-0.865793964183904,42.9393513398753,
15.0047982557594));
#62607=CARTESIAN_POINT('Ctrl Pts',(-0.865845504710373,42.9393586495015,
15.0047717657375));
#62608=CARTESIAN_POINT('Ctrl Pts',(-0.865897044036977,42.9393659591336,
15.0047452734168));
#62609=CARTESIAN_POINT('Ctrl Pts',(-0.926015645569417,42.9478923581244,
14.9738430210856));
#62610=CARTESIAN_POINT('Ctrl Pts',(-0.984497013294306,42.9564230042295,
14.9397834670354));
#62611=CARTESIAN_POINT('Ctrl Pts',(-1.04094057269787,42.9649284253592,14.9026580519905));
#62612=CARTESIAN_POINT('Ctrl Pts',(-1.08152164931343,42.9710435454927,14.8759660905295));
#62613=CARTESIAN_POINT('Ctrl Pts',(-1.1210493387345,42.9771455625012,14.8476894911776));
#62614=CARTESIAN_POINT('Ctrl Pts',(-1.15937493671053,42.9832234671643,14.8178640118327));
#62615=CARTESIAN_POINT('Ctrl Pts',(-1.16231162737626,42.9836891852961,14.8155786409209));
#62616=CARTESIAN_POINT('Ctrl Pts',(-1.16524125182036,42.9841547599697,14.8132841750208));
#62617=CARTESIAN_POINT('Ctrl Pts',(-1.16816373353031,42.9846201857316,14.8109806493365));
#62618=CARTESIAN_POINT('Ctrl Pts',(-1.18014962096974,42.9865290225858,14.801533267862));
#62619=CARTESIAN_POINT('Ctrl Pts',(-1.19201536446151,42.9884353555117,14.7919334860694));
#62620=CARTESIAN_POINT('Ctrl Pts',(-1.2037547431206,42.9903387901022,14.7821837380565));
#62621=CARTESIAN_POINT('Ctrl Pts',(-1.22277701629086,42.9934230804889,14.7663854257755));
#62622=CARTESIAN_POINT('Ctrl Pts',(-1.24146787534786,42.996499826126,14.7501930759828));
#62623=CARTESIAN_POINT('Ctrl Pts',(-1.25981365272742,42.9995712552817,14.7336289146085));
#62624=CARTESIAN_POINT('Ctrl Pts',(-1.25992537907663,42.9995899603799,14.7335280383556));
#62625=CARTESIAN_POINT('Ctrl Pts',(-1.26003709263278,42.9996086652816,14.7334271483098));
#62626=CARTESIAN_POINT('Ctrl Pts',(-1.26014879339496,42.9996273699875,14.7333262444771));
#62627=CARTESIAN_POINT('Ctrl Pts',(-1.31609084749496,43.0089950739053,14.6827915162186));
#62628=CARTESIAN_POINT('Ctrl Pts',(-1.36878818457866,43.0183093018439,14.628856664969));
#62629=CARTESIAN_POINT('Ctrl Pts',(-1.41805397503608,43.0275946032795,14.5720258357116));
#62630=CARTESIAN_POINT('Ctrl Pts',(-1.43876420354246,43.0314979348346,14.54813543531));
#62631=CARTESIAN_POINT('Ctrl Pts',(-1.45886824080916,43.0353962218378,14.5237326689404));
#62632=CARTESIAN_POINT('Ctrl Pts',(-1.47835292496802,43.0392915793856,14.4988523605217));
#62633=CARTESIAN_POINT('Ctrl Pts',(-1.5252709700236,43.0486713855679,14.4389419497667));
#62634=CARTESIAN_POINT('Ctrl Pts',(-1.56859813794963,43.0580345049384,14.3762657123884));
#62635=CARTESIAN_POINT('Ctrl Pts',(-1.6081341418334,43.067409278086,14.3113441550447));
#62636=CARTESIAN_POINT('Ctrl Pts',(-1.62926440674908,43.0724196843151,14.276646422076));
#62637=CARTESIAN_POINT('Ctrl Pts',(-1.64931230767255,43.0774335321756,14.2413066347036));
#62638=CARTESIAN_POINT('Ctrl Pts',(-1.6682503056147,43.0824559227731,14.2053990062672));
#62639=CARTESIAN_POINT('Ctrl Pts',(-1.69949928782609,43.0907432082041,14.146148981756));
#62640=CARTESIAN_POINT('Ctrl Pts',(-1.72778401534493,43.0990713486404,14.0853959924843));
#62641=CARTESIAN_POINT('Ctrl Pts',(-1.75280261215093,43.1074088827253,14.0233804035923));
#62642=CARTESIAN_POINT('Ctrl Pts',(-1.76332832940544,43.1109166144761,13.9972894697517));
#62643=CARTESIAN_POINT('Ctrl Pts',(-1.77327566205206,43.1144259286465,13.9709756242431));
#62644=CARTESIAN_POINT('Ctrl Pts',(-1.78262119037841,43.1179341333482,13.944459332879));
#62645=CARTESIAN_POINT('Ctrl Pts',(-1.78263305732695,43.1179385880653,13.9444256625017));
#62646=CARTESIAN_POINT('Ctrl Pts',(-1.78264492337347,43.1179430428018,13.9443919917987));
#62647=CARTESIAN_POINT('Ctrl Pts',(-1.78265678851792,43.1179474975577,13.9443583207702));
#62648=CARTESIAN_POINT('Ctrl Pts',(-1.80401722676052,43.1259672515009,13.8837414501733));
#62649=CARTESIAN_POINT('Ctrl Pts',(-1.82245389414707,43.1340504487419,13.8220649991582));
#62650=CARTESIAN_POINT('Ctrl Pts',(-1.83781262195428,43.142160944959,13.7596376484174));
#62651=CARTESIAN_POINT('Ctrl Pts',(-1.8453470093919,43.1461396352241,13.7290132468987));
#62652=CARTESIAN_POINT('Ctrl Pts',(-1.85214072866539,43.1501248052658,13.6982089385095));
#62653=CARTESIAN_POINT('Ctrl Pts',(-1.85817623987287,43.1541116697546,13.6672656690419));
#62654=CARTESIAN_POINT('Ctrl Pts',(-1.87103315614179,43.1626045349232,13.60134995603));
#62655=CARTESIAN_POINT('Ctrl Pts',(-1.88042368888652,43.1710975472846,13.5347904585874));
#62656=CARTESIAN_POINT('Ctrl Pts',(-1.88619439323734,43.179549508963,13.4679553974391));
#62657=CARTESIAN_POINT('Ctrl Pts',(-1.88869853933062,43.1832171629495,13.4389529140169));
#62658=CARTESIAN_POINT('Ctrl Pts',(-1.89052098216898,43.1868770013553,13.4098991996398));
#62659=CARTESIAN_POINT('Ctrl Pts',(-1.89164915444521,43.190525266468,13.3808273721726));
#62660=CARTESIAN_POINT('Ctrl Pts',(-1.89269316585455,43.1939013735414,13.353924282808));
#62661=CARTESIAN_POINT('Ctrl Pts',(-1.89314293463907,43.1972678116781,13.3270043227245));
#62662=CARTESIAN_POINT('Ctrl Pts',(-1.89298914402905,43.2006220825191,13.3000918639857));
#62663=CARTESIAN_POINT('Ctrl Pts',(-1.89264191636583,43.2081953382971,13.2393290504546));
#62664=CARTESIAN_POINT('Ctrl Pts',(-1.88921587375014,43.2157069487255,13.1785964328137));
#62665=CARTESIAN_POINT('Ctrl Pts',(-1.88282612266878,43.2232009630549,13.1181934879298));
#62666=CARTESIAN_POINT('Ctrl Pts',(-1.87889104701324,43.2278160901506,13.0809948310636));
#62667=CARTESIAN_POINT('Ctrl Pts',(-1.87383201706931,43.2324246738829,13.0439201696221));
#62668=CARTESIAN_POINT('Ctrl Pts',(-1.86767488783895,43.2370382462145,13.0070297509779));
#62669=CARTESIAN_POINT('Ctrl Pts',(-1.86766817257427,43.2370432780009,13.0069895164927));
#62670=CARTESIAN_POINT('Ctrl Pts',(-1.86766145600323,43.2370483097934,13.0069492822259));
#62671=CARTESIAN_POINT('Ctrl Pts',(-1.86765473812588,43.2370533415919,13.0069090481776));
#62672=CARTESIAN_POINT('Ctrl Pts',(-1.85150139867034,43.2491524534186,12.9101650610084));
#62673=CARTESIAN_POINT('Ctrl Pts',(-1.82779225177506,43.2612687901266,12.8147726777807));
#62674=CARTESIAN_POINT('Ctrl Pts',(-1.79706272814456,43.2734283523782,12.7217319802806));
#62675=CARTESIAN_POINT('Ctrl Pts',(-1.76578946767481,43.2858030693463,12.6270449944947));
#62676=CARTESIAN_POINT('Ctrl Pts',(-1.72724459925867,43.2982226939109,12.534792539745));
#62677=CARTESIAN_POINT('Ctrl Pts',(-1.68194441752588,43.3107058267891,12.446038338779));
#62678=CARTESIAN_POINT('Ctrl Pts',(-1.63731684090383,43.3230036134137,12.3586019367024));
#62679=CARTESIAN_POINT('Ctrl Pts',(-1.58613233761101,43.3353632126334,12.2745597643092));
#62680=CARTESIAN_POINT('Ctrl Pts',(-1.52884857878348,43.3477916956768,12.1949531992576));
#62681=CARTESIAN_POINT('Ctrl Pts',(-1.51695804136936,43.3503715079246,12.1784290594398));
#62682=CARTESIAN_POINT('Ctrl Pts',(-1.5048046046168,43.3529542449554,12.1620961448403));
#62683=CARTESIAN_POINT('Ctrl Pts',(-1.49239220489772,43.355539897961,12.145963956135));
#62684=CARTESIAN_POINT('Ctrl Pts',(-1.49236250936106,43.3555460839005,12.1459253613418));
#62685=CARTESIAN_POINT('Ctrl Pts',(-1.49233281234219,43.3555522698567,12.1458867676974));
#62686=CARTESIAN_POINT('Ctrl Pts',(-1.49230311384122,43.3555584558296,12.145848175202));
#62687=CARTESIAN_POINT('Ctrl Pts',(-1.4545347737477,43.3634253150821,12.0967691158786));
#62688=CARTESIAN_POINT('Ctrl Pts',(-1.41435409216997,43.3713267067413,12.0495178634875));
#62689=CARTESIAN_POINT('Ctrl Pts',(-1.37191233999428,43.3792042996883,12.004384183538));
#62690=CARTESIAN_POINT('Ctrl Pts',(-1.35676188097806,43.3820163690062,11.9882727853682));
#62691=CARTESIAN_POINT('Ctrl Pts',(-1.34132370425351,43.3848253487554,11.9724314847919));
#62692=CARTESIAN_POINT('Ctrl Pts',(-1.32560608944061,43.3876283966831,11.9568742317137));
#62693=CARTESIAN_POINT('Ctrl Pts',(-1.282771636548,43.395267407172,11.9144768048746));
#62694=CARTESIAN_POINT('Ctrl Pts',(-1.23785644605668,43.4028629014454,11.8741844741578));
#62695=CARTESIAN_POINT('Ctrl Pts',(-1.19101162640978,43.4103642763285,11.8362520488016));
#62696=CARTESIAN_POINT('Ctrl Pts',(-1.14129719018095,43.418325169893,11.7959959616699));
#62697=CARTESIAN_POINT('Ctrl Pts',(-1.08940463871221,43.4261804547596,11.7583952441686));
#62698=CARTESIAN_POINT('Ctrl Pts',(-1.03570065855932,43.4339861919705,11.7235726644063));
#62699=CARTESIAN_POINT('Ctrl Pts',(-1.01736716360115,43.436650918931,11.7116849125361));
#62700=CARTESIAN_POINT('Ctrl Pts',(-0.998822227914527,43.4393099284136,
11.7001206320748));
#62701=CARTESIAN_POINT('Ctrl Pts',(-0.980079346897465,43.4419656268008,
11.6888838730866));
#62702=CARTESIAN_POINT('Ctrl Pts',(-0.927109714832717,43.4494709492919,
11.6571274430767));
#62703=CARTESIAN_POINT('Ctrl Pts',(-0.872562133097849,43.4569503499513,
11.6279886360763));
#62704=CARTESIAN_POINT('Ctrl Pts',(-0.816783143296509,43.4644537234662,
11.6015690506751));
#62705=CARTESIAN_POINT('Ctrl Pts',(-0.795010087872118,43.467382628561,11.5912562949354));
#62706=CARTESIAN_POINT('Ctrl Pts',(-0.773049086495344,43.4703152480498,
11.5813574036137));
#62707=CARTESIAN_POINT('Ctrl Pts',(-0.750919415419833,43.473254785114,11.5718767440723));
#62708=CARTESIAN_POINT('Ctrl Pts',(-0.685059041735581,43.4820031758537,
11.5436612419964));
#62709=CARTESIAN_POINT('Ctrl Pts',(-0.617659340501183,43.4908538709827,
11.5190612043455));
#62710=CARTESIAN_POINT('Ctrl Pts',(-0.549098729605882,43.4997554578476,
11.498242316879));
#62711=CARTESIAN_POINT('Ctrl Pts',(-0.524316113045828,43.5029731160797,
11.4907169098188));
#62712=CARTESIAN_POINT('Ctrl Pts',(-0.499382239716299,43.5061973623746,
11.4836857953846));
#62713=CARTESIAN_POINT('Ctrl Pts',(-0.474316482522037,43.5094255604747,
11.4771575059488));
#62714=CARTESIAN_POINT('Ctrl Pts',(-0.379305501034998,43.521661946056,11.4524122256878));
#62715=CARTESIAN_POINT('Ctrl Pts',(-0.282348593018896,43.5339000509646,
11.4349928797521));
#62716=CARTESIAN_POINT('Ctrl Pts',(-0.184667622219309,43.5461382098195,
11.4251095300764));
#62717=CARTESIAN_POINT('Ctrl Pts',(-0.090103312372126,43.5579858914758,
11.4155415238065));
#62718=CARTESIAN_POINT('Ctrl Pts',(0.00509447066960697,43.5699008208718,
11.4129073060295));
#62719=CARTESIAN_POINT('Ctrl Pts',(0.0999221662935547,43.5819092658192,
11.4173630715372));
#62720=CARTESIAN_POINT('Ctrl Pts',(0.124869565019585,43.5850684637963,11.4185353003678));
#62721=CARTESIAN_POINT('Ctrl Pts',(0.149793319885776,43.5882296589615,11.420206805125));
#62722=CARTESIAN_POINT('Ctrl Pts',(0.174675120256322,43.5913923188329,11.4223828576123));
#62723=CARTESIAN_POINT('Ctrl Pts',(0.174677432364299,43.5913926127188,11.4223830598191));
#62724=CARTESIAN_POINT('Ctrl Pts',(0.174679744471885,43.5913929066048,11.4223832620302));
#62725=CARTESIAN_POINT('Ctrl Pts',(0.174682056579137,43.5913932004907,11.4223834642457));
#62726=CARTESIAN_POINT('Ctrl Pts',(0.234958923058415,43.5990548367109,11.4276552418788));
#62727=CARTESIAN_POINT('Ctrl Pts',(0.29495787247848,43.6067330495829,11.4358646026484));
#62728=CARTESIAN_POINT('Ctrl Pts',(0.354406667102056,43.6143454706655,11.447047761332));
#62729=CARTESIAN_POINT('Ctrl Pts',(0.365055960100978,43.615709113159,11.4490510438919));
#62730=CARTESIAN_POINT('Ctrl Pts',(0.375687467747781,43.6170706274019,11.4511497267115));
#62731=CARTESIAN_POINT('Ctrl Pts',(0.386299455019993,43.6184295176617,11.453343977426));
#62732=CARTESIAN_POINT('Ctrl Pts',(0.461063654739058,43.6280032516072,11.4688030422023));
#62733=CARTESIAN_POINT('Ctrl Pts',(0.534875685874753,43.6374476583003,11.4890101183549));
#62734=CARTESIAN_POINT('Ctrl Pts',(0.607241015825486,43.646826890073,11.5136655931181));
#62735=CARTESIAN_POINT('Ctrl Pts',(0.622938784997419,43.648861469553,11.519013954715));
#62736=CARTESIAN_POINT('Ctrl Pts',(0.638568648006123,43.6508930066079,11.52457173361));
#62737=CARTESIAN_POINT('Ctrl Pts',(0.654125826897278,43.6529221965091,11.5303360412774));
#62738=CARTESIAN_POINT('Ctrl Pts',(0.731711944031748,43.6630420881976,11.5590835573286));
#62739=CARTESIAN_POINT('Ctrl Pts',(0.807507317384714,43.673216934486,11.5927719803986));
#62740=CARTESIAN_POINT('Ctrl Pts',(0.880908242422253,43.683511395425,11.6310579954211));
#62741=CARTESIAN_POINT('Ctrl Pts',(0.890693352786457,43.6848837546477,11.6361619213214));
#62742=CARTESIAN_POINT('Ctrl Pts',(0.90043598292481,43.6862582489024,11.641347572303));
#62743=CARTESIAN_POINT('Ctrl Pts',(0.910134769176067,43.6876350399056,11.6466141550489));
#62744=CARTESIAN_POINT('Ctrl Pts',(0.942442438941816,43.6922212745041,11.6641576921204));
#62745=CARTESIAN_POINT('Ctrl Pts',(0.974252312453001,43.6968083379815,11.6826381668839));
#62746=CARTESIAN_POINT('Ctrl Pts',(1.00549856845552,43.7013948596203,11.7020274023685));
#62747=CARTESIAN_POINT('Ctrl Pts',(1.02334506020761,43.7040144797307,11.7131016837521));
#62748=CARTESIAN_POINT('Ctrl Pts',(1.04100765718223,43.7066339147091,11.7244723415158));
#62749=CARTESIAN_POINT('Ctrl Pts',(1.05847448231885,43.7092529340121,11.7361339149813));
#62750=CARTESIAN_POINT('Ctrl Pts',(1.1713629347562,43.7261797099836,11.8115029056946));
#62751=CARTESIAN_POINT('Ctrl Pts',(1.27630931051256,43.7431244522926,11.899183329826));
#62752=CARTESIAN_POINT('Ctrl Pts',(1.37069057407131,43.7600840387654,11.9970973873642));
#62753=CARTESIAN_POINT('Ctrl Pts',(1.42280016977232,43.7694477319502,12.0511575022575));
#62754=CARTESIAN_POINT('Ctrl Pts',(1.47169109919433,43.7788162229859,12.1083378898411));
#62755=CARTESIAN_POINT('Ctrl Pts',(1.51692754710015,43.7881900239829,12.1682924647015));
#62756=CARTESIAN_POINT('Ctrl Pts',(1.51696491775492,43.7881977678509,12.1683419942694));
#62757=CARTESIAN_POINT('Ctrl Pts',(1.51700228604121,43.7882055118733,12.168391525532));
#62758=CARTESIAN_POINT('Ctrl Pts',(1.5170396519587,43.7882132560502,12.1684410584893));
#62759=CARTESIAN_POINT('Ctrl Pts',(1.5515881248574,43.7953735106584,12.2142391586534));
#62760=CARTESIAN_POINT('Ctrl Pts',(1.58411479558681,43.8026662744911,12.261488956581));
#62761=CARTESIAN_POINT('Ctrl Pts',(1.61446369987685,43.8099901329818,12.3100982262894));
#62762=CARTESIAN_POINT('Ctrl Pts',(1.63930499134918,43.815984883294,12.3498860560424));
#62763=CARTESIAN_POINT('Ctrl Pts',(1.66268627178357,43.8220003399112,12.3905842036694));
#62764=CARTESIAN_POINT('Ctrl Pts',(1.68450524095631,43.8279775950811,12.4321225050557));
#62765=CARTESIAN_POINT('Ctrl Pts',(1.72480715082951,43.839018208285,12.50884807653));
#62766=CARTESIAN_POINT('Ctrl Pts',(1.75976124537238,43.8499005705538,12.5884996251357));
#62767=CARTESIAN_POINT('Ctrl Pts',(1.78917403748305,43.8606990979938,12.670275591883));
#62768=CARTESIAN_POINT('Ctrl Pts',(1.79842290822096,43.8640947016508,12.6959900953912));
#62769=CARTESIAN_POINT('Ctrl Pts',(1.80712391329608,43.8674820671572,12.7219150440391));
#62770=CARTESIAN_POINT('Ctrl Pts',(1.81527108401148,43.8708636484753,12.7480265615633));
#62771=CARTESIAN_POINT('Ctrl Pts',(1.84067427841761,43.8814075502329,12.8294432863479));
#62772=CARTESIAN_POINT('Ctrl Pts',(1.86069177781362,43.8918966301114,12.9126701156961));
#62773=CARTESIAN_POINT('Ctrl Pts',(1.87513134105699,43.902396414511,12.9969077356303));
#62774=CARTESIAN_POINT('Ctrl Pts',(1.88005393093667,43.9059758948286,13.0256251731586));
#62775=CARTESIAN_POINT('Ctrl Pts',(1.88432858222577,43.9095566713819,13.0544603891218));
#62776=CARTESIAN_POINT('Ctrl Pts',(1.88794859519248,43.9131415008686,13.0833827340923));
#62777=CARTESIAN_POINT('Ctrl Pts',(1.8944580868007,43.9195877256957,13.1353907693138));
#62778=CARTESIAN_POINT('Ctrl Pts',(1.89884935747155,43.9260462734384,13.1876769477747));
#62779=CARTESIAN_POINT('Ctrl Pts',(1.90108421850662,43.9325286885601,13.2400514451286));
#62780=CARTESIAN_POINT('Ctrl Pts',(1.9027099019481,43.9372441293677,13.2781497213826));
#62781=CARTESIAN_POINT('Ctrl Pts',(1.90319460241082,43.9419721741924,13.3162947414601));
#62782=CARTESIAN_POINT('Ctrl Pts',(1.90253324894795,43.9467224113686,13.3544102360176));
#62783=CARTESIAN_POINT('Ctrl Pts',(1.90253284706,43.9467252979689,13.3544333978501));
#62784=CARTESIAN_POINT('Ctrl Pts',(1.90253244474574,43.9467281845762,13.3544565596831));
#62785=CARTESIAN_POINT('Ctrl Pts',(1.90253204200516,43.9467310711905,13.3544797215166));
#62786=CARTESIAN_POINT('Ctrl Pts',(1.9012587208505,43.9558575096353,13.4277091264005));
#62787=CARTESIAN_POINT('Ctrl Pts',(1.8957235974073,43.9650542157224,13.5009454342743));
#62788=CARTESIAN_POINT('Ctrl Pts',(1.88602216453062,43.9742750416705,13.5736597120378));
#62789=CARTESIAN_POINT('Ctrl Pts',(1.88166260850638,43.9784186262132,13.6063355004188));
#62790=CARTESIAN_POINT('Ctrl Pts',(1.87646184173778,43.9825672206978,13.6389063657602));
#62791=CARTESIAN_POINT('Ctrl Pts',(1.87042863065913,43.9867175295375,13.671326662048));
#62792=CARTESIAN_POINT('Ctrl Pts',(1.87042710275171,43.986718580601,13.6713348724704));
#62793=CARTESIAN_POINT('Ctrl Pts',(1.87042557479108,43.9867196316647,13.671343082883));
#62794=CARTESIAN_POINT('Ctrl Pts',(1.87042404677724,43.9867206827286,13.6713512932859));
#62795=CARTESIAN_POINT('Ctrl Pts',(1.85566478271274,43.9968730320419,13.7506565333898));
#62796=CARTESIAN_POINT('Ctrl Pts',(1.83594055493716,44.0070483275033,13.8290544476903));
#62797=CARTESIAN_POINT('Ctrl Pts',(1.81128975971261,44.0171601272258,13.9059652444678));
#62798=CARTESIAN_POINT('Ctrl Pts',(1.80343449962244,44.0203823687834,13.9304737565432));
#62799=CARTESIAN_POINT('Ctrl Pts',(1.79507882153093,44.0235980767071,13.954831397821));
#62800=CARTESIAN_POINT('Ctrl Pts',(1.78622345395315,44.026804267668,13.9790197714345));
#62801=CARTESIAN_POINT('Ctrl Pts',(1.78622218841255,44.026804725872,13.9790232282497));
#62802=CARTESIAN_POINT('Ctrl Pts',(1.78622092286174,44.0268051840758,13.9790266850614));
#62803=CARTESIAN_POINT('Ctrl Pts',(1.78621965730073,44.0268056422794,13.9790301418696));
#62804=CARTESIAN_POINT('Ctrl Pts',(1.77544514018287,44.030706617887,14.008460125274));
#62805=CARTESIAN_POINT('Ctrl Pts',(1.76394558147227,44.0346018285825,14.0376304480357));
#62806=CARTESIAN_POINT('Ctrl Pts',(1.75172504237321,44.0384820425673,14.066506010278));
#62807=CARTESIAN_POINT('Ctrl Pts',(1.72456897088087,44.0471045237461,14.1306723147493));
#62808=CARTESIAN_POINT('Ctrl Pts',(1.69385165573129,44.0556523962681,14.1933854221277));
#62809=CARTESIAN_POINT('Ctrl Pts',(1.65982723199645,44.0642355969814,14.2543086369607));
#62810=CARTESIAN_POINT('Ctrl Pts',(1.62591803131924,44.0727897308504,14.3150255364965));
#62811=CARTESIAN_POINT('Ctrl Pts',(1.58881380009087,44.0814663514857,14.3739910087394));
#62812=CARTESIAN_POINT('Ctrl Pts',(1.54854748895314,44.0901513341039,14.4307802087173));
#62813=CARTESIAN_POINT('Ctrl Pts',(1.53320531004564,44.0934604665615,14.4524179014052));
#62814=CARTESIAN_POINT('Ctrl Pts',(1.51740463455968,44.0967706625248,14.4737385701792));
#62815=CARTESIAN_POINT('Ctrl Pts',(1.50115693587717,44.1000813952048,14.4947169239003));
#62816=CARTESIAN_POINT('Ctrl Pts',(1.49105654617142,44.1021395137687,14.5077581275876));
#62817=CARTESIAN_POINT('Ctrl Pts',(1.48078346323126,44.1041978305208,14.5206669950275));
#62818=CARTESIAN_POINT('Ctrl Pts',(1.4703404162355,44.1062562463378,14.5334377131575));
#62819=CARTESIAN_POINT('Ctrl Pts',(1.4232052948658,44.115546990639,14.5910788737574));
#62820=CARTESIAN_POINT('Ctrl Pts',(1.37249259276042,44.1248617293685,14.6460396110216));
#62821=CARTESIAN_POINT('Ctrl Pts',(1.31867707979036,44.1341873629787,14.6979414591855));
#62822=CARTESIAN_POINT('Ctrl Pts',(1.30299549290356,44.1369048086679,14.7130654131654));
#62823=CARTESIAN_POINT('Ctrl Pts',(1.28705071957,44.1396231789241,14.7279298312709));
#62824=CARTESIAN_POINT('Ctrl Pts',(1.2708551448673,44.1423421482867,14.742525868927));
#62825=CARTESIAN_POINT('Ctrl Pts',(1.21862685325978,44.1511104153811,14.7895958942277));
#62826=CARTESIAN_POINT('Ctrl Pts',(1.16379442317349,44.1598865918041,14.8338720179614));
#62827=CARTESIAN_POINT('Ctrl Pts',(1.10682778192858,44.1687765663926,14.8751740368781));
#62828=CARTESIAN_POINT('Ctrl Pts',(1.08652577629236,44.1719448120581,14.8898934200559));
#62829=CARTESIAN_POINT('Ctrl Pts',(1.06595249883986,44.1751275627198,14.9042354981446));
#62830=CARTESIAN_POINT('Ctrl Pts',(1.04512843756418,44.1783297805026,14.9181934971272));
#62831=CARTESIAN_POINT('Ctrl Pts',(0.964219328541589,44.1907715700402,14.9724254380762));
#62832=CARTESIAN_POINT('Ctrl Pts',(0.879289177392871,44.2032149235223,15.0206870131516));
#62833=CARTESIAN_POINT('Ctrl Pts',(0.791202840516241,44.2155622228643,15.0623301371084));
#62834=CARTESIAN_POINT('Ctrl Pts',(0.71580631198331,44.2261307575559,15.0979741097713));
#62835=CARTESIAN_POINT('Ctrl Pts',(0.638098070836109,44.2366277067109,15.1287706175789));
#62836=CARTESIAN_POINT('Ctrl Pts',(0.558565667470021,44.2470165405819,15.1543230267766));
#62837=CARTESIAN_POINT('Ctrl Pts',(0.545179759982402,44.2487650602194,15.1586236912999));
#62838=CARTESIAN_POINT('Ctrl Pts',(0.531742184172616,44.2505105119025,15.1627756845355));
#62839=CARTESIAN_POINT('Ctrl Pts',(0.518255278193969,44.2522527150447,15.1667769694065));
#62840=CARTESIAN_POINT('Ctrl Pts',(0.476730225248576,44.2576168124762,15.1790965901101));
#62841=CARTESIAN_POINT('Ctrl Pts',(0.434735080639449,44.2629511539096,15.1899888909904));
#62842=CARTESIAN_POINT('Ctrl Pts',(0.392363468462353,44.2682944556014,15.1994255958125));
#62843=CARTESIAN_POINT('Ctrl Pts',(0.392348669898505,44.2682963217846,15.1994288916437));
#62844=CARTESIAN_POINT('Ctrl Pts',(0.392333871288648,44.2682981879689,15.1994321872973));
#62845=CARTESIAN_POINT('Ctrl Pts',(0.3923190726328,44.2683000541543,15.1994354827733));
#62846=CARTESIAN_POINT('Ctrl Pts',(0.303463056846925,44.2795052475772,15.2192226091348));
#62847=CARTESIAN_POINT('Ctrl Pts',(0.213098743752062,44.2907005039032,15.2325524353331));
#62848=CARTESIAN_POINT('Ctrl Pts',(0.122100826373289,44.3019309442477,15.2395437326749));
#62849=CARTESIAN_POINT('Ctrl Pts',(0.0267244225314325,44.3137017522449,
15.246871425636));
#62850=CARTESIAN_POINT('Ctrl Pts',(-0.0693486369463793,44.3255114195325,
15.2472350622581));
#62851=CARTESIAN_POINT('Ctrl Pts',(-0.165101310109247,44.337394572606,15.240737448503));
#62852=CARTESIAN_POINT('Ctrl Pts',(-0.260764325483668,44.3492665989174,
15.234245918773));
#62853=CARTESIAN_POINT('Ctrl Pts',(-0.356107800931346,44.3612121177935,
15.2209050722059));
#62854=CARTESIAN_POINT('Ctrl Pts',(-0.450101264067399,44.3732463862623,
15.2007983539383));
#62855=CARTESIAN_POINT('Ctrl Pts',(-0.541034403506556,44.3848888321964,
15.181346288285));
#62856=CARTESIAN_POINT('Ctrl Pts',(-0.630703688762427,44.396614449005,15.1555612094307));
#62857=CARTESIAN_POINT('Ctrl Pts',(-0.718161474242711,44.4084172748796,
15.1235116420653));
#62858=CARTESIAN_POINT('Ctrl Pts',(-0.773397886299599,44.4158716798804,
15.1032698408406));
#62859=CARTESIAN_POINT('Ctrl Pts',(-0.827751833483358,44.423356480698,15.0805291321155));
#62860=CARTESIAN_POINT('Ctrl Pts',(-0.880982903069709,44.4308655889996,
15.0553060862276));
#62861=CARTESIAN_POINT('Ctrl Pts',(-0.880991504927449,44.4308668024315,
15.0553020103176));
#62862=CARTESIAN_POINT('Ctrl Pts',(-0.881000106756236,44.4308680158645,
15.0552979343428));
#62863=CARTESIAN_POINT('Ctrl Pts',(-0.881008708556081,44.4308692292984,
15.0552938583032));
#62864=CARTESIAN_POINT('Ctrl Pts',(-0.949777952894382,44.4405703311217,
15.022706938637));
#62865=CARTESIAN_POINT('Ctrl Pts',(-1.01670018024658,44.4503355641457,14.9859787929044));
#62866=CARTESIAN_POINT('Ctrl Pts',(-1.08130811717254,44.460002951837,14.9453570067032));
#62867=CARTESIAN_POINT('Ctrl Pts',(-1.08881927634195,44.4611268584522,14.9406344181728));
#62868=CARTESIAN_POINT('Ctrl Pts',(-1.09629911536165,44.4622494355331,14.935859244514));
#62869=CARTESIAN_POINT('Ctrl Pts',(-1.10374686948965,44.463370423022,14.9310319078346));
#62870=CARTESIAN_POINT('Ctrl Pts',(-1.11576672495049,44.4651795734527,14.923241117732));
#62871=CARTESIAN_POINT('Ctrl Pts',(-1.12770346753595,44.4669846854585,14.9153141979155));
#62872=CARTESIAN_POINT('Ctrl Pts',(-1.13955436632537,44.4687847978907,14.9072526043425));
#62873=CARTESIAN_POINT('Ctrl Pts',(-1.20881460051703,44.4793051989881,14.8601382150673));
#62874=CARTESIAN_POINT('Ctrl Pts',(-1.27514891107262,44.489653444563,14.8084199677914));
#62875=CARTESIAN_POINT('Ctrl Pts',(-1.33806632362854,44.4999383822885,14.752580101493));
#62876=CARTESIAN_POINT('Ctrl Pts',(-1.40200047511709,44.5103895235527,14.6958378686834));
#62877=CARTESIAN_POINT('Ctrl Pts',(-1.46240423535586,44.5207766906942,14.6348368848923));
#62878=CARTESIAN_POINT('Ctrl Pts',(-1.51870614782633,44.5312202034947,14.5701558030753));
#62879=CARTESIAN_POINT('Ctrl Pts',(-1.55879377509555,44.5386561080699,14.5241021081745));
#62880=CARTESIAN_POINT('Ctrl Pts',(-1.59680043494514,44.5461207607961,14.4761843015882));
#62881=CARTESIAN_POINT('Ctrl Pts',(-1.63251480183106,44.5536534130216,14.4266441099927));
#62882=CARTESIAN_POINT('Ctrl Pts',(-1.63252331082678,44.5536552076861,14.4266323069757));
#62883=CARTESIAN_POINT('Ctrl Pts',(-1.63253181969435,44.5536570023525,14.4266205038614));
#62884=CARTESIAN_POINT('Ctrl Pts',(-1.63254032843374,44.5536587970208,14.4266087006498));
#62885=CARTESIAN_POINT('Ctrl Pts',(-1.68445643326028,44.564608972198,14.3545913611944));
#62886=CARTESIAN_POINT('Ctrl Pts',(-1.73159885214559,44.5756300349953,14.2789488134197));
#62887=CARTESIAN_POINT('Ctrl Pts',(-1.77359830303046,44.5867104940924,14.2004365969182));
#62888=CARTESIAN_POINT('Ctrl Pts',(-1.81582089846807,44.5978498240565,14.1215072422621));
#62889=CARTESIAN_POINT('Ctrl Pts',(-1.852846965609,44.609048601566,14.0396788990061));
#62890=CARTESIAN_POINT('Ctrl Pts',(-1.88433431500624,44.6202898644539,13.9556864859498));
#62891=CARTESIAN_POINT('Ctrl Pts',(-1.91569856854481,44.6314871810289,13.8720224307389));
#62892=CARTESIAN_POINT('Ctrl Pts',(-1.94156907374052,44.6427262186232,13.7862116512348));
#62893=CARTESIAN_POINT('Ctrl Pts',(-1.96161764693458,44.6539925222584,13.69893534269));
#62894=CARTESIAN_POINT('Ctrl Pts',(-1.97620527972793,44.6621900482758,13.6354318340719));
#62895=CARTESIAN_POINT('Ctrl Pts',(-1.98771101076676,44.6704020473443,13.5711513935466));
#62896=CARTESIAN_POINT('Ctrl Pts',(-1.99600309484505,44.6786255226448,13.5063407137072));
#62897=CARTESIAN_POINT('Ctrl Pts',(-1.99600413073181,44.6786265499607,13.5063326172474));
#62898=CARTESIAN_POINT('Ctrl Pts',(-1.99600516656828,44.6786275772765,13.5063245207802));
#62899=CARTESIAN_POINT('Ctrl Pts',(-1.99600620235445,44.6786286045924,13.5063164243057));
#62900=CARTESIAN_POINT('Ctrl Pts',(-1.9989524566471,44.6815507655481,13.4832863110676));
#62901=CARTESIAN_POINT('Ctrl Pts',(-2.0014917701668,44.6844732366445,13.4601968132775));
#62902=CARTESIAN_POINT('Ctrl Pts',(-2.00362382472207,44.6873925139984,13.4370592699312));
#62903=CARTESIAN_POINT('Ctrl Pts',(-2.0138298820748,44.7013669744684,13.3263008027942));
#62904=CARTESIAN_POINT('Ctrl Pts',(-2.0147077970061,44.7152691479107,13.2144301717847));
#62905=CARTESIAN_POINT('Ctrl Pts',(-2.00640344852531,44.7291692282355,13.1029507560109));
#62906=CARTESIAN_POINT('Ctrl Pts',(-2.00589556393409,44.730019341478,13.096132800618));
#62907=CARTESIAN_POINT('Ctrl Pts',(-2.00535331908657,44.7308694478072,13.0893163022739));
#62908=CARTESIAN_POINT('Ctrl Pts',(-2.00477674144566,44.7317195636347,13.0825016027861));
#62909=CARTESIAN_POINT('Ctrl Pts',(-1.99472189986248,44.7465445921599,12.963661191844));
#62910=CARTESIAN_POINT('Ctrl Pts',(-1.97422402633385,44.7613736991323,12.8453705757279));
#62911=CARTESIAN_POINT('Ctrl Pts',(-1.94345486610982,44.776271931547,12.729580488958));
#62912=CARTESIAN_POINT('Ctrl Pts',(-1.92391562895981,44.7857327063665,12.6560506965118));
#62913=CARTESIAN_POINT('Ctrl Pts',(-1.90023477131147,44.7952208737969,12.583532124005));
#62914=CARTESIAN_POINT('Ctrl Pts',(-1.87247430467957,44.8047448794644,12.5125442365009));
#62915=CARTESIAN_POINT('Ctrl Pts',(-1.87247199884922,44.8047456705441,12.5125383401294));
#62916=CARTESIAN_POINT('Ctrl Pts',(-1.87246969299075,44.8047464616243,12.5125324437682));
#62917=CARTESIAN_POINT('Ctrl Pts',(-1.87246738710414,44.8047472527049,12.5125265474173));
#62918=CARTESIAN_POINT('Ctrl Pts',(-1.8417656413995,44.8152801017681,12.4340195367457));
#62919=CARTESIAN_POINT('Ctrl Pts',(-1.80607587860346,44.8258945414302,12.3573440782967));
#62920=CARTESIAN_POINT('Ctrl Pts',(-1.76571080889466,44.836476728865,12.2830640674007));
#62921=CARTESIAN_POINT('Ctrl Pts',(-1.71646942493366,44.8493859486034,12.1924498169226));
#62922=CARTESIAN_POINT('Ctrl Pts',(-1.66026211689408,44.8622489307279,12.1053787678795));
#62923=CARTESIAN_POINT('Ctrl Pts',(-1.59771604579451,44.8751219231574,12.022801987044));
#62924=CARTESIAN_POINT('Ctrl Pts',(-1.53522822528026,44.8879829266749,11.9403021118515));
#62925=CARTESIAN_POINT('Ctrl Pts',(-1.46640908545805,44.9008550726673,11.8622913408099));
#62926=CARTESIAN_POINT('Ctrl Pts',(-1.39195572467721,44.9137854253946,11.7898077068253));
#62927=CARTESIAN_POINT('Ctrl Pts',(-1.35621175803568,44.9199930981135,11.7550093771323));
#62928=CARTESIAN_POINT('Ctrl Pts',(-1.31917068762716,44.9262139460458,11.7214859910814));
#62929=CARTESIAN_POINT('Ctrl Pts',(-1.28091943577779,44.9324512723062,11.6893554841697));
#62930=CARTESIAN_POINT('Ctrl Pts',(-1.28091426683009,44.9324521151652,11.6893511423272));
#62931=CARTESIAN_POINT('Ctrl Pts',(-1.28090909786018,44.9324529580248,11.68934680051));
#62932=CARTESIAN_POINT('Ctrl Pts',(-1.28090392886803,44.9324538008848,11.689342458718));
#62933=CARTESIAN_POINT('Ctrl Pts',(-1.18903365872423,44.94743424159,11.6121743003787));
#62934=CARTESIAN_POINT('Ctrl Pts',(-1.09014141607981,44.9625752668603,11.5429731154381));
#62935=CARTESIAN_POINT('Ctrl Pts',(-0.985766402849624,44.9776815456083,
11.4826592838517));
#62936=CARTESIAN_POINT('Ctrl Pts',(-0.97325193505438,44.9794927744939,11.475427711087));
#62937=CARTESIAN_POINT('Ctrl Pts',(-0.960658680559212,44.9813034961629,
11.4683239524804));
#62938=CARTESIAN_POINT('Ctrl Pts',(-0.947989320712283,44.9831133677631,
11.4613496339711));
#62939=CARTESIAN_POINT('Ctrl Pts',(-0.937102327850855,44.9846686207064,
11.4553564854031));
#62940=CARTESIAN_POINT('Ctrl Pts',(-0.926158772207229,44.9862233275243,
11.4494587047961));
#62941=CARTESIAN_POINT('Ctrl Pts',(-0.915160127495719,44.9877773234709,
11.443657227826));
#62942=CARTESIAN_POINT('Ctrl Pts',(-0.803195994864283,45.0035967096614,
11.3845992844179));
#62943=CARTESIAN_POINT('Ctrl Pts',(-0.685498295157008,45.0193461150921,
11.3355123919204));
#62944=CARTESIAN_POINT('Ctrl Pts',(-0.564026643895891,45.0351569854134,
11.2974601095493));
#62945=CARTESIAN_POINT('Ctrl Pts',(-0.557153255633243,45.0360516324307,
11.2953069478173));
#62946=CARTESIAN_POINT('Ctrl Pts',(-0.550267782542978,45.0369464774048,
11.2931891028702));
#62947=CARTESIAN_POINT('Ctrl Pts',(-0.543370578909281,45.0378415445592,
11.2911067625676));
#62948=CARTESIAN_POINT('Ctrl Pts',(-0.481520058743433,45.0458680393563,
11.2724334222236));
#62949=CARTESIAN_POINT('Ctrl Pts',(-0.418731397380921,45.053911575045,11.2566180320663));
#62950=CARTESIAN_POINT('Ctrl Pts',(-0.355289380165877,45.0619836125773,
11.2437966393052));
#62951=CARTESIAN_POINT('Ctrl Pts',(-0.355285043067044,45.0619841644075,
11.2437957627938));
#62952=CARTESIAN_POINT('Ctrl Pts',(-0.355280705964929,45.0619847162379,
11.2437948862964));
#62953=CARTESIAN_POINT('Ctrl Pts',(-0.355276368859519,45.0619852680685,
11.243794009813));
#62954=CARTESIAN_POINT('Ctrl Pts',(-0.349648787210502,45.0627012920588,
11.242656734663));
#62955=CARTESIAN_POINT('Ctrl Pts',(-0.344015669854361,45.0634175707409,
11.2415429346111));
#62956=CARTESIAN_POINT('Ctrl Pts',(-0.338377233770639,45.0641340836512,
11.2404526226096));
#62957=CARTESIAN_POINT('Ctrl Pts',(-0.212337755202137,45.0801507436369,
11.2160801983943));
#62958=CARTESIAN_POINT('Ctrl Pts',(-0.083657625338293,45.0962819756428,
11.203452144954));
#62959=CARTESIAN_POINT('Ctrl Pts',(0.0454031143779827,45.1124275059506,
11.2026060087752));
#62960=CARTESIAN_POINT('Ctrl Pts',(0.122713040983513,45.1220989967994,11.2020991565285));
#62961=CARTESIAN_POINT('Ctrl Pts',(0.200163706613968,45.1317761380361,11.2058176283785));
#62962=CARTESIAN_POINT('Ctrl Pts',(0.277304443770296,45.141444268965,11.2137694907024));
#62963=CARTESIAN_POINT('Ctrl Pts',(0.392755226298408,45.1559138387731,11.2256704494137));
#62964=CARTESIAN_POINT('Ctrl Pts',(0.507541491897695,45.1703677451665,11.2470625359803));
#62965=CARTESIAN_POINT('Ctrl Pts',(0.619988601592955,45.1849028038661,11.2779180352251));
#62966=CARTESIAN_POINT('Ctrl Pts',(0.632706684454347,45.1865467596906,11.2814078785584));
#62967=CARTESIAN_POINT('Ctrl Pts',(0.645394870547359,45.1881917558853,11.2850187320195));
#62968=CARTESIAN_POINT('Ctrl Pts',(0.658050758780454,45.1898379341977,11.2887505194805));
#62969=CARTESIAN_POINT('Ctrl Pts',(0.666998222341376,45.191001749822,11.2913888196701));
#62970=CARTESIAN_POINT('Ctrl Pts',(0.675929375511245,45.1921661297048,11.2940875173707));
#62971=CARTESIAN_POINT('Ctrl Pts',(0.684843296158863,45.1933311104401,11.2968465526485));
#62972=CARTESIAN_POINT('Ctrl Pts',(0.684848158254035,45.1933317458784,11.2968480575634));
#62973=CARTESIAN_POINT('Ctrl Pts',(0.684853020344242,45.193332381317,11.2968495624963));
#62974=CARTESIAN_POINT('Ctrl Pts',(0.684857882429488,45.1933330167558,11.2968510674472));
#62975=CARTESIAN_POINT('Ctrl Pts',(0.775542254410143,45.2051847966284,11.3249204085195));
#62976=CARTESIAN_POINT('Ctrl Pts',(0.864500574667007,45.2171028831587,11.3592540114329));
#62977=CARTESIAN_POINT('Ctrl Pts',(0.950951991990921,45.2290358758107,11.3994507400536));
#62978=CARTESIAN_POINT('Ctrl Pts',(1.11212620474213,45.2512829453903,11.4743908195936));
#62979=CARTESIAN_POINT('Ctrl Pts',(1.26460168681221,45.2735846116156,11.5697127495115));
#62980=CARTESIAN_POINT('Ctrl Pts',(1.40341572670576,45.2959102457559,11.6827721945687));
#62981=CARTESIAN_POINT('Ctrl Pts',(1.44821014969757,45.3031145883427,11.7192557707905));
#62982=CARTESIAN_POINT('Ctrl Pts',(1.49158325573292,45.3103216000242,11.7575872908086));
#62983=CARTESIAN_POINT('Ctrl Pts',(1.53337112977183,45.3175309541919,11.7976817952021));
#62984=CARTESIAN_POINT('Ctrl Pts',(1.55105511791145,45.3205818424346,11.8146491752487));
#62985=CARTESIAN_POINT('Ctrl Pts',(1.56845528293424,45.3236331684876,11.8319323814174));
#62986=CARTESIAN_POINT('Ctrl Pts',(1.58555880455248,45.3266863052577,11.849524300512));
#62987=CARTESIAN_POINT('Ctrl Pts',(1.58556698423901,45.3266877654074,11.8495327137725));
#62988=CARTESIAN_POINT('Ctrl Pts',(1.58557516385734,45.3266892255575,11.8495411271033));
#62989=CARTESIAN_POINT('Ctrl Pts',(1.58558334340749,45.3266906857082,11.8495495405043));
#62990=CARTESIAN_POINT('Ctrl Pts',(1.67599372359701,45.3428300542994,11.9425447258912));
#62991=CARTESIAN_POINT('Ctrl Pts',(1.75807542442181,45.3590280166517,12.0441179598847));
#62992=CARTESIAN_POINT('Ctrl Pts',(1.8306691593267,45.3752881408786,12.1525001696805));
#62993=CARTESIAN_POINT('Ctrl Pts',(1.9033168266553,45.3915603453203,12.2609629004092));
#62994=CARTESIAN_POINT('Ctrl Pts',(1.96646025163579,45.4078950327212,12.3762469632662));
#62995=CARTESIAN_POINT('Ctrl Pts',(2.01889794999029,45.4242878521849,12.4965442673756));
#62996=CARTESIAN_POINT('Ctrl Pts',(2.05891676953857,45.436798341863,12.5883514262778));
#62997=CARTESIAN_POINT('Ctrl Pts',(2.09269894674285,45.4493425300974,12.6830775196885));
#62998=CARTESIAN_POINT('Ctrl Pts',(2.11970969578712,45.4619143413547,12.7798970723477));
#62999=CARTESIAN_POINT('Ctrl Pts',(2.11971337779344,45.4619160550979,12.7799102704343));
#63000=CARTESIAN_POINT('Ctrl Pts',(2.11971705967376,45.4619177688419,12.7799234685589));
#63001=CARTESIAN_POINT('Ctrl Pts',(2.1197207414281,45.4619194825866,12.7799366667217));
#63002=CARTESIAN_POINT('Ctrl Pts',(2.14488606212673,45.473633174392,12.8701480085141));
#63003=CARTESIAN_POINT('Ctrl Pts',(2.16416769647576,45.4853817456121,12.9621390488384));
#63004=CARTESIAN_POINT('Ctrl Pts',(2.17752086339295,45.4971268278867,13.0551903597028));
#63005=CARTESIAN_POINT('Ctrl Pts',(2.19789478370435,45.5150471738089,13.1971656681956));
#63006=CARTESIAN_POINT('Ctrl Pts',(2.20447572595291,45.5329691475165,13.3416848784884));
#63007=CARTESIAN_POINT('Ctrl Pts',(2.19698946825817,45.5509580385708,13.4860284921698));
#63008=CARTESIAN_POINT('Ctrl Pts',(2.1921617577059,45.5625586490103,13.5791122751943));
#63009=CARTESIAN_POINT('Ctrl Pts',(2.18147855175247,45.5741869045399,13.6721180984126));
#63010=CARTESIAN_POINT('Ctrl Pts',(2.16489369591591,45.5858440596454,13.7642000865692));
#63011=CARTESIAN_POINT('Ctrl Pts',(2.15857076358717,45.5902883191315,13.7993061004862));
#63012=CARTESIAN_POINT('Ctrl Pts',(2.1513905601623,45.5947367776815,13.8342778892848));
#63013=CARTESIAN_POINT('Ctrl Pts',(2.1433525037659,45.599189498898,13.8690689663171));
#63014=CARTESIAN_POINT('Ctrl Pts',(2.14335156752272,45.5991900175345,13.8690730186535));
#63015=CARTESIAN_POINT('Ctrl Pts',(2.14335063126784,45.5991905361712,13.8690770709878));
#63016=CARTESIAN_POINT('Ctrl Pts',(2.14334969500126,45.5991910548079,13.8690811233198));
#63017=CARTESIAN_POINT('Ctrl Pts',(2.12029927780217,45.6119596331554,13.9688475214958));
#63018=CARTESIAN_POINT('Ctrl Pts',(2.09015480355828,45.6247828779577,14.0672843773186));
#63019=CARTESIAN_POINT('Ctrl Pts',(2.05333535530513,45.6376364238151,14.1633752639895));
#63020=CARTESIAN_POINT('Ctrl Pts',(2.05017992087395,45.6387379753887,14.171610273114));
#63021=CARTESIAN_POINT('Ctrl Pts',(2.04697549230673,45.6398397493399,14.1798280608758));
#63022=CARTESIAN_POINT('Ctrl Pts',(2.04372235015577,45.6409417302387,14.1880279931464));
#63023=CARTESIAN_POINT('Ctrl Pts',(2.00503673649245,45.6540462320831,14.2855396901957));
#63024=CARTESIAN_POINT('Ctrl Pts',(1.95946432547649,45.667180363089,14.3805303543247));
#63025=CARTESIAN_POINT('Ctrl Pts',(1.90739615061957,45.6803410718172,14.4720865331734));
#63026=CARTESIAN_POINT('Ctrl Pts',(1.85220623644864,45.6942908287874,14.5691319484652));
#63027=CARTESIAN_POINT('Ctrl Pts',(1.7896938670021,45.7082755242419,14.6623505984215));
#63028=CARTESIAN_POINT('Ctrl Pts',(1.72036142470787,45.7223009067304,14.75053057276));
#63029=CARTESIAN_POINT('Ctrl Pts',(1.69298913966996,45.7278380947269,14.7853438190898));
#63030=CARTESIAN_POINT('Ctrl Pts',(1.66455587907725,45.7333812079543,14.8193690720306));
#63031=CARTESIAN_POINT('Ctrl Pts',(1.63510297141474,45.7389289160858,14.8525234594651));
#63032=CARTESIAN_POINT('Ctrl Pts',(1.63510159445506,45.738929175448,14.8525250094735));
#63033=CARTESIAN_POINT('Ctrl Pts',(1.63510021749315,45.7389294348102,14.85252655948));
#63034=CARTESIAN_POINT('Ctrl Pts',(1.63509884052901,45.7389296941724,14.8525281094847));
#63035=CARTESIAN_POINT('Ctrl Pts',(1.56613403134531,45.7519197672924,14.9301595954892));
#63036=CARTESIAN_POINT('Ctrl Pts',(1.49147302194478,45.7649111277806,15.0031318085196));
#63037=CARTESIAN_POINT('Ctrl Pts',(1.41197344679732,45.7779126670361,15.0707752935465));
#63038=CARTESIAN_POINT('Ctrl Pts',(1.39514738493469,45.7806644390225,15.0850920173977));
#63039=CARTESIAN_POINT('Ctrl Pts',(1.37810471388298,45.7834166663575,15.0991701635101));
#63040=CARTESIAN_POINT('Ctrl Pts',(1.36085377109113,45.7861694322808,15.1130035985599));
#63041=CARTESIAN_POINT('Ctrl Pts',(1.26113857677847,45.8020811764825,15.1929646581178));
#63042=CARTESIAN_POINT('Ctrl Pts',(1.15446609125249,45.8180109660089,15.2647499446223));
#63043=CARTESIAN_POINT('Ctrl Pts',(1.04229941144345,45.8340003826846,15.3272985880928));
#63044=CARTESIAN_POINT('Ctrl Pts',(0.964178247229751,45.8451365939724,15.3708620853473));
#63045=CARTESIAN_POINT('Ctrl Pts',(0.883389045608882,45.8563023000698,15.4099489244777));
#63046=CARTESIAN_POINT('Ctrl Pts',(0.800370417838151,45.8675181404225,15.4442127136742));
#63047=CARTESIAN_POINT('Ctrl Pts',(0.768259093867673,45.8718563894738,15.4574658312562));
#63048=CARTESIAN_POINT('Ctrl Pts',(0.735813330122108,45.8762022324817,15.4699973713265));
#63049=CARTESIAN_POINT('Ctrl Pts',(0.703060616133092,45.8805553092923,15.4817854332903));
#63050=CARTESIAN_POINT('Ctrl Pts',(0.703050939619478,45.8805565953722,15.481788915974));
#63051=CARTESIAN_POINT('Ctrl Pts',(0.703041263080088,45.8805578814527,15.4817923985924));
#63052=CARTESIAN_POINT('Ctrl Pts',(0.703031586514911,45.8805591675338,15.4817958811455));
#63053=CARTESIAN_POINT('Ctrl Pts',(0.598913190449675,45.8943972085069,15.5192676326809));
#63054=CARTESIAN_POINT('Ctrl Pts',(0.491811322180734,45.9083071390249,15.5491856344644));
#63055=CARTESIAN_POINT('Ctrl Pts',(0.382840015976741,45.922258918402,15.5713404404648));
#63056=CARTESIAN_POINT('Ctrl Pts',(0.273289653390351,45.9362848353404,15.5936129736198));
#63057=CARTESIAN_POINT('Ctrl Pts',(0.16184872763076,45.9503529969648,15.6080373508393));
#63058=CARTESIAN_POINT('Ctrl Pts',(0.0496935301666531,45.9644259055572,
15.6143695599238));
#63059=CARTESIAN_POINT('Ctrl Pts',(-0.0623519980788118,45.9784850531745,
15.6206955771559));
#63060=CARTESIAN_POINT('Ctrl Pts',(-0.175110226864188,45.9925487458726,
15.6189427438539));
#63061=CARTESIAN_POINT('Ctrl Pts',(-0.28735619715166,46.0065744352014,15.6088725393529));
#63062=CARTESIAN_POINT('Ctrl Pts',(-0.336779260054703,46.0127500914337,
15.604438524045));
#63063=CARTESIAN_POINT('Ctrl Pts',(-0.386102348209196,46.0189183298531,
15.5983922846779));
#63064=CARTESIAN_POINT('Ctrl Pts',(-0.435218281183437,46.0250754033888,
15.5907156564064));
#63065=CARTESIAN_POINT('Ctrl Pts',(-0.435230082382689,46.0250768827632,
15.5907138119251));
#63066=CARTESIAN_POINT('Ctrl Pts',(-0.435241883569989,46.0250783621369,
15.5907119673496));
#63067=CARTESIAN_POINT('Ctrl Pts',(-0.435253684745325,46.0250798415099,
15.5907101226801));
#63068=CARTESIAN_POINT('Ctrl Pts',(-0.525371743418507,46.0363768712413,
15.5766235565477));
#63069=CARTESIAN_POINT('Ctrl Pts',(-0.614753314310338,46.0476966561241,
15.5570477433176));
#63070=CARTESIAN_POINT('Ctrl Pts',(-0.702841229104749,46.0590791391817,
15.5322464666312));
#63071=CARTESIAN_POINT('Ctrl Pts',(-0.815299827109943,46.0736107362738,
15.5005835897042));
#63072=CARTESIAN_POINT('Ctrl Pts',(-0.925682269708267,46.0882487675148,
15.4603969024718));
#63073=CARTESIAN_POINT('Ctrl Pts',(-1.03285245568836,46.102958952506,15.4121867479535));
#63074=CARTESIAN_POINT('Ctrl Pts',(-1.0452004310303,46.1046538362079,15.4066320519923));
#63075=CARTESIAN_POINT('Ctrl Pts',(-1.05750574276826,46.1063496784497,15.4009707890295));
#63076=CARTESIAN_POINT('Ctrl Pts',(-1.06976663537864,46.1080464273473,15.3952036835102));
#63077=CARTESIAN_POINT('Ctrl Pts',(-1.18897462636356,46.1245432709069,15.3391323121512));
#63078=CARTESIAN_POINT('Ctrl Pts',(-1.30398312889218,46.1411250683823,15.2730541157071));
#63079=CARTESIAN_POINT('Ctrl Pts',(-1.41303318927676,46.1577210886726,15.1977111356521));
#63080=CARTESIAN_POINT('Ctrl Pts',(-1.50084466817589,46.1710848693105,15.1370419486754));
#63081=CARTESIAN_POINT('Ctrl Pts',(-1.58478982824556,46.1844572504357,15.0703635161614));
#63082=CARTESIAN_POINT('Ctrl Pts',(-1.66390124624768,46.1977957708119,14.9981333392991));
#63083=CARTESIAN_POINT('Ctrl Pts',(-1.68290645862786,46.2010001301698,14.9807812315226));
#63084=CARTESIAN_POINT('Ctrl Pts',(-1.70163286462932,46.2042025364822,14.9631088938852));
#63085=CARTESIAN_POINT('Ctrl Pts',(-1.7200673811099,46.2074024033346,14.9451229832622));
#63086=CARTESIAN_POINT('Ctrl Pts',(-1.7460829147076,46.2119181845699,14.9197405403546));
#63087=CARTESIAN_POINT('Ctrl Pts',(-1.77151646079242,46.2164288955996,14.8937341201424));
#63088=CARTESIAN_POINT('Ctrl Pts',(-1.79633063772826,46.2209329275884,14.867124224798));
#63089=CARTESIAN_POINT('Ctrl Pts',(-1.7963377999747,46.2209342276108,14.8671165442439));
#63090=CARTESIAN_POINT('Ctrl Pts',(-1.79634496216954,46.2209355276327,14.8671088636395));
#63091=CARTESIAN_POINT('Ctrl Pts',(-1.7963521243128,46.2209368276541,14.8671011829849));
#63092=CARTESIAN_POINT('Ctrl Pts',(-1.8580267719732,46.2321315713293,14.8009615301429));
#63093=CARTESIAN_POINT('Ctrl Pts',(-1.91588801512161,46.243332586979,14.7310686861218));
#63094=CARTESIAN_POINT('Ctrl Pts',(-1.96966602037887,46.2546052295084,14.6579467026471));
#63095=CARTESIAN_POINT('Ctrl Pts',(-2.04086980476799,46.2695305656995,14.5611308776545));
#63096=CARTESIAN_POINT('Ctrl Pts',(-2.10493619863944,46.2845858219809,14.458629663659));
#63097=CARTESIAN_POINT('Ctrl Pts',(-2.16125877011487,46.2997260694423,14.3516151544837));
#63098=CARTESIAN_POINT('Ctrl Pts',(-2.16793241666151,46.301520033346,14.3389350336922));
#63099=CARTESIAN_POINT('Ctrl Pts',(-2.17449729258174,46.3033151917321,14.3261915119305));
#63100=CARTESIAN_POINT('Ctrl Pts',(-2.18095234819548,46.3051114708695,14.3133865127906));
#63101=CARTESIAN_POINT('Ctrl Pts',(-2.2423176437236,46.3221878845696,14.1916551748319));
#63102=CARTESIAN_POINT('Ctrl Pts',(-2.29375669115427,46.3393645221848,14.0643671729683));
#63103=CARTESIAN_POINT('Ctrl Pts',(-2.3343019945624,46.3565508938873,13.9333222913705));
#63104=CARTESIAN_POINT('Ctrl Pts',(-2.36673028871117,46.3702966220006,13.8285120763779));
#63105=CARTESIAN_POINT('Ctrl Pts',(-2.3921868447487,46.3840478092587,13.7212985838361));
#63106=CARTESIAN_POINT('Ctrl Pts',(-2.41018104824501,46.3977527520996,13.6126860575908));
#63107=CARTESIAN_POINT('Ctrl Pts',(-2.41458682489408,46.401108328086,13.5860929087456));
#63108=CARTESIAN_POINT('Ctrl Pts',(-2.4185454856787,46.4044611347154,13.5594159140209));
#63109=CARTESIAN_POINT('Ctrl Pts',(-2.42205031287158,46.4078104189869,13.5326698291747));
#63110=CARTESIAN_POINT('Ctrl Pts',(-2.42671081461347,46.4122640894027,13.4971045450237));
#63111=CARTESIAN_POINT('Ctrl Pts',(-2.4305686623175,46.4167115284011,13.4614179034804));
#63112=CARTESIAN_POINT('Ctrl Pts',(-2.43360857407939,46.4211510309047,13.4256462336321));
#63113=CARTESIAN_POINT('Ctrl Pts',(-2.43360923252887,46.4211519925077,13.4256384854344));
#63114=CARTESIAN_POINT('Ctrl Pts',(-2.43360989093997,46.4211529541102,13.4256307372327));
#63115=CARTESIAN_POINT('Ctrl Pts',(-2.43361054931271,46.4211539157124,13.425622989027));
#63116=CARTESIAN_POINT('Ctrl Pts',(-2.44118605491686,46.4322185033857,13.3364689698517));
#63117=CARTESIAN_POINT('Ctrl Pts',(-2.44367563763571,46.4432709808867,13.2467458408072));
#63118=CARTESIAN_POINT('Ctrl Pts',(-2.44116990612555,46.4543970479552,13.1569972656756));
#63119=CARTESIAN_POINT('Ctrl Pts',(-2.43756619939952,46.4703983962905,13.0279221662322));
#63120=CARTESIAN_POINT('Ctrl Pts',(-2.42363224404003,46.4865569668884,12.898760902024));
#63121=CARTESIAN_POINT('Ctrl Pts',(-2.39968396120161,46.502820237758,12.7710505777282));
#63122=CARTESIAN_POINT('Ctrl Pts',(-2.39583844700153,46.5054317251657,12.7505433927709));
#63123=CARTESIAN_POINT('Ctrl Pts',(-2.39173460861502,46.5080459155969,12.730073614735));
#63124=CARTESIAN_POINT('Ctrl Pts',(-2.38737362867296,46.510662595552,12.7096476098486));
#63125=CARTESIAN_POINT('Ctrl Pts',(-2.35555178287611,46.529756374276,12.560600105302));
#63126=CARTESIAN_POINT('Ctrl Pts',(-2.31003584733003,46.5489807973168,12.4138849447933));
#63127=CARTESIAN_POINT('Ctrl Pts',(-2.25134135194109,46.5682193411139,12.2721586464856));
#63128=CARTESIAN_POINT('Ctrl Pts',(-2.20846714539796,46.5822724017097,12.1686327102632));
#63129=CARTESIAN_POINT('Ctrl Pts',(-2.1585595379306,46.5963319308722,12.0677701985499));
#63130=CARTESIAN_POINT('Ctrl Pts',(-2.10187305059963,46.6103505794577,11.9706580098738));
#63131=CARTESIAN_POINT('Ctrl Pts',(-2.08096405430936,46.6155214038476,11.934837861398));
#63132=CARTESIAN_POINT('Ctrl Pts',(-2.05913317880697,46.6206866739007,11.899527659463));
#63133=CARTESIAN_POINT('Ctrl Pts',(-2.03639456038824,46.6258440409837,11.8647807478773));
#63134=CARTESIAN_POINT('Ctrl Pts',(-2.03638593685606,46.625845996895,11.8647675702468));
#63135=CARTESIAN_POINT('Ctrl Pts',(-2.03637731319332,46.6258479528052,11.8647543926974));
#63136=CARTESIAN_POINT('Ctrl Pts',(-2.03636868940005,46.6258499087143,11.864741215229));
#63137=CARTESIAN_POINT('Ctrl Pts',(-1.99141350257691,46.6360459156751,11.7960480618037));
#63138=CARTESIAN_POINT('Ctrl Pts',(-1.94288302261679,46.6462057173813,11.7295064414119));
#63139=CARTESIAN_POINT('Ctrl Pts',(-1.89105741220381,46.6564390616992,11.6654615457098));
#63140=CARTESIAN_POINT('Ctrl Pts',(-1.88709149184184,46.6572221615658,11.6605605526694));
#63141=CARTESIAN_POINT('Ctrl Pts',(-1.88310626025049,46.6580056935545,11.6556741540323));
#63142=CARTESIAN_POINT('Ctrl Pts',(-1.87910183479348,46.6587897073237,11.6508024920328));
#63143=CARTESIAN_POINT('Ctrl Pts',(1.6569451353564,55.4128966646337,10.6605449173006));
#63144=CARTESIAN_POINT('Ctrl Pts',(2.33530670602075,55.5119034702439,11.0720924681345));
#63145=CARTESIAN_POINT('Ctrl Pts',(3.35287144550745,55.7089215617343,12.4309775396479));
#63146=CARTESIAN_POINT('Ctrl Pts',(3.06131862396214,56.0060657212896,14.970206851602));
#63147=CARTESIAN_POINT('Ctrl Pts',(1.11674766776748,56.3032657896637,16.6277723342266));
#63148=CARTESIAN_POINT('Ctrl Pts',(-1.45201060496089,56.602088525808,16.5144825668909));
#63149=CARTESIAN_POINT('Ctrl Pts',(-2.9552727303039,56.8520507440691,14.979981386742));
#63150=CARTESIAN_POINT('Ctrl Pts',(-3.29622519867115,57.052306151596,13.3826435061434));
#63151=CARTESIAN_POINT('Ctrl Pts',(-3.03946287691416,57.252676609567,11.7672071495042));
#63152=CARTESIAN_POINT('Ctrl Pts',(-1.90135817724995,57.4530663770427,10.4790510860224));
#63153=CARTESIAN_POINT('Ctrl Pts',(-0.331321547087517,57.653223522874,10.0240350930701));
#63154=CARTESIAN_POINT('Ctrl Pts',(1.02092307270453,57.8198122673918,10.1438419603152));
#63155=CARTESIAN_POINT('Ctrl Pts',(2.32847716926071,58.002702432299,10.9045066475814));
#63156=CARTESIAN_POINT('Ctrl Pts',(3.17902663186017,58.2016159780822,12.3119941431888));
#63157=CARTESIAN_POINT('Ctrl Pts',(3.25111765677419,58.3997743068538,13.9484260261249));
#63158=CARTESIAN_POINT('Ctrl Pts',(2.53332529252753,58.5970285722796,15.4132580743736));
#63159=CARTESIAN_POINT('Ctrl Pts',(1.20880262079472,58.7932309276008,16.349001183064));
#63160=CARTESIAN_POINT('Ctrl Pts',(-0.392972327268547,58.9882406659482,
16.5356913377198));
#63161=CARTESIAN_POINT('Ctrl Pts',(-1.87723242415658,59.1819184781718,15.9349461681502));
#63162=CARTESIAN_POINT('Ctrl Pts',(-2.71710555490916,59.3420967355076,14.9109753802198));
#63163=CARTESIAN_POINT('Ctrl Pts',(-3.03243667131599,59.4694445491574,13.9321695038961));
#63164=CARTESIAN_POINT('Ctrl Pts',(-3.09841455447119,59.5962431685408,12.9100621162179));
#63165=CARTESIAN_POINT('Ctrl Pts',(-2.69924485240655,59.7536690381048,11.6714562710649));
#63166=CARTESIAN_POINT('Ctrl Pts',(-1.57613832723902,59.9407574424593,10.6072778298864));
#63167=CARTESIAN_POINT('Ctrl Pts',(-0.096551163052406,60.1259118027667,
10.2150729201606));
#63168=CARTESIAN_POINT('Ctrl Pts',(1.37396628627166,60.3090339467634,10.5757102953909));
#63169=CARTESIAN_POINT('Ctrl Pts',(2.47908226284073,60.4900310898842,11.5848804741311));
#63170=CARTESIAN_POINT('Ctrl Pts',(2.95980408366685,60.6688191325761,12.9826417343107));
#63171=CARTESIAN_POINT('Ctrl Pts',(2.74235929646795,60.8257126597751,14.2617726150318));
#63172=CARTESIAN_POINT('Ctrl Pts',(2.13344390025228,60.9614695210831,15.1810775758813));
#63173=CARTESIAN_POINT('Ctrl Pts',(1.14324694123969,61.1152052069727,15.9444605983494));
#63174=CARTESIAN_POINT('Ctrl Pts',(-0.442597201666302,61.3046784881151,
16.1881055945206));
#63175=CARTESIAN_POINT('Ctrl Pts',(-1.95016975236964,61.5090501034515,15.3377070645724));
#63176=CARTESIAN_POINT('Ctrl Pts',(-2.63888887238414,61.6915669650262,13.9936833394969));
#63177=CARTESIAN_POINT('Ctrl Pts',(-2.60879331776602,61.8532873127061,12.6578979527681));
#63178=CARTESIAN_POINT('Ctrl Pts',(-1.95119277387709,62.0124516622465,11.5172602409941));
#63179=CARTESIAN_POINT('Ctrl Pts',(-0.846601874313005,62.1690601894784,
10.8418271444237));
#63180=CARTESIAN_POINT('Ctrl Pts',(0.425857363513597,62.3231222193529,10.7795975324474));
#63181=CARTESIAN_POINT('Ctrl Pts',(1.36594609467601,62.4494013640976,11.2333728797989));
#63182=CARTESIAN_POINT('Ctrl Pts',(1.91361895881445,62.5491746001873,11.8247167504303));
#63183=CARTESIAN_POINT('Ctrl Pts',(2.20031261426614,62.623386180769,12.351148983469));
#63184=CARTESIAN_POINT('Ctrl Pts',(2.34638492720226,62.6969812241368,12.927312881863));
#63185=CARTESIAN_POINT('Ctrl Pts',(2.34622867202676,62.794297702193,13.7136951888079));
#63186=CARTESIAN_POINT('Ctrl Pts',(1.98055868552105,62.9144348967284,14.6366736894937));
#63187=CARTESIAN_POINT('Ctrl Pts',(1.07943680968674,63.0562449888743,15.3885632620892));
#63188=CARTESIAN_POINT('Ctrl Pts',(-0.0517025031410053,63.1957665233168,
15.611357253593));
#63189=CARTESIAN_POINT('Ctrl Pts',(-1.25748872761872,63.3483316662509,15.2359395671154));
#63190=CARTESIAN_POINT('Ctrl Pts',(-2.13867141013038,63.5131145797047,14.153379855809));
#63191=CARTESIAN_POINT('Ctrl Pts',(-2.16335040768803,63.6893115604284,12.660199850989));
#63192=CARTESIAN_POINT('Ctrl Pts',(-1.2796523659689,63.8621839816488,11.4927639172216));
#63193=CARTESIAN_POINT('Ctrl Pts',(0.113042382290236,64.0320007008191,11.1257732842045));
#63194=CARTESIAN_POINT('Ctrl Pts',(1.19376322125476,64.1712099717327,11.5955981161));
#63195=CARTESIAN_POINT('Ctrl Pts',(1.74482084921513,64.2813450206176,12.3015104532762));
#63196=CARTESIAN_POINT('Ctrl Pts',(1.99967883271567,64.3770450715635,13.0361210359255));
#63197=CARTESIAN_POINT('Ctrl Pts',(1.92373662025134,64.4855227576122,13.9302995954116));
#63198=CARTESIAN_POINT('Ctrl Pts',(1.37247448803971,64.6065013765781,14.7653662718488));
#63199=CARTESIAN_POINT('Ctrl Pts',(0.494716294691718,64.7265690605065,15.2299530497279));
#63200=CARTESIAN_POINT('Ctrl Pts',(-0.491871158051163,64.8458671269723,
15.2191438616901));
#63201=CARTESIAN_POINT('Ctrl Pts',(-1.34795918795173,64.96455763081,14.7381624934));
#63202=CARTESIAN_POINT('Ctrl Pts',(-1.737771459396,65.0532306509411,14.1172205890816));
#63203=CARTESIAN_POINT('Ctrl Pts',(-1.89283496250823,65.1319236578043,13.5043914212779));
#63204=CARTESIAN_POINT('Ctrl Pts',(-1.89254479014124,65.2105336050236,12.8629868281662));
#63205=CARTESIAN_POINT('Ctrl Pts',(-1.5131484507725,65.3185043266858,12.0544839835084));
#63206=CARTESIAN_POINT('Ctrl Pts',(-0.726972137876947,65.436307457049,11.4786714103702));
#63207=CARTESIAN_POINT('Ctrl Pts',(0.240309264892923,65.554283263124,11.3496940189649));
#63208=CARTESIAN_POINT('Ctrl Pts',(1.15372183914517,65.6725903488457,11.7010113985837));
#63209=CARTESIAN_POINT('Ctrl Pts',(1.78960549170489,65.7913838071524,12.4501752820213));
#63210=CARTESIAN_POINT('Ctrl Pts',(1.98978935163561,65.9108195532194,13.4176318348034));
#63211=CARTESIAN_POINT('Ctrl Pts',(1.70010179189264,66.031048010758,14.3690921123399));
#63212=CARTESIAN_POINT('Ctrl Pts',(0.983696228421434,66.1522187579812,15.0698078200568));
#63213=CARTESIAN_POINT('Ctrl Pts',(-0.0976755268654362,66.2880612365788,
15.3766078480273));
#63214=CARTESIAN_POINT('Ctrl Pts',(-1.31878244840489,66.4392396164331,14.9904843787632));
#63215=CARTESIAN_POINT('Ctrl Pts',(-2.11559642723716,66.6066695529819,13.8144955958308));
#63216=CARTESIAN_POINT('Ctrl Pts',(-2.02851560781646,66.75208241469,12.5861000530642));
#63217=CARTESIAN_POINT('Ctrl Pts',(-1.46871591953313,66.8743804483054,11.7598210561588));
#63218=CARTESIAN_POINT('Ctrl Pts',(-0.590976964864925,67.0052427017216,
11.1517409461587));
#63219=CARTESIAN_POINT('Ctrl Pts',(0.836486125966097,67.1715005769598,11.088655253674));
#63220=CARTESIAN_POINT('Ctrl Pts',(2.17249609611971,67.3756418705779,12.2305198194672));
#63221=CARTESIAN_POINT('Ctrl Pts',(2.37549715084904,67.5847068153988,14.0174281878148));
#63222=CARTESIAN_POINT('Ctrl Pts',(1.27924295687799,67.7989571326317,15.4990495841261));
#63223=CARTESIAN_POINT('Ctrl Pts',(-0.578620920351347,68.0185939823309,
15.8438079846843));
#63224=CARTESIAN_POINT('Ctrl Pts',(-2.29959856019092,68.2557971598705,14.7465525063924));
#63225=CARTESIAN_POINT('Ctrl Pts',(-2.59210142572018,68.4223406725752,13.3131908810002));
#63226=CARTESIAN_POINT('Ctrl Pts',(-2.40813948819331,68.5130695044136,12.607364467103));
#63227=CARTESIAN_POINT('Ctrl Pts',(1.55030632904987,55.7588406051485,10.8358132077334));
#63228=CARTESIAN_POINT('Ctrl Pts',(2.17876663993083,55.8514133669438,11.2297589453932));
#63229=CARTESIAN_POINT('Ctrl Pts',(3.10425265743942,56.0346852578565,12.5086978226667));
#63230=CARTESIAN_POINT('Ctrl Pts',(2.7983392353447,56.3084852816261,14.8432409534713));
#63231=CARTESIAN_POINT('Ctrl Pts',(0.999166163143576,56.5799450362436,16.3288210786526));
#63232=CARTESIAN_POINT('Ctrl Pts',(-1.32580643434958,56.8507000918492,16.1904044489405));
#63233=CARTESIAN_POINT('Ctrl Pts',(-2.65653224227183,57.0755242670608,14.7903593192062));
#63234=CARTESIAN_POINT('Ctrl Pts',(-2.94151465380921,57.2547579143383,13.3570145845722));
#63235=CARTESIAN_POINT('Ctrl Pts',(-2.69226601616852,57.4335381145205,11.9192191403096));
#63236=CARTESIAN_POINT('Ctrl Pts',(-1.66478551166155,57.6115643239159,10.7899644198409));
#63237=CARTESIAN_POINT('Ctrl Pts',(-0.270097413097286,57.788721156688,10.40668375296));
#63238=CARTESIAN_POINT('Ctrl Pts',(0.922243286047465,57.9358340402107,10.5289617109777));
#63239=CARTESIAN_POINT('Ctrl Pts',(2.06444297016673,58.0969552999316,11.2149702554646));
#63240=CARTESIAN_POINT('Ctrl Pts',(2.79453271510212,58.2717826325117,12.462035133664));
#63241=CARTESIAN_POINT('Ctrl Pts',(2.8377849285338,58.4456085398852,13.897952306082));
#63242=CARTESIAN_POINT('Ctrl Pts',(2.19145453480309,58.6183767694301,15.1717938539383));
#63243=CARTESIAN_POINT('Ctrl Pts',(1.02160522451961,58.7900344295843,15.9740909181386));
#63244=CARTESIAN_POINT('Ctrl Pts',(-0.380669222056866,58.9605337467761,
16.1177395446806));
#63245=CARTESIAN_POINT('Ctrl Pts',(-1.67032812037787,59.1298305650957,15.574657980914));
#63246=CARTESIAN_POINT('Ctrl Pts',(-2.39184175344818,59.2698766903008,14.6693785233005));
#63247=CARTESIAN_POINT('Ctrl Pts',(-2.65547925022823,59.3812757961609,13.8095358651761));
#63248=CARTESIAN_POINT('Ctrl Pts',(-2.70048215198635,59.4922450908539,12.9145183722852));
#63249=CARTESIAN_POINT('Ctrl Pts',(-2.33557323358447,59.6301401972359,11.8349012228523));
#63250=CARTESIAN_POINT('Ctrl Pts',(-1.33720550047092,59.794285375669,10.915598661706));
#63251=CARTESIAN_POINT('Ctrl Pts',(-0.0317735574344565,59.9570811821498,
10.5895801462829));
#63252=CARTESIAN_POINT('Ctrl Pts',(1.25950858227736,60.1185138351077,10.9261995573682));
#63253=CARTESIAN_POINT('Ctrl Pts',(2.2233718578003,60.2785742015327,11.8326346868727));
#63254=CARTESIAN_POINT('Ctrl Pts',(2.63150737695493,60.4372585851517,13.0790938708883));
#63255=CARTESIAN_POINT('Ctrl Pts',(2.42070552945755,60.5770896003784,14.2157979806749));
#63256=CARTESIAN_POINT('Ctrl Pts',(1.86333929704872,60.6985554821939,15.0295958228732));
#63257=CARTESIAN_POINT('Ctrl Pts',(0.964146758236579,60.8365676763953,15.7006770391375));
#63258=CARTESIAN_POINT('Ctrl Pts',(-0.469990621989699,61.0075823543855,
15.8990905951955));
#63259=CARTESIAN_POINT('Ctrl Pts',(-1.82942006965859,61.1935399322503,15.1047258503496));
#63260=CARTESIAN_POINT('Ctrl Pts',(-2.44101035487483,61.3609220053499,13.8624175643746));
#63261=CARTESIAN_POINT('Ctrl Pts',(-2.39290165806376,61.5103093723956,12.6295218273013));
#63262=CARTESIAN_POINT('Ctrl Pts',(-1.76327705757714,61.6584778781679,11.5783996321574));
#63263=CARTESIAN_POINT('Ctrl Pts',(-0.716199583790733,61.8054689868533,
10.9624222170237));
#63264=CARTESIAN_POINT('Ctrl Pts',(0.488992325435071,61.9513295435539,10.9244754634972));
#63265=CARTESIAN_POINT('Ctrl Pts',(1.37900585512795,62.0719795781345,11.3737626521626));
#63266=CARTESIAN_POINT('Ctrl Pts',(1.89495908614165,62.1679858723417,11.952452288719));
#63267=CARTESIAN_POINT('Ctrl Pts',(2.16225961813357,62.2397432439528,12.4664773515498));
#63268=CARTESIAN_POINT('Ctrl Pts',(2.29327778325782,62.3112572030224,13.0287746925004));
#63269=CARTESIAN_POINT('Ctrl Pts',(2.27811114094167,62.4062990558202,13.7962768006778));
#63270=CARTESIAN_POINT('Ctrl Pts',(1.90119161550483,62.5245351899349,14.69731375192));
#63271=CARTESIAN_POINT('Ctrl Pts',(0.991059706471317,62.6655805612644,15.4273887252442));
#63272=CARTESIAN_POINT('Ctrl Pts',(-0.150004376109035,62.8058564957149,
15.6286856953522));
#63273=CARTESIAN_POINT('Ctrl Pts',(-1.36709509943824,62.9609447222707,15.222648270889));
#63274=CARTESIAN_POINT('Ctrl Pts',(-2.25211611298564,63.130653191994,14.0905190910481));
#63275=CARTESIAN_POINT('Ctrl Pts',(-2.24624586275741,63.3148678618416,12.5297620164941));
#63276=CARTESIAN_POINT('Ctrl Pts',(-1.28301168864727,63.4983480200434,11.311171244946));
#63277=CARTESIAN_POINT('Ctrl Pts',(0.224770595741629,63.6812901487001,10.9483526840942));
#63278=CARTESIAN_POINT('Ctrl Pts',(1.39390275914629,63.8334601868623,11.4879250790583));
#63279=CARTESIAN_POINT('Ctrl Pts',(1.98317789908194,63.9551256179044,12.2820193030557));
#63280=CARTESIAN_POINT('Ctrl Pts',(2.24617475003574,64.0615735288727,13.1053181121864));
#63281=CARTESIAN_POINT('Ctrl Pts',(2.13668022844515,64.1832525517915,14.105364041827));
#63282=CARTESIAN_POINT('Ctrl Pts',(1.48954809134978,64.3202627986689,15.034777364303));
#63283=CARTESIAN_POINT('Ctrl Pts',(0.473982051015632,64.4574800889518,15.5400576078666));
#63284=CARTESIAN_POINT('Ctrl Pts',(-0.66171351991401,64.594983404464,15.4986622727337));
#63285=CARTESIAN_POINT('Ctrl Pts',(-1.64085117064997,64.7328610307015,14.914831237791));
#63286=CARTESIAN_POINT('Ctrl Pts',(-2.07753209225151,64.8366078315501,14.1771813960306));
#63287=CARTESIAN_POINT('Ctrl Pts',(-2.24009694071431,64.929048128958,13.4531318429259));
#63288=CARTESIAN_POINT('Ctrl Pts',(-2.21963294989472,65.0216743325075,12.6981819858978));
#63289=CARTESIAN_POINT('Ctrl Pts',(-1.74549286459253,65.1495231060764,11.7537198628781));
#63290=CARTESIAN_POINT('Ctrl Pts',(-0.79283887697972,65.2896804488173,11.0942726574537));
#63291=CARTESIAN_POINT('Ctrl Pts',(0.365435937342801,65.4305951420548,10.9712986683346));
#63292=CARTESIAN_POINT('Ctrl Pts',(1.4473487981291,65.5723372986805,11.4211295951556));
#63293=CARTESIAN_POINT('Ctrl Pts',(2.18589654308168,65.714972902499,12.340214248751));
#63294=CARTESIAN_POINT('Ctrl Pts',(2.39511056864538,65.8585655679861,13.508592320582));
#63295=CARTESIAN_POINT('Ctrl Pts',(2.01640605087595,66.0031741366381,14.6424709362779));
#63296=CARTESIAN_POINT('Ctrl Pts',(1.13352498395727,66.1488542435468,15.4610899116906));
#63297=CARTESIAN_POINT('Ctrl Pts',(-0.173417136522122,66.3119687801929,
15.7946856755799));
#63298=CARTESIAN_POINT('Ctrl Pts',(-1.62240671165605,66.4930630885744,15.293817234782));
#63299=CARTESIAN_POINT('Ctrl Pts',(-2.53500320867109,66.6928009644741,13.8672779219842));
#63300=CARTESIAN_POINT('Ctrl Pts',(-2.39383160202435,66.8653436855591,12.4138986555751));
#63301=CARTESIAN_POINT('Ctrl Pts',(-1.709215002913,67.0097186748878,11.4559652991775));
#63302=CARTESIAN_POINT('Ctrl Pts',(-0.660294050672969,67.1635832522325,
10.7671026808167));
#63303=CARTESIAN_POINT('Ctrl Pts',(1.00756509210864,67.3578056337846,10.7361814279581));
#63304=CARTESIAN_POINT('Ctrl Pts',(2.5182626185487,67.59394679212,12.0948221133186));
#63305=CARTESIAN_POINT('Ctrl Pts',(2.69974491017161,67.8331851043461,14.1434923407273));
#63306=CARTESIAN_POINT('Ctrl Pts',(1.42035678851664,68.0755129907451,15.7878664622788));
#63307=CARTESIAN_POINT('Ctrl Pts',(-0.662768296243718,68.3209020968419,
16.1235997088386));
#63308=CARTESIAN_POINT('Ctrl Pts',(-2.53145414382765,68.5825321030457,14.8705287716948));
#63309=CARTESIAN_POINT('Ctrl Pts',(-2.81335053070336,68.7636377248232,13.3051962830399));
#63310=CARTESIAN_POINT('Ctrl Pts',(-2.60004493251108,68.8615196046778,12.5484192313165));
#63311=CARTESIAN_POINT('Ctrl Pts',(1.44366752274332,56.1047845456634,11.0110814981665));
#63312=CARTESIAN_POINT('Ctrl Pts',(2.02222657384092,56.1909232636435,11.387425422652));
#63313=CARTESIAN_POINT('Ctrl Pts',(2.85563386937139,56.3604489539787,12.5864181056853));
#63314=CARTESIAN_POINT('Ctrl Pts',(2.53535984672727,56.6109048419626,14.7162750553406));
#63315=CARTESIAN_POINT('Ctrl Pts',(0.881584658519683,56.8566242828234,16.0298698230785));
#63316=CARTESIAN_POINT('Ctrl Pts',(-1.19960226373825,57.0993116578905,15.8663263309902));
#63317=CARTESIAN_POINT('Ctrl Pts',(-2.35779175423974,57.2989977900524,14.6007372516703));
#63318=CARTESIAN_POINT('Ctrl Pts',(-2.58680410894727,57.4572096770807,13.3313856630009));
#63319=CARTESIAN_POINT('Ctrl Pts',(-2.34506915542287,57.6143996194741,12.0712311311148));
#63320=CARTESIAN_POINT('Ctrl Pts',(-1.42821284607315,57.7700622707892,11.1008777536595));
#63321=CARTESIAN_POINT('Ctrl Pts',(-0.208873279107056,57.9242187905022,
10.78933241285));
#63322=CARTESIAN_POINT('Ctrl Pts',(0.823563499390395,58.0518558130299,10.9140814616404));
#63323=CARTESIAN_POINT('Ctrl Pts',(1.80040877107275,58.191208167564,11.5254338633479));
#63324=CARTESIAN_POINT('Ctrl Pts',(2.41003879834408,58.3419492869412,12.6120761241389));
#63325=CARTESIAN_POINT('Ctrl Pts',(2.42445220029341,58.4914427729167,13.8474785860391));
#63326=CARTESIAN_POINT('Ctrl Pts',(1.84958377707867,58.6397249665805,14.930329633503));
#63327=CARTESIAN_POINT('Ctrl Pts',(0.834407828244496,58.7868379315678,15.5991806532132));
#63328=CARTESIAN_POINT('Ctrl Pts',(-0.368366116845181,58.9328268276039,
15.6997877516412));
#63329=CARTESIAN_POINT('Ctrl Pts',(-1.46342381659914,59.0777426520196,15.214369793678));
#63330=CARTESIAN_POINT('Ctrl Pts',(-2.06657795198719,59.1976566450941,14.4277816663813));
#63331=CARTESIAN_POINT('Ctrl Pts',(-2.27852182914047,59.2931070431642,13.6869022264562));
#63332=CARTESIAN_POINT('Ctrl Pts',(-2.30254974950152,59.388247013167,12.9189746283525));
#63333=CARTESIAN_POINT('Ctrl Pts',(-1.97190161476237,59.5066113563671,11.9983461746398));
#63334=CARTESIAN_POINT('Ctrl Pts',(-1.09827267370282,59.6478133088788,11.2239194935258));
#63335=CARTESIAN_POINT('Ctrl Pts',(0.0330040481834923,59.7882505615329,
10.9640873724053));
#63336=CARTESIAN_POINT('Ctrl Pts',(1.14505087828308,59.9279937234519,11.2766888193456));
#63337=CARTESIAN_POINT('Ctrl Pts',(1.96766145275984,60.0671173131813,12.0803888996145));
#63338=CARTESIAN_POINT('Ctrl Pts',(2.30321067024301,60.2056980377275,13.175546007466));
#63339=CARTESIAN_POINT('Ctrl Pts',(2.09905176244713,60.3284665409815,14.1698233463179));
#63340=CARTESIAN_POINT('Ctrl Pts',(1.59323469384517,60.4356414433047,14.8781140698653));
#63341=CARTESIAN_POINT('Ctrl Pts',(0.785046575233456,60.5579301458178,15.4568934799259));
#63342=CARTESIAN_POINT('Ctrl Pts',(-0.497384042313105,60.710486220656,15.6100755958704));
#63343=CARTESIAN_POINT('Ctrl Pts',(-1.70867038694753,60.8780297610492,14.8717446361267));
#63344=CARTESIAN_POINT('Ctrl Pts',(-2.24313183736552,61.0302770456738,13.7311517892522));
#63345=CARTESIAN_POINT('Ctrl Pts',(-2.17700999836153,61.1673314320849,12.6011457018345));
#63346=CARTESIAN_POINT('Ctrl Pts',(-1.5753613412772,61.3045040940893,11.6395390233208));
#63347=CARTESIAN_POINT('Ctrl Pts',(-0.585797293268466,61.4418777842281,
11.0830172896236));
#63348=CARTESIAN_POINT('Ctrl Pts',(0.552127287356539,61.579536867755,11.069353394547));
#63349=CARTESIAN_POINT('Ctrl Pts',(1.39206561557985,61.6945577921715,11.5141524245262));
#63350=CARTESIAN_POINT('Ctrl Pts',(1.87629921346887,61.7867971444959,12.0801878270077));
#63351=CARTESIAN_POINT('Ctrl Pts',(2.12420662200097,61.8561003071363,12.5818057196306));
#63352=CARTESIAN_POINT('Ctrl Pts',(2.24017063931338,61.9255331819081,13.1302365031378));
#63353=CARTESIAN_POINT('Ctrl Pts',(2.20999360985659,62.0183004094474,13.8788584125477));
#63354=CARTESIAN_POINT('Ctrl Pts',(1.82182454548863,62.1346354831413,14.7579538143466));
#63355=CARTESIAN_POINT('Ctrl Pts',(0.902682603255894,62.2749161336543,15.4662141883991));
#63356=CARTESIAN_POINT('Ctrl Pts',(-0.248306249077079,62.4159464681129,
15.6460141371113));
#63357=CARTESIAN_POINT('Ctrl Pts',(-1.47670147125775,62.5735577782905,15.2093569746626));
#63358=CARTESIAN_POINT('Ctrl Pts',(-2.36556081584091,62.7481918042831,14.0276583262871));
#63359=CARTESIAN_POINT('Ctrl Pts',(-2.3291413178268,62.9404241632548,12.3993241819992));
#63360=CARTESIAN_POINT('Ctrl Pts',(-1.28637101132565,63.1345120584382,11.1295785726704));
#63361=CARTESIAN_POINT('Ctrl Pts',(0.336498809193019,63.3305795965811,10.7709320839836));
#63362=CARTESIAN_POINT('Ctrl Pts',(1.5940422970378,63.495710401992,11.3802520420165));
#63363=CARTESIAN_POINT('Ctrl Pts',(2.22153494894874,63.6289062151912,12.2625281528353));
#63364=CARTESIAN_POINT('Ctrl Pts',(2.49267066735581,63.7461019861821,13.1745151884475));
#63365=CARTESIAN_POINT('Ctrl Pts',(2.34962383663894,63.8809823459707,14.2804284882425));
#63366=CARTESIAN_POINT('Ctrl Pts',(1.60662169465985,64.0340242207596,15.304188456757));
#63367=CARTESIAN_POINT('Ctrl Pts',(0.453247807339546,64.1883911173971,15.8501621660054));
#63368=CARTESIAN_POINT('Ctrl Pts',(-0.831555881776861,64.3440996819558,
15.7781806837776));
#63369=CARTESIAN_POINT('Ctrl Pts',(-1.93374315334822,64.501164430593,15.091499982182));
#63370=CARTESIAN_POINT('Ctrl Pts',(-2.41729272510702,64.6199850121592,14.2371422029794));
#63371=CARTESIAN_POINT('Ctrl Pts',(-2.58735891892037,64.7261726001119,13.401872264574));
#63372=CARTESIAN_POINT('Ctrl Pts',(-2.54672110964819,64.8328150599913,12.5333771436294));
#63373=CARTESIAN_POINT('Ctrl Pts',(-1.97783727841256,64.9805418854671,11.4529557422479));
#63374=CARTESIAN_POINT('Ctrl Pts',(-0.858705616082495,65.1430534405857,
10.7098739045374));
#63375=CARTESIAN_POINT('Ctrl Pts',(0.490562609792683,65.3069070209856,10.5929033177043));
#63376=CARTESIAN_POINT('Ctrl Pts',(1.74097575711306,65.4720842485154,11.1412477917274));
#63377=CARTESIAN_POINT('Ctrl Pts',(2.58218759445846,65.6385619978454,12.2302532154808));
#63378=CARTESIAN_POINT('Ctrl Pts',(2.80043178565517,65.8063115827527,13.5995528063605));
#63379=CARTESIAN_POINT('Ctrl Pts',(2.33271030985925,65.9753002625182,14.915849760216));
#63380=CARTESIAN_POINT('Ctrl Pts',(1.28335373949313,66.1454897291123,15.8523720033243));
#63381=CARTESIAN_POINT('Ctrl Pts',(-0.249158746178807,66.3358763238071,
16.2127635031324));
#63382=CARTESIAN_POINT('Ctrl Pts',(-1.92603097490719,66.5468865607158,15.5971500908009));
#63383=CARTESIAN_POINT('Ctrl Pts',(-2.95440999010503,66.7789323759663,13.9200602481374));
#63384=CARTESIAN_POINT('Ctrl Pts',(-2.75914759623228,66.9786049564283,12.2416972580859));
#63385=CARTESIAN_POINT('Ctrl Pts',(-1.94971408629286,67.14505690147,11.1521095421962));
#63386=CARTESIAN_POINT('Ctrl Pts',(-0.729611136481014,67.3219238027436,
10.3824644154745));
#63387=CARTESIAN_POINT('Ctrl Pts',(1.17864405825117,67.5441106906095,10.383707602242));
#63388=CARTESIAN_POINT('Ctrl Pts',(2.8640291409777,67.8122517136621,11.9591244071702));
#63389=CARTESIAN_POINT('Ctrl Pts',(3.02399266949419,68.0816633932933,14.2695564936399));
#63390=CARTESIAN_POINT('Ctrl Pts',(1.56147062015531,68.3520688488585,16.0766833404313));
#63391=CARTESIAN_POINT('Ctrl Pts',(-0.746915672136096,68.6232102113529,
16.4033914329926));
#63392=CARTESIAN_POINT('Ctrl Pts',(-2.76330972746438,68.909267046221,14.9945050369972));
#63393=CARTESIAN_POINT('Ctrl Pts',(-3.03459963568654,69.1049347770713,13.2972016850794));
#63394=CARTESIAN_POINT('Ctrl Pts',(-2.79195037682888,69.2099697049419,12.4894739955298));
#63395=CARTESIAN_POINT('Ctrl Pts',(1.33702871643679,56.4507284861783,11.1863497885993));
#63396=CARTESIAN_POINT('Ctrl Pts',(1.865686507751,56.5304331603432,11.5450918999109));
#63397=CARTESIAN_POINT('Ctrl Pts',(2.60701508130335,56.6862126501008,12.664138388704));
#63398=CARTESIAN_POINT('Ctrl Pts',(2.27238045810983,56.9133244022991,14.5893091572099));
#63399=CARTESIAN_POINT('Ctrl Pts',(0.764003153895783,57.1333035294033,15.7309185675046));
#63400=CARTESIAN_POINT('Ctrl Pts',(-1.07339809312691,57.3479232239317,15.5422482130399));
#63401=CARTESIAN_POINT('Ctrl Pts',(-2.05905126620767,57.5224713130439,14.4111151841345));
#63402=CARTESIAN_POINT('Ctrl Pts',(-2.23209356408533,57.659661439823,13.3057567414297));
#63403=CARTESIAN_POINT('Ctrl Pts',(-1.99787229467723,57.7952611244277,12.2232431219201));
#63404=CARTESIAN_POINT('Ctrl Pts',(-1.19164018048475,57.9285602176624,11.4117910874779));
#63405=CARTESIAN_POINT('Ctrl Pts',(-0.147649145116826,58.0597164243163,
11.1719810727399));
#63406=CARTESIAN_POINT('Ctrl Pts',(0.724883712733328,58.1678775858489,11.2992012123028));
#63407=CARTESIAN_POINT('Ctrl Pts',(1.53637457197876,58.2854610351965,11.8358974712311));
#63408=CARTESIAN_POINT('Ctrl Pts',(2.02554488158604,58.4121159413706,12.7621171146141));
#63409=CARTESIAN_POINT('Ctrl Pts',(2.01111947205303,58.5372770059481,13.7970048659963));
#63410=CARTESIAN_POINT('Ctrl Pts',(1.50771301935423,58.6610731637311,14.6888654130677));
#63411=CARTESIAN_POINT('Ctrl Pts',(0.647210431969383,58.7836414335513,15.2242703882877));
#63412=CARTESIAN_POINT('Ctrl Pts',(-0.3560630116335,58.9051199084318,15.2818359586019));
#63413=CARTESIAN_POINT('Ctrl Pts',(-1.25651951282042,59.0256547389435,14.8540816064417));
#63414=CARTESIAN_POINT('Ctrl Pts',(-1.74131415052621,59.1254365998873,14.1861848094619));
#63415=CARTESIAN_POINT('Ctrl Pts',(-1.9015644080527,59.2049382901675,13.5642685877362));
#63416=CARTESIAN_POINT('Ctrl Pts',(-1.90461734701668,59.28424893548,12.9234308844198));
#63417=CARTESIAN_POINT('Ctrl Pts',(-1.60822999594029,59.3830825154982,12.161791126427));
#63418=CARTESIAN_POINT('Ctrl Pts',(-0.859339846934732,59.5013412420884,
11.5322403253455));
#63419=CARTESIAN_POINT('Ctrl Pts',(0.0977816538014409,59.6194199409159,
11.3385945985277));
#63420=CARTESIAN_POINT('Ctrl Pts',(1.0305931742888,59.7374736117961,11.6271780813229));
#63421=CARTESIAN_POINT('Ctrl Pts',(1.71195104771939,59.8556604248299,12.3281431123561));
#63422=CARTESIAN_POINT('Ctrl Pts',(1.9749139635311,59.9741374903032,13.2719981440439));
#63423=CARTESIAN_POINT('Ctrl Pts',(1.77739799543672,60.0798434815848,14.1238487119609));
#63424=CARTESIAN_POINT('Ctrl Pts',(1.32313009064161,60.1727274044155,14.7266323168573));
#63425=CARTESIAN_POINT('Ctrl Pts',(0.605946392230338,60.2792926152404,15.213109920714));
#63426=CARTESIAN_POINT('Ctrl Pts',(-0.524777462636502,60.4133900869263,
15.3210605965453));
#63427=CARTESIAN_POINT('Ctrl Pts',(-1.58792070423647,60.5625195898481,14.638763421904));
#63428=CARTESIAN_POINT('Ctrl Pts',(-2.04525331985621,60.6996320859974,13.5998860141298));
#63429=CARTESIAN_POINT('Ctrl Pts',(-1.96111833865927,60.8243534917744,12.5727695763677));
#63430=CARTESIAN_POINT('Ctrl Pts',(-1.38744562497725,60.9505303100106,11.7006784144841));
#63431=CARTESIAN_POINT('Ctrl Pts',(-0.455395002746195,61.078286581603,11.2036123622235));
#63432=CARTESIAN_POINT('Ctrl Pts',(0.61526224927801,61.207744191956,11.2142313255967));
#63433=CARTESIAN_POINT('Ctrl Pts',(1.40512537603178,61.3171360062083,11.6545421968898));
#63434=CARTESIAN_POINT('Ctrl Pts',(1.85763934079607,61.4056084166502,12.2079233652964));
#63435=CARTESIAN_POINT('Ctrl Pts',(2.0861536258684,61.47245737032,12.6971340877114));
#63436=CARTESIAN_POINT('Ctrl Pts',(2.18706349536892,61.5398091607938,13.2316983137753));
#63437=CARTESIAN_POINT('Ctrl Pts',(2.1418760787715,61.6303017630745,13.9614400244176));
#63438=CARTESIAN_POINT('Ctrl Pts',(1.74245747547242,61.7447357763476,14.8185938767729));
#63439=CARTESIAN_POINT('Ctrl Pts',(0.81430550004047,61.8842517060443,15.505039651554));
#63440=CARTESIAN_POINT('Ctrl Pts',(-0.346608122045112,62.0260364405109,
15.6633425788705));
#63441=CARTESIAN_POINT('Ctrl Pts',(-1.58630784307727,62.1861708343101,15.1960656784363));
#63442=CARTESIAN_POINT('Ctrl Pts',(-2.47900551869618,62.3657304165722,13.9647975615262));
#63443=CARTESIAN_POINT('Ctrl Pts',(-2.41203677289619,62.5659804646678,12.2688863475043));
#63444=CARTESIAN_POINT('Ctrl Pts',(-1.28973033400403,62.7706760968329,10.9479859003946));
#63445=CARTESIAN_POINT('Ctrl Pts',(0.448227022644404,62.9798690444623,10.5935114838732));
#63446=CARTESIAN_POINT('Ctrl Pts',(1.7941818349293,63.1579606171217,11.2725790049749));
#63447=CARTESIAN_POINT('Ctrl Pts',(2.45989199881554,63.302686812478,12.2430370026149));
#63448=CARTESIAN_POINT('Ctrl Pts',(2.73916658467588,63.4306304434913,13.2437122647084));
#63449=CARTESIAN_POINT('Ctrl Pts',(2.56256744483272,63.5787121401499,14.4554929346579));
#63450=CARTESIAN_POINT('Ctrl Pts',(1.7236952979699,63.7477856428504,15.5735995492112));
#63451=CARTESIAN_POINT('Ctrl Pts',(0.432513563663454,63.9193021458423,16.1602667241441));
#63452=CARTESIAN_POINT('Ctrl Pts',(-1.00139824363972,64.0932159594475,16.0576990948213));
#63453=CARTESIAN_POINT('Ctrl Pts',(-2.22663513604646,64.2694678304844,15.2681687265729));
#63454=CARTESIAN_POINT('Ctrl Pts',(-2.75705335796253,64.4033621927682,14.2971030099283));
#63455=CARTESIAN_POINT('Ctrl Pts',(-2.93462089712645,64.5232970712658,13.3506126862221));
#63456=CARTESIAN_POINT('Ctrl Pts',(-2.87380926940167,64.6439557874752,12.3685723013612));
#63457=CARTESIAN_POINT('Ctrl Pts',(-2.21018169223259,64.8115606648577,11.1521916216177));
#63458=CARTESIAN_POINT('Ctrl Pts',(-0.924572355185274,64.9964264323541,
10.325475151621));
#63459=CARTESIAN_POINT('Ctrl Pts',(0.615689282242555,65.1832188999163,10.2145079670741));
#63460=CARTESIAN_POINT('Ctrl Pts',(2.03460271609701,65.3718311983502,10.8613659882994));
#63461=CARTESIAN_POINT('Ctrl Pts',(2.97847864583523,65.5621510931919,12.1202921822106));
#63462=CARTESIAN_POINT('Ctrl Pts',(3.20575300266493,65.7540575975192,13.6905132921389));
#63463=CARTESIAN_POINT('Ctrl Pts',(2.64901456884257,65.9474263883983,15.1892285841541));
#63464=CARTESIAN_POINT('Ctrl Pts',(1.43318249502898,66.1421252146777,16.2436540949582));
#63465=CARTESIAN_POINT('Ctrl Pts',(-0.324900355835495,66.3597838674212,
16.630841330685));
#63466=CARTESIAN_POINT('Ctrl Pts',(-2.22965523815834,66.6007100328571,15.9004829468197));
#63467=CARTESIAN_POINT('Ctrl Pts',(-3.37381677153895,66.8650637874584,13.9728425742908));
#63468=CARTESIAN_POINT('Ctrl Pts',(-3.12446359044018,67.0918662272974,12.0694958605968));
#63469=CARTESIAN_POINT('Ctrl Pts',(-2.19021316967273,67.2803951280524,10.8482537852148));
#63470=CARTESIAN_POINT('Ctrl Pts',(-0.798928222289059,67.4802643532546,
9.99782615013244));
#63471=CARTESIAN_POINT('Ctrl Pts',(1.34972302439372,67.7304157474343,10.0312337765259));
#63472=CARTESIAN_POINT('Ctrl Pts',(3.20979566340669,68.0305566352042,11.8234267010217));
#63473=CARTESIAN_POINT('Ctrl Pts',(3.34824042881676,68.3301416822406,14.3956206465524));
#63474=CARTESIAN_POINT('Ctrl Pts',(1.70258445179397,68.6286247069719,16.3655002185839));
#63475=CARTESIAN_POINT('Ctrl Pts',(-0.831063048028466,68.925518325864,16.6831831571466));
#63476=CARTESIAN_POINT('Ctrl Pts',(-2.9951653111011,69.2360019893962,15.1184813022997));
#63477=CARTESIAN_POINT('Ctrl Pts',(-3.25584874066971,69.4462318293195,13.2892070871188));
#63478=CARTESIAN_POINT('Ctrl Pts',(-2.98385582114668,69.5584198052059,12.4305287597433));
#63479=CARTESIAN_POINT('Ctrl Pts',(1.36952200671963,56.456522023403,11.210153809184));
#63480=CARTESIAN_POINT('Ctrl Pts',(1.46915479225293,56.4711352014148,11.2795181510653));
#63481=CARTESIAN_POINT('Ctrl Pts',(1.56373629895278,56.485870845212,11.3557719878152));
#63482=CARTESIAN_POINT('Ctrl Pts',(1.65197830956387,56.5006895712442,11.4383671401521));
#63483=CARTESIAN_POINT('Ctrl Pts',(1.70737706113225,56.5099928375267,11.4902207673913));
#63484=CARTESIAN_POINT('Ctrl Pts',(1.76027691285286,56.5193288095134,11.5445726741234));
#63485=CARTESIAN_POINT('Ctrl Pts',(1.81035947915606,56.5286873433543,11.601276770048));
#63486=CARTESIAN_POINT('Ctrl Pts',(1.88979050117883,56.543529991455,11.6912095475521));
#63487=CARTESIAN_POINT('Ctrl Pts',(1.96213299726991,56.558429483682,11.7870613695224));
#63488=CARTESIAN_POINT('Ctrl Pts',(2.02695886821799,56.5733438778432,11.8875325464049));
#63489=CARTESIAN_POINT('Ctrl Pts',(2.09252685586196,56.5884290097169,11.9891539020159));
#63490=CARTESIAN_POINT('Ctrl Pts',(2.15040431437628,56.6035293837288,12.095499941867));
#63491=CARTESIAN_POINT('Ctrl Pts',(2.20018409192502,56.6185997150804,12.2051859417651));
#63492=CARTESIAN_POINT('Ctrl Pts',(2.24899952968614,56.6333781021757,12.3127470913916));
#63493=CARTESIAN_POINT('Ctrl Pts',(2.29002742551468,56.6481275864915,12.4235187978667));
#63494=CARTESIAN_POINT('Ctrl Pts',(2.32292804780908,56.6628037938509,12.5361744777578));
#63495=CARTESIAN_POINT('Ctrl Pts',(2.34058678061769,56.6706809465104,12.5966400985223));
#63496=CARTESIAN_POINT('Ctrl Pts',(2.35590503222919,56.6785369620146,12.6576482027778));
#63497=CARTESIAN_POINT('Ctrl Pts',(2.36883652287042,56.6863647942985,12.7189930735352));
#63498=CARTESIAN_POINT('Ctrl Pts',(2.39398426951609,56.7015875051616,12.8382898592361));
#63499=CARTESIAN_POINT('Ctrl Pts',(2.41022684587955,56.7168011823224,12.9592973300442));
#63500=CARTESIAN_POINT('Ctrl Pts',(2.41708988396143,56.73199278412,13.0805678610677));
#63501=CARTESIAN_POINT('Ctrl Pts',(2.42441418136815,56.7482054013782,13.2099888879205));
#63502=CARTESIAN_POINT('Ctrl Pts',(2.4210541734813,56.7643928764075,13.3397084907732));
#63503=CARTESIAN_POINT('Ctrl Pts',(2.40748602314114,56.7805392535346,13.4680953009946));
#63504=CARTESIAN_POINT('Ctrl Pts',(2.39363959749359,56.7970167839836,13.5991152541414));
#63505=CARTESIAN_POINT('Ctrl Pts',(2.36916218100632,56.8134515121532,13.7287459024911));
#63506=CARTESIAN_POINT('Ctrl Pts',(2.33461478926672,56.8298263323069,13.8552462620182));
#63507=CARTESIAN_POINT('Ctrl Pts',(2.30038099907859,56.8460525111668,13.9805983233087));
#63508=CARTESIAN_POINT('Ctrl Pts',(2.25625968067984,56.8622198625916,14.1028753579633));
#63509=CARTESIAN_POINT('Ctrl Pts',(2.20284497159892,56.8783116252546,14.2203959349855));
#63510=CARTESIAN_POINT('Ctrl Pts',(2.16523804021797,56.8896411227784,14.3031369692805));
#63511=CARTESIAN_POINT('Ctrl Pts',(2.12302543917162,56.9009331488864,14.383520485037));
#63512=CARTESIAN_POINT('Ctrl Pts',(2.07642721540174,56.9121818271769,14.4609687618267));
#63513=CARTESIAN_POINT('Ctrl Pts',(2.05084753377501,56.9183566893522,14.5034833064283));
#63514=CARTESIAN_POINT('Ctrl Pts',(2.02393973676091,56.9245292662071,14.5451342256592));
#63515=CARTESIAN_POINT('Ctrl Pts',(1.99573526534201,56.9306991957531,14.5858283392573));
#63516=CARTESIAN_POINT('Ctrl Pts',(1.87461643961411,56.9571948038551,14.760581596634));
#63517=CARTESIAN_POINT('Ctrl Pts',(1.72958135983153,56.9836417604212,14.9176889956811));
#63518=CARTESIAN_POINT('Ctrl Pts',(1.56726157064771,57.0100104770603,15.0528795939312));
#63519=CARTESIAN_POINT('Ctrl Pts',(1.41029786293072,57.0355091026574,15.1836092951987));
#63520=CARTESIAN_POINT('Ctrl Pts',(1.23717304322571,57.0609345399046,15.2938430214388));
#63521=CARTESIAN_POINT('Ctrl Pts',(1.05391732366964,57.0862582787262,15.3797486128614));
#63522=CARTESIAN_POINT('Ctrl Pts',(0.959359416725181,57.0993250454541,15.4240749396982));
#63523=CARTESIAN_POINT('Ctrl Pts',(0.862104619060483,57.1123647089386,15.4619246795065));
#63524=CARTESIAN_POINT('Ctrl Pts',(0.762982644582906,57.1253731946399,15.4927768488092));
#63525=CARTESIAN_POINT('Ctrl Pts',(0.745090725751282,57.1277212791239,15.4983457906292));
#63526=CARTESIAN_POINT('Ctrl Pts',(0.727137971166554,57.1300683475208,15.5036867518304));
#63527=CARTESIAN_POINT('Ctrl Pts',(0.709129923407988,57.1324143756952,15.5088003294947));
#63528=CARTESIAN_POINT('Ctrl Pts',(0.576167781695582,57.1497362383857,15.5465563509793));
#63529=CARTESIAN_POINT('Ctrl Pts',(0.440014625634233,57.166977374934,15.5719390453827));
#63530=CARTESIAN_POINT('Ctrl Pts',(0.30295689367336,57.1841542470737,15.5851230291766));
#63531=CARTESIAN_POINT('Ctrl Pts',(0.162785739243805,57.2017213114258,15.5986065021769));
#63532=CARTESIAN_POINT('Ctrl Pts',(0.0216699639080719,57.2192211623843,
15.5993309988529));
#63533=CARTESIAN_POINT('Ctrl Pts',(-0.117938738247654,57.2366727970848,
15.5875382594333));
#63534=CARTESIAN_POINT('Ctrl Pts',(-0.255122987319975,57.2538213656518,
15.5759503134328));
#63535=CARTESIAN_POINT('Ctrl Pts',(-0.390850693548286,57.2709233908915,
15.5522766269456));
#63536=CARTESIAN_POINT('Ctrl Pts',(-0.522811632813748,57.2879980833134,
15.5167927491621));
#63537=CARTESIAN_POINT('Ctrl Pts',(-0.594243683425765,57.2972408205965,
15.4975848974458));
#63538=CARTESIAN_POINT('Ctrl Pts',(-0.664572399923294,57.3064755683326,
15.4749171931375));
#63539=CARTESIAN_POINT('Ctrl Pts',(-0.73343539588025,57.315705502545,15.4488383768472));
#63540=CARTESIAN_POINT('Ctrl Pts',(-0.812199921677987,57.3262625714219,
15.4190097937318));
#63541=CARTESIAN_POINT('Ctrl Pts',(-0.889046791608116,57.3368133410116,
15.3847187452103));
#63542=CARTESIAN_POINT('Ctrl Pts',(-0.963590004270745,57.3473627169651,
15.3463487943232));
#63543=CARTESIAN_POINT('Ctrl Pts',(-1.08193195564432,57.3641105024645,15.2854341288574));
#63544=CARTESIAN_POINT('Ctrl Pts',(-1.19471796432954,57.3807339436101,15.214041258376));
#63545=CARTESIAN_POINT('Ctrl Pts',(-1.3003244675683,57.3972693450953,15.1336235297956));
#63546=CARTESIAN_POINT('Ctrl Pts',(-1.41254409492565,57.4148402004495,15.0481700088717));
#63547=CARTESIAN_POINT('Ctrl Pts',(-1.51665560727272,57.4323116416365,14.9525269778875));
#63548=CARTESIAN_POINT('Ctrl Pts',(-1.61074790517429,57.4497293507773,14.848487847841));
#63549=CARTESIAN_POINT('Ctrl Pts',(-1.70484020307585,57.4671470599181,14.7444487177944));
#63550=CARTESIAN_POINT('Ctrl Pts',(-1.78891233014478,57.4845110575209,14.6320149368002));
#63551=CARTESIAN_POINT('Ctrl Pts',(-1.8611057861045,57.5018689170491,14.5130081981115));
#63552=CARTESIAN_POINT('Ctrl Pts',(-1.9315731818671,57.5188117706735,14.3968467698753));
#63553=CARTESIAN_POINT('Ctrl Pts',(-1.99072369019082,57.5357488018311,14.2744246847192));
#63554=CARTESIAN_POINT('Ctrl Pts',(-2.03825416039261,57.5527258161985,14.1481060172276));
#63555=CARTESIAN_POINT('Ctrl Pts',(-2.04206738360015,57.5540878297639,14.1379718596571));
#63556=CARTESIAN_POINT('Ctrl Pts',(-2.04580584336057,57.5554501013471,14.1278126166248));
#63557=CARTESIAN_POINT('Ctrl Pts',(-2.04946939738334,57.5568126549421,14.1176295051128));
#63558=CARTESIAN_POINT('Ctrl Pts',(-2.08629397670067,57.5705084985468,14.015272942267));
#63559=CARTESIAN_POINT('Ctrl Pts',(-2.11552985890596,57.584067304602,13.9104423303983));
#63560=CARTESIAN_POINT('Ctrl Pts',(-2.13703900698149,57.5975463105243,13.8042550242954));
#63561=CARTESIAN_POINT('Ctrl Pts',(-2.15823222694189,57.610827335712,13.6996274059752));
#63562=CARTESIAN_POINT('Ctrl Pts',(-2.17192429643729,57.624030899012,13.5936813263486));
#63563=CARTESIAN_POINT('Ctrl Pts',(-2.17793518415767,57.6372124451921,13.4874740432984));
#63564=CARTESIAN_POINT('Ctrl Pts',(-2.18130687263158,57.6446063725771,13.4278991703739));
#63565=CARTESIAN_POINT('Ctrl Pts',(-2.18226084418098,57.6519933839862,13.3682420118614));
#63566=CARTESIAN_POINT('Ctrl Pts',(-2.18075809699843,57.6593833431459,13.3086899191046));
#63567=CARTESIAN_POINT('Ctrl Pts',(-2.17908779112742,57.667597294444,13.2424976737842));
#63568=CARTESIAN_POINT('Ctrl Pts',(-2.17438685459266,57.6758318257226,13.1764779016195));
#63569=CARTESIAN_POINT('Ctrl Pts',(-2.16660982827104,57.6840728077332,13.1109318190068));
#63570=CARTESIAN_POINT('Ctrl Pts',(-2.15443325449219,57.6969758019257,13.0083056122999));
#63571=CARTESIAN_POINT('Ctrl Pts',(-2.13471323311804,57.7098946288363,12.9068415882772));
#63572=CARTESIAN_POINT('Ctrl Pts',(-2.10799407319067,57.7227746974414,12.8075421459927));
#63573=CARTESIAN_POINT('Ctrl Pts',(-2.0812749132633,57.7356547660465,12.7082427037083));
#63574=CARTESIAN_POINT('Ctrl Pts',(-2.0475571847817,57.748496067773,12.6111090901458));
#63575=CARTESIAN_POINT('Ctrl Pts',(-2.00743360751768,57.7612436457027,12.5171219278902));
#63576=CARTESIAN_POINT('Ctrl Pts',(-1.95960297560244,57.7764398158685,12.4050814352636));
#63577=CARTESIAN_POINT('Ctrl Pts',(-1.90250269344863,57.7916004469951,12.297099083334));
#63578=CARTESIAN_POINT('Ctrl Pts',(-1.83697618143483,57.8067259564533,12.1948146325061));
#63579=CARTESIAN_POINT('Ctrl Pts',(-1.76997508043438,57.8221918458428,12.0902284030536));
#63580=CARTESIAN_POINT('Ctrl Pts',(-1.69416479782066,57.8376210170525,11.9916007489786));
#63581=CARTESIAN_POINT('Ctrl Pts',(-1.61049800291813,57.8530142661307,11.9006699114393));
#63582=CARTESIAN_POINT('Ctrl Pts',(-1.59288421178826,57.8562549002961,11.8815268716999));
#63583=CARTESIAN_POINT('Ctrl Pts',(-1.57492237912845,57.8594939435387,11.8627248618025));
#63584=CARTESIAN_POINT('Ctrl Pts',(-1.55662163580077,57.8627314050621,11.844279930786));
#63585=CARTESIAN_POINT('Ctrl Pts',(-1.46954820889466,57.8781349798938,11.756520470752));
#63586=CARTESIAN_POINT('Ctrl Pts',(-1.37480023118978,57.8935027266487,11.6768479525723));
#63587=CARTESIAN_POINT('Ctrl Pts',(-1.27418433883334,57.90883586577,11.606036012281));
#63588=CARTESIAN_POINT('Ctrl Pts',(-1.17428500528259,57.9240598064775,11.5357283752183));
#63589=CARTESIAN_POINT('Ctrl Pts',(-1.06860244194075,57.9392496346171,11.4741560655824));
#63590=CARTESIAN_POINT('Ctrl Pts',(-0.958921897657103,57.9544067765099,
11.4220290587066));
#63591=CARTESIAN_POINT('Ctrl Pts',(-0.942941105331535,57.9566152186581,
11.4144339936303));
#63592=CARTESIAN_POINT('Ctrl Pts',(-0.926875446568214,57.9588229672423,
11.4070393564504));
#63593=CARTESIAN_POINT('Ctrl Pts',(-0.91073044638101,57.9610300270125,11.3998472488055));
#63594=CARTESIAN_POINT('Ctrl Pts',(-0.802078772554052,57.9758829682009,
11.3514462252752));
#63595=CARTESIAN_POINT('Ctrl Pts',(-0.68951124289933,57.9906778732759,11.3120840084787));
#63596=CARTESIAN_POINT('Ctrl Pts',(-0.57468075747263,58.0054375483017,11.2825376714842));
#63597=CARTESIAN_POINT('Ctrl Pts',(-0.490862048121693,58.0162111412767,
11.2609707868392));
#63598=CARTESIAN_POINT('Ctrl Pts',(-0.405838698862453,58.0269659749054,
11.2446331488682));
#63599=CARTESIAN_POINT('Ctrl Pts',(-0.320263597472245,58.0377110484851,
11.2338127230293));
#63600=CARTESIAN_POINT('Ctrl Pts',(-0.262819530238262,58.0449239026813,
11.2265492870615));
#63601=CARTESIAN_POINT('Ctrl Pts',(-0.205127001097988,58.0521323611149,
11.2217716976632));
#63602=CARTESIAN_POINT('Ctrl Pts',(-0.147388309001223,58.0593391764746,
11.2194302960943));
#63603=CARTESIAN_POINT('Ctrl Pts',(-0.0354529472583231,58.0733106998155,
11.2148911279545));
#63604=CARTESIAN_POINT('Ctrl Pts',(0.0764822901895972,58.0872450371051,
11.2195100301769));
#63605=CARTESIAN_POINT('Ctrl Pts',(0.187089969165227,58.1011471073447,11.2328499431645));
#63606=CARTESIAN_POINT('Ctrl Pts',(0.301642484454331,58.1155449966091,11.2466656257701));
#63607=CARTESIAN_POINT('Ctrl Pts',(0.414772366645668,58.1299082752455,11.2698355625883));
#63608=CARTESIAN_POINT('Ctrl Pts',(0.525011184291908,58.1442421967197,11.3019287802839));
#63609=CARTESIAN_POINT('Ctrl Pts',(0.557083914043899,58.1484124880884,11.3112659368318));
#63610=CARTESIAN_POINT('Ctrl Pts',(0.588911895013926,58.1525802932436,11.3213587438726));
#63611=CARTESIAN_POINT('Ctrl Pts',(0.620458802335199,58.1567457385606,11.3321973951995));
#63612=CARTESIAN_POINT('Ctrl Pts',(0.720698748189065,58.169981394556,11.3666370887985));
#63613=CARTESIAN_POINT('Ctrl Pts',(0.818219758215847,58.1831868276257,11.4086523751259));
#63614=CARTESIAN_POINT('Ctrl Pts',(0.911694682471907,58.196363142706,11.4579120813134));
#63615=CARTESIAN_POINT('Ctrl Pts',(0.942996064161856,58.2007754155254,11.4744073807489));
#63616=CARTESIAN_POINT('Ctrl Pts',(0.973843827233434,58.2051844247905,11.491714600034));
#63617=CARTESIAN_POINT('Ctrl Pts',(1.00418852593819,58.2095902163625,11.5098200550111));
#63618=CARTESIAN_POINT('Ctrl Pts',(1.0952104818817,58.2228058284293,11.5641291763935));
#63619=CARTESIAN_POINT('Ctrl Pts',(1.18170356584887,58.2359924796513,11.6256236394623));
#63620=CARTESIAN_POINT('Ctrl Pts',(1.26282540655847,58.2491515207159,11.6932280698124));
#63621=CARTESIAN_POINT('Ctrl Pts',(1.33673971272878,58.2611414038553,11.7548259640374));
#63622=CARTESIAN_POINT('Ctrl Pts',(1.40619469115228,58.273108368793,11.8214951503265));
#63623=CARTESIAN_POINT('Ctrl Pts',(1.47058191229359,58.2850535092159,11.8923978684573));
#63624=CARTESIAN_POINT('Ctrl Pts',(1.55934551451336,58.3015209646234,11.990143672002));
#63625=CARTESIAN_POINT('Ctrl Pts',(1.63872811823348,58.3179912427726,12.0962091899425));
#63626=CARTESIAN_POINT('Ctrl Pts',(1.70711030016581,58.3344279546954,12.208568079396));
#63627=CARTESIAN_POINT('Ctrl Pts',(1.76850836920012,58.3491859273839,12.3094513600452));
#63628=CARTESIAN_POINT('Ctrl Pts',(1.82103804330843,58.363916839067,12.4154066166125));
#63629=CARTESIAN_POINT('Ctrl Pts',(1.86355177000897,58.3785946681204,12.5249412106564));
#63630=CARTESIAN_POINT('Ctrl Pts',(1.8958257431273,58.3897372307012,12.6080935668025));
#63631=CARTESIAN_POINT('Ctrl Pts',(1.9223280224056,58.400849207458,12.6933080865615));
#63632=CARTESIAN_POINT('Ctrl Pts',(1.94306795259562,58.4119193850068,12.7797880655436));
#63633=CARTESIAN_POINT('Ctrl Pts',(1.97369195728146,58.4282653016044,12.9074819997715));
#63634=CARTESIAN_POINT('Ctrl Pts',(1.99172875240901,58.4446042581234,13.0378664290804));
#63635=CARTESIAN_POINT('Ctrl Pts',(1.99726345184883,58.4609280668734,13.1685019735049));
#63636=CARTESIAN_POINT('Ctrl Pts',(2.00285136787762,58.4774088303831,13.3003935894014));
#63637=CARTESIAN_POINT('Ctrl Pts',(1.99569569652062,58.493874145555,13.4325428006213));
#63638=CARTESIAN_POINT('Ctrl Pts',(1.97583337247747,58.5103156295835,13.5624486156509));
#63639=CARTESIAN_POINT('Ctrl Pts',(1.96494735116715,58.5193267777814,13.6336466017313));
#63640=CARTESIAN_POINT('Ctrl Pts',(1.95024355218929,58.5283307689126,13.7041707270376));
#63641=CARTESIAN_POINT('Ctrl Pts',(1.93172152819956,58.5373262414551,13.7736076911243));
#63642=CARTESIAN_POINT('Ctrl Pts',(1.92646290178778,58.5398801648019,13.7933216842334));
#63643=CARTESIAN_POINT('Ctrl Pts',(1.92089668302801,58.5424317495683,13.8129486176893));
#63644=CARTESIAN_POINT('Ctrl Pts',(1.91502289079323,58.5449811871001,13.8324784185738));
#63645=CARTESIAN_POINT('Ctrl Pts',(1.88328902704021,58.5587548277138,13.9379904992913));
#63646=CARTESIAN_POINT('Ctrl Pts',(1.84257471791898,58.5724658315662,14.040667129551));
#63647=CARTESIAN_POINT('Ctrl Pts',(1.79383537303964,58.5861443504739,14.1390694208639));
#63648=CARTESIAN_POINT('Ctrl Pts',(1.74509660439038,58.5998227076647,14.2374705487971));
#63649=CARTESIAN_POINT('Ctrl Pts',(1.68833337657972,58.6134685911499,14.3315967117396));
#63650=CARTESIAN_POINT('Ctrl Pts',(1.6243790725386,58.6271113319548,14.4204004062708));
#63651=CARTESIAN_POINT('Ctrl Pts',(1.57100352011599,58.6384974120308,14.4945149842313));
#63652=CARTESIAN_POINT('Ctrl Pts',(1.51261982577684,58.6498812961438,14.5649221359379));
#63653=CARTESIAN_POINT('Ctrl Pts',(1.44983275270448,58.6612796689561,14.6308315551199));
#63654=CARTESIAN_POINT('Ctrl Pts',(1.38345085869734,58.6733306459941,14.7005145625308));
#63655=CARTESIAN_POINT('Ctrl Pts',(1.31201748268334,58.685294084935,14.7653544008138));
#63656=CARTESIAN_POINT('Ctrl Pts',(1.23624186293984,58.6971928215782,14.8243406496));
#63657=CARTESIAN_POINT('Ctrl Pts',(1.21186318343082,58.7010209062335,14.8433178200865));
#63658=CARTESIAN_POINT('Ctrl Pts',(1.18703539965888,58.7048422908144,14.8616893301434));
#63659=CARTESIAN_POINT('Ctrl Pts',(1.16178303325293,58.7086577263161,14.8794222478575));
#63660=CARTESIAN_POINT('Ctrl Pts',(1.07934652366972,58.7211132396032,14.9373114697061));
#63661=CARTESIAN_POINT('Ctrl Pts',(0.992382662271615,58.7335054044598,14.9883910564383));
#63662=CARTESIAN_POINT('Ctrl Pts',(0.902162503100363,58.7458600482291,15.0324453600377));
#63663=CARTESIAN_POINT('Ctrl Pts',(0.811942343929102,58.7582146919983,15.0764996636372));
#63664=CARTESIAN_POINT('Ctrl Pts',(0.718467402301991,58.7705318247608,15.1135283473514));
#63665=CARTESIAN_POINT('Ctrl Pts',(0.623030282885385,58.7828365159479,15.143373103638));
#63666=CARTESIAN_POINT('Ctrl Pts',(0.517947159259993,58.7963848647779,15.1762343240269));
#63667=CARTESIAN_POINT('Ctrl Pts',(0.410297161681419,58.8100682620767,15.2004102053103));
#63668=CARTESIAN_POINT('Ctrl Pts',(0.301564826465718,58.8238266280958,15.2157189812137));
#63669=CARTESIAN_POINT('Ctrl Pts',(0.195041967533067,58.8373054196594,15.2307166778303));
#63670=CARTESIAN_POINT('Ctrl Pts',(0.0874789688953521,58.8508561503634,
15.2372043414448));
#63671=CARTESIAN_POINT('Ctrl Pts',(-0.0197408061838438,58.8644239434151,
15.2349638258398));
#63672=CARTESIAN_POINT('Ctrl Pts',(-0.12696058126305,58.8779917364668,15.2327233102347));
#63673=CARTESIAN_POINT('Ctrl Pts',(-0.233838514980572,58.8915765723245,
15.2217552850595));
#63674=CARTESIAN_POINT('Ctrl Pts',(-0.33898369743854,58.9051254605321,15.2017859192415));
#63675=CARTESIAN_POINT('Ctrl Pts',(-0.388101430627564,58.911454715572,15.1924573893053));
#63676=CARTESIAN_POINT('Ctrl Pts',(-0.436804588784485,58.9177326978257,
15.181186213811));
#63677=CARTESIAN_POINT('Ctrl Pts',(-0.48493597423247,58.9239726430724,15.1679472005774));
#63678=CARTESIAN_POINT('Ctrl Pts',(-0.590618795069899,58.9376737865031,
15.1388780962786));
#63679=CARTESIAN_POINT('Ctrl Pts',(-0.693545745303446,58.9511918737145,
15.1003183673063));
#63680=CARTESIAN_POINT('Ctrl Pts',(-0.792416488328475,58.964663578416,15.0533507465721));
#63681=CARTESIAN_POINT('Ctrl Pts',(-0.88980790192202,58.9779337160143,15.0070858674332));
#63682=CARTESIAN_POINT('Ctrl Pts',(-0.983262368726927,58.9911588756171,
14.9526627861704));
#63683=CARTESIAN_POINT('Ctrl Pts',(-1.07153430160592,59.0044647352171,14.8911656444755));
#63684=CARTESIAN_POINT('Ctrl Pts',(-1.11674862865751,59.0112802140226,14.859665803171));
#63685=CARTESIAN_POINT('Ctrl Pts',(-1.16060329803473,59.0181167827722,14.8263107762819));
#63686=CARTESIAN_POINT('Ctrl Pts',(-1.20293243047534,59.024990783203,14.7912513816117));
#63687=CARTESIAN_POINT('Ctrl Pts',(-1.29308763872583,59.0396314551145,14.7165797111713));
#63688=CARTESIAN_POINT('Ctrl Pts',(-1.3766548618386,59.0545307734405,14.6338784592106));
#63689=CARTESIAN_POINT('Ctrl Pts',(-1.4521181887582,59.0694624048309,14.5445224940884));
#63690=CARTESIAN_POINT('Ctrl Pts',(-1.52508091871205,59.0838992529447,14.458127480522));
#63691=CARTESIAN_POINT('Ctrl Pts',(-1.59046897631651,59.0983662889856,14.3655135371929));
#63692=CARTESIAN_POINT('Ctrl Pts',(-1.64695323383549,59.1126678517981,14.2679037639584));
#63693=CARTESIAN_POINT('Ctrl Pts',(-1.67968449607391,59.1209552618376,14.2113412591986));
#63694=CARTESIAN_POINT('Ctrl Pts',(-1.70942665510631,59.1291872755138,14.1531006644654));
#63695=CARTESIAN_POINT('Ctrl Pts',(-1.73592496734939,59.1373273010696,14.0934128830763));
#63696=CARTESIAN_POINT('Ctrl Pts',(-1.74601632931443,59.1404272699859,14.0706819634101));
#63697=CARTESIAN_POINT('Ctrl Pts',(-1.75563724386547,59.1435139094074,14.0477410856583));
#63698=CARTESIAN_POINT('Ctrl Pts',(-1.76478956866252,59.1465852431225,14.0246091300138));
#63699=CARTESIAN_POINT('Ctrl Pts',(-1.80536798654199,59.1602025333413,13.922049596417));
#63700=CARTESIAN_POINT('Ctrl Pts',(-1.83657035143438,59.1736094947579,13.8159541542144));
#63701=CARTESIAN_POINT('Ctrl Pts',(-1.8584594990833,59.1869805087201,13.708080846563));
#63702=CARTESIAN_POINT('Ctrl Pts',(-1.86827580838667,59.192976813869,13.6597044652407));
#63703=CARTESIAN_POINT('Ctrl Pts',(-1.8762193674693,59.1989657744317,13.6109711615938));
#63704=CARTESIAN_POINT('Ctrl Pts',(-1.88229770380362,59.2049625373459,13.5620423520191));
#63705=CARTESIAN_POINT('Ctrl Pts',(-1.89325814455268,59.2157758851095,13.4738140459876));
#63706=CARTESIAN_POINT('Ctrl Pts',(-1.89815786692028,59.2266198901948,13.3849386548247));
#63707=CARTESIAN_POINT('Ctrl Pts',(-1.89705304640125,59.2375636303809,13.2962222606873));
#63708=CARTESIAN_POINT('Ctrl Pts',(-1.89617891964835,59.2462222458833,13.2260304311549));
#63709=CARTESIAN_POINT('Ctrl Pts',(-1.89154479315468,59.2549432457717,13.1559378089459));
#63710=CARTESIAN_POINT('Ctrl Pts',(-1.88315639628323,59.2637596239283,13.0863502148045));
#63711=CARTESIAN_POINT('Ctrl Pts',(-1.87190005597408,59.2755902698008,12.9929710324704));
#63712=CARTESIAN_POINT('Ctrl Pts',(-1.85392161476602,59.2875105766096,12.9003063603965));
#63713=CARTESIAN_POINT('Ctrl Pts',(-1.82927755571808,59.2994348418841,12.8095092266655));
#63714=CARTESIAN_POINT('Ctrl Pts',(-1.80470413682341,59.3113249272402,12.718972355395));
#63715=CARTESIAN_POINT('Ctrl Pts',(-1.77350406515564,59.3232189330005,12.6302935786374));
#63716=CARTESIAN_POINT('Ctrl Pts',(-1.73577654944931,59.33503556681,12.544589431288));
#63717=CARTESIAN_POINT('Ctrl Pts',(-1.72310881099013,59.3390032287078,12.5158126167228));
#63718=CARTESIAN_POINT('Ctrl Pts',(-1.70970546851552,59.342962199326,12.4873708617542));
#63719=CARTESIAN_POINT('Ctrl Pts',(-1.69557111796058,59.3469094990656,12.459305403527));
#63720=CARTESIAN_POINT('Ctrl Pts',(-1.65390985097694,59.3585442400944,12.3765819318206));
#63721=CARTESIAN_POINT('Ctrl Pts',(-1.60589658641429,59.3700772980045,12.2971313838428));
#63722=CARTESIAN_POINT('Ctrl Pts',(-1.55240337212546,59.3814349689118,12.2215710200243));
#63723=CARTESIAN_POINT('Ctrl Pts',(-1.54939948336779,59.3820727541039,12.2173279598452));
#63724=CARTESIAN_POINT('Ctrl Pts',(-1.54637831753911,59.3827099872707,12.2130971534733));
#63725=CARTESIAN_POINT('Ctrl Pts',(-1.5433400298968,59.38334665573,12.2088787054353));
#63726=CARTESIAN_POINT('Ctrl Pts',(-1.48531316216982,59.3955060957916,12.1283124934336));
#63727=CARTESIAN_POINT('Ctrl Pts',(-1.42093213095254,59.4077161778422,12.0524321900086));
#63728=CARTESIAN_POINT('Ctrl Pts',(-1.35115712210107,59.4199965915774,11.9819264213592));
#63729=CARTESIAN_POINT('Ctrl Pts',(-1.28018237202813,59.432488159977,11.9102083464931));
#63730=CARTESIAN_POINT('Ctrl Pts',(-1.20362531570199,59.4450525045962,11.8440503158963));
#63731=CARTESIAN_POINT('Ctrl Pts',(-1.12245738108134,59.4577094768668,11.7842139500287));
#63732=CARTESIAN_POINT('Ctrl Pts',(-1.04285713935044,59.4701219899734,11.7255332750846));
#63733=CARTESIAN_POINT('Ctrl Pts',(-0.958821080636736,59.4826235875242,
11.6729318434965));
#63734=CARTESIAN_POINT('Ctrl Pts',(-0.871247569242309,59.4952321297453,
11.627173841781));
#63735=CARTESIAN_POINT('Ctrl Pts',(-0.856026546876538,59.4974236018022,
11.619220711246));
#63736=CARTESIAN_POINT('Ctrl Pts',(-0.840698643668718,59.4996183024387,
11.61147444279));
#63737=CARTESIAN_POINT('Ctrl Pts',(-0.825268565222567,59.5018163226858,
11.6039392134727));
#63738=CARTESIAN_POINT('Ctrl Pts',(-0.749854981388678,59.5125590149383,
11.5671112316964));
#63739=CARTESIAN_POINT('Ctrl Pts',(-0.671975232143976,59.5232278785692,
11.5351623712557));
#63740=CARTESIAN_POINT('Ctrl Pts',(-0.592288075088419,59.5338228938777,
11.5086453437354));
#63741=CARTESIAN_POINT('Ctrl Pts',(-0.534497448341847,59.5415065984757,
11.4894146960817));
#63742=CARTESIAN_POINT('Ctrl Pts',(-0.475757099452308,59.5491514566829,
11.4730402248142));
#63743=CARTESIAN_POINT('Ctrl Pts',(-0.416327025131937,59.5567573322003,
11.4597179131493));
#63744=CARTESIAN_POINT('Ctrl Pts',(-0.332861466849647,59.5674392748622,
11.4410076188507));
#63745=CARTESIAN_POINT('Ctrl Pts',(-0.248035654363545,59.5780443502871,
11.4283199523734));
#63746=CARTESIAN_POINT('Ctrl Pts',(-0.162744825157152,59.5885717398189,
11.4214702052937));
#63747=CARTESIAN_POINT('Ctrl Pts',(-0.0774539959507597,59.5990991293507,
11.414620458214));
#63748=CARTESIAN_POINT('Ctrl Pts',(0.00830053247729802,59.609548837757,
11.4136083750919));
#63749=CARTESIAN_POINT('Ctrl Pts',(0.0936270681948237,59.6199194861507,
11.4181939671387));
#63750=CARTESIAN_POINT('Ctrl Pts',(0.186566867222982,59.6312154560315,11.4231887088057));
#63751=CARTESIAN_POINT('Ctrl Pts',(0.279136406833507,59.6426668287692,11.4350438175505));
#63752=CARTESIAN_POINT('Ctrl Pts',(0.370372628682501,59.654224037212,11.4534565807964));
#63753=CARTESIAN_POINT('Ctrl Pts',(0.462195851790772,59.6658556031389,11.4719878092199));
#63754=CARTESIAN_POINT('Ctrl Pts',(0.552669731572818,59.6775943565418,11.4971608886472));
#63755=CARTESIAN_POINT('Ctrl Pts',(0.640837575008383,59.6893935521328,11.5287134846517));
#63756=CARTESIAN_POINT('Ctrl Pts',(0.726403413497647,59.700844530459,11.5593349020351));
#63757=CARTESIAN_POINT('Ctrl Pts',(0.809798661279672,59.7123524427399,11.5959646870322));
#63758=CARTESIAN_POINT('Ctrl Pts',(0.890153554389046,59.7238781358003,11.6384105630698));
#63759=CARTESIAN_POINT('Ctrl Pts',(0.92372720212957,59.7286937673543,11.6561451755493));
#63760=CARTESIAN_POINT('Ctrl Pts',(0.956770035111332,59.7335125461735,11.6748957055525));
#63761=CARTESIAN_POINT('Ctrl Pts',(0.989217984613843,59.7383318061232,11.6946508071429));
#63762=CARTESIAN_POINT('Ctrl Pts',(1.0505133797862,59.7474355691525,11.7319689359375));
#63763=CARTESIAN_POINT('Ctrl Pts',(1.10970588496588,59.7564248801717,11.7727467116865));
#63764=CARTESIAN_POINT('Ctrl Pts',(1.16628383133372,59.7653417868353,11.8169196632499));
#63765=CARTESIAN_POINT('Ctrl Pts',(1.23412840109227,59.7760343576161,11.8698889752554));
#63766=CARTESIAN_POINT('Ctrl Pts',(1.29821302930044,59.7866229642167,11.9277420092064));
#63767=CARTESIAN_POINT('Ctrl Pts',(1.35807742641337,59.7971752733908,11.989773943096));
#63768=CARTESIAN_POINT('Ctrl Pts',(1.41801592431191,59.8077406443252,12.0518826607712));
#63769=CARTESIAN_POINT('Ctrl Pts',(1.47372275725937,59.8182696433691,12.1181806836443));
#63770=CARTESIAN_POINT('Ctrl Pts',(1.52473198283119,59.828824653008,12.1879088572466));
#63771=CARTESIAN_POINT('Ctrl Pts',(1.5671879292086,59.8376097878188,12.2459449392742));
#63772=CARTESIAN_POINT('Ctrl Pts',(1.60638916190907,59.8464128458041,12.3063562701437));
#63773=CARTESIAN_POINT('Ctrl Pts',(1.64207304820684,59.8552667761938,12.3686783630951));
#63774=CARTESIAN_POINT('Ctrl Pts',(1.68474217136199,59.8658538922679,12.4432002085365));
#63775=CARTESIAN_POINT('Ctrl Pts',(1.72240275794083,59.8766262430058,12.5206967959212));
#63776=CARTESIAN_POINT('Ctrl Pts',(1.75474908250705,59.8874898709194,12.6003740149981));
#63777=CARTESIAN_POINT('Ctrl Pts',(1.78696605902631,59.8983100568324,12.6797326169582));
#63778=CARTESIAN_POINT('Ctrl Pts',(1.81391228100278,59.9092207784099,12.761253861667));
#63779=CARTESIAN_POINT('Ctrl Pts',(1.83531021566769,59.9201363585182,12.8441978620612));
#63780=CARTESIAN_POINT('Ctrl Pts',(1.85629914264622,59.9308432943701,12.9255564415149));
#63781=CARTESIAN_POINT('Ctrl Pts',(1.87195111963573,59.9415549103696,13.0082837455269));
#63782=CARTESIAN_POINT('Ctrl Pts',(1.88201041978646,59.9521972755145,13.0917298756377));
#63783=CARTESIAN_POINT('Ctrl Pts',(1.88913208181775,59.9597317288702,13.1508070606866));
#63784=CARTESIAN_POINT('Ctrl Pts',(1.89345078665872,59.9672316148274,13.210245563423));
#63785=CARTESIAN_POINT('Ctrl Pts',(1.89487217930387,59.9746728473432,13.2698301275761));
#63786=CARTESIAN_POINT('Ctrl Pts',(1.89490682209874,59.9748542082729,13.2712823482843));
#63787=CARTESIAN_POINT('Ctrl Pts',(1.89493974355676,59.9750355344513,13.2727346563888));
#63788=CARTESIAN_POINT('Ctrl Pts',(1.89497094555377,59.9752168255432,13.2741870487142));
#63789=CARTESIAN_POINT('Ctrl Pts',(1.89677829811965,59.9857179777607,13.3583157983999));
#63790=CARTESIAN_POINT('Ctrl Pts',(1.89280614713868,59.9960846861283,13.4425444573657));
#63791=CARTESIAN_POINT('Ctrl Pts',(1.88326890729464,60.0064013269797,13.5262189405871));
#63792=CARTESIAN_POINT('Ctrl Pts',(1.87373988880451,60.0167090746129,13.609821294183));
#63793=CARTESIAN_POINT('Ctrl Pts',(1.85865402480473,60.0269668514144,13.6928706812733));
#63794=CARTESIAN_POINT('Ctrl Pts',(1.83821308355048,60.0372517759125,13.7746646005829));
#63795=CARTESIAN_POINT('Ctrl Pts',(1.81795152205156,60.0474464449171,13.8557407362518));
#63796=CARTESIAN_POINT('Ctrl Pts',(1.79242724450045,60.0576677876008,13.9355831774851));
#63797=CARTESIAN_POINT('Ctrl Pts',(1.76184393626309,60.0679839244412,14.0134579846426));
#63798=CARTESIAN_POINT('Ctrl Pts',(1.73773376718324,60.0761165895389,14.0748501255142));
#63799=CARTESIAN_POINT('Ctrl Pts',(1.71047943775938,60.0843080332466,14.1350183263249));
#63800=CARTESIAN_POINT('Ctrl Pts',(1.68019112349398,60.0925885199882,14.1935827800625));
#63801=CARTESIAN_POINT('Ctrl Pts',(1.64617234989821,60.1018888726343,14.2593603230119));
#63802=CARTESIAN_POINT('Ctrl Pts',(1.60827967828574,60.1113122103187,14.3232153087731));
#63803=CARTESIAN_POINT('Ctrl Pts',(1.56681116476779,60.1207766078547,14.3847055551712));
#63804=CARTESIAN_POINT('Ctrl Pts',(1.52570925077873,60.1301573360381,14.4456522012942));
#63805=CARTESIAN_POINT('Ctrl Pts',(1.48109535301017,60.1395783988457,14.5042762946321));
#63806=CARTESIAN_POINT('Ctrl Pts',(1.43323386744353,60.1489670428787,14.5601903354092));
#63807=CARTESIAN_POINT('Ctrl Pts',(1.3909742468693,60.157256809271,14.6095600137641));
#63808=CARTESIAN_POINT('Ctrl Pts',(1.34618279641613,60.1655213958391,14.6568178708656));
#63809=CARTESIAN_POINT('Ctrl Pts',(1.29901616765672,60.1737153708029,14.7017191651865));
#63810=CARTESIAN_POINT('Ctrl Pts',(1.27653538709293,60.1776208217108,14.7231202313896));
#63811=CARTESIAN_POINT('Ctrl Pts',(1.25354142483049,60.1814968462128,14.743987430385));
#63812=CARTESIAN_POINT('Ctrl Pts',(1.23003893721349,60.1853508455441,14.7642795404087));
#63813=CARTESIAN_POINT('Ctrl Pts',(1.17850318108619,60.1938018134966,14.8087756486729));
#63814=CARTESIAN_POINT('Ctrl Pts',(1.1245194032915,60.202147329404,14.8505083976961));
#63815=CARTESIAN_POINT('Ctrl Pts',(1.06840191913485,60.2104604779086,14.8892670571694));
#63816=CARTESIAN_POINT('Ctrl Pts',(1.01245611748207,60.2187481936596,14.9279071406979));
#63817=CARTESIAN_POINT('Ctrl Pts',(0.954389243181839,60.2270037432293,14.9635904930496));
#63818=CARTESIAN_POINT('Ctrl Pts',(0.894559103236365,60.2352927338508,14.9960864424661));
#63819=CARTESIAN_POINT('Ctrl Pts',(0.853701766196935,60.2409531933424,15.0182775648491));
#63820=CARTESIAN_POINT('Ctrl Pts',(0.812023143287833,60.2466291062208,15.0389818208246));
#63821=CARTESIAN_POINT('Ctrl Pts',(0.769650774154881,60.2523395235873,15.0581229548416));
#63822=CARTESIAN_POINT('Ctrl Pts',(0.689645595206691,60.2631216198597,15.0942641922478));
#63823=CARTESIAN_POINT('Ctrl Pts',(0.606941476645531,60.2740524261799,15.1249449266891));
#63824=CARTESIAN_POINT('Ctrl Pts',(0.522444982365712,60.285071073973,15.149965228729));
#63825=CARTESIAN_POINT('Ctrl Pts',(0.437621342071081,60.2961323827871,15.1750824021499));
#63826=CARTESIAN_POINT('Ctrl Pts',(0.350992113414438,60.307282198988,15.1944962313341));
#63827=CARTESIAN_POINT('Ctrl Pts',(0.263432036152865,60.3184657956524,15.2080342251105));
#63828=CARTESIAN_POINT('Ctrl Pts',(0.176159419448295,60.3296126764638,15.2215277735259));
#63829=CARTESIAN_POINT('Ctrl Pts',(0.0879623625203319,60.3407931092736,
15.2291851981355));
#63830=CARTESIAN_POINT('Ctrl Pts',(-0.000342428140762663,60.35195985489,
15.2308486929397));
#63831=CARTESIAN_POINT('Ctrl Pts',(-0.0873515597100696,60.3629627555396,
15.2324877799835));
#63832=CARTESIAN_POINT('Ctrl Pts',(-0.174465405949206,60.3739523744458,
15.2283088106122));
#63833=CARTESIAN_POINT('Ctrl Pts',(-0.260951948886756,60.3848902619989,
15.2181551593732));
#63834=CARTESIAN_POINT('Ctrl Pts',(-0.295577040787573,60.3892692711356,
15.2140901210986));
#63835=CARTESIAN_POINT('Ctrl Pts',(-0.330102133728782,60.3936400645258,
15.2090672793448));
#63836=CARTESIAN_POINT('Ctrl Pts',(-0.364482390228697,60.3980004808765,
15.2030755991657));
#63837=CARTESIAN_POINT('Ctrl Pts',(-0.407226977467079,60.4034217376114,
15.195626210412));
#63838=CARTESIAN_POINT('Ctrl Pts',(-0.449747605612096,60.4088269411944,
15.1866792819153));
#63839=CARTESIAN_POINT('Ctrl Pts',(-0.491974712434599,60.414212316012,15.176297632117));
#63840=CARTESIAN_POINT('Ctrl Pts',(-0.588087657829569,60.4264699456419,
15.1526680014071));
#63841=CARTESIAN_POINT('Ctrl Pts',(-0.682389832285348,60.4387055858607,
15.1214097839479));
#63842=CARTESIAN_POINT('Ctrl Pts',(-0.773961605253539,60.4509579910253,
15.0831399777681));
#63843=CARTESIAN_POINT('Ctrl Pts',(-0.868104331035284,60.4635543925384,
15.0437957153156));
#63844=CARTESIAN_POINT('Ctrl Pts',(-0.959361818712132,60.4761685462156,
14.9970390198292));
#63845=CARTESIAN_POINT('Ctrl Pts',(-1.04668730101127,60.4888365227693,14.9435163114177));
#63846=CARTESIAN_POINT('Ctrl Pts',(-1.13321362150058,60.5013885679499,14.8904834177017));
#63847=CARTESIAN_POINT('Ctrl Pts',(-1.2158795732269,60.5139934528858,14.8308062486209));
#63848=CARTESIAN_POINT('Ctrl Pts',(-1.29361658023214,60.5266802484715,14.7651142565974));
#63849=CARTESIAN_POINT('Ctrl Pts',(-1.36959167559692,60.5390794974474,14.7009111755816));
#63850=CARTESIAN_POINT('Ctrl Pts',(-1.44085830285566,60.5515569720563,14.6309616720683));
#63851=CARTESIAN_POINT('Ctrl Pts',(-1.50637402923232,60.5641341783868,14.5558736210541));
#63852=CARTESIAN_POINT('Ctrl Pts',(-1.52762443586511,60.5682136683599,14.53151837529));
#63853=CARTESIAN_POINT('Ctrl Pts',(-1.54826947951281,60.5723036066061,14.5066227524367));
#63854=CARTESIAN_POINT('Ctrl Pts',(-1.56827268040012,60.5764045990175,14.4812082615031));
#63855=CARTESIAN_POINT('Ctrl Pts',(-1.62937100982656,60.5889307835386,14.4035815382592));
#63856=CARTESIAN_POINT('Ctrl Pts',(-1.68486113862731,60.6014260076282,14.3213353076629));
#63857=CARTESIAN_POINT('Ctrl Pts',(-1.73373650575351,60.6139032535682,14.2350744823463));
#63858=CARTESIAN_POINT('Ctrl Pts',(-1.78382192982385,60.6266894113177,14.146678010449));
#63859=CARTESIAN_POINT('Ctrl Pts',(-1.8269594190976,60.6394567134822,14.0540656621294));
#63860=CARTESIAN_POINT('Ctrl Pts',(-1.86279055072064,60.652215379453,13.9584928980425));
#63861=CARTESIAN_POINT('Ctrl Pts',(-1.89878988776966,60.6650339396205,13.8624714778077));
#63862=CARTESIAN_POINT('Ctrl Pts',(-1.92741307745339,60.6778437918713,13.7634626856993));
#63863=CARTESIAN_POINT('Ctrl Pts',(-1.9483285077907,60.6906513214101,13.6627802207895));
#63864=CARTESIAN_POINT('Ctrl Pts',(-1.95371074865907,60.6939471277977,13.6368712498228));
#63865=CARTESIAN_POINT('Ctrl Pts',(-1.95858278705612,60.6972427595641,13.6108516132584));
#63866=CARTESIAN_POINT('Ctrl Pts',(-1.96293944415645,60.7005382821062,13.5847440033346));
#63867=CARTESIAN_POINT('Ctrl Pts',(-1.97300581117807,60.7081528220328,13.5244205081643));
#63868=CARTESIAN_POINT('Ctrl Pts',(-1.98031066061398,60.7157785521554,13.463570155228));
#63869=CARTESIAN_POINT('Ctrl Pts',(-1.98479348719843,60.7234144908285,13.4024573530112));
#63870=CARTESIAN_POINT('Ctrl Pts',(-1.99657422568646,60.7434815166044,13.2418546779747));
#63871=CARTESIAN_POINT('Ctrl Pts',(-1.98886620028509,60.7636184653362,13.07944306302));
#63872=CARTESIAN_POINT('Ctrl Pts',(-1.96190927563821,60.7838131630534,12.9199097467551));
#63873=CARTESIAN_POINT('Ctrl Pts',(-1.94350514443476,60.7976005617004,12.8109925715832));
#63874=CARTESIAN_POINT('Ctrl Pts',(-1.91612902463564,60.8114150450154,12.7034157944574));
#63875=CARTESIAN_POINT('Ctrl Pts',(-1.87984993124581,60.8252549333523,12.5986590852905));
#63876=CARTESIAN_POINT('Ctrl Pts',(-1.87237181125249,60.8281077153821,12.5770658433416));
#63877=CARTESIAN_POINT('Ctrl Pts',(-1.86452114578359,60.8309602703639,12.5555931375228));
#63878=CARTESIAN_POINT('Ctrl Pts',(-1.85629745446083,60.8338128756041,12.5342537835132));
#63879=CARTESIAN_POINT('Ctrl Pts',(-1.81970534913029,60.8465058169271,12.4393022758562));
#63880=CARTESIAN_POINT('Ctrl Pts',(-1.77572703052217,60.8592002794464,12.3469869163756));
#63881=CARTESIAN_POINT('Ctrl Pts',(-1.72496264541799,60.8719164694528,12.2582888657482));
#63882=CARTESIAN_POINT('Ctrl Pts',(-1.6724160717148,60.8850790875761,12.166476886837));
#63883=CARTESIAN_POINT('Ctrl Pts',(-1.61259705340655,60.898265031652,12.0785409582365));
#63884=CARTESIAN_POINT('Ctrl Pts',(-1.54619418402695,60.9114891754909,11.9956227499056));
#63885=CARTESIAN_POINT('Ctrl Pts',(-1.47979131464733,60.9247133193299,11.9127045415747));
#63886=CARTESIAN_POINT('Ctrl Pts',(-1.40680339243252,60.9379756658135,11.8348051182777));
#63887=CARTESIAN_POINT('Ctrl Pts',(-1.32796230537848,60.9512833737372,11.7631079740704));
#63888=CARTESIAN_POINT('Ctrl Pts',(-1.26598629827422,60.961744398967,11.7067477324149));
#63889=CARTESIAN_POINT('Ctrl Pts',(-1.20049286612118,60.9722144435424,11.6540711597815));
#63890=CARTESIAN_POINT('Ctrl Pts',(-1.13182440260108,60.9826983981754,11.6056255448801));
#63891=CARTESIAN_POINT('Ctrl Pts',(-1.09084918772005,60.9889542872963,11.5767175224945));
#63892=CARTESIAN_POINT('Ctrl Pts',(-1.04874369202499,60.9952150927196,11.5493162091802));
#63893=CARTESIAN_POINT('Ctrl Pts',(-1.00566818612401,61.0014816988447,11.5234423362574));
#63894=CARTESIAN_POINT('Ctrl Pts',(-0.962594463826959,61.0077480454919,
11.49756953468));
#63895=CARTESIAN_POINT('Ctrl Pts',(-0.91855080808143,61.0140201924027,11.4732240671337));
#63896=CARTESIAN_POINT('Ctrl Pts',(-0.87361793905202,61.0202985106828,11.450524928987));
#63897=CARTESIAN_POINT('Ctrl Pts',(-0.773152929515877,61.0343361477069,
11.3997721241999));
#63898=CARTESIAN_POINT('Ctrl Pts',(-0.668239101491088,61.0484050465533,
11.3572500207284));
#63899=CARTESIAN_POINT('Ctrl Pts',(-0.560352649403341,61.0625060042088,
11.3235457214749));
#63900=CARTESIAN_POINT('Ctrl Pts',(-0.518148271713797,61.0680221939728,
11.3103608502707));
#63901=CARTESIAN_POINT('Ctrl Pts',(-0.475489546815452,61.0735432233592,
11.2985253351017));
#63902=CARTESIAN_POINT('Ctrl Pts',(-0.432466963195663,61.0790688840395,
11.2880738510178));
#63903=CARTESIAN_POINT('Ctrl Pts',(-0.320866162986129,61.0934024758821,
11.2609626482726));
#63904=CARTESIAN_POINT('Ctrl Pts',(-0.206749271624201,61.107768758523,11.2429306468698));
#63905=CARTESIAN_POINT('Ctrl Pts',(-0.091645956239233,61.1221689807695,
11.2345907989729));
#63906=CARTESIAN_POINT('Ctrl Pts',(-0.0601010265759873,61.126115470029,
11.2323052009046));
#63907=CARTESIAN_POINT('Ctrl Pts',(-0.028482293873111,61.1300644798337,
11.2307474565802));
#63908=CARTESIAN_POINT('Ctrl Pts',(0.00317813948409761,61.1340159710391,
11.2299298964506));
#63909=CARTESIAN_POINT('Ctrl Pts',(0.118796983769572,61.1484461855977,11.2269442974773));
#63910=CARTESIAN_POINT('Ctrl Pts',(0.23497465217744,61.1629098763671,11.2338327438001));
#63911=CARTESIAN_POINT('Ctrl Pts',(0.350030063026787,61.1774019927302,11.2503173834763));
#63912=CARTESIAN_POINT('Ctrl Pts',(0.432372184468717,61.1877736179908,11.2621150050928));
#63913=CARTESIAN_POINT('Ctrl Pts',(0.514138539597379,61.1981596985619,11.2788270263037));
#63914=CARTESIAN_POINT('Ctrl Pts',(0.594704550095013,61.2085568151962,11.3003375309651));
#63915=CARTESIAN_POINT('Ctrl Pts',(0.701692939563703,61.2223637637711,11.3289026074305));
#63916=CARTESIAN_POINT('Ctrl Pts',(0.806767964229992,61.2362149107861,11.3659430373292));
#63917=CARTESIAN_POINT('Ctrl Pts',(0.908473479897716,61.2501016666349,11.4111383449384));
#63918=CARTESIAN_POINT('Ctrl Pts',(1.00021889379422,61.2626284814755,11.451907640247));
#63919=CARTESIAN_POINT('Ctrl Pts',(1.08922237606095,61.2751843254157,11.4993116533713));
#63920=CARTESIAN_POINT('Ctrl Pts',(1.17444482557351,61.287765803511,11.5530942618712));
#63921=CARTESIAN_POINT('Ctrl Pts',(1.26814532044362,61.3015989041841,11.612227237521));
#63922=CARTESIAN_POINT('Ctrl Pts',(1.35727408503484,61.3154629378033,11.6790699682437));
#63923=CARTESIAN_POINT('Ctrl Pts',(1.44090431072691,61.3293571514557,11.7525023543434));
#63924=CARTESIAN_POINT('Ctrl Pts',(1.46205543896261,61.3328711715635,11.771074321622));
#63925=CARTESIAN_POINT('Ctrl Pts',(1.48285511373977,61.3363871419884,11.7900677939993));
#63926=CARTESIAN_POINT('Ctrl Pts',(1.50328887112793,61.339905090742,11.8094646946219));
#63927=CARTESIAN_POINT('Ctrl Pts',(1.5794445722949,61.3530163286269,11.8817560769321));
#63928=CARTESIAN_POINT('Ctrl Pts',(1.65032057243723,61.3661424004616,11.9599808167139));
#63929=CARTESIAN_POINT('Ctrl Pts',(1.71516743938303,61.3792867600178,12.0431980663506));
#63930=CARTESIAN_POINT('Ctrl Pts',(1.75938636176628,61.3882498671403,12.0999437084448));
#63931=CARTESIAN_POINT('Ctrl Pts',(1.80080259418761,61.3972216164688,12.159011698473));
#63932=CARTESIAN_POINT('Ctrl Pts',(1.83918332776035,61.406204877657,12.2201166228578));
#63933=CARTESIAN_POINT('Ctrl Pts',(1.88406660745716,61.4167101022051,12.2915740744675));
#63934=CARTESIAN_POINT('Ctrl Pts',(1.92481866657411,61.4272340928429,12.3658161772094));
#63935=CARTESIAN_POINT('Ctrl Pts',(1.96110251039936,61.4377829526498,12.4423180005748));
#63936=CARTESIAN_POINT('Ctrl Pts',(1.99085484123667,61.4464328952646,12.5050486078773));
#63937=CARTESIAN_POINT('Ctrl Pts',(2.01760384199706,61.4550996769869,12.5692989446145));
#63938=CARTESIAN_POINT('Ctrl Pts',(2.04118161774851,61.463789852119,12.6347984710244));
#63939=CARTESIAN_POINT('Ctrl Pts',(2.0494963355269,61.4668544479668,12.6578969211266));
#63940=CARTESIAN_POINT('Ctrl Pts',(2.05741679693751,61.4699219790975,12.6811508977909));
#63941=CARTESIAN_POINT('Ctrl Pts',(2.06494465670457,61.4729928172606,12.7045450077392));
#63942=CARTESIAN_POINT('Ctrl Pts',(2.09243054740177,61.4842051305491,12.7899621075384));
#63943=CARTESIAN_POINT('Ctrl Pts',(2.11458011981301,61.4954464062451,12.877260276532));
#63944=CARTESIAN_POINT('Ctrl Pts',(2.13125540857689,61.5067073051811,12.9657828175091));
#63945=CARTESIAN_POINT('Ctrl Pts',(2.14789143364656,61.5179416891645,13.0540969229964));
#63946=CARTESIAN_POINT('Ctrl Pts',(2.15907783747761,61.5291955981566,13.1436300129846));
#63947=CARTESIAN_POINT('Ctrl Pts',(2.16465876667325,61.5404530657803,13.2336822050908));
#63948=CARTESIAN_POINT('Ctrl Pts',(2.17398320685921,61.5592616870373,13.3841385627104));
#63949=CARTESIAN_POINT('Ctrl Pts',(2.16767126813817,61.5780856248973,13.5360794717045));
#63950=CARTESIAN_POINT('Ctrl Pts',(2.14549595895314,61.5969303796965,13.6861414620898));
#63951=CARTESIAN_POINT('Ctrl Pts',(2.14109490036659,61.6006704344226,13.7159237576056));
#63952=CARTESIAN_POINT('Ctrl Pts',(2.13606886954778,61.6044113291931,13.7456321435509));
#63953=CARTESIAN_POINT('Ctrl Pts',(2.13041587611228,61.6081531367628,13.7752404432675));
#63954=CARTESIAN_POINT('Ctrl Pts',(2.11280862816456,61.6198076582838,13.8674607298055));
#63955=CARTESIAN_POINT('Ctrl Pts',(2.08941019597058,61.6315190928153,13.9587167983496));
#63956=CARTESIAN_POINT('Ctrl Pts',(2.0600668219164,61.6432768391579,14.0482459937675));
#63957=CARTESIAN_POINT('Ctrl Pts',(2.02936375310375,61.6555794085343,14.1419237365717));
#63958=CARTESIAN_POINT('Ctrl Pts',(1.9921508370218,61.6679327262336,14.233710857238));
#63959=CARTESIAN_POINT('Ctrl Pts',(1.94883949167143,61.6803182038231,14.3228166045752));
#63960=CARTESIAN_POINT('Ctrl Pts',(1.90537869029098,61.6927464204292,14.4122298323462));
#63961=CARTESIAN_POINT('Ctrl Pts',(1.85577632749744,61.7052070191149,14.4989425067665));
#63962=CARTESIAN_POINT('Ctrl Pts',(1.8004760420889,61.7176746273994,14.5821118430939));
#63963=CARTESIAN_POINT('Ctrl Pts',(1.75932809814522,61.7269515496252,14.6439966446596));
#63964=CARTESIAN_POINT('Ctrl Pts',(1.71502599467862,61.7362322161595,14.703918634141));
#63965=CARTESIAN_POINT('Ctrl Pts',(1.66776687229128,61.7455038255094,14.7615187689036));
#63966=CARTESIAN_POINT('Ctrl Pts',(1.59763392570811,61.7592629740172,14.8469978673384));
#63967=CARTESIAN_POINT('Ctrl Pts',(1.52100707003437,61.7730735779605,14.9276302297976));
#63968=CARTESIAN_POINT('Ctrl Pts',(1.43862385219125,61.7869320574814,15.0022941683172));
#63969=CARTESIAN_POINT('Ctrl Pts',(1.36031021816126,61.8001059528671,15.0732698416344));
#63970=CARTESIAN_POINT('Ctrl Pts',(1.27679594274065,61.8133231251821,15.1388517715873));
#63971=CARTESIAN_POINT('Ctrl Pts',(1.18873969579851,61.8265819222932,15.1981121666516));
#63972=CARTESIAN_POINT('Ctrl Pts',(1.09666770856855,61.8404453770813,15.2600750883871));
#63973=CARTESIAN_POINT('Ctrl Pts',(0.99963118253683,61.8543543316727,15.3151261617681));
#63974=CARTESIAN_POINT('Ctrl Pts',(0.898912823232068,61.8683084208655,15.3628784602649));
#63975=CARTESIAN_POINT('Ctrl Pts',(0.858386533620023,61.873923161453,15.3820926680011));
#63976=CARTESIAN_POINT('Ctrl Pts',(0.817264179198787,61.8795452274309,15.4001257646514));
#63977=CARTESIAN_POINT('Ctrl Pts',(0.775629168390384,61.8851746664602,15.4169549299689));
#63978=CARTESIAN_POINT('Ctrl Pts',(0.685817155271583,61.897318082353,15.4532575797562));
#63979=CARTESIAN_POINT('Ctrl Pts',(0.593362597818468,61.9094279499761,15.4837639692001));
#63980=CARTESIAN_POINT('Ctrl Pts',(0.499132047757716,61.9215309125639,15.5082773603599));
#63981=CARTESIAN_POINT('Ctrl Pts',(0.404521099924699,61.933682733404,15.532889709229));
#63982=CARTESIAN_POINT('Ctrl Pts',(0.308120225844149,61.9458275940093,15.551461626621));
#63983=CARTESIAN_POINT('Ctrl Pts',(0.21075956535082,61.9579992118371,15.5638169852688));
#63984=CARTESIAN_POINT('Ctrl Pts',(0.113205540709764,61.9701950032326,15.5761968824044));
#63985=CARTESIAN_POINT('Ctrl Pts',(0.0146880365663079,61.9824176616428,
15.582336657944));
#63986=CARTESIAN_POINT('Ctrl Pts',(-0.0840090766511814,61.9947078352595,
15.5820655802065));
#63987=CARTESIAN_POINT('Ctrl Pts',(-0.13444640871128,62.0009885008998,15.5819270509485));
#63988=CARTESIAN_POINT('Ctrl Pts',(-0.184931484660247,62.0072869061431,
15.5801143038734));
#63989=CARTESIAN_POINT('Ctrl Pts',(-0.235364843567225,62.0136091475188,
15.5766036679292));
#63990=CARTESIAN_POINT('Ctrl Pts',(-0.26994468556806,62.0179440185763,15.5741965858132));
#63991=CARTESIAN_POINT('Ctrl Pts',(-0.304500286908054,62.0222901049293,
15.5709912696112));
#63992=CARTESIAN_POINT('Ctrl Pts',(-0.338999847063386,62.0266494928043,
15.5670034814));
#63993=CARTESIAN_POINT('Ctrl Pts',(-0.451703931082599,62.0408908574803,
15.5539760684249));
#63994=CARTESIAN_POINT('Ctrl Pts',(-0.563680880569419,62.0551893687934,
15.5324319507017));
#63995=CARTESIAN_POINT('Ctrl Pts',(-0.673761042537445,62.0695164405951,
15.5027165105806));
#63996=CARTESIAN_POINT('Ctrl Pts',(-0.784111718606247,62.0838787201479,
15.4729280468973));
#63997=CARTESIAN_POINT('Ctrl Pts',(-0.892556452373441,62.0982696942304,
15.4349266344889));
#63998=CARTESIAN_POINT('Ctrl Pts',(-0.997865993481773,62.1126540724659,
15.3890504899903));
#63999=CARTESIAN_POINT('Ctrl Pts',(-1.10268296977809,62.1269711705815,15.3433889221982));
#64000=CARTESIAN_POINT('Ctrl Pts',(-1.2043937851748,62.1412817210782,15.2899248919537));
#64001=CARTESIAN_POINT('Ctrl Pts',(-1.30173641567575,62.1555446619255,15.2290020161442));
#64002=CARTESIAN_POINT('Ctrl Pts',(-1.33746396564815,62.1607795721519,15.2066415654481));
#64003=CARTESIAN_POINT('Ctrl Pts',(-1.37260261002422,62.1660080087906,15.1832765211277));
#64004=CARTESIAN_POINT('Ctrl Pts',(-1.40708839617374,62.171227733778,15.1589246924533));
#64005=CARTESIAN_POINT('Ctrl Pts',(-1.4815991685812,62.1825055900773,15.1063095786149));
#64006=CARTESIAN_POINT('Ctrl Pts',(-1.55318222100573,62.1938572267572,15.0493158946748));
#64007=CARTESIAN_POINT('Ctrl Pts',(-1.62123624053169,62.2052677199323,14.9881020864936));
#64008=CARTESIAN_POINT('Ctrl Pts',(-1.70919033190374,62.2200148218128,14.9089883924679));
#64009=CARTESIAN_POINT('Ctrl Pts',(-1.79125060481977,62.2348604481774,14.8228239298759));
#64010=CARTESIAN_POINT('Ctrl Pts',(-1.86660942439318,62.2497664850856,14.730702390601));
#64011=CARTESIAN_POINT('Ctrl Pts',(-1.94228821598917,62.2647358127247,14.638189705135));
#64012=CARTESIAN_POINT('Ctrl Pts',(-2.01120743413818,62.2797660598917,14.5396685205953));
#64013=CARTESIAN_POINT('Ctrl Pts',(-2.07251726871229,62.2948120763592,14.4362881380417));
#64014=CARTESIAN_POINT('Ctrl Pts',(-2.13388727297309,62.30987285904,14.332806297618));
#64015=CARTESIAN_POINT('Ctrl Pts',(-2.18763165103999,62.3249494318462,14.2244553837266));
#64016=CARTESIAN_POINT('Ctrl Pts',(-2.23288424985752,62.3399900837948,14.1124376546826));
#64017=CARTESIAN_POINT('Ctrl Pts',(-2.26016929432925,62.3490588415684,14.044896589673));
#64018=CARTESIAN_POINT('Ctrl Pts',(-2.28436697702911,62.3581144170538,13.9760234597122));
#64019=CARTESIAN_POINT('Ctrl Pts',(-2.30528819609144,62.3671443726308,13.906090902458));
#64020=CARTESIAN_POINT('Ctrl Pts',(-2.33117525897419,62.3783176712398,13.8195592093574));
#64021=CARTESIAN_POINT('Ctrl Pts',(-2.3522325795562,62.389560868264,13.7314261277675));
#64022=CARTESIAN_POINT('Ctrl Pts',(-2.36810889832169,62.4008599357382,13.6421621895604));
#64023=CARTESIAN_POINT('Ctrl Pts',(-2.39025521020944,62.4166213144319,13.5176454772758));
#64024=CARTESIAN_POINT('Ctrl Pts',(-2.40231955223421,62.4324916509277,13.3909260949408));
#64025=CARTESIAN_POINT('Ctrl Pts',(-2.40436278109046,62.4484275093813,13.2636193065498));
#64026=CARTESIAN_POINT('Ctrl Pts',(-2.40641819902219,62.4644584347096,13.1355530574407));
#64027=CARTESIAN_POINT('Ctrl Pts',(-2.39833131619744,62.4805556608201,13.0068926973835));
#64028=CARTESIAN_POINT('Ctrl Pts',(-2.38017332370241,62.4966688169118,12.879334371197));
#64029=CARTESIAN_POINT('Ctrl Pts',(-2.36199507708613,62.5127999462358,12.7516337615612));
#64030=CARTESIAN_POINT('Ctrl Pts',(-2.33372206985597,62.5289470290862,12.6250384379951));
#64031=CARTESIAN_POINT('Ctrl Pts',(-2.29545331523554,62.5450535149947,12.5012935366798));
#64032=CARTESIAN_POINT('Ctrl Pts',(-2.2777550052266,62.5525023484776,12.4440647178372));
#64033=CARTESIAN_POINT('Ctrl Pts',(-2.25791927630086,62.5599424159396,12.3874460872777));
#64034=CARTESIAN_POINT('Ctrl Pts',(-2.23595894097234,62.5673677011894,12.3316125240405));
#64035=CARTESIAN_POINT('Ctrl Pts',(-2.20325929085431,62.5784241912685,12.248474541155));
#64036=CARTESIAN_POINT('Ctrl Pts',(-2.16597892862786,62.5895536077964,12.1669980756594));
#64037=CARTESIAN_POINT('Ctrl Pts',(-2.12413456271561,62.6007408015926,12.0877263643258));
#64038=CARTESIAN_POINT('Ctrl Pts',(-2.06280503129239,62.6171374021505,11.9715411430849));
#64039=CARTESIAN_POINT('Ctrl Pts',(-1.99166944133828,62.6336583962586,11.8600904636704));
#64040=CARTESIAN_POINT('Ctrl Pts',(-1.91183578353717,62.6502506069489,11.7546857033027));
#64041=CARTESIAN_POINT('Ctrl Pts',(-1.83147654432938,62.6669520517351,11.6485870152891));
#64042=CARTESIAN_POINT('Ctrl Pts',(-1.74230347665068,62.6837256461713,11.5486152012365));
#64043=CARTESIAN_POINT('Ctrl Pts',(-1.64548519487996,62.7005107585213,11.4561434919834));
#64044=CARTESIAN_POINT('Ctrl Pts',(-1.54866258252202,62.7172966216531,11.363667646561));
#64045=CARTESIAN_POINT('Ctrl Pts',(-1.44419361983878,62.7340939872039,11.2786939854489));
#64046=CARTESIAN_POINT('Ctrl Pts',(-1.33329535227736,62.7508360309726,11.2026127655733));
#64047=CARTESIAN_POINT('Ctrl Pts',(-1.28567692813959,62.7580248695238,11.1699443760969));
#64048=CARTESIAN_POINT('Ctrl Pts',(-1.23687374844507,62.7652034321293,11.1389156099597));
#64049=CARTESIAN_POINT('Ctrl Pts',(-1.18698511474629,62.7723660906114,11.1096364226772));
#64050=CARTESIAN_POINT('Ctrl Pts',(-1.1169662830485,62.7824189010732,11.0685430045058));
#64051=CARTESIAN_POINT('Ctrl Pts',(-1.04473989886747,62.7924325160741,11.0308791404912));
#64052=CARTESIAN_POINT('Ctrl Pts',(-0.970669154241979,62.802513573085,10.9968390349676));
#64053=CARTESIAN_POINT('Ctrl Pts',(-0.96417153747111,62.8033979012422,10.9938529766844));
#64054=CARTESIAN_POINT('Ctrl Pts',(-0.957659702528321,62.8042827525257,
10.9908947829975));
#64055=CARTESIAN_POINT('Ctrl Pts',(-0.95113387948199,62.8051682013071,10.9879645736141));
#64056=CARTESIAN_POINT('Ctrl Pts',(2.62606127725066,71.5535446069272,11.6247283617098));
#64057=CARTESIAN_POINT('Ctrl Pts',(3.07369675274833,71.6548048472623,12.3017885911471));
#64058=CARTESIAN_POINT('Ctrl Pts',(3.39947547686869,71.8540694654572,13.9926794859483));
#64059=CARTESIAN_POINT('Ctrl Pts',(2.00035370322902,72.1534741441049,16.1563562104496));
#64060=CARTESIAN_POINT('Ctrl Pts',(-0.479193598718106,72.4505896841945,
16.7743438931863));
#64061=CARTESIAN_POINT('Ctrl Pts',(-2.72820677080343,72.749329075019,15.5345476487549));
#64062=CARTESIAN_POINT('Ctrl Pts',(-3.53053655760175,73.0491815267796,13.0830348300015));
#64063=CARTESIAN_POINT('Ctrl Pts',(-2.44583127626423,73.3496165328875,10.73926097503));
#64064=CARTESIAN_POINT('Ctrl Pts',(-0.0515057170124552,73.6501034404386,
9.76262003450415));
#64065=CARTESIAN_POINT('Ctrl Pts',(2.08813716621235,73.9167737645113,10.5786304219304));
#64066=CARTESIAN_POINT('Ctrl Pts',(3.14505930727665,74.1494556326765,12.1881664149021));
#64067=CARTESIAN_POINT('Ctrl Pts',(3.28302856381622,74.3482934483014,13.8249014301578));
#64068=CARTESIAN_POINT('Ctrl Pts',(2.62022018676624,74.5463751228733,15.3232742760889));
#64069=CARTESIAN_POINT('Ctrl Pts',(1.32704205219576,74.7435517804002,16.3159859655964));
#64070=CARTESIAN_POINT('Ctrl Pts',(-0.00839796692879819,74.9069885873292,
16.5242436918362));
#64071=CARTESIAN_POINT('Ctrl Pts',(-1.03406743711528,75.0371432170061,16.2943148716111));
#64072=CARTESIAN_POINT('Ctrl Pts',(-1.96986838717684,75.1668758709914,15.8219854723893));
#64073=CARTESIAN_POINT('Ctrl Pts',(-2.67823089801238,75.2959450476796,15.024243908725));
#64074=CARTESIAN_POINT('Ctrl Pts',(-2.99017889307188,75.4082368997061,14.1724204800879));
#64075=CARTESIAN_POINT('Ctrl Pts',(-3.06457943071697,75.4642187845407,13.7291125469622));
#64076=CARTESIAN_POINT('Ctrl Pts',(-3.08233538140113,75.4961587160299,13.4737488921684));
#64077=CARTESIAN_POINT('Ctrl Pts',(-3.0984392379095,75.6397395192991,12.3218754758916));
#64078=CARTESIAN_POINT('Ctrl Pts',(-1.89880363741605,75.9006508147323,10.2819015113804));
#64079=CARTESIAN_POINT('Ctrl Pts',(0.905612844857268,76.2108186357633,10.1560618488092));
#64080=CARTESIAN_POINT('Ctrl Pts',(2.4356553389957,76.4548900770423,11.4712451450617));
#64081=CARTESIAN_POINT('Ctrl Pts',(3.17219985054598,76.6961315682435,13.3281170575199));
#64082=CARTESIAN_POINT('Ctrl Pts',(2.56238501016055,76.8811530474602,14.8814311629097));
#64083=CARTESIAN_POINT('Ctrl Pts',(1.72783980301917,77.0124960583169,15.5266153278474));
#64084=CARTESIAN_POINT('Ctrl Pts',(1.53551862751901,77.0416343818686,15.6589169268593));
#64085=CARTESIAN_POINT('Ctrl Pts',(1.17818387297515,77.0924962062513,15.8569804874213));
#64086=CARTESIAN_POINT('Ctrl Pts',(0.623815753643446,77.1647861338154,16.0404402005033));
#64087=CARTESIAN_POINT('Ctrl Pts',(-0.0702939325535233,77.250932262354,
16.0883675706203));
#64088=CARTESIAN_POINT('Ctrl Pts',(-0.97706182894233,77.3649831053848,15.9240026281399));
#64089=CARTESIAN_POINT('Ctrl Pts',(-1.96791083657319,77.5060145445082,15.3088785584671));
#64090=CARTESIAN_POINT('Ctrl Pts',(-2.64752139679713,77.672758908484,14.1087106115944));
#64091=CARTESIAN_POINT('Ctrl Pts',(-2.66935132912839,77.8369818342363,12.7510168963697));
#64092=CARTESIAN_POINT('Ctrl Pts',(-2.04802128466415,77.9986630811314,11.5672470590297));
#64093=CARTESIAN_POINT('Ctrl Pts',(-0.953406375685504,78.1577929882928,
10.8374874366033));
#64094=CARTESIAN_POINT('Ctrl Pts',(0.336148931890551,78.3143710867681,10.7228295007321));
#64095=CARTESIAN_POINT('Ctrl Pts',(1.50307999575334,78.4684077961839,11.2321414818918));
#64096=CARTESIAN_POINT('Ctrl Pts',(2.27244152083141,78.6199207500098,12.2206815704071));
#64097=CARTESIAN_POINT('Ctrl Pts',(2.47025450075222,78.7689406968174,13.4369060696769));
#64098=CARTESIAN_POINT('Ctrl Pts',(2.06838453699815,78.9155054863287,14.580422079702));
#64099=CARTESIAN_POINT('Ctrl Pts',(1.18267230002556,79.0596632019735,15.3776880766993));
#64100=CARTESIAN_POINT('Ctrl Pts',(0.0417367172907162,79.2014711616318,
15.651091689114));
#64101=CARTESIAN_POINT('Ctrl Pts',(-1.07091431074263,79.3409947472366,15.348470280034));
#64102=CARTESIAN_POINT('Ctrl Pts',(-1.98410802505723,79.4935674136222,14.4759887843483));
#64103=CARTESIAN_POINT('Ctrl Pts',(-2.29250453277775,79.6583660808514,13.1152303337474));
#64104=CARTESIAN_POINT('Ctrl Pts',(-1.65329344570907,79.8345871894848,11.7642469664184));
#64105=CARTESIAN_POINT('Ctrl Pts',(-0.561194871313656,79.9786744458678,
11.2211155923112));
#64106=CARTESIAN_POINT('Ctrl Pts',(0.248468418157764,80.078205765166,11.2502761671321));
#64107=CARTESIAN_POINT('Ctrl Pts',(0.683379628434247,80.134714093272,11.3779527164502));
#64108=CARTESIAN_POINT('Ctrl Pts',(1.50537944865847,80.247265487895,11.7682049163228));
#64109=CARTESIAN_POINT('Ctrl Pts',(2.06939217422075,80.3720681591741,12.736646766933));
#64110=CARTESIAN_POINT('Ctrl Pts',(1.90567271165315,80.5225053556114,13.9535241790153));
#64111=CARTESIAN_POINT('Ctrl Pts',(1.44391453743883,80.6310252212425,14.7196833195633));
#64112=CARTESIAN_POINT('Ctrl Pts',(0.57711443901227,80.7520545863008,15.2239016882313));
#64113=CARTESIAN_POINT('Ctrl Pts',(-0.415289947510754,80.8721738215391,
15.2506488494656));
#64114=CARTESIAN_POINT('Ctrl Pts',(-1.29478405254176,80.9915321525424,14.801994928262));
#64115=CARTESIAN_POINT('Ctrl Pts',(-1.84882892486789,81.1102808484601,13.9907678349858));
#64116=CARTESIAN_POINT('Ctrl Pts',(-1.92183367763277,81.1990029414579,13.2607435842994));
#64117=CARTESIAN_POINT('Ctrl Pts',(-1.8217052798405,81.2580564159435,12.7970006616204));
#64118=CARTESIAN_POINT('Ctrl Pts',(-1.71726172276848,81.2974025519046,12.4987499564163));
#64119=CARTESIAN_POINT('Ctrl Pts',(-1.43925958278793,81.366216398273,12.0170756654402));
#64120=CARTESIAN_POINT('Ctrl Pts',(-0.803691837170658,81.4644268389926,
11.5113131401901));
#64121=CARTESIAN_POINT('Ctrl Pts',(0.157310001461349,81.5823031737216,11.3451440479436));
#64122=CARTESIAN_POINT('Ctrl Pts',(1.08175881202912,81.7003494145943,11.6587285348207));
#64123=CARTESIAN_POINT('Ctrl Pts',(1.74459855235824,81.8187309164738,12.3798675479581));
#64124=CARTESIAN_POINT('Ctrl Pts',(1.98175103862329,81.9375991758226,13.3341054677106));
#64125=CARTESIAN_POINT('Ctrl Pts',(1.73131320698376,82.0571102816978,14.2902754504896));
#64126=CARTESIAN_POINT('Ctrl Pts',(1.04838542790616,82.1774164300365,15.0148406760434));
#64127=CARTESIAN_POINT('Ctrl Pts',(0.0950356967664279,82.2986627179121,
15.3241799164539));
#64128=CARTESIAN_POINT('Ctrl Pts',(-1.01123848225145,82.4345915545847,15.1190339956634));
#64129=CARTESIAN_POINT('Ctrl Pts',(-1.93343043195045,82.5858630943909,14.2288726578984));
#64130=CARTESIAN_POINT('Ctrl Pts',(-2.1256356945421,82.7533957188934,12.8212136757709));
#64131=CARTESIAN_POINT('Ctrl Pts',(-1.50138332796606,82.8988937003856,11.7583081310997));
#64132=CARTESIAN_POINT('Ctrl Pts',(-0.632429912249052,83.0212610196965,
11.2664585694225));
#64133=CARTESIAN_POINT('Ctrl Pts',(0.424674872888512,83.1521963337219,11.1113494661316));
#64134=CARTESIAN_POINT('Ctrl Pts',(1.73233529621671,83.3185416832946,11.6891669232624));
#64135=CARTESIAN_POINT('Ctrl Pts',(2.42258940526503,83.5227848964116,13.3064020986805));
#64136=CARTESIAN_POINT('Ctrl Pts',(1.81060149541817,83.7319444375417,14.9983668615199));
#64137=CARTESIAN_POINT('Ctrl Pts',(0.169716220670518,83.9462835131092,15.8393531505486));
#64138=CARTESIAN_POINT('Ctrl Pts',(-1.64864304635011,84.1660018217439,15.3229733594306));
#64139=CARTESIAN_POINT('Ctrl Pts',(-2.69270309708095,84.4008278320615,13.5930908615205));
#64140=CARTESIAN_POINT('Ctrl Pts',(-2.34009646860672,84.5648308878988,12.2032471101965));
#64141=CARTESIAN_POINT('Ctrl Pts',(-1.89038667730081,84.6529546621916,11.6566997621504));
#64142=CARTESIAN_POINT('Ctrl Pts',(2.45537460810738,71.8997412275771,11.7369673410428));
#64143=CARTESIAN_POINT('Ctrl Pts',(2.86465514317376,71.9944459875631,12.3761438649969));
#64144=CARTESIAN_POINT('Ctrl Pts',(3.14183581063553,72.1798336583578,13.9534707954349));
#64145=CARTESIAN_POINT('Ctrl Pts',(1.82121553961701,72.4557236515511,15.9258509314207));
#64146=CARTESIAN_POINT('Ctrl Pts',(-0.451459878047153,72.7271148628889,
16.454626209561));
#64147=CARTESIAN_POINT('Ctrl Pts',(-2.47125649787517,72.9978001233845,15.3003831479765));
#64148=CARTESIAN_POINT('Ctrl Pts',(-3.15929694060047,73.267507381235,13.0852384125598));
#64149=CARTESIAN_POINT('Ctrl Pts',(-2.15920493547541,73.535967111269,11.0060938504777));
#64150=CARTESIAN_POINT('Ctrl Pts',(-0.0200714085127461,73.8029233628205,
10.1699982444172));
#64151=CARTESIAN_POINT('Ctrl Pts',(1.86030659853292,74.0386635562282,10.9184680604956));
#64152=CARTESIAN_POINT('Ctrl Pts',(2.77130128735905,74.2436551756362,12.3489582116326));
#64153=CARTESIAN_POINT('Ctrl Pts',(2.87251295759163,74.4184202620592,13.7887881944876));
#64154=CARTESIAN_POINT('Ctrl Pts',(2.27296651564915,74.5921831870885,15.0946922490105));
#64155=CARTESIAN_POINT('Ctrl Pts',(1.12856013061699,74.7648878883527,15.9481703025818));
#64156=CARTESIAN_POINT('Ctrl Pts',(-0.0420118937118654,74.9078827780563,
16.1140624242939));
#64157=CARTESIAN_POINT('Ctrl Pts',(-0.935852251025538,75.0216999964023,
15.9006181548314));
#64158=CARTESIAN_POINT('Ctrl Pts',(-1.74799302734623,75.1351234789987,15.4764072161691));
#64159=CARTESIAN_POINT('Ctrl Pts',(-2.35725039846603,75.247946473202,14.7706510349632));
#64160=CARTESIAN_POINT('Ctrl Pts',(-2.61943865821339,75.3461227134966,14.0223232072198));
#64161=CARTESIAN_POINT('Ctrl Pts',(-2.67900504266786,75.3950740424631,13.6339039044037));
#64162=CARTESIAN_POINT('Ctrl Pts',(-2.69137681403548,75.4230063808888,13.4104334520196));
#64163=CARTESIAN_POINT('Ctrl Pts',(-2.69118459524818,75.5485825065238,12.4031854715294));
#64164=CARTESIAN_POINT('Ctrl Pts',(-1.61715338616522,75.7769418229487,10.6324544464939));
#64165=CARTESIAN_POINT('Ctrl Pts',(0.846315643470564,76.0493083690221,10.5555177734551));
#64166=CARTESIAN_POINT('Ctrl Pts',(2.17807352495375,76.2644764381485,11.7341625679922));
#64167=CARTESIAN_POINT('Ctrl Pts',(2.8051524329496,76.4778185988283,13.3850640198186));
#64168=CARTESIAN_POINT('Ctrl Pts',(2.24430249048783,76.642344041271,14.7582423366972));
#64169=CARTESIAN_POINT('Ctrl Pts',(1.48979469934905,76.7597131591705,15.3229864188903));
#64170=CARTESIAN_POINT('Ctrl Pts',(1.31604755489563,76.7857668522089,15.4385204013053));
#64171=CARTESIAN_POINT('Ctrl Pts',(0.9935887065671,76.8312864599085,15.610685427541));
#64172=CARTESIAN_POINT('Ctrl Pts',(0.494170705343874,76.8961015211196,15.7672982479309));
#64173=CARTESIAN_POINT('Ctrl Pts',(-0.130228120937696,76.9735420130962,
15.8004817055351));
#64174=CARTESIAN_POINT('Ctrl Pts',(-0.944846658431455,77.0763476093393,
15.6393426684008));
#64175=CARTESIAN_POINT('Ctrl Pts',(-1.83275135211394,77.2040199705238,15.0686965094999));
#64176=CARTESIAN_POINT('Ctrl Pts',(-2.43422897081155,77.3559138629566,13.9660529667295));
#64177=CARTESIAN_POINT('Ctrl Pts',(-2.43412964201641,77.5065223841571,12.7211217363066));
#64178=CARTESIAN_POINT('Ctrl Pts',(-1.84244736467127,77.6558779466535,11.6375025646228));
#64179=CARTESIAN_POINT('Ctrl Pts',(-0.812508634489196,77.8040179721768,
10.9754960366569));
#64180=CARTESIAN_POINT('Ctrl Pts',(0.399169147060676,77.9509840951834,10.888554482799));
#64181=CARTESIAN_POINT('Ctrl Pts',(1.49515333246982,78.0968241859332,11.3897674493044));
#64182=CARTESIAN_POINT('Ctrl Pts',(2.21309666412229,78.2415857024887,12.346800944208));
#64183=CARTESIAN_POINT('Ctrl Pts',(2.38257715684069,78.3853267723206,13.5227887118762));
#64184=CARTESIAN_POINT('Ctrl Pts',(1.97070979036788,78.5281048583051,14.6289215533792));
#64185=CARTESIAN_POINT('Ctrl Pts',(1.0846356356463,78.6699825164188,15.3966558175012));
#64186=CARTESIAN_POINT('Ctrl Pts',(-0.0546578360320794,78.8110261821086,
15.6465003144658));
#64187=CARTESIAN_POINT('Ctrl Pts',(-1.16663794159566,78.9513037625806,15.320240485781));
#64188=CARTESIAN_POINT('Ctrl Pts',(-2.07635850104646,79.106398067496,14.4152732562341));
#64189=CARTESIAN_POINT('Ctrl Pts',(-2.36611662039193,79.2761195563421,13.0084404449859));
#64190=CARTESIAN_POINT('Ctrl Pts',(-1.66972195348897,79.4603539256571,11.6104800674147));
#64191=CARTESIAN_POINT('Ctrl Pts',(-0.499241727900942,79.6132764154737,
11.0587123014677));
#64192=CARTESIAN_POINT('Ctrl Pts',(0.368381431253317,79.7200919455142,11.1100688932815));
#64193=CARTESIAN_POINT('Ctrl Pts',(0.834024390540476,79.7810729395003,11.2590830141615));
#64194=CARTESIAN_POINT('Ctrl Pts',(1.71327073675581,79.9029752811733,11.7022803019732));
#64195=CARTESIAN_POINT('Ctrl Pts',(2.31023027030925,80.039893650478,12.7769722273746));
#64196=CARTESIAN_POINT('Ctrl Pts',(2.0952937696238,80.2072118206172,14.1251984017593));
#64197=CARTESIAN_POINT('Ctrl Pts',(1.55681308005668,80.3289253095954,14.9709562403181));
#64198=CARTESIAN_POINT('Ctrl Pts',(0.562156846133121,80.4659772183401,15.5172494438125));
#64199=CARTESIAN_POINT('Ctrl Pts',(-0.571635535172935,80.6032374513939,
15.5193058729101));
#64200=CARTESIAN_POINT('Ctrl Pts',(-1.57105590216914,80.7407895484418,14.9769995665407));
#64201=CARTESIAN_POINT('Ctrl Pts',(-2.18972564985028,80.8787156023155,14.0191108554115));
#64202=CARTESIAN_POINT('Ctrl Pts',(-2.25281448620538,80.9825022603659,13.1637487406573));
#64203=CARTESIAN_POINT('Ctrl Pts',(-2.12068431526726,81.0518598050773,12.6228061624787));
#64204=CARTESIAN_POINT('Ctrl Pts',(-1.98850067502905,81.0981436402853,12.2756453504514));
#64205=CARTESIAN_POINT('Ctrl Pts',(-1.64588283908225,81.1792688423294,11.7171923425473));
#64206=CARTESIAN_POINT('Ctrl Pts',(-0.878376654572089,81.2955409216237,
11.1389422271489));
#64207=CARTESIAN_POINT('Ctrl Pts',(0.268860592398065,81.4357574199077,10.9718961823663));
#64208=CARTESIAN_POINT('Ctrl Pts',(1.36168464727168,81.5767306353953,11.3754866253281));
#64209=CARTESIAN_POINT('Ctrl Pts',(2.13170024959015,81.7185337285348,12.2596742591993));
#64210=CARTESIAN_POINT('Ctrl Pts',(2.38537574225421,81.861230869759,13.411638936312));
#64211=CARTESIAN_POINT('Ctrl Pts',(2.0538618627471,82.0048858136013,14.5517127600868));
#64212=CARTESIAN_POINT('Ctrl Pts',(1.21016878839885,82.1495577534274,15.4001780362731));
#64213=CARTESIAN_POINT('Ctrl Pts',(0.0554960675800941,82.2953007614427,
15.7411221116997));
#64214=CARTESIAN_POINT('Ctrl Pts',(-1.26478769570871,82.4584859871312,15.4599241062122));
#64215=CARTESIAN_POINT('Ctrl Pts',(-2.33986872524533,82.6396574319745,14.3656368632881));
#64216=CARTESIAN_POINT('Ctrl Pts',(-2.52469843952306,82.8394791673108,12.6823557101889));
#64217=CARTESIAN_POINT('Ctrl Pts',(-1.75208427106857,83.0120920363884,11.441919509068));
#64218=CARTESIAN_POINT('Ctrl Pts',(-0.712950690786717,83.1565241170819,
10.8875878228662));
#64219=CARTESIAN_POINT('Ctrl Pts',(0.533306351324057,83.3104483484253,10.7361019540252));
#64220=CARTESIAN_POINT('Ctrl Pts',(2.04196476140802,83.5047430421028,11.4494235183952));
#64221=CARTESIAN_POINT('Ctrl Pts',(2.79244898421244,83.7409671959345,13.3383065741216));
#64222=CARTESIAN_POINT('Ctrl Pts',(2.0450220032682,83.9802835859361,15.2551413117453));
#64223=CARTESIAN_POINT('Ctrl Pts',(0.167912320780133,84.2226842947316,16.1606000614443));
#64224=CARTESIAN_POINT('Ctrl Pts',(-1.84816591142016,84.4681399480701,15.5361778286278));
#64225=CARTESIAN_POINT('Ctrl Pts',(-2.95469492563506,84.7271265431151,13.6033326154612));
#64226=CARTESIAN_POINT('Ctrl Pts',(-2.53671169284916,84.9054952968908,12.1013400726277));
#64227=CARTESIAN_POINT('Ctrl Pts',(-2.04018169331035,85.000602884221,11.5215710376628));
#64228=CARTESIAN_POINT('Ctrl Pts',(2.28468793896408,72.245937848227,11.8492063203758));
#64229=CARTESIAN_POINT('Ctrl Pts',(2.65561353359917,72.334087127864,12.4504991388465));
#64230=CARTESIAN_POINT('Ctrl Pts',(2.88419614440235,72.5055978512584,13.9142621049215));
#64231=CARTESIAN_POINT('Ctrl Pts',(1.64207737600503,72.7579731589971,15.695345652392));
#64232=CARTESIAN_POINT('Ctrl Pts',(-0.423726157376209,73.0036400415831,
16.1349085259356));
#64233=CARTESIAN_POINT('Ctrl Pts',(-2.21430622494689,73.24627117175,15.0662186471979));
#64234=CARTESIAN_POINT('Ctrl Pts',(-2.78805732359919,73.4858332356904,13.0874419951179));
#64235=CARTESIAN_POINT('Ctrl Pts',(-1.87257859468661,73.7223176896503,11.2729267259256));
#64236=CARTESIAN_POINT('Ctrl Pts',(0.0113628999869613,73.9557432852023,
10.5773764543301));
#64237=CARTESIAN_POINT('Ctrl Pts',(1.63247603085348,74.1605533479452,11.2583056990608));
#64238=CARTESIAN_POINT('Ctrl Pts',(2.39754326744144,74.3378547185957,12.5097500083632));
#64239=CARTESIAN_POINT('Ctrl Pts',(2.46199735136702,74.488547075817,13.7526749588175));
#64240=CARTESIAN_POINT('Ctrl Pts',(1.92571284453205,74.6379912513037,14.8661102219322));
#64241=CARTESIAN_POINT('Ctrl Pts',(0.930078209038217,74.7862239963053,15.5803546395671));
#64242=CARTESIAN_POINT('Ctrl Pts',(-0.0756258204949394,74.9087769687833,
15.7038811567516));
#64243=CARTESIAN_POINT('Ctrl Pts',(-0.837637064935803,75.0062567757983,
15.5069214380518));
#64244=CARTESIAN_POINT('Ctrl Pts',(-1.52611766751561,75.1033710870057,15.1308289599487));
#64245=CARTESIAN_POINT('Ctrl Pts',(-2.03626989891968,75.1999478987245,14.5170581612014));
#64246=CARTESIAN_POINT('Ctrl Pts',(-2.2486984233549,75.2840085272871,13.8722259343517));
#64247=CARTESIAN_POINT('Ctrl Pts',(-2.29343065461876,75.3259293003855,13.5386952618452));
#64248=CARTESIAN_POINT('Ctrl Pts',(-2.30041824666983,75.3498540457475,13.3471180118707));
#64249=CARTESIAN_POINT('Ctrl Pts',(-2.28392995258685,75.4574254937484,12.4844954671671));
#64250=CARTESIAN_POINT('Ctrl Pts',(-1.33550313491438,75.6532328311649,10.9830073816075));
#64251=CARTESIAN_POINT('Ctrl Pts',(0.787018442083865,75.8877981022809,10.9549736981013));
#64252=CARTESIAN_POINT('Ctrl Pts',(1.92049171091181,76.0740627992544,11.9970799909228));
#64253=CARTESIAN_POINT('Ctrl Pts',(2.43810501535319,76.2595056294131,13.4420109821172));
#64254=CARTESIAN_POINT('Ctrl Pts',(1.92621997081512,76.4035350350817,14.6350535104845));
#64255=CARTESIAN_POINT('Ctrl Pts',(1.25174959567892,76.5069302600241,15.1193575099331));
#64256=CARTESIAN_POINT('Ctrl Pts',(1.09657648227224,76.5298993225489,15.2181238757514));
#64257=CARTESIAN_POINT('Ctrl Pts',(0.808993540159056,76.5700767135657,15.3643903676609));
#64258=CARTESIAN_POINT('Ctrl Pts',(0.364525657044304,76.6274169084238,15.4941562953586));
#64259=CARTESIAN_POINT('Ctrl Pts',(-0.190162309321864,76.6961517638386,
15.5125958404498));
#64260=CARTESIAN_POINT('Ctrl Pts',(-0.912631487920573,76.7877121132939,
15.3546827086616));
#64261=CARTESIAN_POINT('Ctrl Pts',(-1.69759186765469,76.9020253965394,14.8285144605326));
#64262=CARTESIAN_POINT('Ctrl Pts',(-2.22093654482596,77.039068817429,13.8233953218645));
#64263=CARTESIAN_POINT('Ctrl Pts',(-2.19890795490443,77.1760629340776,12.6912265762433));
#64264=CARTESIAN_POINT('Ctrl Pts',(-1.63687344467838,77.3130928121755,11.7077580702161));
#64265=CARTESIAN_POINT('Ctrl Pts',(-0.671610893292886,77.4502429560611,
11.1135046367102));
#64266=CARTESIAN_POINT('Ctrl Pts',(0.462189362230805,77.5875971035986,11.0542794648659));
#64267=CARTESIAN_POINT('Ctrl Pts',(1.4872266691863,77.7252405756827,11.5473934167169));
#64268=CARTESIAN_POINT('Ctrl Pts',(2.15375180741318,77.8632506549678,12.4729203180088));
#64269=CARTESIAN_POINT('Ctrl Pts',(2.29489981292916,78.0017128478238,13.6086713540756));
#64270=CARTESIAN_POINT('Ctrl Pts',(1.87303504373762,78.1407042302814,14.6774210270564));
#64271=CARTESIAN_POINT('Ctrl Pts',(0.986598971267029,78.2803018308642,15.4156235583032));
#64272=CARTESIAN_POINT('Ctrl Pts',(-0.151052389354876,78.4205812025852,
15.6419089398177));
#64273=CARTESIAN_POINT('Ctrl Pts',(-1.2623615724487,78.5616127779246,15.2920106915281));
#64274=CARTESIAN_POINT('Ctrl Pts',(-2.1686089770357,78.7192287213697,14.3545577281199));
#64275=CARTESIAN_POINT('Ctrl Pts',(-2.43972870800612,78.8938730318327,12.9016505562244));
#64276=CARTESIAN_POINT('Ctrl Pts',(-1.68615046126887,79.0861206618293,11.4567131684111));
#64277=CARTESIAN_POINT('Ctrl Pts',(-0.43728858448823,79.2478783850796,10.8963090106243));
#64278=CARTESIAN_POINT('Ctrl Pts',(0.488294444348867,79.3619781258626,10.9698616194307));
#64279=CARTESIAN_POINT('Ctrl Pts',(0.984669152646702,79.4274317857285,11.140213311873));
#64280=CARTESIAN_POINT('Ctrl Pts',(1.92116202485315,79.5586850744516,11.6363556876237));
#64281=CARTESIAN_POINT('Ctrl Pts',(2.55106836639776,79.7077191417819,12.8172976878161));
#64282=CARTESIAN_POINT('Ctrl Pts',(2.28491482759442,79.8919182856231,14.2968726245033));
#64283=CARTESIAN_POINT('Ctrl Pts',(1.66971162267453,80.0268253979483,15.2222291610727));
#64284=CARTESIAN_POINT('Ctrl Pts',(0.547199253253971,80.1798998503795,15.8105971993939));
#64285=CARTESIAN_POINT('Ctrl Pts',(-0.727981122835118,80.3343010812489,
15.7879628963548));
#64286=CARTESIAN_POINT('Ctrl Pts',(-1.84732775179652,80.4900469443413,15.1520042048194));
#64287=CARTESIAN_POINT('Ctrl Pts',(-2.53062237483268,80.6471503561707,14.0474538758371));
#64288=CARTESIAN_POINT('Ctrl Pts',(-2.583795294778,80.7660015792739,13.0667538970152));
#64289=CARTESIAN_POINT('Ctrl Pts',(-2.419663350694,80.8456631942111,12.4486116633369));
#64290=CARTESIAN_POINT('Ctrl Pts',(-2.25973962728962,80.8988847286658,12.0525407444864));
#64291=CARTESIAN_POINT('Ctrl Pts',(-1.85250609537659,80.9923212863861,11.4173090196543));
#64292=CARTESIAN_POINT('Ctrl Pts',(-0.953061471973522,81.1266550042549,
10.7665713141076));
#64293=CARTESIAN_POINT('Ctrl Pts',(0.380411183334777,81.2892116660939,10.598648316789));
#64294=CARTESIAN_POINT('Ctrl Pts',(1.64161048251426,81.4531118561961,11.0922447158354));
#64295=CARTESIAN_POINT('Ctrl Pts',(2.51880194682208,81.6183365405957,12.1394809704407));
#64296=CARTESIAN_POINT('Ctrl Pts',(2.78900044588513,81.7848625636954,13.4891724049134));
#64297=CARTESIAN_POINT('Ctrl Pts',(2.37641051851043,81.9526613455049,14.8131500696841));
#64298=CARTESIAN_POINT('Ctrl Pts',(1.37195214889153,82.1216990768183,15.785515396503));
#64299=CARTESIAN_POINT('Ctrl Pts',(0.0159564383937635,82.2919388049734,
16.1580643069455));
#64300=CARTESIAN_POINT('Ctrl Pts',(-1.51833690916597,82.4823804196777,15.800814216761));
#64301=CARTESIAN_POINT('Ctrl Pts',(-2.7463070185402,82.6934517695579,14.502401068678));
#64302=CARTESIAN_POINT('Ctrl Pts',(-2.92376118450403,82.9255626157282,12.5434977446069));
#64303=CARTESIAN_POINT('Ctrl Pts',(-2.00278521417108,83.1252903723912,11.1255308870361));
#64304=CARTESIAN_POINT('Ctrl Pts',(-0.793471469324382,83.2917872144671,
10.5087170763097));
#64305=CARTESIAN_POINT('Ctrl Pts',(0.641937829759612,83.4687003631288,10.3608544419188));
#64306=CARTESIAN_POINT('Ctrl Pts',(2.35159422659933,83.6909444009111,11.2096801135279));
#64307=CARTESIAN_POINT('Ctrl Pts',(3.16230856315989,83.9591494954575,13.3702110495627));
#64308=CARTESIAN_POINT('Ctrl Pts',(2.27944251111824,84.2286227343307,15.5119157619708));
#64309=CARTESIAN_POINT('Ctrl Pts',(0.166108420889751,84.4990850763539,16.48184697234));
#64310=CARTESIAN_POINT('Ctrl Pts',(-2.04768877649022,84.7702780743964,15.7493822978251));
#64311=CARTESIAN_POINT('Ctrl Pts',(-3.21668675418916,85.0534252541687,13.6135743694018));
#64312=CARTESIAN_POINT('Ctrl Pts',(-2.7333269170916,85.246159705883,11.999433035059));
#64313=CARTESIAN_POINT('Ctrl Pts',(-2.18997670931989,85.3482511062504,11.3864423131751));
#64314=CARTESIAN_POINT('Ctrl Pts',(2.11400126982079,72.5921344688769,11.9614452997087));
#64315=CARTESIAN_POINT('Ctrl Pts',(2.44657192402459,72.6737282681649,12.5248544126962));
#64316=CARTESIAN_POINT('Ctrl Pts',(2.62655647816917,72.8313620441591,13.8750534144082));
#64317=CARTESIAN_POINT('Ctrl Pts',(1.46293921239302,73.0602226664433,15.464840373363));
#64318=CARTESIAN_POINT('Ctrl Pts',(-0.395992436705256,73.2801652202774,
15.8151908423103));
#64319=CARTESIAN_POINT('Ctrl Pts',(-1.95735595201862,73.4947422201155,14.8320541464193));
#64320=CARTESIAN_POINT('Ctrl Pts',(-2.4168177065979,73.7041590901459,13.0896455776762));
#64321=CARTESIAN_POINT('Ctrl Pts',(-1.5859522538978,73.9086682680316,11.5397596013732));
#64322=CARTESIAN_POINT('Ctrl Pts',(0.0427972084866695,74.1085632075843,
10.9847546642431));
#64323=CARTESIAN_POINT('Ctrl Pts',(1.40464546317404,74.282443139662,11.598143337626));
#64324=CARTESIAN_POINT('Ctrl Pts',(2.02378524752384,74.4320542615553,12.6705418050936));
#64325=CARTESIAN_POINT('Ctrl Pts',(2.05148174514243,74.5586738895749,13.7165617231474));
#64326=CARTESIAN_POINT('Ctrl Pts',(1.57845917341493,74.6837993155188,14.6375281948537));
#64327=CARTESIAN_POINT('Ctrl Pts',(0.731596287459446,74.8075601042579,15.2125389765525));
#64328=CARTESIAN_POINT('Ctrl Pts',(-0.109239747278009,74.9096711595105,
15.2936998892093));
#64329=CARTESIAN_POINT('Ctrl Pts',(-0.739421878846066,74.9908135551944,
15.1132247212721));
#64330=CARTESIAN_POINT('Ctrl Pts',(-1.30424230768499,75.0716186950129,14.7852507037284));
#64331=CARTESIAN_POINT('Ctrl Pts',(-1.71528939937333,75.1519493242468,14.2634652874395));
#64332=CARTESIAN_POINT('Ctrl Pts',(-1.87795818849642,75.2218943410776,13.7221286614836));
#64333=CARTESIAN_POINT('Ctrl Pts',(-1.90785626656966,75.2567845583079,13.4434866192867));
#64334=CARTESIAN_POINT('Ctrl Pts',(-1.90945967930417,75.2767017106063,13.2838025717218));
#64335=CARTESIAN_POINT('Ctrl Pts',(-1.87667530992554,75.3662684809731,12.5658054628048));
#64336=CARTESIAN_POINT('Ctrl Pts',(-1.05385288366353,75.5295238393814,11.333560316721));
#64337=CARTESIAN_POINT('Ctrl Pts',(0.727721240697154,75.7262878355396,11.3544296227473));
#64338=CARTESIAN_POINT('Ctrl Pts',(1.66290989686987,75.8836491603605,12.2599974138533));
#64339=CARTESIAN_POINT('Ctrl Pts',(2.07105759775679,76.0411926599979,13.4989579444158));
#64340=CARTESIAN_POINT('Ctrl Pts',(1.60813745114241,76.1647260288924,14.5118646842719));
#64341=CARTESIAN_POINT('Ctrl Pts',(1.01370449200879,76.2541473608778,14.9157286009759));
#64342=CARTESIAN_POINT('Ctrl Pts',(0.877105409648848,76.2740317928892,14.9977273501975));
#64343=CARTESIAN_POINT('Ctrl Pts',(0.624398373750998,76.3088669672229,15.1180953077808));
#64344=CARTESIAN_POINT('Ctrl Pts',(0.234880608744721,76.3587322957282,15.2210143427862));
#64345=CARTESIAN_POINT('Ctrl Pts',(-0.250096497706049,76.4187615145809,
15.2247099753646));
#64346=CARTESIAN_POINT('Ctrl Pts',(-0.880416317409708,76.4990766172484,
15.0700227489227));
#64347=CARTESIAN_POINT('Ctrl Pts',(-1.56243238319545,76.6000308225549,14.5883324115654));
#64348=CARTESIAN_POINT('Ctrl Pts',(-2.00764411884039,76.7222237719016,13.6807376769993));
#64349=CARTESIAN_POINT('Ctrl Pts',(-1.96368626779247,76.8456034839983,12.6613314161801));
#64350=CARTESIAN_POINT('Ctrl Pts',(-1.43129952468551,76.9703076776975,11.7780135758093));
#64351=CARTESIAN_POINT('Ctrl Pts',(-0.530713152096587,77.0964679399452,
11.2515132367637));
#64352=CARTESIAN_POINT('Ctrl Pts',(0.525209577400925,77.2242101120139,11.2200044469327));
#64353=CARTESIAN_POINT('Ctrl Pts',(1.47930000590277,77.3536569654321,11.7050193841296));
#64354=CARTESIAN_POINT('Ctrl Pts',(2.09440695070407,77.4849156074468,12.5990396918098));
#64355=CARTESIAN_POINT('Ctrl Pts',(2.20722246901762,77.6180989233271,13.6945539962748));
#64356=CARTESIAN_POINT('Ctrl Pts',(1.77536029710735,77.7533036022579,14.7259205007336));
#64357=CARTESIAN_POINT('Ctrl Pts',(0.88856230688776,77.8906211453096,15.4345912991052));
#64358=CARTESIAN_POINT('Ctrl Pts',(-0.247446942677673,78.030136223062,15.6373175651695));
#64359=CARTESIAN_POINT('Ctrl Pts',(-1.35808520330174,78.1719217932686,15.263780897275));
#64360=CARTESIAN_POINT('Ctrl Pts',(-2.26085945302493,78.3320593752434,14.2938422000058));
#64361=CARTESIAN_POINT('Ctrl Pts',(-2.51334079562032,78.5116265073234,12.7948606674629));
#64362=CARTESIAN_POINT('Ctrl Pts',(-1.70257896904877,78.7118873980016,11.3029462694074));
#64363=CARTESIAN_POINT('Ctrl Pts',(-0.375335441075516,78.8824803546856,
10.7339057197809));
#64364=CARTESIAN_POINT('Ctrl Pts',(0.608207457444419,79.0038643062108,10.8296543455799));
#64365=CARTESIAN_POINT('Ctrl Pts',(1.13531391475293,79.0737906319567,11.0213436095844));
#64366=CARTESIAN_POINT('Ctrl Pts',(2.12905331295049,79.2143948677298,11.5704310732741));
#64367=CARTESIAN_POINT('Ctrl Pts',(2.79190646248625,79.3755446330857,12.8576231482577));
#64368=CARTESIAN_POINT('Ctrl Pts',(2.47453588556505,79.5766247506289,14.4685468472474));
#64369=CARTESIAN_POINT('Ctrl Pts',(1.78261016529238,79.7247254863011,15.4735020818274));
#64370=CARTESIAN_POINT('Ctrl Pts',(0.53224166037482,79.8938224824188,16.1039449549752));
#64371=CARTESIAN_POINT('Ctrl Pts',(-0.884326710497297,80.0653647111037,
16.0566199197993));
#64372=CARTESIAN_POINT('Ctrl Pts',(-2.12359960142391,80.2393043402407,15.3270088430981));
#64373=CARTESIAN_POINT('Ctrl Pts',(-2.87151909981507,80.415585110026,14.0757968962628));
#64374=CARTESIAN_POINT('Ctrl Pts',(-2.91477610335063,80.5495008981822,12.9697590533731));
#64375=CARTESIAN_POINT('Ctrl Pts',(-2.71864238612076,80.6394665833449,12.2744171641952));
#64376=CARTESIAN_POINT('Ctrl Pts',(-2.53097857955019,80.6996258170464,11.8294361385213));
#64377=CARTESIAN_POINT('Ctrl Pts',(-2.05912935167091,80.8053737304426,11.1174256967615));
#64378=CARTESIAN_POINT('Ctrl Pts',(-1.02774628937495,80.957769086886,10.3942004010663));
#64379=CARTESIAN_POINT('Ctrl Pts',(0.491961774271491,81.14266591228,10.2254004512117));
#64380=CARTESIAN_POINT('Ctrl Pts',(1.92153631775683,81.3294930769971,10.8090028063427));
#64381=CARTESIAN_POINT('Ctrl Pts',(2.90590364405399,81.5181393526567,12.0192876816821));
#64382=CARTESIAN_POINT('Ctrl Pts',(3.19262514951605,81.708494257632,13.5667058735148));
#64383=CARTESIAN_POINT('Ctrl Pts',(2.69895917427376,81.9004368774085,15.0745873792813));
#64384=CARTESIAN_POINT('Ctrl Pts',(1.5337355093842,82.0938404002092,16.1708527567328));
#64385=CARTESIAN_POINT('Ctrl Pts',(-0.0235831907925716,82.2885768485042,
16.5750065021912));
#64386=CARTESIAN_POINT('Ctrl Pts',(-1.77188612262323,82.5062748522241,16.1417043273099));
#64387=CARTESIAN_POINT('Ctrl Pts',(-3.15274531183509,82.7472461071415,14.6391652740677));
#64388=CARTESIAN_POINT('Ctrl Pts',(-3.32282392948499,83.0116460641456,12.4046397790249));
#64389=CARTESIAN_POINT('Ctrl Pts',(-2.25348615727359,83.238488708394,10.8091422650043));
#64390=CARTESIAN_POINT('Ctrl Pts',(-0.873992247862047,83.4270503118526,
10.1298463297532));
#64391=CARTESIAN_POINT('Ctrl Pts',(0.750569308195157,83.6269523778323,9.98560692981242));
#64392=CARTESIAN_POINT('Ctrl Pts',(2.66122369179064,83.8771457597194,10.9699367086606));
#64393=CARTESIAN_POINT('Ctrl Pts',(3.53216814210731,84.1773317949803,13.4021155250038));
#64394=CARTESIAN_POINT('Ctrl Pts',(2.51386301896827,84.4769618827252,15.7686902121962));
#64395=CARTESIAN_POINT('Ctrl Pts',(0.164304520999366,84.7754858579762,16.8030938832357));
#64396=CARTESIAN_POINT('Ctrl Pts',(-2.24721164156027,85.0724162007226,15.9625867670223));
#64397=CARTESIAN_POINT('Ctrl Pts',(-3.47867858274328,85.3797239652224,13.6238161233426));
#64398=CARTESIAN_POINT('Ctrl Pts',(-2.92994214133404,85.5868241148751,11.8975259974901));
#64399=CARTESIAN_POINT('Ctrl Pts',(-2.33977172532943,85.6958993282798,11.2513135886875));
#64400=CARTESIAN_POINT('Ctrl Pts',(2.15580107008468,72.6023598638413,12.0348501216199));
#64401=CARTESIAN_POINT('Ctrl Pts',(2.16192017837505,72.6039627934161,12.0461164217861));
#64402=CARTESIAN_POINT('Ctrl Pts',(2.16794896383192,72.6055628651636,12.0574294127845));
#64403=CARTESIAN_POINT('Ctrl Pts',(2.1738869405785,72.6071602218535,12.0687872536258));
#64404=CARTESIAN_POINT('Ctrl Pts',(2.21802819426934,72.6190345234706,12.1532182568705));
#64405=CARTESIAN_POINT('Ctrl Pts',(2.2571383557657,72.6307519284214,12.2401050802808));
#64406=CARTESIAN_POINT('Ctrl Pts',(2.29106954971183,72.6424358407151,12.3287779317616));
#64407=CARTESIAN_POINT('Ctrl Pts',(2.31366187768963,72.6502153128735,12.3878187703058));
#64408=CARTESIAN_POINT('Ctrl Pts',(2.33395858787518,72.6579798501987,12.4476503642754));
#64409=CARTESIAN_POINT('Ctrl Pts',(2.35192204040781,72.6657647884643,12.5080637449848));
#64410=CARTESIAN_POINT('Ctrl Pts',(2.35913568189839,72.6688910111975,12.5323241408569));
#64411=CARTESIAN_POINT('Ctrl Pts',(2.36597362167121,72.672020934687,12.5566802346146));
#64412=CARTESIAN_POINT('Ctrl Pts',(2.37243396813088,72.6751572074983,12.5811204503354));
#64413=CARTESIAN_POINT('Ctrl Pts',(2.40069571426959,72.6888772992249,12.6880378078779));
#64414=CARTESIAN_POINT('Ctrl Pts',(2.42173598994609,72.7027242333294,12.7965775482791));
#64415=CARTESIAN_POINT('Ctrl Pts',(2.43557776633446,72.7166225538976,12.9058136538946));
#64416=CARTESIAN_POINT('Ctrl Pts',(2.44159629602123,72.7226656695056,12.9533105015584));
#64417=CARTESIAN_POINT('Ctrl Pts',(2.44625339444013,72.7287185409955,13.0009394630651));
#64418=CARTESIAN_POINT('Ctrl Pts',(2.44954849542459,72.7347751585101,13.0486262392927));
#64419=CARTESIAN_POINT('Ctrl Pts',(2.45898976623568,72.7521288500734,13.1852605247354));
#64420=CARTESIAN_POINT('Ctrl Pts',(2.45732387889671,72.7693965007803,13.3223587491889));
#64421=CARTESIAN_POINT('Ctrl Pts',(2.44450040696102,72.7864518110501,13.4579925334706));
#64422=CARTESIAN_POINT('Ctrl Pts',(2.44275221189448,72.7887769231119,13.4764831820038));
#64423=CARTESIAN_POINT('Ctrl Pts',(2.44079668027458,72.7910981002317,13.4949466863257));
#64424=CARTESIAN_POINT('Ctrl Pts',(2.43863370702352,72.7934150333741,13.5133782324569));
#64425=CARTESIAN_POINT('Ctrl Pts',(2.43101421930226,72.8015768743126,13.578306885348));
#64426=CARTESIAN_POINT('Ctrl Pts',(2.42078933591859,72.8097296752927,13.6428321004225));
#64427=CARTESIAN_POINT('Ctrl Pts',(2.4079517140088,72.8178702372941,13.7067146591538));
#64428=CARTESIAN_POINT('Ctrl Pts',(2.40049642993096,72.8225977641444,13.7438136348291));
#64429=CARTESIAN_POINT('Ctrl Pts',(2.39216034593699,72.827321030583,13.7806948458528));
#64430=CARTESIAN_POINT('Ctrl Pts',(2.38294349257466,72.8320393982253,13.8173116957368));
#64431=CARTESIAN_POINT('Ctrl Pts',(2.38179041241278,72.8326296925385,13.8218926694739));
#64432=CARTESIAN_POINT('Ctrl Pts',(2.38062353024195,72.8332199194457,13.8264695779706));
#64433=CARTESIAN_POINT('Ctrl Pts',(2.37944282951223,72.8338100856936,13.8310423918975));
#64434=CARTESIAN_POINT('Ctrl Pts',(2.37505304890306,72.8360042914612,13.8480438634816));
#64435=CARTESIAN_POINT('Ctrl Pts',(2.3704722711849,72.8381976588027,13.8649887411019));
#64436=CARTESIAN_POINT('Ctrl Pts',(2.36570237798596,72.8403905339749,13.8818764406027));
#64437=CARTESIAN_POINT('Ctrl Pts',(2.34233269716483,72.8511343369738,13.9646162694997));
#64438=CARTESIAN_POINT('Ctrl Pts',(2.31455794741775,72.8616876594999,14.045967816978));
#64439=CARTESIAN_POINT('Ctrl Pts',(2.28258923074345,72.8722215415317,14.1254793035469));
#64440=CARTESIAN_POINT('Ctrl Pts',(2.27581984726379,72.874452093597,14.1423158800385));
#64441=CARTESIAN_POINT('Ctrl Pts',(2.26886250892418,72.8766817502705,14.1590697932812));
#64442=CARTESIAN_POINT('Ctrl Pts',(2.26171938489829,72.8789120969552,14.1757365035937));
#64443=CARTESIAN_POINT('Ctrl Pts',(2.21603499722703,72.8931764471494,14.2823297046028));
#64444=CARTESIAN_POINT('Ctrl Pts',(2.16268031957557,72.9075604542274,14.3853643597476));
#64445=CARTESIAN_POINT('Ctrl Pts',(2.10244343550131,72.9220139605729,14.4839797541313));
#64446=CARTESIAN_POINT('Ctrl Pts',(2.09215488785125,72.9244826405359,14.5008234073139));
#64447=CARTESIAN_POINT('Ctrl Pts',(2.08166544187366,72.9269533544155,14.5175381318809));
#64448=CARTESIAN_POINT('Ctrl Pts',(2.07097887523531,72.9294258602769,14.5341196249307));
#64449=CARTESIAN_POINT('Ctrl Pts',(2.0074454631808,72.9441253179249,14.632699352739));
#64450=CARTESIAN_POINT('Ctrl Pts',(1.93694733610837,72.9588863338002,14.7265680673354));
#64451=CARTESIAN_POINT('Ctrl Pts',(1.86035589125161,72.97358065531,14.8147952427477));
#64452=CARTESIAN_POINT('Ctrl Pts',(1.84758283533787,72.9760312082486,14.8295087743537));
#64453=CARTESIAN_POINT('Ctrl Pts',(1.83464024041615,72.9784799230308,14.8440654955037));
#64454=CARTESIAN_POINT('Ctrl Pts',(1.82153205289834,72.9809262250919,14.8584611940775));
#64455=CARTESIAN_POINT('Ctrl Pts',(1.74342569442705,72.9955027441918,14.9442393073152));
#64456=CARTESIAN_POINT('Ctrl Pts',(1.65946718255774,73.0099450409698,15.0243272921312));
#64457=CARTESIAN_POINT('Ctrl Pts',(1.57042581740269,73.0243423290664,15.0976555791592));
#64458=CARTESIAN_POINT('Ctrl Pts',(1.55938921075379,73.0261268615166,15.1067445622263));
#64459=CARTESIAN_POINT('Ctrl Pts',(1.54827457741663,73.0279106956431,15.1157296765225));
#64460=CARTESIAN_POINT('Ctrl Pts',(1.53708343697713,73.0296939954808,15.1246088739482));
#64461=CARTESIAN_POINT('Ctrl Pts',(1.49923675511284,73.0357248358578,15.1546369271208));
#64462=CARTESIAN_POINT('Ctrl Pts',(1.46051578423071,73.0417494318799,15.1834527654948));
#64463=CARTESIAN_POINT('Ctrl Pts',(1.42098929437649,73.0477663904587,15.2109790637862));
#64464=CARTESIAN_POINT('Ctrl Pts',(1.39571046045946,73.0516144856769,15.2285832761871));
#64465=CARTESIAN_POINT('Ctrl Pts',(1.37010340299785,73.0554592777747,15.2456593263385));
#64466=CARTESIAN_POINT('Ctrl Pts',(1.34418259454164,73.0593009687491,15.2621899621411));
#64467=CARTESIAN_POINT('Ctrl Pts',(1.32300331453945,73.0624399236534,15.2756967539863));
#64468=CARTESIAN_POINT('Ctrl Pts',(1.30161062933687,73.0655773917466,15.2888419327909));
#64469=CARTESIAN_POINT('Ctrl Pts',(1.28001612212571,73.068713528788,15.3016244983358));
#64470=CARTESIAN_POINT('Ctrl Pts',(1.25855902645133,73.0718297097634,15.3143257250496));
#64471=CARTESIAN_POINT('Ctrl Pts',(1.23690409112748,73.074944365242,15.3266680187035));
#64472=CARTESIAN_POINT('Ctrl Pts',(1.21507475280123,73.0780375247887,15.3386641411617));
#64473=CARTESIAN_POINT('Ctrl Pts',(1.10130146538182,73.0941588989175,15.4011872588099));
#64474=CARTESIAN_POINT('Ctrl Pts',(0.98254969375926,73.1101790706159,15.453953177252));
#64475=CARTESIAN_POINT('Ctrl Pts',(0.860533429664269,73.1261844231029,15.4967042795224));
#64476=CARTESIAN_POINT('Ctrl Pts',(0.840874461480389,73.1287631671551,15.5035922347109));
#64477=CARTESIAN_POINT('Ctrl Pts',(0.821130823890476,73.1313415135199,15.5102201352121));
#64478=CARTESIAN_POINT('Ctrl Pts',(0.801309776798585,73.1339198083819,15.5165868159723));
#64479=CARTESIAN_POINT('Ctrl Pts',(0.653862888784499,73.1530994991431,15.5639479498577));
#64480=CARTESIAN_POINT('Ctrl Pts',(0.502131670630755,73.1722760403049,15.596854524438));
#64481=CARTESIAN_POINT('Ctrl Pts',(0.349169946951665,73.191436916284,15.6149530377744));
#64482=CARTESIAN_POINT('Ctrl Pts',(0.197225453902707,73.2104703680325,15.632931191836));
#64483=CARTESIAN_POINT('Ctrl Pts',(0.0440672956689506,73.2294879697,15.6362965414167));
#64484=CARTESIAN_POINT('Ctrl Pts',(-0.107296279315945,73.2484596733022,
15.6247246061563));
#64485=CARTESIAN_POINT('Ctrl Pts',(-0.169382485558562,73.2562414735321,
15.6199780377743));
#64486=CARTESIAN_POINT('Ctrl Pts',(-0.231166633660567,73.2640153744315,
15.6127186623935));
#64487=CARTESIAN_POINT('Ctrl Pts',(-0.292440818079412,73.2717786369157,
15.6029258396425));
#64488=CARTESIAN_POINT('Ctrl Pts',(-0.310486323983427,73.2740649504802,
15.6000418120141));
#64489=CARTESIAN_POINT('Ctrl Pts',(-0.328487611692874,73.2763503415797,
15.5969380586081));
#64490=CARTESIAN_POINT('Ctrl Pts',(-0.346440106727422,73.2786330779197,
15.5936157835197));
#64491=CARTESIAN_POINT('Ctrl Pts',(-0.346450065622348,73.2786343442357,
15.5936139405341));
#64492=CARTESIAN_POINT('Ctrl Pts',(-0.346460024503054,73.2786356105509,
15.5936120974813));
#64493=CARTESIAN_POINT('Ctrl Pts',(-0.346469983369502,73.2786368768654,
15.593610254361));
#64494=CARTESIAN_POINT('Ctrl Pts',(-0.457116323583858,73.2927060544194,
15.5731325717345));
#64495=CARTESIAN_POINT('Ctrl Pts',(-0.566006383550437,73.306681464898,15.5443376672788));
#64496=CARTESIAN_POINT('Ctrl Pts',(-0.672080024035714,73.3205943231013,
15.5078791483193));
#64497=CARTESIAN_POINT('Ctrl Pts',(-0.710542744613808,73.3256391803822,
15.494659145489));
#64498=CARTESIAN_POINT('Ctrl Pts',(-0.748635013790737,73.3306757873652,
15.4804320013116));
#64499=CARTESIAN_POINT('Ctrl Pts',(-0.786305931834455,73.3357055426912,
15.4652305097075));
#64500=CARTESIAN_POINT('Ctrl Pts',(-0.906109752180169,73.351701539995,15.4168856096176));
#64501=CARTESIAN_POINT('Ctrl Pts',(-1.02165254345175,73.3676303883617,15.3586820909752));
#64502=CARTESIAN_POINT('Ctrl Pts',(-1.13135734234018,73.3835579983143,15.2916599425043));
#64503=CARTESIAN_POINT('Ctrl Pts',(-1.15422573328892,73.386878170403,15.2776889156305));
#64504=CARTESIAN_POINT('Ctrl Pts',(-1.17684034207221,73.3901982654702,15.2633348389487));
#64505=CARTESIAN_POINT('Ctrl Pts',(-1.19918673917259,73.3935188435732,15.2486073777911));
#64506=CARTESIAN_POINT('Ctrl Pts',(-1.30762698986721,73.4096325965118,15.1771394998663));
#64507=CARTESIAN_POINT('Ctrl Pts',(-1.40975438516136,73.4257600997185,15.0968766406711));
#64508=CARTESIAN_POINT('Ctrl Pts',(-1.50398226142444,73.4419645783231,15.0088841574503));
#64509=CARTESIAN_POINT('Ctrl Pts',(-1.51950548048396,73.4446341245456,14.9943881648969));
#64510=CARTESIAN_POINT('Ctrl Pts',(-1.53481419809293,73.447305745063,14.9796824189891));
#64511=CARTESIAN_POINT('Ctrl Pts',(-1.54990119041512,73.4499797049384,14.9647717256329));
#64512=CARTESIAN_POINT('Ctrl Pts',(-1.57165429876864,73.4538351413076,14.9432728131076));
#64513=CARTESIAN_POINT('Ctrl Pts',(-1.59294695284777,73.4576953883003,14.9213475693769));
#64514=CARTESIAN_POINT('Ctrl Pts',(-1.61375807842776,73.4615611018664,14.8990099929552));
#64515=CARTESIAN_POINT('Ctrl Pts',(-1.66414575427112,73.470920726425,14.8449264905739));
#64516=CARTESIAN_POINT('Ctrl Pts',(-1.71171359747127,73.480313309835,14.7884222347898));
#64517=CARTESIAN_POINT('Ctrl Pts',(-1.7562799676571,73.4896314192762,14.7297818120333));
#64518=CARTESIAN_POINT('Ctrl Pts',(-1.76228567573715,73.4908871160028,14.7218795023029));
#64519=CARTESIAN_POINT('Ctrl Pts',(-1.76823692368156,73.4921414701709,14.7139383385766));
#64520=CARTESIAN_POINT('Ctrl Pts',(-1.77413330815155,73.4933942281411,14.7059589578865));
#64521=CARTESIAN_POINT('Ctrl Pts',(-1.77414438921039,73.4933965824456,14.7059439622587));
#64522=CARTESIAN_POINT('Ctrl Pts',(-1.77415547007825,73.4933989367447,14.7059289664928));
#64523=CARTESIAN_POINT('Ctrl Pts',(-1.77416655075512,73.4934012910384,14.705913970589));
#64524=CARTESIAN_POINT('Ctrl Pts',(-1.82681983952755,73.5045884508566,14.6346562609334));
#64525=CARTESIAN_POINT('Ctrl Pts',(-1.87515911625464,73.5156527416839,14.5602781537274));
#64526=CARTESIAN_POINT('Ctrl Pts',(-1.91895260074508,73.5266327185297,14.4833995315359));
#64527=CARTESIAN_POINT('Ctrl Pts',(-1.93911324416827,73.531687429306,14.4480079086289));
#64528=CARTESIAN_POINT('Ctrl Pts',(-1.9583107599767,73.5367242273436,14.4120870492267));
#64529=CARTESIAN_POINT('Ctrl Pts',(-1.97652406882038,73.5417466436806,14.3757007775802));
#64530=CARTESIAN_POINT('Ctrl Pts',(-2.02030622038373,73.553819803762,14.2882334604812));
#64531=CARTESIAN_POINT('Ctrl Pts',(-2.05839898090737,73.5658119149367,14.1980736548514));
#64532=CARTESIAN_POINT('Ctrl Pts',(-2.09053924690994,73.5777931504987,14.1060587105315));
#64533=CARTESIAN_POINT('Ctrl Pts',(-2.10172875730914,73.5819643717296,14.0740240604056));
#64534=CARTESIAN_POINT('Ctrl Pts',(-2.1121967939929,73.5861342171208,14.0417650171957));
#64535=CARTESIAN_POINT('Ctrl Pts',(-2.12193239364035,73.5903054616774,14.0093183825834));
#64536=CARTESIAN_POINT('Ctrl Pts',(-2.1505626523661,73.6025721750993,13.9138999618008));
#64537=CARTESIAN_POINT('Ctrl Pts',(-2.17285889501759,73.6148532268291,13.8168552171571));
#64538=CARTESIAN_POINT('Ctrl Pts',(-2.18856600348633,73.6272217037332,13.7190552747927));
#64539=CARTESIAN_POINT('Ctrl Pts',(-2.19327238703961,73.6309277197957,13.6897510880182));
#64540=CARTESIAN_POINT('Ctrl Pts',(-2.19738702241765,73.6346415366831,13.6603794056819));
#64541=CARTESIAN_POINT('Ctrl Pts',(-2.20090267875922,73.6383649959301,13.6309644939029));
#64542=CARTESIAN_POINT('Ctrl Pts',(-2.20373076100735,73.6413602400537,13.6073024001856));
#64543=CARTESIAN_POINT('Ctrl Pts',(-2.20617146824096,73.6443616997158,13.5836117511436));
#64544=CARTESIAN_POINT('Ctrl Pts',(-2.20822122713813,73.6473702483784,13.5599045428459));
#64545=CARTESIAN_POINT('Ctrl Pts',(-2.21452692848637,73.656625487804,13.4869737335044));
#64546=CARTESIAN_POINT('Ctrl Pts',(-2.21713216075013,73.665950917194,13.4138715163576));
#64547=CARTESIAN_POINT('Ctrl Pts',(-2.21609970788283,73.6752549137358,13.340961115631));
#64548=CARTESIAN_POINT('Ctrl Pts',(-2.21529108434837,73.6825418619409,13.2838572343777));
#64549=CARTESIAN_POINT('Ctrl Pts',(-2.21225139475122,73.6898157910752,13.2268700014323));
#64550=CARTESIAN_POINT('Ctrl Pts',(-2.20700918463086,73.6970355538379,13.1701517901074));
#64551=CARTESIAN_POINT('Ctrl Pts',(-2.20551912316951,73.6990877207686,13.1540300363218));
#64552=CARTESIAN_POINT('Ctrl Pts',(-2.20385120819904,73.7011353779884,13.1379308463664));
#64553=CARTESIAN_POINT('Ctrl Pts',(-2.20200878525503,73.7031758546802,13.1218581211112));
#64554=CARTESIAN_POINT('Ctrl Pts',(-2.2020038117226,73.7031813628492,13.1218147335597));
#64555=CARTESIAN_POINT('Ctrl Pts',(-2.20199883689239,73.7031868709847,13.1217713461652));
#64556=CARTESIAN_POINT('Ctrl Pts',(-2.20199386076437,73.7031923790868,13.1217279589276));
#64557=CARTESIAN_POINT('Ctrl Pts',(-2.19276919631323,73.7134032081921,13.0412974100706));
#64558=CARTESIAN_POINT('Ctrl Pts',(-2.17908064415196,73.723499157845,12.9614044145176));
#64559=CARTESIAN_POINT('Ctrl Pts',(-2.16110800790781,73.7335132188269,12.8825566075815));
#64560=CARTESIAN_POINT('Ctrl Pts',(-2.15188713482429,73.7386509395324,12.8421036873312));
#64561=CARTESIAN_POINT('Ctrl Pts',(-2.1415393667158,73.74376705314,12.8019262799138));
#64562=CARTESIAN_POINT('Ctrl Pts',(-2.13009387019467,73.7488656773271,12.7620949609708));
#64563=CARTESIAN_POINT('Ctrl Pts',(-2.10664860637749,73.7593098366477,12.6805034127946));
#64564=CARTESIAN_POINT('Ctrl Pts',(-2.07858308300931,73.7696893584977,12.6003650885137));
#64565=CARTESIAN_POINT('Ctrl Pts',(-2.04611071225278,73.7800714069487,12.5222386907462));
#64566=CARTESIAN_POINT('Ctrl Pts',(-2.03095970140821,73.7849154797713,12.485786350734));
#64567=CARTESIAN_POINT('Ctrl Pts',(-2.01484971883731,73.7897600075159,12.4497726276748));
#64568=CARTESIAN_POINT('Ctrl Pts',(-1.9978048528833,73.794611309703,12.4142572843166));
#64569=CARTESIAN_POINT('Ctrl Pts',(-1.96095408042119,73.8050997602148,12.3374735864842));
#64570=CARTESIAN_POINT('Ctrl Pts',(-1.91972962868822,73.8156218527174,12.263011969038));
#64571=CARTESIAN_POINT('Ctrl Pts',(-1.87435580531654,73.8262430152286,12.1914288817111));
#64572=CARTESIAN_POINT('Ctrl Pts',(-1.86946470236314,73.8273879308533,12.1837125328601));
#64573=CARTESIAN_POINT('Ctrl Pts',(-1.86452539796778,73.8285339911167,12.1760296798575));
#64574=CARTESIAN_POINT('Ctrl Pts',(-1.85953818476383,73.8296812732155,12.1683810538582));
#64575=CARTESIAN_POINT('Ctrl Pts',(-1.81930052417095,73.8389377348526,12.1066706748604));
#64576=CARTESIAN_POINT('Ctrl Pts',(-1.77593483395429,73.8482765385491,12.0471757256674));
#64577=CARTESIAN_POINT('Ctrl Pts',(-1.72974674754801,73.8576244811704,11.990142400919));
#64578=CARTESIAN_POINT('Ctrl Pts',(-1.69842882972124,73.8639628710377,11.9514708490789));
#64579=CARTESIAN_POINT('Ctrl Pts',(-1.66581268519627,73.8703055972869,11.9139301370438));
#64580=CARTESIAN_POINT('Ctrl Pts',(-1.63198357026612,73.8766315687028,11.8775879042256));
#64581=CARTESIAN_POINT('Ctrl Pts',(-1.58621468770642,73.8851902508736,11.8284189150501));
#64582=CARTESIAN_POINT('Ctrl Pts',(-1.53837185948978,73.8936192613437,11.7813332420409));
#64583=CARTESIAN_POINT('Ctrl Pts',(-1.48849343993653,73.901996996571,11.736671370713));
#64584=CARTESIAN_POINT('Ctrl Pts',(-1.47682194376587,73.9039573775433,11.726220541179));
#64585=CARTESIAN_POINT('Ctrl Pts',(-1.4650391333866,73.9059149229783,11.7159025973676));
#64586=CARTESIAN_POINT('Ctrl Pts',(-1.45314578222703,73.9078705859488,11.7057221988261));
#64587=CARTESIAN_POINT('Ctrl Pts',(-1.45308771947485,73.9078801333987,11.7056724986239));
#64588=CARTESIAN_POINT('Ctrl Pts',(-1.45302965393809,73.9078896808523,11.705622801649));
#64589=CARTESIAN_POINT('Ctrl Pts',(-1.45297158561719,73.9078992283094,11.7055731079019));
#64590=CARTESIAN_POINT('Ctrl Pts',(-1.40195888298438,73.9162866172158,11.6619174226086));
#64591=CARTESIAN_POINT('Ctrl Pts',(-1.34879776939936,73.924676340523,11.6207571729945));
#64592=CARTESIAN_POINT('Ctrl Pts',(-1.29389435594591,73.9330056935469,11.5821578726855));
#64593=CARTESIAN_POINT('Ctrl Pts',(-1.25845225271705,73.9383825867333,11.557240653517));
#64594=CARTESIAN_POINT('Ctrl Pts',(-1.22228411112995,73.9437344221045,11.5333895253827));
#64595=CARTESIAN_POINT('Ctrl Pts',(-1.18549692114481,73.9490454273909,11.5106108692279));
#64596=CARTESIAN_POINT('Ctrl Pts',(-1.12270205757729,73.95811118785,11.4717282417135));
#64597=CARTESIAN_POINT('Ctrl Pts',(-1.05801534278977,73.9671275808998,11.4360770145799));
#64598=CARTESIAN_POINT('Ctrl Pts',(-0.991780224657834,73.9761565253841,
11.4038822871771));
#64599=CARTESIAN_POINT('Ctrl Pts',(-0.957465927451193,73.9808341328714,
11.3872032281561));
#64600=CARTESIAN_POINT('Ctrl Pts',(-0.922736814478702,73.9855149989163,
11.3714522399752));
#64601=CARTESIAN_POINT('Ctrl Pts',(-0.887645822571864,73.9902070189536,
11.3566623625175));
#64602=CARTESIAN_POINT('Ctrl Pts',(-0.842566350883857,73.9962345996214,
11.3376626185407));
#64603=CARTESIAN_POINT('Ctrl Pts',(-0.796885996201166,74.0022810870724,
11.3202472120307));
#64604=CARTESIAN_POINT('Ctrl Pts',(-0.750710375381237,74.0083616693734,
11.3044781595841));
#64605=CARTESIAN_POINT('Ctrl Pts',(-0.679517172795227,74.0177366624956,
11.280165560739));
#64606=CARTESIAN_POINT('Ctrl Pts',(-0.607139682664314,74.0271948678836,
11.2597667286002));
#64607=CARTESIAN_POINT('Ctrl Pts',(-0.534019870815996,74.0366803874199,
11.243273778465));
#64608=CARTESIAN_POINT('Ctrl Pts',(-0.498490175439331,74.0412895023929,
11.2352596783278));
#64609=CARTESIAN_POINT('Ctrl Pts',(-0.462784429619876,74.0459051630657,
11.2281677067626));
#64610=CARTESIAN_POINT('Ctrl Pts',(-0.426948933582017,74.05052150681,11.221996981732));
#64611=CARTESIAN_POINT('Ctrl Pts',(-0.355656275019391,74.0597054572156,
11.2097206791457));
#64612=CARTESIAN_POINT('Ctrl Pts',(-0.283869348663841,74.0688646074762,
11.2010327111927));
#64613=CARTESIAN_POINT('Ctrl Pts',(-0.211981529695926,74.0779444575951,
11.1959149698796));
#64614=CARTESIAN_POINT('Ctrl Pts',(-0.17470091938458,74.0826532157524,11.1932609386083));
#64615=CARTESIAN_POINT('Ctrl Pts',(-0.137392377266259,74.0873407536378,
11.1915668031196));
#64616=CARTESIAN_POINT('Ctrl Pts',(-0.100105390170106,74.0920001644583,
11.1908289012013));
#64617=CARTESIAN_POINT('Ctrl Pts',(-0.0578756745461771,74.0972772224683,
11.1899931836871));
#64618=CARTESIAN_POINT('Ctrl Pts',(-0.0156664371984247,74.102550467867,
11.1904616056632));
#64619=CARTESIAN_POINT('Ctrl Pts',(0.0264309564992198,74.1078180194713,
11.1922550027768));
#64620=CARTESIAN_POINT('Ctrl Pts',(0.0265158087497896,74.1078286368414,
11.1922586175798));
#64621=CARTESIAN_POINT('Ctrl Pts',(0.0266006607436696,74.1078392541547,
11.192262237628));
#64622=CARTESIAN_POINT('Ctrl Pts',(0.0266855124800557,74.107849871411,11.1922658629217));
#64623=CARTESIAN_POINT('Ctrl Pts',(0.101313419299133,74.1171878490496,11.1954543431238));
#64624=CARTESIAN_POINT('Ctrl Pts',(0.175740356384215,74.1264815954097,11.2027045332465));
#64625=CARTESIAN_POINT('Ctrl Pts',(0.249507613526737,74.1357024290768,11.2137816289139));
#64626=CARTESIAN_POINT('Ctrl Pts',(0.291954329481528,74.1410082262921,11.2201555453589));
#64627=CARTESIAN_POINT('Ctrl Pts',(0.334183004514007,74.1462899310993,11.2277956156468));
#64628=CARTESIAN_POINT('Ctrl Pts',(0.376110260413564,74.151542474569,11.2366504666802));
#64629=CARTESIAN_POINT('Ctrl Pts',(0.443050390905403,74.159928569431,11.2507879262144));
#64630=CARTESIAN_POINT('Ctrl Pts',(0.5092165201533,74.1683035555664,11.2681827010546));
#64631=CARTESIAN_POINT('Ctrl Pts',(0.574267704063896,74.1767163627487,11.2888025522495));
#64632=CARTESIAN_POINT('Ctrl Pts',(0.592177927910872,74.1790326197445,11.2944797148835));
#64633=CARTESIAN_POINT('Ctrl Pts',(0.610003344532317,74.1813517045966,11.3004012665055));
#64634=CARTESIAN_POINT('Ctrl Pts',(0.627736187584336,74.1836745492012,11.3065663057738));
#64635=CARTESIAN_POINT('Ctrl Pts',(0.704214690597216,74.1936925523816,11.3331549905588));
#64636=CARTESIAN_POINT('Ctrl Pts',(0.778985410996104,74.203783708351,11.3642799566572));
#64637=CARTESIAN_POINT('Ctrl Pts',(0.851609159976651,74.2139085837343,11.3995796397699));
#64638=CARTESIAN_POINT('Ctrl Pts',(0.884238568050055,74.2184576285744,11.4154395723858));
#64639=CARTESIAN_POINT('Ctrl Pts',(0.916435142903122,74.2230135643075,11.4321426550204));
#64640=CARTESIAN_POINT('Ctrl Pts',(0.948161545368537,74.2275732271854,11.4496583945888));
#64641=CARTESIAN_POINT('Ctrl Pts',(1.01668234420536,74.2374209161302,11.4874878481095));
#64642=CARTESIAN_POINT('Ctrl Pts',(1.08300862473964,74.2472846895342,11.5291051564584));
#64643=CARTESIAN_POINT('Ctrl Pts',(1.14673563186435,74.2571223825849,11.574167656761));
#64644=CARTESIAN_POINT('Ctrl Pts',(1.17864519414785,74.262048339307,11.5967314758532));
#64645=CARTESIAN_POINT('Ctrl Pts',(1.20990383371369,74.2669678611424,11.6201593300922));
#64646=CARTESIAN_POINT('Ctrl Pts',(1.24046515772503,74.2718762846754,11.6444102687014));
#64647=CARTESIAN_POINT('Ctrl Pts',(1.2990789038412,74.2812901795278,11.690921288911));
#64648=CARTESIAN_POINT('Ctrl Pts',(1.35512147007713,74.2906619910334,11.7404559421409));
#64649=CARTESIAN_POINT('Ctrl Pts',(1.40824761554792,74.299957959209,11.7927028910783));
#64650=CARTESIAN_POINT('Ctrl Pts',(1.41481470112055,74.3011070623097,11.7991612964744));
#64651=CARTESIAN_POINT('Ctrl Pts',(1.42133728667879,74.3022550132775,11.8056611609397));
#64652=CARTESIAN_POINT('Ctrl Pts',(1.42781477355712,74.3034017540735,11.8122019108332));
#64653=CARTESIAN_POINT('Ctrl Pts',(1.42784095932973,74.3034063898673,11.8122283523517));
#64654=CARTESIAN_POINT('Ctrl Pts',(1.42786714438612,74.303411025645,11.8122547945592));
#64655=CARTESIAN_POINT('Ctrl Pts',(1.4278933287262,74.3034156614065,11.8122812374555));
#64656=CARTESIAN_POINT('Ctrl Pts',(1.47479074149944,74.3117185332416,11.8596417368433));
#64657=CARTESIAN_POINT('Ctrl Pts',(1.51939244327982,74.3199700398038,11.9092158068034));
#64658=CARTESIAN_POINT('Ctrl Pts',(1.56144817870571,74.3282053919733,11.9607895161716));
#64659=CARTESIAN_POINT('Ctrl Pts',(1.58736784102869,74.3332809790527,11.9925752671049));
#64660=CARTESIAN_POINT('Ctrl Pts',(1.61231989656539,74.3383503093373,12.0251196975741));
#64661=CARTESIAN_POINT('Ctrl Pts',(1.63624194944416,74.3434204545349,12.0583636868686));
#64662=CARTESIAN_POINT('Ctrl Pts',(1.65582144490069,74.3475702189954,12.0855729126256));
#64663=CARTESIAN_POINT('Ctrl Pts',(1.67471225449499,74.3517209114023,12.113252850473));
#64664=CARTESIAN_POINT('Ctrl Pts',(1.69288239112283,74.3558768547122,12.1413737924115));
#64665=CARTESIAN_POINT('Ctrl Pts',(1.73572447055419,74.365675859367,12.2076781715634));
#64666=CARTESIAN_POINT('Ctrl Pts',(1.77455982308679,74.3755054254738,12.2764389500244));
#64667=CARTESIAN_POINT('Ctrl Pts',(1.80926351293272,74.385335506677,12.3471105565211));
#64668=CARTESIAN_POINT('Ctrl Pts',(1.82146603669404,74.3887919633244,12.3719601319223));
#64669=CARTESIAN_POINT('Ctrl Pts',(1.83315791100867,74.392248542058,12.3970463909998));
#64670=CARTESIAN_POINT('Ctrl Pts',(1.84433416221169,74.3957041270959,12.4223470642232));
#64671=CARTESIAN_POINT('Ctrl Pts',(1.87484008529833,74.4051362532598,12.4914060337626));
#64672=CARTESIAN_POINT('Ctrl Pts',(1.90150357679853,74.4145597466018,12.5620571447373));
#64673=CARTESIAN_POINT('Ctrl Pts',(1.92422782173927,74.4239450681702,12.6338132953026));
#64674=CARTESIAN_POINT('Ctrl Pts',(1.92908398492622,74.4259507081031,12.649147559553));
#64675=CARTESIAN_POINT('Ctrl Pts',(1.93376035428528,74.427954627965,12.6645324463498));
#64676=CARTESIAN_POINT('Ctrl Pts',(1.93825613759087,74.4299565772684,12.6799634688133));
#64677=CARTESIAN_POINT('Ctrl Pts',(1.9393309096904,74.4304351677853,12.6836524438559));
#64678=CARTESIAN_POINT('Ctrl Pts',(1.9403954060336,74.4309136531687,12.6873441413251));
#64679=CARTESIAN_POINT('Ctrl Pts',(1.94144959634439,74.4313920380659,12.6910385265463));
#64680=CARTESIAN_POINT('Ctrl Pts',(1.94753699656449,74.4341544617941,12.7123716778554));
#64681=CARTESIAN_POINT('Ctrl Pts',(1.95328078631335,74.4369135371217,12.7337944611126));
#64682=CARTESIAN_POINT('Ctrl Pts',(1.95868003122727,74.4396701426473,12.7552996071111));
#64683=CARTESIAN_POINT('Ctrl Pts',(1.97787033392747,74.4494678264541,12.8317344175158));
#64684=CARTESIAN_POINT('Ctrl Pts',(1.9927007065785,74.45923013598,12.9091803746465));
#64685=CARTESIAN_POINT('Ctrl Pts',(2.00305822928529,74.4689777601459,12.9871152481655));
#64686=CARTESIAN_POINT('Ctrl Pts',(2.01052114765116,74.4760012275784,13.0432697568634));
#64687=CARTESIAN_POINT('Ctrl Pts',(2.01566185350558,74.4830169451425,13.0996769724923));
#64688=CARTESIAN_POINT('Ctrl Pts',(2.01844171971378,74.4900306880044,13.1561252536584));
#64689=CARTESIAN_POINT('Ctrl Pts',(2.0223428691589,74.4998734851121,13.2353424404779));
#64690=CARTESIAN_POINT('Ctrl Pts',(2.02159300613646,74.5097140822882,13.3146491714498));
#64691=CARTESIAN_POINT('Ctrl Pts',(2.01608782135885,74.5195725971845,13.3934914521823));
#64692=CARTESIAN_POINT('Ctrl Pts',(2.01518934110372,74.5211815678798,13.4063590007513));
#64693=CARTESIAN_POINT('Ctrl Pts',(2.01416419210897,74.5227910014299,13.4192140663617));
#64694=CARTESIAN_POINT('Ctrl Pts',(2.01301192188643,74.5244009684201,13.4320541093707));
#64695=CARTESIAN_POINT('Ctrl Pts',(2.00708142438712,74.5326871369099,13.4981391660412));
#64696=CARTESIAN_POINT('Ctrl Pts',(1.99778796228407,74.5409879174046,13.5638386790392));
#64697=CARTESIAN_POINT('Ctrl Pts',(1.9852685667007,74.5492782813175,13.6288398715573));
#64698=CARTESIAN_POINT('Ctrl Pts',(1.98094021513431,74.5521445226938,13.6513128425229));
#64699=CARTESIAN_POINT('Ctrl Pts',(1.97622622120035,74.5550095766191,13.6737027951074));
#64700=CARTESIAN_POINT('Ctrl Pts',(1.9711320027107,74.5578725918486,13.6959982219969));
#64701=CARTESIAN_POINT('Ctrl Pts',(1.96718807432242,74.5600891294907,13.7132592733665));
#64702=CARTESIAN_POINT('Ctrl Pts',(1.9630162436556,74.5623044470594,13.7304636824044));
#64703=CARTESIAN_POINT('Ctrl Pts',(1.95862195803157,74.5645181885269,13.747607152374));
#64704=CARTESIAN_POINT('Ctrl Pts',(1.93049173004795,74.5786895596001,13.857351889047));
#64705=CARTESIAN_POINT('Ctrl Pts',(1.89317217966602,74.5928057813007,13.9645512450797));
#64706=CARTESIAN_POINT('Ctrl Pts',(1.8473907998134,74.6068822020894,14.0677907233878));
#64707=CARTESIAN_POINT('Ctrl Pts',(1.83888623714562,74.6094971036743,14.0869689704369));
#64708=CARTESIAN_POINT('Ctrl Pts',(1.83008973864687,74.6121106136852,14.1060104417081));
#64709=CARTESIAN_POINT('Ctrl Pts',(1.82100607332705,74.6147228056702,14.1249059048358));
#64710=CARTESIAN_POINT('Ctrl Pts',(1.77579474554523,74.6277242388917,14.218952630136));
#64711=CARTESIAN_POINT('Ctrl Pts',(1.72346712437599,74.6406937697442,14.3093851165373));
#64712=CARTESIAN_POINT('Ctrl Pts',(1.66457756792296,74.6536459079467,14.3950771829617));
#64713=CARTESIAN_POINT('Ctrl Pts',(1.64931634734291,74.6570024528079,14.4172842703712));
#64714=CARTESIAN_POINT('Ctrl Pts',(1.63361449454355,74.6603577968262,14.4391727328735));
#64715=CARTESIAN_POINT('Ctrl Pts',(1.61748182560175,74.6637121236636,14.4607224276072));
#64716=CARTESIAN_POINT('Ctrl Pts',(1.58627959143489,74.6701997353432,14.5024017445093));
#64717=CARTESIAN_POINT('Ctrl Pts',(1.55346490905361,74.6766837372837,14.5428150216422));
#64718=CARTESIAN_POINT('Ctrl Pts',(1.51910631662569,74.683165766496,14.5818178250006));
#64719=CARTESIAN_POINT('Ctrl Pts',(1.519028822493,74.6831803863973,14.581905793925));
#64720=CARTESIAN_POINT('Ctrl Pts',(1.51895132050671,74.6831950062885,14.5819937556725));
#64721=CARTESIAN_POINT('Ctrl Pts',(1.51887381066809,74.6832096261694,14.5820817102422));
#64722=CARTESIAN_POINT('Ctrl Pts',(1.50558108259855,74.6857168962855,14.5971656814981));
#64723=CARTESIAN_POINT('Ctrl Pts',(1.4920601355563,74.6882233561188,14.6120355654605));
#64724=CARTESIAN_POINT('Ctrl Pts',(1.47831532366195,74.6907294675882,14.6266831059059));
#64725=CARTESIAN_POINT('Ctrl Pts',(1.41866624898481,74.7016053698074,14.6902497986028));
#64726=CARTESIAN_POINT('Ctrl Pts',(1.35479218909004,74.7124763142226,14.7496347287381));
#64727=CARTESIAN_POINT('Ctrl Pts',(1.28740183232951,74.7233337414734,14.8045175217916));
#64728=CARTESIAN_POINT('Ctrl Pts',(1.22693477957409,74.7330757380724,14.8537619671761));
#64729=CARTESIAN_POINT('Ctrl Pts',(1.16363647191518,74.7428069340349,14.8993827722767));
#64730=CARTESIAN_POINT('Ctrl Pts',(1.09798669092278,74.7525254754109,14.9411636149424));
#64731=CARTESIAN_POINT('Ctrl Pts',(1.02420938336678,74.7634471845964,14.9881169791836));
#64732=CARTESIAN_POINT('Ctrl Pts',(0.947467312276564,74.7743520707771,15.0302211078564));
#64733=CARTESIAN_POINT('Ctrl Pts',(0.868473044750292,74.7852330922427,15.067141180662));
#64734=CARTESIAN_POINT('Ctrl Pts',(0.815124851004688,74.7925815095327,15.0920748784961));
#64735=CARTESIAN_POINT('Ctrl Pts',(0.760748902071486,74.7999191685314,15.1146451328699));
#64736=CARTESIAN_POINT('Ctrl Pts',(0.705554870479162,74.8072454720367,15.1347579546826));
#64737=CARTESIAN_POINT('Ctrl Pts',(0.705512057820929,74.8072511548709,15.1347735557058));
#64738=CARTESIAN_POINT('Ctrl Pts',(0.705469244669996,74.8072568376982,15.1347891552507));
#64739=CARTESIAN_POINT('Ctrl Pts',(0.705426431026517,74.8072625205189,15.1348047533174));
#64740=CARTESIAN_POINT('Ctrl Pts',(0.645100516539383,74.8152698126569,15.156782972391));
#64741=CARTESIAN_POINT('Ctrl Pts',(0.583741977736648,74.8232708914926,15.1758472221042));
#64742=CARTESIAN_POINT('Ctrl Pts',(0.521641228908294,74.8312665354659,15.1918447534929));
#64743=CARTESIAN_POINT('Ctrl Pts',(0.488248291436797,74.8355659689555,15.2004469777082));
#64744=CARTESIAN_POINT('Ctrl Pts',(0.45464163788152,74.8398637245999,15.2081623978426));
#64745=CARTESIAN_POINT('Ctrl Pts',(0.420872611953215,74.8441591806084,15.2149674285766));
#64746=CARTESIAN_POINT('Ctrl Pts',(0.393277639352099,74.8476692904681,15.2205282829836));
#64747=CARTESIAN_POINT('Ctrl Pts',(0.365572672690947,74.8511780646081,15.2254814472713));
#64748=CARTESIAN_POINT('Ctrl Pts',(0.337783856362672,74.8546854022102,15.2298146768192));
#64749=CARTESIAN_POINT('Ctrl Pts',(0.265257556785499,74.8638392364234,15.2411240143821));
#64750=CARTESIAN_POINT('Ctrl Pts',(0.192156085109537,74.8729837677774,15.2482080863385));
#64751=CARTESIAN_POINT('Ctrl Pts',(0.118967764499052,74.8821167241471,15.2511597356922));
#64752=CARTESIAN_POINT('Ctrl Pts',(0.0915763247955409,74.8855348217565,
15.2522644191256));
#64753=CARTESIAN_POINT('Ctrl Pts',(0.0641721975875338,74.8889513631873,
15.2527902925941));
#64754=CARTESIAN_POINT('Ctrl Pts',(0.0367791242492394,74.892366462911,15.252742140314));
#64755=CARTESIAN_POINT('Ctrl Pts',(-0.0333491909333243,74.901109373458,
15.2526188668781));
#64756=CARTESIAN_POINT('Ctrl Pts',(-0.103401965497628,74.9098424726392,
15.2487346624949));
#64757=CARTESIAN_POINT('Ctrl Pts',(-0.172949517403085,74.9185639227761,
15.2411882329299));
#64758=CARTESIAN_POINT('Ctrl Pts',(-0.203152651108026,74.9223514770087,
15.2379109670176));
#64759=CARTESIAN_POINT('Ctrl Pts',(-0.233261142036416,74.9261369134886,
15.2339431705582));
#64760=CARTESIAN_POINT('Ctrl Pts',(-0.263242806676454,74.9299204465575,
15.2292933908425));
#64761=CARTESIAN_POINT('Ctrl Pts',(-0.26324487004777,74.9299207069445,15.2292930708395));
#64762=CARTESIAN_POINT('Ctrl Pts',(-0.263246933418519,74.9299209673314,
15.2292927508333));
#64763=CARTESIAN_POINT('Ctrl Pts',(-0.263248996788635,74.9299212277183,
15.2292924308239));
#64764=CARTESIAN_POINT('Ctrl Pts',(-0.343335449250516,74.9400277344896,
15.216871769703));
#64765=CARTESIAN_POINT('Ctrl Pts',(-0.422566406385879,74.9501267421625,
15.1995584594227));
#64766=CARTESIAN_POINT('Ctrl Pts',(-0.500372848947576,74.9602178008868,
15.1774906759502));
#64767=CARTESIAN_POINT('Ctrl Pts',(-0.533467373120428,74.9645099748493,
15.168104270795));
#64768=CARTESIAN_POINT('Ctrl Pts',(-0.566303544687431,74.968800630062,15.1578578177866));
#64769=CARTESIAN_POINT('Ctrl Pts',(-0.598834860827465,74.9730893735596,
15.1467627706444));
#64770=CARTESIAN_POINT('Ctrl Pts',(-0.643694027475191,74.9790033506775,
15.1314632184661));
#64771=CARTESIAN_POINT('Ctrl Pts',(-0.68797634563979,74.9849140526127,15.1145487039482));
#64772=CARTESIAN_POINT('Ctrl Pts',(-0.731565348541546,74.9908212280144,
15.0960452135253));
#64773=CARTESIAN_POINT('Ctrl Pts',(-0.731573386736688,74.9908223173495,
15.0960418013191));
#64774=CARTESIAN_POINT('Ctrl Pts',(-0.731581424908254,74.9908234066844,
15.0960383890588));
#64775=CARTESIAN_POINT('Ctrl Pts',(-0.731589463056202,74.9908244960192,
15.0960349767445));
#64776=CARTESIAN_POINT('Ctrl Pts',(-0.79445314485466,74.9993438212396,15.0693484015454));
#64777=CARTESIAN_POINT('Ctrl Pts',(-0.855855254470442,75.0078532350169,
15.0393737720039));
#64778=CARTESIAN_POINT('Ctrl Pts',(-0.915407830563247,75.0163465056109,
15.0062009476611));
#64779=CARTESIAN_POINT('Ctrl Pts',(-0.971425808638196,75.0243356788278,
14.9749970154614));
#64780=CARTESIAN_POINT('Ctrl Pts',(-1.02581131808626,75.0323112182964,14.9409608397735));
#64781=CARTESIAN_POINT('Ctrl Pts',(-1.07831624700676,75.0402791188551,14.9043633413764));
#64782=CARTESIAN_POINT('Ctrl Pts',(-1.1027578997126,75.0439882688769,14.8873267818741));
#64783=CARTESIAN_POINT('Ctrl Pts',(-1.12679272620587,75.047695853712,14.8697349449566));
#64784=CARTESIAN_POINT('Ctrl Pts',(-1.15039918302486,75.0514029488734,14.8516135820113));
#64785=CARTESIAN_POINT('Ctrl Pts',(-1.15042313215987,75.0514067097818,14.8515951975934));
#64786=CARTESIAN_POINT('Ctrl Pts',(-1.15044708086044,75.0514104706908,14.8515768126246));
#64787=CARTESIAN_POINT('Ctrl Pts',(-1.15047102912656,75.0514142316002,14.8515584271049));
#64788=CARTESIAN_POINT('Ctrl Pts',(-1.23163381332312,75.0641602851648,14.7892482807145));
#64789=CARTESIAN_POINT('Ctrl Pts',(-1.30780791253006,75.0769127374865,14.7206058432401));
#64790=CARTESIAN_POINT('Ctrl Pts',(-1.37817228584358,75.089663154856,14.646599244424));
#64791=CARTESIAN_POINT('Ctrl Pts',(-1.43987402621517,75.100843854763,14.5817036768106));
#64792=CARTESIAN_POINT('Ctrl Pts',(-1.49710857111955,75.1120228402846,14.5126836757894));
#64793=CARTESIAN_POINT('Ctrl Pts',(-1.54930332365839,75.1231904560488,14.4401619423412));
#64794=CARTESIAN_POINT('Ctrl Pts',(-1.55608174661695,75.1246407708679,14.430743697037));
#64795=CARTESIAN_POINT('Ctrl Pts',(-1.56277512510347,75.1260908846029,14.4212664482243));
#64796=CARTESIAN_POINT('Ctrl Pts',(-1.56938216741063,75.1275407677611,14.4117316114416));
#64797=CARTESIAN_POINT('Ctrl Pts',(-1.61630638655644,75.1378380584229,14.3440137507241));
#64798=CARTESIAN_POINT('Ctrl Pts',(-1.65887797582533,75.1481240462068,14.2733878730649));
#64799=CARTESIAN_POINT('Ctrl Pts',(-1.69662379552537,75.1583882525853,14.2003271148885));
#64800=CARTESIAN_POINT('Ctrl Pts',(-1.70283559236494,75.1600774241347,14.1883035692259));
#64801=CARTESIAN_POINT('Ctrl Pts',(-1.70891660919459,75.1617659922579,14.1762141568186));
#64802=CARTESIAN_POINT('Ctrl Pts',(-1.71486464298032,75.1634538942864,14.1640610826852));
#64803=CARTESIAN_POINT('Ctrl Pts',(-1.72499159849874,75.166327668945,14.1433695994836));
#64804=CARTESIAN_POINT('Ctrl Pts',(-1.73473317330876,75.1691995488222,14.1224931836789));
#64805=CARTESIAN_POINT('Ctrl Pts',(-1.74407844997948,75.1720692639313,14.1014421786624));
#64806=CARTESIAN_POINT('Ctrl Pts',(-1.74408173925696,75.1720702739912,14.1014347692941));
#64807=CARTESIAN_POINT('Ctrl Pts',(-1.74408502848537,75.1720712840509,14.1014273599041));
#64808=CARTESIAN_POINT('Ctrl Pts',(-1.74408831766465,75.1720722941103,14.1014199504926));
#64809=CARTESIAN_POINT('Ctrl Pts',(-1.74912296447396,75.1736183613032,14.0900785893136));
#64810=CARTESIAN_POINT('Ctrl Pts',(-1.75404253371793,75.1751637110891,14.0786881199489));
#64811=CARTESIAN_POINT('Ctrl Pts',(-1.7588451242202,75.1767080631392,14.067250592328));
#64812=CARTESIAN_POINT('Ctrl Pts',(-1.79041612375115,75.1868602378511,13.99206321606));
#64813=CARTESIAN_POINT('Ctrl Pts',(-1.81692814272135,75.1969686342519,13.9148403841097));
#64814=CARTESIAN_POINT('Ctrl Pts',(-1.83838148126977,75.2070493575475,13.8363131439182));
#64815=CARTESIAN_POINT('Ctrl Pts',(-1.85206261976672,75.2134779966726,13.7862350618324));
#64816=CARTESIAN_POINT('Ctrl Pts',(-1.86390894119643,75.2199323255159,13.7357262251899));
#64817=CARTESIAN_POINT('Ctrl Pts',(-1.87375377347736,75.2263904479145,13.6848691987371));
#64818=CARTESIAN_POINT('Ctrl Pts',(-1.87651059499211,75.2281988983041,13.6706278444204));
#64819=CARTESIAN_POINT('Ctrl Pts',(-1.87911033479588,75.230007607253,13.6563594683737));
#64820=CARTESIAN_POINT('Ctrl Pts',(-1.88154905044117,75.2318160032327,13.642066552674));
#64821=CARTESIAN_POINT('Ctrl Pts',(-1.88156664190423,75.2318290479397,13.6419634519705));
#64822=CARTESIAN_POINT('Ctrl Pts',(-1.88158422499357,75.2318420926342,13.6418603499602));
#64823=CARTESIAN_POINT('Ctrl Pts',(-1.88160179970896,75.2318551373163,13.6417572466445));
#64824=CARTESIAN_POINT('Ctrl Pts',(-1.89503969316487,75.2418292986761,13.562922890464));
#64825=CARTESIAN_POINT('Ctrl Pts',(-1.90358372662692,75.2517961590833,13.4833253137894));
#64826=CARTESIAN_POINT('Ctrl Pts',(-1.90696701947769,75.2617621701583,13.4035272721076));
#64827=CARTESIAN_POINT('Ctrl Pts',(-1.90865777948337,75.2667425646099,13.3636491582821));
#64828=CARTESIAN_POINT('Ctrl Pts',(-1.90905877377697,75.2717227893684,13.3237206427298));
#64829=CARTESIAN_POINT('Ctrl Pts',(-1.90834857578517,75.2767000324125,13.2838187135308));
#64830=CARTESIAN_POINT('Ctrl Pts',(-1.90764161704859,75.2816545739556,13.2440987794006));
#64831=CARTESIAN_POINT('Ctrl Pts',(-1.90583467804834,75.2866060300103,13.2044062106991));
#64832=CARTESIAN_POINT('Ctrl Pts',(-1.90268039003633,75.2915583348428,13.1648413210216));
#64833=CARTESIAN_POINT('Ctrl Pts',(-1.90266563946863,75.2915814935738,13.1646563015873));
#64834=CARTESIAN_POINT('Ctrl Pts',(-1.90265085931897,75.2916046524839,13.1644712836647));
#64835=CARTESIAN_POINT('Ctrl Pts',(-1.9026360495646,75.2916278115732,13.1642862672715));
#64836=CARTESIAN_POINT('Ctrl Pts',(-1.8981808083416,75.2985947960977,13.1086275006487));
#64837=CARTESIAN_POINT('Ctrl Pts',(-1.89104293007554,75.3055776417841,13.0531101156009));
#64838=CARTESIAN_POINT('Ctrl Pts',(-1.8814359156998,75.3125852593552,12.9980115027018));
#64839=CARTESIAN_POINT('Ctrl Pts',(-1.87338588903486,75.318457167744,12.9518426009295));
#64840=CARTESIAN_POINT('Ctrl Pts',(-1.8636032509819,75.3243465465202,12.9059672560355));
#64841=CARTESIAN_POINT('Ctrl Pts',(-1.85223213673048,75.3302609830586,12.8605276268862));
#64842=CARTESIAN_POINT('Ctrl Pts',(-1.83959362228345,75.336834630107,12.810023393372));
#64843=CARTESIAN_POINT('Ctrl Pts',(-1.82513037668464,75.3434690387466,12.7600435140782));
#64844=CARTESIAN_POINT('Ctrl Pts',(-1.80875091426492,75.3501234806354,12.7107244307332));
#64845=CARTESIAN_POINT('Ctrl Pts',(-1.79237145184519,75.3567779225242,12.6614053473882));
#64846=CARTESIAN_POINT('Ctrl Pts',(-1.77407495138808,75.3634523924017,12.6127472908621));
#64847=CARTESIAN_POINT('Ctrl Pts',(-1.75378330692145,75.3700981471543,12.564947614224));
#64848=CARTESIAN_POINT('Ctrl Pts',(-1.73423929954464,75.3764990418734,12.5189090965297));
#64849=CARTESIAN_POINT('Ctrl Pts',(-1.71284271627196,75.3828739576428,12.4736621112999));
#64850=CARTESIAN_POINT('Ctrl Pts',(-1.68961024576259,75.3892021479551,12.4293618498602));
#64851=CARTESIAN_POINT('Ctrl Pts',(-1.65465228155192,75.3987241938506,12.3627031209357));
#64852=CARTESIAN_POINT('Ctrl Pts',(-1.61553399868203,75.4081406901443,12.2981852149581));
#64853=CARTESIAN_POINT('Ctrl Pts',(-1.57268896769164,75.4174769600211,12.2362421749446));
#64854=CARTESIAN_POINT('Ctrl Pts',(-1.55687507894415,75.4209229309945,12.2133793056501));
#64855=CARTESIAN_POINT('Ctrl Pts',(-1.54055321361141,75.4243580404324,12.1908667787775));
#64856=CARTESIAN_POINT('Ctrl Pts',(-1.52374410223504,75.4277837981028,12.1687250189737));
#64857=CARTESIAN_POINT('Ctrl Pts',(-1.47900264321441,75.4369022692104,12.1097894442891));
#64858=CARTESIAN_POINT('Ctrl Pts',(-1.43081223803484,75.445954538049,12.0534836353524));
#64859=CARTESIAN_POINT('Ctrl Pts',(-1.37959434194762,75.4549673385587,12.0002103269436));
#64860=CARTESIAN_POINT('Ctrl Pts',(-1.36112325376369,75.458217691379,11.980997980232));
#64861=CARTESIAN_POINT('Ctrl Pts',(-1.3422582300322,75.4614629743166,11.9621795815972));
#64862=CARTESIAN_POINT('Ctrl Pts',(-1.32301830800744,75.4647046552193,11.9437725482982));
#64863=CARTESIAN_POINT('Ctrl Pts',(-1.27098277329551,75.4734719776088,11.8939896116033));
#64864=CARTESIAN_POINT('Ctrl Pts',(-1.21620842607349,75.4822123776369,11.8472210800521));
#64865=CARTESIAN_POINT('Ctrl Pts',(-1.15909057545261,75.490949156467,11.8038212767092));
#64866=CARTESIAN_POINT('Ctrl Pts',(-1.15473759094654,75.4916149914462,11.8005137525383));
#64867=CARTESIAN_POINT('Ctrl Pts',(-1.15037098756579,75.4922808080305,11.7972257703682));
#64868=CARTESIAN_POINT('Ctrl Pts',(-1.14599093612188,75.4929466178375,11.7939574754032));
#64869=CARTESIAN_POINT('Ctrl Pts',(-1.09923734883009,75.500053611289,11.7590710098211));
#64870=CARTESIAN_POINT('Ctrl Pts',(-1.05097004323201,75.5071704646145,11.7264028158223));
#64871=CARTESIAN_POINT('Ctrl Pts',(-1.00143818770449,75.5143409295118,11.696049786287));
#64872=CARTESIAN_POINT('Ctrl Pts',(-0.9672702277746,75.5192872444575,11.6751117235824));
#64873=CARTESIAN_POINT('Ctrl Pts',(-0.932499888278065,75.524259199438,11.6552744312169));
#64874=CARTESIAN_POINT('Ctrl Pts',(-0.897198351310015,75.5292728555587,
11.6365600239425));
#64875=CARTESIAN_POINT('Ctrl Pts',(-0.897135623778236,75.529281764357,11.6365267701899));
#64876=CARTESIAN_POINT('Ctrl Pts',(-0.897072894089373,75.5292906732001,
11.6364935201442));
#64877=CARTESIAN_POINT('Ctrl Pts',(-0.897010162243998,75.5292995820881,
11.6364602738058));
#64878=CARTESIAN_POINT('Ctrl Pts',(-0.848793065296281,75.5361471522735,
11.6109063957864));
#64879=CARTESIAN_POINT('Ctrl Pts',(-0.799303600639264,75.543020762987,11.5875467945996));
#64880=CARTESIAN_POINT('Ctrl Pts',(-0.748872763198369,75.5499555577861,
11.5663189927731));
#64881=CARTESIAN_POINT('Ctrl Pts',(-0.714420144622406,75.5546931717589,
11.5518168865887));
#64882=CARTESIAN_POINT('Ctrl Pts',(-0.679527838667414,75.559459454955,11.5383086274129));
#64883=CARTESIAN_POINT('Ctrl Pts',(-0.644294595743942,75.5642670645859,
11.5257621898246));
#64884=CARTESIAN_POINT('Ctrl Pts',(-0.583888688816627,75.5725095082502,
11.5042518524744));
#64885=CARTESIAN_POINT('Ctrl Pts',(-0.522372346675663,75.5808060797152,
11.4857360608543));
#64886=CARTESIAN_POINT('Ctrl Pts',(-0.460057431799019,75.589105955884,11.4703277296083));
#64887=CARTESIAN_POINT('Ctrl Pts',(-0.430652191081433,75.5930225119308,
11.4630568268037));
#64888=CARTESIAN_POINT('Ctrl Pts',(-0.401069881618514,75.5969397081773,
11.4564779380468));
#64889=CARTESIAN_POINT('Ctrl Pts',(-0.371347266997866,75.6008516946164,
11.4506029146664));
#64890=CARTESIAN_POINT('Ctrl Pts',(-0.305962402846651,75.6094574214392,
11.4376788294027));
#64891=CARTESIAN_POINT('Ctrl Pts',(-0.239894421453448,75.6180374864646,
11.4281615585366));
#64892=CARTESIAN_POINT('Ctrl Pts',(-0.173491447715413,75.6265396084448,
11.4221589217094));
#64893=CARTESIAN_POINT('Ctrl Pts',(-0.144978066637523,75.6301904124728,
11.419581394504));
#64894=CARTESIAN_POINT('Ctrl Pts',(-0.116403531130909,75.6338267590699,
11.4176521294849));
#64895=CARTESIAN_POINT('Ctrl Pts',(-0.0877982390560473,75.6374441231734,
11.4163803841385));
#64896=CARTESIAN_POINT('Ctrl Pts',(-0.0489006230125617,75.6423630325703,
11.4146510585975));
#64897=CARTESIAN_POINT('Ctrl Pts',(-0.00994327625232608,75.6472475382857,
11.414136431099));
#64898=CARTESIAN_POINT('Ctrl Pts',(0.0290034066344337,75.6520888411402,
11.4148571492207));
#64899=CARTESIAN_POINT('Ctrl Pts',(0.0966315685909427,75.6604954213481,
11.4161086252966));
#64900=CARTESIAN_POINT('Ctrl Pts',(0.16423318315411,75.6687716473232,11.4210869881037));
#64901=CARTESIAN_POINT('Ctrl Pts',(0.231391873384125,75.6769704240339,11.429666307699));
#64902=CARTESIAN_POINT('Ctrl Pts',(0.258994454213436,75.6803401651066,11.4331924539324));
#64903=CARTESIAN_POINT('Ctrl Pts',(0.286522821661356,75.6836969046949,11.4373269787138));
#64904=CARTESIAN_POINT('Ctrl Pts',(0.313950515650403,75.6870446558327,11.4420617230722));
#64905=CARTESIAN_POINT('Ctrl Pts',(0.379256533066087,75.69501573405,11.453335266435));
#64906=CARTESIAN_POINT('Ctrl Pts',(0.44398850254222,75.7029363581561,11.4680103200387));
#64907=CARTESIAN_POINT('Ctrl Pts',(0.507747595471506,75.710858621323,11.4859568730678));
#64908=CARTESIAN_POINT('Ctrl Pts',(0.53513379017223,75.714261440146,11.4936653860482));
#64909=CARTESIAN_POINT('Ctrl Pts',(0.562341145438018,75.7176646451403,11.5019773913128));
#64910=CARTESIAN_POINT('Ctrl Pts',(0.589340981957953,75.721072741656,11.5108825196477));
#64911=CARTESIAN_POINT('Ctrl Pts',(0.65865362053499,75.7298218376683,11.5337433225751));
#64912=CARTESIAN_POINT('Ctrl Pts',(0.726614803478868,75.7386900862247,11.5603150939239));
#64913=CARTESIAN_POINT('Ctrl Pts',(0.792731839442396,75.7477073109522,11.5904922109949));
#64914=CARTESIAN_POINT('Ctrl Pts',(0.809092813106204,75.7499386659145,11.5979596815258));
#64915=CARTESIAN_POINT('Ctrl Pts',(0.825341087495351,75.7521791616775,11.6056478154616));
#64916=CARTESIAN_POINT('Ctrl Pts',(0.841469654748839,75.7544292860038,11.6135548221577));
#64917=CARTESIAN_POINT('Ctrl Pts',(0.859238357464154,75.7569082284666,11.6222659028844));
#64918=CARTESIAN_POINT('Ctrl Pts',(0.87685468981896,75.7593864049395,11.6312687689277));
#64919=CARTESIAN_POINT('Ctrl Pts',(0.894305628425393,75.7618633458217,11.6405607880959));
#64920=CARTESIAN_POINT('Ctrl Pts',(0.903139747007031,75.7631172376591,11.6452646496501));
#64921=CARTESIAN_POINT('Ctrl Pts',(0.911931388265836,75.7643707989428,11.6500425499173));
#64922=CARTESIAN_POINT('Ctrl Pts',(0.920679184464007,75.765624010736,11.6548942660476));
#64923=CARTESIAN_POINT('Ctrl Pts',(0.976183407168826,75.7735755616055,11.6856781030844));
#64924=CARTESIAN_POINT('Ctrl Pts',(1.03009096683839,75.7815373641079,11.719530489887));
#64925=CARTESIAN_POINT('Ctrl Pts',(1.08211815751369,75.7894993738068,11.7561513401554));
#64926=CARTESIAN_POINT('Ctrl Pts',(1.11865528182004,75.7950908526916,11.7818690570088));
#64927=CARTESIAN_POINT('Ctrl Pts',(1.15426350246226,75.8006821379589,11.8089498719097));
#64928=CARTESIAN_POINT('Ctrl Pts',(1.18885608630365,75.8062707195369,11.8372861931718));
#64929=CARTESIAN_POINT('Ctrl Pts',(1.26095224823748,75.817918166408,11.8963433603292));
#64930=CARTESIAN_POINT('Ctrl Pts',(1.32866192715258,75.8295574124541,11.9608676517253));
#64931=CARTESIAN_POINT('Ctrl Pts',(1.39143020206034,75.8412258672627,12.0300131362008));
#64932=CARTESIAN_POINT('Ctrl Pts',(1.39819263057232,75.8424829846776,12.0374626223684));
#64933=CARTESIAN_POINT('Ctrl Pts',(1.4048977027914,75.8437404447991,12.0449657969394));
#64934=CARTESIAN_POINT('Ctrl Pts',(1.41154472262835,75.8449982970642,12.0525216376492));
#64935=CARTESIAN_POINT('Ctrl Pts',(1.47519562629064,75.8570433090111,12.1248752789662));
#64936=CARTESIAN_POINT('Ctrl Pts',(1.53345912753552,75.869068147836,12.2021451994932));
#64937=CARTESIAN_POINT('Ctrl Pts',(1.58568533590138,75.8811243127768,12.2833577550705));
#64938=CARTESIAN_POINT('Ctrl Pts',(1.58953613559223,75.8820132510643,12.2893458076919));
#64939=CARTESIAN_POINT('Ctrl Pts',(1.5933541260633,75.8829023627213,12.2953553140732));
#64940=CARTESIAN_POINT('Ctrl Pts',(1.59713905249284,75.8837916698498,12.3013858934346));
#64941=CARTESIAN_POINT('Ctrl Pts',(1.59716100967478,75.883796828914,12.3014208781379));
#64942=CARTESIAN_POINT('Ctrl Pts',(1.59718296574323,75.8838019879847,12.3014558635489));
#64943=CARTESIAN_POINT('Ctrl Pts',(1.59720492069803,75.8838071470618,12.3014908496674));
#64944=CARTESIAN_POINT('Ctrl Pts',(1.64421070095242,75.8948527833314,12.3763964830218));
#64945=CARTESIAN_POINT('Ctrl Pts',(1.68611306586749,75.9059285477027,12.454549496737));
#64946=CARTESIAN_POINT('Ctrl Pts',(1.7224412023541,75.9169784004475,12.5351730844704));
#64947=CARTESIAN_POINT('Ctrl Pts',(1.7258457009239,75.9180139396054,12.5427287401047));
#64948=CARTESIAN_POINT('Ctrl Pts',(1.72920123537447,75.9190492465905,12.5503060570557));
#64949=CARTESIAN_POINT('Ctrl Pts',(1.73250741417377,75.9200842724326,12.557904373156));
#64950=CARTESIAN_POINT('Ctrl Pts',(1.77029251842462,75.9319132029662,12.6447427395626));
#64951=CARTESIAN_POINT('Ctrl Pts',(1.80163260646769,75.9437053249773,12.7343288544185));
#64952=CARTESIAN_POINT('Ctrl Pts',(1.82597858705125,75.9554081493042,12.8256992037765));
#64953=CARTESIAN_POINT('Ctrl Pts',(1.83126185966317,75.9579477558333,12.8455273007656));
#64954=CARTESIAN_POINT('Ctrl Pts',(1.83621586635653,75.9604832474547,12.8654394204659));
#64955=CARTESIAN_POINT('Ctrl Pts',(1.84083516476731,75.9630142551579,12.8854257223643));
#64956=CARTESIAN_POINT('Ctrl Pts',(1.86238082771495,75.9748195628131,12.9786472651136));
#64957=CARTESIAN_POINT('Ctrl Pts',(1.87693370588993,75.9867185332742,13.0733722423359));
#64958=CARTESIAN_POINT('Ctrl Pts',(1.88394226763736,75.9986685723865,13.168608630988));
#64959=CARTESIAN_POINT('Ctrl Pts',(1.88455932889628,75.9997207006896,13.1769936160954));
#64960=CARTESIAN_POINT('Ctrl Pts',(1.88511733747509,76.0007728324774,13.1853824812178));
#64961=CARTESIAN_POINT('Ctrl Pts',(1.88561596325121,76.0018249466931,13.1937743533224));
#64962=CARTESIAN_POINT('Ctrl Pts',(1.88562071927659,76.0018349820386,13.1938543972323));
#64963=CARTESIAN_POINT('Ctrl Pts',(1.88562546992771,76.0018450174184,13.1939344416131));
#64964=CARTESIAN_POINT('Ctrl Pts',(1.88563021520441,76.0018550528325,13.1940144864636));
#64965=CARTESIAN_POINT('Ctrl Pts',(1.88934921213212,76.0097200682497,13.2567477203733));
#64966=CARTESIAN_POINT('Ctrl Pts',(1.88976376963936,76.01760579953,13.3197665736573));
#64967=CARTESIAN_POINT('Ctrl Pts',(1.88707397236113,76.0255711291619,13.3826907579127));
#64968=CARTESIAN_POINT('Ctrl Pts',(1.88495763313559,76.0318382704371,13.4321996634546));
#64969=CARTESIAN_POINT('Ctrl Pts',(1.88092054514117,76.0381547895768,13.481650542398));
#64970=CARTESIAN_POINT('Ctrl Pts',(1.87507453210503,76.0445515341352,13.5308755365519));
#64971=CARTESIAN_POINT('Ctrl Pts',(1.86621950738515,76.0542407583709,13.6054372142926));
#64972=CARTESIAN_POINT('Ctrl Pts',(1.8530094099864,76.0639800127981,13.679516890321));
#64973=CARTESIAN_POINT('Ctrl Pts',(1.83553504488097,76.0736838726472,13.7526145805329));
#64974=CARTESIAN_POINT('Ctrl Pts',(1.8264729764718,76.0787162181003,13.7905224681876));
#64975=CARTESIAN_POINT('Ctrl Pts',(1.81626422543518,76.0837389263354,13.8281654089272));
#64976=CARTESIAN_POINT('Ctrl Pts',(1.80492310978648,76.0887393302903,13.8654684660956));
#64977=CARTESIAN_POINT('Ctrl Pts',(1.78342243897396,76.0982191771322,13.9361882063155));
#64978=CARTESIAN_POINT('Ctrl Pts',(1.75785031253306,76.1076189232886,14.0056947908024));
#64979=CARTESIAN_POINT('Ctrl Pts',(1.72828352214613,76.1168660130861,14.0735310977614));
#64980=CARTESIAN_POINT('Ctrl Pts',(1.72219223376294,76.1187710792067,14.0875065919943));
#64981=CARTESIAN_POINT('Ctrl Pts',(1.7159313692519,76.120669646444,14.1014110208233));
#64982=CARTESIAN_POINT('Ctrl Pts',(1.70950156945226,76.1225610499344,14.1152401152146));
#64983=CARTESIAN_POINT('Ctrl Pts',(1.67857438950661,76.1316586545134,14.1817577213696));
#64984=CARTESIAN_POINT('Ctrl Pts',(1.64373119636544,76.1405928160376,14.2465505915588));
#64985=CARTESIAN_POINT('Ctrl Pts',(1.60524457886279,76.1494565148589,14.3092026896844));
#64986=CARTESIAN_POINT('Ctrl Pts',(1.58471620064246,76.1541843234751,14.3426206944371));
#64987=CARTESIAN_POINT('Ctrl Pts',(1.56315070554684,76.1588922065802,14.3754303553122));
#64988=CARTESIAN_POINT('Ctrl Pts',(1.54058507095701,76.1635950968011,14.4075726254229));
#64989=CARTESIAN_POINT('Ctrl Pts',(1.50468300191011,76.17107742524,14.4587111828717));
#64990=CARTESIAN_POINT('Ctrl Pts',(1.46625175666687,76.1785485603453,14.5081577299275));
#64991=CARTESIAN_POINT('Ctrl Pts',(1.42553043846439,76.1861085972088,14.5556602595519));
#64992=CARTESIAN_POINT('Ctrl Pts',(1.39344501459786,76.1920653539622,14.5930887826207));
#64993=CARTESIAN_POINT('Ctrl Pts',(1.35993781077964,76.1980774328039,14.6293115024797));
#64994=CARTESIAN_POINT('Ctrl Pts',(1.3251174969929,76.2041965854019,14.6642262173261));
#64995=CARTESIAN_POINT('Ctrl Pts',(1.27871197201487,76.2123516666705,14.7107575519323));
#64996=CARTESIAN_POINT('Ctrl Pts',(1.22980912458991,76.2205534344995,14.7548720734239));
#64997=CARTESIAN_POINT('Ctrl Pts',(1.17859700383456,76.2287601237931,14.7961622794986));
#64998=CARTESIAN_POINT('Ctrl Pts',(1.15685510209923,76.2322442410209,14.8136918719049));
#64999=CARTESIAN_POINT('Ctrl Pts',(1.13469750425527,76.2357292223335,14.8307127456576));
#65000=CARTESIAN_POINT('Ctrl Pts',(1.11214088953549,76.2392117709786,14.8471954707205));
#65001=CARTESIAN_POINT('Ctrl Pts',(1.1120683588603,76.2392229690953,14.8472484708357));
#65002=CARTESIAN_POINT('Ctrl Pts',(1.11199582380467,76.2392341672263,14.8473014655748));
#65003=CARTESIAN_POINT('Ctrl Pts',(1.11192328436901,76.2392453653717,14.8473544549371));
#65004=CARTESIAN_POINT('Ctrl Pts',(1.07975507531341,76.2442112749825,14.8708530232226));
#65005=CARTESIAN_POINT('Ctrl Pts',(1.04672524814866,76.2491799969426,14.8932938242039));
#65006=CARTESIAN_POINT('Ctrl Pts',(1.01314163335639,76.2541489889907,14.9147600024979));
#65007=CARTESIAN_POINT('Ctrl Pts',(0.979548542731243,76.259119383072,14.9362322376122));
#65008=CARTESIAN_POINT('Ctrl Pts',(0.945401876828864,76.2640900161531,14.9567296890912));
#65009=CARTESIAN_POINT('Ctrl Pts',(0.910604768726041,76.2690624667108,14.9761262412943));
#65010=CARTESIAN_POINT('Ctrl Pts',(0.889373533642221,76.2720963759202,14.987960924752));
#65011=CARTESIAN_POINT('Ctrl Pts',(0.867899895825725,76.275130992031,14.9993858049844));
#65012=CARTESIAN_POINT('Ctrl Pts',(0.846204859160859,76.2781661497328,15.0103947483936));
#65013=CARTESIAN_POINT('Ctrl Pts',(0.796822753343998,76.2850747565776,15.0354532360449));
#65014=CARTESIAN_POINT('Ctrl Pts',(0.746295197571573,76.2919894181333,15.0583600802408));
#65015=CARTESIAN_POINT('Ctrl Pts',(0.694854334359175,76.2989088701488,15.0790498124819));
#65016=CARTESIAN_POINT('Ctrl Pts',(0.694804855660447,76.2989155256647,15.0790697130233));
#65017=CARTESIAN_POINT('Ctrl Pts',(0.694755376114044,76.2989221811735,15.0790896115014));
#65018=CARTESIAN_POINT('Ctrl Pts',(0.694705895720112,76.2989288366753,15.0791095079162));
#65019=CARTESIAN_POINT('Ctrl Pts',(0.616257700799937,76.3094807352923,15.1106540794923));
#65020=CARTESIAN_POINT('Ctrl Pts',(0.535681447237287,76.3200146847492,15.1370128233276));
#65021=CARTESIAN_POINT('Ctrl Pts',(0.453661557581416,76.3305748587873,15.1580026317918));
#65022=CARTESIAN_POINT('Ctrl Pts',(0.380788019203144,76.3399574274701,15.1766517865162));
#65023=CARTESIAN_POINT('Ctrl Pts',(0.306771473373925,76.3493533885477,15.1910536728427));
#65024=CARTESIAN_POINT('Ctrl Pts',(0.232129202297214,76.3588065019626,15.201088110003));
#65025=CARTESIAN_POINT('Ctrl Pts',(0.232080751365556,76.3588126380588,15.2010946234413));
#65026=CARTESIAN_POINT('Ctrl Pts',(0.232032300165493,76.3588187741885,15.2011011350494));
#65027=CARTESIAN_POINT('Ctrl Pts',(0.231983848697136,76.3588249103517,15.2011076448271));
#65028=CARTESIAN_POINT('Ctrl Pts',(0.137991589429435,76.3707286123759,15.2137361314379));
#65029=CARTESIAN_POINT('Ctrl Pts',(0.0429853382493918,76.3827589998507,
15.2194764706094));
#65030=CARTESIAN_POINT('Ctrl Pts',(-0.0520240868000823,76.3948323315213,
15.2182468575097));
#65031=CARTESIAN_POINT('Ctrl Pts',(-0.0577682407686029,76.3955622704299,
15.2181725166013));
#65032=CARTESIAN_POINT('Ctrl Pts',(-0.0635123907735374,76.3962923643382,
15.2180727002637));
#65033=CARTESIAN_POINT('Ctrl Pts',(-0.0692563074998502,76.3970225939822,
15.2179473912935));
#65034=CARTESIAN_POINT('Ctrl Pts',(-0.128876426799208,76.4046021569473,
15.2166467220632));
#65035=CARTESIAN_POINT('Ctrl Pts',(-0.188474756072447,76.4121963263439,
15.2125994948107));
#65036=CARTESIAN_POINT('Ctrl Pts',(-0.247812949518697,76.4197844676737,
15.2057811438586));
#65037=CARTESIAN_POINT('Ctrl Pts',(-0.247822696909592,76.4197857141657,
15.2057800238189));
#65038=CARTESIAN_POINT('Ctrl Pts',(-0.247832444293133,76.4197869606571,
15.2057789037042));
#65039=CARTESIAN_POINT('Ctrl Pts',(-0.247842191669441,76.4197882071481,
15.2057777835145));
#65040=CARTESIAN_POINT('Ctrl Pts',(-0.296768621773948,76.4260449015995,
15.2001550515277));
#65041=CARTESIAN_POINT('Ctrl Pts',(-0.345511860507362,76.4322899800438,
15.1926421540169));
#65042=CARTESIAN_POINT('Ctrl Pts',(-0.393923595077852,76.4384991181169,
15.1832364327955));
#65043=CARTESIAN_POINT('Ctrl Pts',(-0.472724647314597,76.4486058952854,
15.1679264932556));
#65044=CARTESIAN_POINT('Ctrl Pts',(-0.55065561839925,76.4586178271985,15.1475983375985));
#65045=CARTESIAN_POINT('Ctrl Pts',(-0.627072151467601,76.4686417005575,
15.1224496752263));
#65046=CARTESIAN_POINT('Ctrl Pts',(-0.63608060953238,76.4698233773384,15.119484993877));
#65047=CARTESIAN_POINT('Ctrl Pts',(-0.64506808015541,76.471005227474,15.116453318266));
#65048=CARTESIAN_POINT('Ctrl Pts',(-0.654033554488171,76.4721874318132,
15.1133549679532));
#65049=CARTESIAN_POINT('Ctrl Pts',(-0.674750719656962,76.4749192362498,
15.1061953874561));
#65050=CARTESIAN_POINT('Ctrl Pts',(-0.69534887222477,76.4776536452001,15.0986812613525));
#65051=CARTESIAN_POINT('Ctrl Pts',(-0.715817134101095,76.4803915333587,
15.0908145306932));
#65052=CARTESIAN_POINT('Ctrl Pts',(-0.743519894557304,76.4840971269393,
15.0801673073802));
#65053=CARTESIAN_POINT('Ctrl Pts',(-0.770984721891046,76.4878090925378,
15.06887420287));
#65054=CARTESIAN_POINT('Ctrl Pts',(-0.798189458128453,76.4915296306858,
15.056951901387));
#65055=CARTESIAN_POINT('Ctrl Pts',(-0.911084414566109,76.5069692213686,
15.0074764095161));
#65056=CARTESIAN_POINT('Ctrl Pts',(-1.01943964134501,76.5225282019892,14.9471703884302));
#65057=CARTESIAN_POINT('Ctrl Pts',(-1.12135445929174,76.5381286396529,14.877182845032));
#65058=CARTESIAN_POINT('Ctrl Pts',(-1.2017001135926,76.5504274142247,14.8220074045953));
#65059=CARTESIAN_POINT('Ctrl Pts',(-1.27804160555201,76.5627518078509,14.7608149186131));
#65060=CARTESIAN_POINT('Ctrl Pts',(-1.34943037510579,76.57506064616,14.6941830749454));
#65061=CARTESIAN_POINT('Ctrl Pts',(-1.39751624084463,76.5833516021469,14.6493013672404));
#65062=CARTESIAN_POINT('Ctrl Pts',(-1.44336147044613,76.5916368827775,14.6019471847877));
#65063=CARTESIAN_POINT('Ctrl Pts',(-1.48668558555809,76.5999089266508,14.5522850350241));
#65064=CARTESIAN_POINT('Ctrl Pts',(-1.49158704091489,76.60084478082,14.5466665288097));
#65065=CARTESIAN_POINT('Ctrl Pts',(-1.49645619035975,76.6017805347959,14.5410186158649));
#65066=CARTESIAN_POINT('Ctrl Pts',(-1.50129260439728,76.6027162098982,14.5353416113803));
#65067=CARTESIAN_POINT('Ctrl Pts',(-1.52167244313396,76.6066589880696,14.5114196652845));
#65068=CARTESIAN_POINT('Ctrl Pts',(-1.54147096485587,76.6106003627238,14.486981144753));
#65069=CARTESIAN_POINT('Ctrl Pts',(-1.56066967448821,76.6145419509358,14.462062680762));
#65070=CARTESIAN_POINT('Ctrl Pts',(-1.62763578885548,76.6282904190389,14.3751457607483));
#65071=CARTESIAN_POINT('Ctrl Pts',(-1.68731612124307,76.6420412457091,14.2823730686698));
#65072=CARTESIAN_POINT('Ctrl Pts',(-1.73899513408363,76.6558316937168,14.185139277798));
#65073=CARTESIAN_POINT('Ctrl Pts',(-1.78985545719773,76.6694036759008,14.0894458473409));
#65074=CARTESIAN_POINT('Ctrl Pts',(-1.83296499614123,76.6830141672576,13.9894312397797));
#65075=CARTESIAN_POINT('Ctrl Pts',(-1.86762072967996,76.6966756005143,13.8864282818764));
#65076=CARTESIAN_POINT('Ctrl Pts',(-1.89216199676877,76.7063498693332,13.8134873037834));
#65077=CARTESIAN_POINT('Ctrl Pts',(-1.91246355224693,76.7160492137621,13.7390479787698));
#65078=CARTESIAN_POINT('Ctrl Pts',(-1.92827250707106,76.7257702474795,13.6635842692239));
#65079=CARTESIAN_POINT('Ctrl Pts',(-1.92827968198353,76.7257746593819,13.6635500199319));
#65080=CARTESIAN_POINT('Ctrl Pts',(-1.92828685597066,76.7257790712888,13.6635157704289));
#65081=CARTESIAN_POINT('Ctrl Pts',(-1.92829402903243,76.7257834832001,13.6634815207149));
#65082=CARTESIAN_POINT('Ctrl Pts',(-1.94524041126691,76.7362066383932,13.5825664579412));
#65083=CARTESIAN_POINT('Ctrl Pts',(-1.95702124385381,76.746654153287,13.5004726711336));
#65084=CARTESIAN_POINT('Ctrl Pts',(-1.96353759162479,76.756969596949,13.4178452341049));
#65085=CARTESIAN_POINT('Ctrl Pts',(-1.96430620794729,76.758186324271,13.4080991617622));
#65086=CARTESIAN_POINT('Ctrl Pts',(-1.96500158041824,76.7594012065497,13.3983457239801));
#65087=CARTESIAN_POINT('Ctrl Pts',(-1.96562354819451,76.7606139810479,13.3885860263595));
#65088=CARTESIAN_POINT('Ctrl Pts',(-1.96602724284844,76.7614011449493,13.3822513931138));
#65089=CARTESIAN_POINT('Ctrl Pts',(-1.96640002443412,76.7621874395988,13.3759140270023));
#65090=CARTESIAN_POINT('Ctrl Pts',(-1.96674185096452,76.762972801968,13.369574190282));
#65091=CARTESIAN_POINT('Ctrl Pts',(-1.97173157861374,76.7744369335669,13.2770300026252));
#65092=CARTESIAN_POINT('Ctrl Pts',(-1.97012670401495,76.7857014028749,13.1839488204329));
#65093=CARTESIAN_POINT('Ctrl Pts',(-1.96201561172285,76.7969266255661,13.0912432452857));
#65094=CARTESIAN_POINT('Ctrl Pts',(-1.95484308074262,76.8068529406188,13.0092649388088));
#65095=CARTESIAN_POINT('Ctrl Pts',(-1.94257920657521,76.8167502917483,12.9275798932984));
#65096=CARTESIAN_POINT('Ctrl Pts',(-1.92530718457434,76.8267249305343,12.8469077778324));
#65097=CARTESIAN_POINT('Ctrl Pts',(-1.92300670533757,76.8280534634311,12.8361629717751));
#65098=CARTESIAN_POINT('Ctrl Pts',(-1.92061742967071,76.8293833739384,12.8254360763024));
#65099=CARTESIAN_POINT('Ctrl Pts',(-1.91813959563186,76.8307149190786,12.8147287361971));
#65100=CARTESIAN_POINT('Ctrl Pts',(-1.9079801459258,76.8361744315682,12.7708272151185));
#65101=CARTESIAN_POINT('Ctrl Pts',(-1.89633200080765,76.8416609959429,12.7272575490495));
#65102=CARTESIAN_POINT('Ctrl Pts',(-1.88321815517742,76.8471892187894,12.6841450721228));
#65103=CARTESIAN_POINT('Ctrl Pts',(-1.88321681362367,76.8471897843297,12.6841406616923));
#65104=CARTESIAN_POINT('Ctrl Pts',(-1.88321547205458,76.8471903498704,12.6841362512665));
#65105=CARTESIAN_POINT('Ctrl Pts',(-1.88321413047017,76.8471909154116,12.6841318408456));
#65106=CARTESIAN_POINT('Ctrl Pts',(-1.85561868320266,76.8588236991485,12.5934125855832));
#65107=CARTESIAN_POINT('Ctrl Pts',(-1.82141417942789,76.8706001098608,12.5044844413145));
#65108=CARTESIAN_POINT('Ctrl Pts',(-1.7810669786483,76.8824653213828,12.4182971120898));
#65109=CARTESIAN_POINT('Ctrl Pts',(-1.74067621942913,76.8943433424699,12.3320167358754));
#65110=CARTESIAN_POINT('Ctrl Pts',(-1.69413295237097,76.906309356748,12.2484822131731));
#65111=CARTESIAN_POINT('Ctrl Pts',(-1.64189620607594,76.9183086184102,12.1685643294944));
#65112=CARTESIAN_POINT('Ctrl Pts',(-1.59030313053314,76.9301600229733,12.0896312086111));
#65113=CARTESIAN_POINT('Ctrl Pts',(-1.53315848344633,76.9420431346575,12.0142237961768));
#65114=CARTESIAN_POINT('Ctrl Pts',(-1.47085200607609,76.9539180294252,11.9431258890206));
#65115=CARTESIAN_POINT('Ctrl Pts',(-1.43887697541807,76.9600121008651,11.9066391888092));
#65116=CARTESIAN_POINT('Ctrl Pts',(-1.40554141244029,76.9661042828369,11.871286756175));
#65117=CARTESIAN_POINT('Ctrl Pts',(-1.37088976906968,76.9721914266629,11.8371724623512));
#65118=CARTESIAN_POINT('Ctrl Pts',(-1.3708804480234,76.9721930640614,11.8371632858481));
#65119=CARTESIAN_POINT('Ctrl Pts',(-1.37087112688185,76.9721947014595,11.8371541094346));
#65120=CARTESIAN_POINT('Ctrl Pts',(-1.37086180564508,76.9721963388573,11.8371449331108));
#65121=CARTESIAN_POINT('Ctrl Pts',(-1.35497785140035,76.9749865642426,11.8215079193249));
#65122=CARTESIAN_POINT('Ctrl Pts',(-1.33882684784642,76.9777759223102,11.8061391757218));
#65123=CARTESIAN_POINT('Ctrl Pts',(-1.32241583834212,76.9805609549376,11.7910442661207));
#65124=CARTESIAN_POINT('Ctrl Pts',(-1.26061011048626,76.9910497044928,11.734195120151));
#65125=CARTESIAN_POINT('Ctrl Pts',(-1.19511367713146,77.0014774844399,11.6812232869333));
#65126=CARTESIAN_POINT('Ctrl Pts',(-1.12643793634185,77.0118924418064,11.6324249051649));
#65127=CARTESIAN_POINT('Ctrl Pts',(-1.05763810402149,77.0223262181618,11.5835383486522));
#65128=CARTESIAN_POINT('Ctrl Pts',(-0.985645517210265,77.032747692906,11.5388423265716));
#65129=CARTESIAN_POINT('Ctrl Pts',(-0.911016984403536,77.0431983409845,
11.4986938705813));
#65130=CARTESIAN_POINT('Ctrl Pts',(-0.836716025017025,77.0536031171371,
11.4587216416525));
#65131=CARTESIAN_POINT('Ctrl Pts',(-0.759801326271844,77.064037300583,11.4232596668721));
#65132=CARTESIAN_POINT('Ctrl Pts',(-0.680885783738669,77.0745271496242,
11.3926851118145));
#65133=CARTESIAN_POINT('Ctrl Pts',(-0.623293559583517,77.0821825964214,
11.3703719327904));
#65134=CARTESIAN_POINT('Ctrl Pts',(-0.564637168277213,77.0898674127886,
11.3506625403562));
#65135=CARTESIAN_POINT('Ctrl Pts',(-0.505178035093774,77.0975846091653,
11.3336993763504));
#65136=CARTESIAN_POINT('Ctrl Pts',(-0.505171807848367,77.097585417399,11.3336975997725));
#65137=CARTESIAN_POINT('Ctrl Pts',(-0.505165580593133,77.0975862256336,
11.3336958232242));
#65138=CARTESIAN_POINT('Ctrl Pts',(-0.505159353328048,77.097587033869,11.3336940467055));
#65139=CARTESIAN_POINT('Ctrl Pts',(-0.427970794669812,77.1076053200649,
11.3116736393542));
#65140=CARTESIAN_POINT('Ctrl Pts',(-0.349268028875698,77.1177520080522,
11.2942127955183));
#65141=CARTESIAN_POINT('Ctrl Pts',(-0.269698011573538,77.1279543471805,
11.2814182132585));
#65142=CARTESIAN_POINT('Ctrl Pts',(-0.249182504980679,77.1305848123073,
11.278119391094));
#65143=CARTESIAN_POINT('Ctrl Pts',(-0.228609489462926,77.1332189671837,
11.2751305338261));
#65144=CARTESIAN_POINT('Ctrl Pts',(-0.207990316034561,77.1358555448891,
11.2724529787815));
#65145=CARTESIAN_POINT('Ctrl Pts',(-0.10725594034829,77.1487364690456,11.259371861019));
#65146=CARTESIAN_POINT('Ctrl Pts',(-0.00541727235168708,77.1616738252754,
11.2537213749054));
#65147=CARTESIAN_POINT('Ctrl Pts',(0.0963934601931026,77.1745429068827,
11.2556178907869));
#65148=CARTESIAN_POINT('Ctrl Pts',(0.17795911434822,77.1848529698145,11.2571372842204));
#65149=CARTESIAN_POINT('Ctrl Pts',(0.259510820212742,77.1951193141316,11.2634973388782));
#65150=CARTESIAN_POINT('Ctrl Pts',(0.340547509078918,77.2052984574678,11.2747743781765));
#65151=CARTESIAN_POINT('Ctrl Pts',(0.39663827639075,77.2123441051651,11.2825799511348));
#65152=CARTESIAN_POINT('Ctrl Pts',(0.452487902306173,77.2193491360449,11.2927430994818));
#65153=CARTESIAN_POINT('Ctrl Pts',(0.50790757268455,77.2263613506863,11.3052703577388));
#65154=CARTESIAN_POINT('Ctrl Pts',(0.507914707147799,77.2263622534053,11.3052719704381));
#65155=CARTESIAN_POINT('Ctrl Pts',(0.507921841603943,77.2263631561244,11.3052735831766));
#65156=CARTESIAN_POINT('Ctrl Pts',(0.507928976052952,77.2263640588436,11.3052751959543));
#65157=CARTESIAN_POINT('Ctrl Pts',(0.587522134718372,77.2364349519282,11.3232676252247));
#65158=CARTESIAN_POINT('Ctrl Pts',(0.666100435522896,77.2465264961178,11.3460970025154));
#65159=CARTESIAN_POINT('Ctrl Pts',(0.743194502175447,77.2566484730819,11.3735298284475));
#65160=CARTESIAN_POINT('Ctrl Pts',(0.821686836697399,77.2669540340206,11.401460208092));
#65161=CARTESIAN_POINT('Ctrl Pts',(0.898640612120766,77.2772913354049,11.4341640505644));
#65162=CARTESIAN_POINT('Ctrl Pts',(0.973518518869272,77.2876640329312,11.4714023624243));
#65163=CARTESIAN_POINT('Ctrl Pts',(1.04830534795594,77.298024113638,11.5085953795034));
#65164=CARTESIAN_POINT('Ctrl Pts',(1.12102068657583,77.3084196510644,11.5503131175396));
#65165=CARTESIAN_POINT('Ctrl Pts',(1.19109289573764,77.3188451736256,11.5963036137688));
#65166=CARTESIAN_POINT('Ctrl Pts',(1.26064147502899,77.3291927891949,11.6419504359812));
#65167=CARTESIAN_POINT('Ctrl Pts',(1.32758505909059,77.3395700470451,11.69180718385));
#65168=CARTESIAN_POINT('Ctrl Pts',(1.39134313883558,77.3499607493381,11.7455983626169));
#65169=CARTESIAN_POINT('Ctrl Pts',(1.40192323838504,77.351684996133,11.7545245415187));
#65170=CARTESIAN_POINT('Ctrl Pts',(1.41241559772089,77.3534095869227,11.7635589824088));
#65171=CARTESIAN_POINT('Ctrl Pts',(1.42281754746619,77.3551344158924,11.7727003302305));
#65172=CARTESIAN_POINT('Ctrl Pts',(1.42282233205405,77.3551352092624,11.772704534979));
#65173=CARTESIAN_POINT('Ctrl Pts',(1.42282711662277,77.3551360026326,11.77270873975));
#65174=CARTESIAN_POINT('Ctrl Pts',(1.42283190117237,77.3551367960028,11.7727129445437));
#65175=CARTESIAN_POINT('Ctrl Pts',(1.49178772355645,77.3665709952717,11.83331321602));
#65176=CARTESIAN_POINT('Ctrl Pts',(1.55686292742098,77.3781202132658,11.8986606409092));
#65177=CARTESIAN_POINT('Ctrl Pts',(1.61748310439179,77.3896949852914,11.9680812937928));
#65178=CARTESIAN_POINT('Ctrl Pts',(1.62634461250205,77.3913869951354,11.9782292628237));
#65179=CARTESIAN_POINT('Ctrl Pts',(1.63511096716908,77.3930795478172,11.9884641933827));
#65180=CARTESIAN_POINT('Ctrl Pts',(1.64378042463416,77.3947723606193,11.9987839027811));
#65181=CARTESIAN_POINT('Ctrl Pts',(1.70831329689349,77.4073731574692,12.0756007613956));
#65182=CARTESIAN_POINT('Ctrl Pts',(1.76748340896777,77.4199876766516,12.1571160574602));
#65183=CARTESIAN_POINT('Ctrl Pts',(1.82069415277911,77.4325363819662,12.2426072139777));
#65184=CARTESIAN_POINT('Ctrl Pts',(1.82353306578513,77.4332058836528,12.2471683596929));
#65185=CARTESIAN_POINT('Ctrl Pts',(1.82635503030065,77.4338752086482,12.2517408672331));
#65186=CARTESIAN_POINT('Ctrl Pts',(1.82915995940703,77.4345443486145,12.2563246423749));
#65187=CARTESIAN_POINT('Ctrl Pts',(1.88152687236951,77.4470369261602,12.3419019046812));
#65188=CARTESIAN_POINT('Ctrl Pts',(1.92796415656752,77.4594676719648,12.4314258227001));
#65189=CARTESIAN_POINT('Ctrl Pts',(1.96781410106725,77.4719740172061,12.5240025913411));
#65190=CARTESIAN_POINT('Ctrl Pts',(1.98315658591846,77.4767890405347,12.5596452424985));
#65191=CARTESIAN_POINT('Ctrl Pts',(1.9975217601537,77.4816149068815,12.5957378830938));
#65192=CARTESIAN_POINT('Ctrl Pts',(2.01087099221024,77.4864577737665,12.6322193067018));
#65193=CARTESIAN_POINT('Ctrl Pts',(2.0108720939687,77.4864581734651,12.6322223176403));
#65194=CARTESIAN_POINT('Ctrl Pts',(2.01087319572024,77.4864585731638,12.6322253285815));
#65195=CARTESIAN_POINT('Ctrl Pts',(2.01087429746486,77.4864589728627,12.6322283395253));
#65196=CARTESIAN_POINT('Ctrl Pts',(2.04106169996882,77.4974105760809,12.7147271066467));
#65197=CARTESIAN_POINT('Ctrl Pts',(2.06608403955404,77.5084003137361,12.7993526711409));
#65198=CARTESIAN_POINT('Ctrl Pts',(2.08580312643331,77.5194164056155,12.8853238092665));
#65199=CARTESIAN_POINT('Ctrl Pts',(2.08730391839802,77.5202548248728,12.8918669516587));
#65200=CARTESIAN_POINT('Ctrl Pts',(2.08877401506984,77.5210933966942,12.8984178811239));
#65201=CARTESIAN_POINT('Ctrl Pts',(2.09021336741114,77.5219321158401,12.9049762501793));
#65202=CARTESIAN_POINT('Ctrl Pts',(2.10996961694659,77.5334441996157,12.9949950536975));
#65203=CARTESIAN_POINT('Ctrl Pts',(2.12393616280023,77.5449809014144,13.0864086301881));
#65204=CARTESIAN_POINT('Ctrl Pts',(2.13200609891081,77.556523293635,13.1785445195497));
#65205=CARTESIAN_POINT('Ctrl Pts',(2.13423662267569,77.559713601439,13.2040108042889));
#65206=CARTESIAN_POINT('Ctrl Pts',(2.13601636211932,77.5629043424034,13.2295323125144));
#65207=CARTESIAN_POINT('Ctrl Pts',(2.13734235872415,77.5660951135256,13.2550948890815));
#65208=CARTESIAN_POINT('Ctrl Pts',(2.14232969036316,77.5780962255288,13.3512407211473));
#65209=CARTESIAN_POINT('Ctrl Pts',(2.14089489791625,77.5901027681026,13.4479841449771));
#65210=CARTESIAN_POINT('Ctrl Pts',(2.13289656690917,77.6021470596629,13.5443487324733));
#65211=CARTESIAN_POINT('Ctrl Pts',(2.13107517228774,77.6048898078497,13.5662930532581));
#65212=CARTESIAN_POINT('Ctrl Pts',(2.12891362379868,77.6076345153341,13.5882177374866));
#65213=CARTESIAN_POINT('Ctrl Pts',(2.12641063000288,77.6103815666591,13.6101112935434));
#65214=CARTESIAN_POINT('Ctrl Pts',(2.1236052103067,77.6134605322987,13.6346501531619));
#65215=CARTESIAN_POINT('Ctrl Pts',(2.12037088223282,77.6165423238692,13.6591495531585));
#65216=CARTESIAN_POINT('Ctrl Pts',(2.11670601944608,77.6196280495591,13.6835941296998));
#65217=CARTESIAN_POINT('Ctrl Pts',(2.11670524046315,77.6196287054439,13.6835993255035));
#65218=CARTESIAN_POINT('Ctrl Pts',(2.11670446146078,77.6196293613288,13.6836045213047));
#65219=CARTESIAN_POINT('Ctrl Pts',(2.11670368243896,77.6196300172139,13.6836097171035));
#65220=CARTESIAN_POINT('Ctrl Pts',(2.09538566729208,77.6375783829701,13.8257933032405));
#65221=CARTESIAN_POINT('Ctrl Pts',(2.05947832160496,77.655611188779,13.9662187126111));
#65222=CARTESIAN_POINT('Ctrl Pts',(2.0099402891869,77.673671542634,14.1021424064051));
#65223=CARTESIAN_POINT('Ctrl Pts',(1.98606321552611,77.6823765391444,14.1676569190038));
#65224=CARTESIAN_POINT('Ctrl Pts',(1.95901852711184,77.6910885492128,14.2321287723318));
#65225=CARTESIAN_POINT('Ctrl Pts',(1.9289030818708,77.6998046301978,14.2952632597381));
#65226=CARTESIAN_POINT('Ctrl Pts',(1.88358371898808,77.7129210637724,14.3902714763619));
#65227=CARTESIAN_POINT('Ctrl Pts',(1.83129880201968,77.7260495789763,14.4822625088632));
#65228=CARTESIAN_POINT('Ctrl Pts',(1.7724595102298,77.7392058631395,14.5700920668984));
#65229=CARTESIAN_POINT('Ctrl Pts',(1.7492554525336,77.744394218871,14.604728821864));
#65230=CARTESIAN_POINT('Ctrl Pts',(1.72503253993325,77.7495868944068,14.6387186414649));
#65231=CARTESIAN_POINT('Ctrl Pts',(1.69981784227148,77.7547848549544,14.6719926195448));
#65232=CARTESIAN_POINT('Ctrl Pts',(1.69981660386776,77.7547851102489,14.671994253775));
#65233=CARTESIAN_POINT('Ctrl Pts',(1.69981536546164,77.7547853655434,14.6719958880034));
#65234=CARTESIAN_POINT('Ctrl Pts',(1.69981412705314,77.7547856208379,14.67199752223));
#65235=CARTESIAN_POINT('Ctrl Pts',(1.64313040410961,77.7664708153475,14.7467984065401));
#65236=CARTESIAN_POINT('Ctrl Pts',(1.58143200068949,77.7782306262676,14.8179957495507));
#65237=CARTESIAN_POINT('Ctrl Pts',(1.51529722136469,77.7900116645491,14.8850828315672));
#65238=CARTESIAN_POINT('Ctrl Pts',(1.44377162948131,77.8027530049556,14.957638350735));
#65239=CARTESIAN_POINT('Ctrl Pts',(1.36704130178963,77.8155220989792,15.0254047507615));
#65240=CARTESIAN_POINT('Ctrl Pts',(1.28579953138186,77.8283149763608,15.0877474472356));
#65241=CARTESIAN_POINT('Ctrl Pts',(1.20448669408966,77.8411190444136,15.150144678479));
#65242=CARTESIAN_POINT('Ctrl Pts',(1.11865162134025,77.8539471269003,15.207104864544));
#65243=CARTESIAN_POINT('Ctrl Pts',(1.02907503919655,77.8667820022936,15.2579246110916));
#65244=CARTESIAN_POINT('Ctrl Pts',(0.970030639997629,77.875242109704,15.2914224442365));
#65245=CARTESIAN_POINT('Ctrl Pts',(0.909362676786896,77.8837048759993,15.3222509845227));
#65246=CARTESIAN_POINT('Ctrl Pts',(0.847321744242881,77.8921618205561,15.3502070063442));
#65247=CARTESIAN_POINT('Ctrl Pts',(0.847318445389668,77.8921622702304,15.3502084928275));
#65248=CARTESIAN_POINT('Ctrl Pts',(0.847315146532601,77.8921627199048,15.3502099793027));
#65249=CARTESIAN_POINT('Ctrl Pts',(0.847311847671628,77.8921631695792,15.3502114657698));
#65250=CARTESIAN_POINT('Ctrl Pts',(0.751839703651021,77.9051771691595,15.3932312238575));
#65251=CARTESIAN_POINT('Ctrl Pts',(0.653001772150457,77.9182546770568,15.4295023368545));
#65252=CARTESIAN_POINT('Ctrl Pts',(0.551921930566669,77.9313687437658,15.4587289085861));
#65253=CARTESIAN_POINT('Ctrl Pts',(0.546319225166615,77.9320956369941,15.4603488940224));
#65254=CARTESIAN_POINT('Ctrl Pts',(0.540709636524094,77.9328226424649,15.4619472488097));
#65255=CARTESIAN_POINT('Ctrl Pts',(0.535093357459425,77.9335497555618,15.4635239269901));
#65256=CARTESIAN_POINT('Ctrl Pts',(0.433033464499162,77.9467629673682,15.4921755670641));
#65257=CARTESIAN_POINT('Ctrl Pts',(0.328762471159584,77.9600120971272,15.5136736717721));
#65258=CARTESIAN_POINT('Ctrl Pts',(0.223256850228694,77.9732939102643,15.5277683984637));
#65259=CARTESIAN_POINT('Ctrl Pts',(0.113355082324048,77.987129142282,15.5424504160459));
#65260=CARTESIAN_POINT('Ctrl Pts',(0.0020733120532726,78.0010049627816,
15.549097396372));
#65261=CARTESIAN_POINT('Ctrl Pts',(-0.109329002057391,78.0149269846661,
15.5473790722238));
#65262=CARTESIAN_POINT('Ctrl Pts',(-0.153880271922976,78.0204945867308,
15.5466918915001));
#65263=CARTESIAN_POINT('Ctrl Pts',(-0.198447432834363,78.0260691514268,
15.5446669978625));
#65264=CARTESIAN_POINT('Ctrl Pts',(-0.242936648274478,78.0316492858954,
15.5412872090875));
#65265=CARTESIAN_POINT('Ctrl Pts',(-0.347325188771049,78.0447423936787,
15.5333569452266));
#65266=CARTESIAN_POINT('Ctrl Pts',(-0.451458589162047,78.0578354273157,
15.5179519585374));
#65267=CARTESIAN_POINT('Ctrl Pts',(-0.554255689722849,78.0709375224221,
15.4953540740277));
#65268=CARTESIAN_POINT('Ctrl Pts',(-0.577203339882884,78.0738623354103,
15.4903094925632));
#65269=CARTESIAN_POINT('Ctrl Pts',(-0.600084417394092,78.0767875992885,
15.4849066746044));
#65270=CARTESIAN_POINT('Ctrl Pts',(-0.62288694974159,78.079713414447,15.4791491029078));
#65271=CARTESIAN_POINT('Ctrl Pts',(-0.748692098686231,78.0958555957712,
15.4473836764269));
#65272=CARTESIAN_POINT('Ctrl Pts',(-0.872105958835944,78.1120145928236,
15.4048215640543));
#65273=CARTESIAN_POINT('Ctrl Pts',(-0.991312055030119,78.1282337846007,
15.3520022596885));
#65274=CARTESIAN_POINT('Ctrl Pts',(-1.06979246515111,78.1389118360018,15.3172281935855));
#65275=CARTESIAN_POINT('Ctrl Pts',(-1.14645373737088,78.1496165478377,15.2780078421207));
#65276=CARTESIAN_POINT('Ctrl Pts',(-1.22081454342312,78.1603660617898,15.2344625968421));
#65277=CARTESIAN_POINT('Ctrl Pts',(-1.25027921111984,78.1646254408003,15.217208262872));
#65278=CARTESIAN_POINT('Ctrl Pts',(-1.2793831890253,78.1688919399429,15.1992742662859));
#65279=CARTESIAN_POINT('Ctrl Pts',(-1.30809417781881,78.1731652012549,15.1806685500313));
#65280=CARTESIAN_POINT('Ctrl Pts',(-1.30812371705732,78.1731695977905,15.1806494075805));
#65281=CARTESIAN_POINT('Ctrl Pts',(-1.30815325587059,78.1731739943298,15.1806302644248));
#65282=CARTESIAN_POINT('Ctrl Pts',(-1.30818279425854,78.1731783908727,15.1806111205643));
#65283=CARTESIAN_POINT('Ctrl Pts',(-1.41737792056874,78.189431175567,15.109841643521));
#65284=CARTESIAN_POINT('Ctrl Pts',(-1.5207631788598,78.2057337640861,15.0294435545618));
#65285=CARTESIAN_POINT('Ctrl Pts',(-1.61694821230293,78.2220782538494,14.9406692825966));
#65286=CARTESIAN_POINT('Ctrl Pts',(-1.62982206252277,78.2242658760355,14.9287873230054));
#65287=CARTESIAN_POINT('Ctrl Pts',(-1.64256688192539,78.2264542493202,14.916755246334));
#65288=CARTESIAN_POINT('Ctrl Pts',(-1.65517929332439,78.2286433552017,14.9045760001642));
#65289=CARTESIAN_POINT('Ctrl Pts',(-1.76407406223872,78.2475439580723,14.7994211526694));
#65290=CARTESIAN_POINT('Ctrl Pts',(-1.86309701647429,78.2664987986576,14.6832927316156));
#65291=CARTESIAN_POINT('Ctrl Pts',(-1.94996231045361,78.285474771462,14.5582134121645));
#65292=CARTESIAN_POINT('Ctrl Pts',(-1.99849692699484,78.2960772977573,14.4883273100322));
#65293=CARTESIAN_POINT('Ctrl Pts',(-2.04323398820215,78.3066860509469,14.415649484336));
#65294=CARTESIAN_POINT('Ctrl Pts',(-2.08377078159536,78.3172933926086,14.3405580188543));
#65295=CARTESIAN_POINT('Ctrl Pts',(-2.08378709230659,78.3172976606642,14.3405278044464));
#65296=CARTESIAN_POINT('Ctrl Pts',(-2.0838034023366,78.3173019287196,14.3404975896503));
#65297=CARTESIAN_POINT('Ctrl Pts',(-2.08381971168551,78.3173061967748,14.3404673744656));
#65298=CARTESIAN_POINT('Ctrl Pts',(-2.12724565660621,78.3286704967171,14.260015178002));
#65299=CARTESIAN_POINT('Ctrl Pts',(-2.16584353660947,78.3400337477527,14.1768104245508));
#65300=CARTESIAN_POINT('Ctrl Pts',(-2.19948308923245,78.3514450876868,14.0914575837564));
#65301=CARTESIAN_POINT('Ctrl Pts',(-2.2475372827229,78.3677462181841,13.9695308158096));
#65302=CARTESIAN_POINT('Ctrl Pts',(-2.28549512559791,78.3841529438893,13.8431691311632));
#65303=CARTESIAN_POINT('Ctrl Pts',(-2.31292841914167,78.4006375907827,13.7141136233115));
#65304=CARTESIAN_POINT('Ctrl Pts',(-2.32514673585844,78.4079795687478,13.656634521633));
#65305=CARTESIAN_POINT('Ctrl Pts',(-2.33527668108419,78.4153370111229,13.5986208868508));
#65306=CARTESIAN_POINT('Ctrl Pts',(-2.3432770851121,78.4227075131537,13.5402262096473));
#65307=CARTESIAN_POINT('Ctrl Pts',(-2.35893393412833,78.437131639369,13.4259474005852));
#65308=CARTESIAN_POINT('Ctrl Pts',(-2.36643003500849,78.451603907741,13.3102103371841));
#65309=CARTESIAN_POINT('Ctrl Pts',(-2.36545462636837,78.4660907289047,13.1943147466042));
#65310=CARTESIAN_POINT('Ctrl Pts',(-2.3648207581295,78.4755049738069,13.1190001237149));
#65311=CARTESIAN_POINT('Ctrl Pts',(-2.36061034689751,78.4849253656596,13.0436188684554));
#65312=CARTESIAN_POINT('Ctrl Pts',(-2.35274996603477,78.4943427127835,12.968527724849));
#65313=CARTESIAN_POINT('Ctrl Pts',(-2.34751826938446,78.5006106919392,12.9185487109394));
#65314=CARTESIAN_POINT('Ctrl Pts',(-2.3406699929971,78.5068771835314,12.868701506355));
#65315=CARTESIAN_POINT('Ctrl Pts',(-2.33218792754542,78.5131394588166,12.819097278665));
#65316=CARTESIAN_POINT('Ctrl Pts',(-2.33218084850186,78.5131446852463,12.8190558794928));
#65317=CARTESIAN_POINT('Ctrl Pts',(-2.33217376831915,78.5131499116753,12.8190144804834));
#65318=CARTESIAN_POINT('Ctrl Pts',(-2.33216668699728,78.5131551381034,12.8189730816368));
#65319=CARTESIAN_POINT('Ctrl Pts',(-2.31698524176577,78.5243599291308,12.7302192680173));
#65320=CARTESIAN_POINT('Ctrl Pts',(-2.29656927625846,78.5355608981172,12.6422135313059));
#65321=CARTESIAN_POINT('Ctrl Pts',(-2.27116370661245,78.5468272037072,12.5554795194696));
#65322=CARTESIAN_POINT('Ctrl Pts',(-2.2368150186937,78.5620594075152,12.4382139140918));
#65323=CARTESIAN_POINT('Ctrl Pts',(-2.19333698767226,78.5774162578449,12.3232372644642));
#65324=CARTESIAN_POINT('Ctrl Pts',(-2.14131353447015,78.5928567706968,12.2118170719353));
#65325=CARTESIAN_POINT('Ctrl Pts',(-2.12842492193079,78.5966820989921,12.1842131432805));
#65326=CARTESIAN_POINT('Ctrl Pts',(-2.11501156929086,78.6005125671688,12.1568275809929));
#65327=CARTESIAN_POINT('Ctrl Pts',(-2.10108189738572,78.6043475619254,12.1296798495071));
#65328=CARTESIAN_POINT('Ctrl Pts',(-2.0357411851411,78.6223365921446,12.0023364258291));
#65329=CARTESIAN_POINT('Ctrl Pts',(-1.95903634319664,78.6404233998862,11.8802289007183));
#65330=CARTESIAN_POINT('Ctrl Pts',(-1.87195445874316,78.6585095289508,11.7655542465218));
#65331=CARTESIAN_POINT('Ctrl Pts',(-1.86692715734923,78.6595536545164,11.7589339941867));
#65332=CARTESIAN_POINT('Ctrl Pts',(-1.86186528308215,78.6605977783431,11.7523385067422));
#65333=CARTESIAN_POINT('Ctrl Pts',(-1.85676903010409,78.6616418816847,11.7457682038198));
#65334=CARTESIAN_POINT('Ctrl Pts',(-1.79446025389726,78.67440749629,11.6654371181837));
#65335=CARTESIAN_POINT('Ctrl Pts',(-1.72701058074564,78.6871690082607,11.5888748317974));
#65336=CARTESIAN_POINT('Ctrl Pts',(-1.65483746441543,78.6998883415336,11.5168887899053));
#65337=CARTESIAN_POINT('Ctrl Pts',(-1.6279452206241,78.7046276603912,11.4900662514509));
#65338=CARTESIAN_POINT('Ctrl Pts',(-1.60039753415085,78.7093611264458,11.4638786844688));
#65339=CARTESIAN_POINT('Ctrl Pts',(-1.57221713776477,78.7140867817196,11.4383663647336));
#65340=CARTESIAN_POINT('Ctrl Pts',(-1.57220858679433,78.7140882156575,11.4383586233559));
#65341=CARTESIAN_POINT('Ctrl Pts',(-1.57220003576561,78.7140896495947,11.4383508820403));
#65342=CARTESIAN_POINT('Ctrl Pts',(-1.57219148467867,78.7140910835312,11.438343140787));
#65343=CARTESIAN_POINT('Ctrl Pts',(-1.50634963536783,78.7251321394107,11.3787368660992));
#65344=CARTESIAN_POINT('Ctrl Pts',(-1.43701291110985,78.7361571730373,11.3227866844017));
#65345=CARTESIAN_POINT('Ctrl Pts',(-1.3646606564299,78.7472508903118,11.2707448125877));
#65346=CARTESIAN_POINT('Ctrl Pts',(-1.25704704269546,78.7637512054844,11.193339983724));
#65347=CARTESIAN_POINT('Ctrl Pts',(-1.14273590660334,78.780408671037,11.1245581429311));
#65348=CARTESIAN_POINT('Ctrl Pts',(-1.02326272375693,78.7971727676276,11.0651276515219));
#65349=CARTESIAN_POINT('Ctrl Pts',(-1.00348002954322,78.7999486122877,11.055286989287));
#65350=CARTESIAN_POINT('Ctrl Pts',(-0.983555729790525,78.8027273840396,
11.0457028076324));
#65351=CARTESIAN_POINT('Ctrl Pts',(-0.963496713582175,78.8055088578284,
11.0363785244326));
#65352=CARTESIAN_POINT('Ctrl Pts',(-0.820137989090681,78.8253876260803,
10.9697392968433));
#65353=CARTESIAN_POINT('Ctrl Pts',(-0.669897993251188,78.8454022618114,
10.9163786242148));
#65354=CARTESIAN_POINT('Ctrl Pts',(-0.515481627642138,78.8654394717011,
10.8776113001209));
#65355=CARTESIAN_POINT('Ctrl Pts',(-0.40414780216269,78.8798862514849,10.8496601533759));
#65356=CARTESIAN_POINT('Ctrl Pts',(-0.290644999770457,78.8943437228425,
10.8292975903655));
#65357=CARTESIAN_POINT('Ctrl Pts',(-0.176056080459361,78.9087697597579,
10.8170014127815));
#65358=CARTESIAN_POINT('Ctrl Pts',(-0.147309435278708,78.9123887847654,
10.8139167004357));
#65359=CARTESIAN_POINT('Ctrl Pts',(-0.118494434526164,78.9160058347536,
10.8113393877997));
#65360=CARTESIAN_POINT('Ctrl Pts',(-0.0896281377141354,78.9196202514175,
10.809276495863));
#65361=CARTESIAN_POINT('Ctrl Pts',(-0.0895780721078092,78.9196265202494,
10.8092729179903));
#65362=CARTESIAN_POINT('Ctrl Pts',(-0.0895280063471258,78.9196327890733,
10.809269341665));
#65363=CARTESIAN_POINT('Ctrl Pts',(-0.0894779404322766,78.9196390578894,
10.8092657668871));
#65364=CARTESIAN_POINT('Ctrl Pts',(-0.0189960371881366,78.9284641854592,
10.8042332581691));
#65365=CARTESIAN_POINT('Ctrl Pts',(0.0518292881978163,78.9372714066356,
10.8022646760837));
#65366=CARTESIAN_POINT('Ctrl Pts',(0.122616109482706,78.9461112930357,10.8033530299608));
#65367=CARTESIAN_POINT('Ctrl Pts',(0.139060825042286,78.9481649156563,10.8036058689725));
#65368=CARTESIAN_POINT('Ctrl Pts',(0.155503594876505,78.9502202956633,10.8040235450871));
#65369=CARTESIAN_POINT('Ctrl Pts',(0.171939877407273,78.952278049441,10.8046057292954));
#65370=CARTESIAN_POINT('Ctrl Pts',(3.10725610873535,87.7143427064635,13.0695248188307));
#65371=CARTESIAN_POINT('Ctrl Pts',(3.1757813234749,87.8112593268296,13.8431174629201));
#65372=CARTESIAN_POINT('Ctrl Pts',(2.70607125735979,88.0061219845433,15.451413371914));
#65373=CARTESIAN_POINT('Ctrl Pts',(0.523695573931209,88.3010140160292,16.7441283328975));
#65374=CARTESIAN_POINT('Ctrl Pts',(-1.97106212602582,88.5980351971415,16.2018249379459));
#65375=CARTESIAN_POINT('Ctrl Pts',(-3.43495695755572,88.8966756526658,14.0914727997129));
#65376=CARTESIAN_POINT('Ctrl Pts',(-3.06482110497942,89.196419298767,11.5400069829436));
#65377=CARTESIAN_POINT('Ctrl Pts',(-1.05291748826742,89.4967419819177,9.92398169476627));
#65378=CARTESIAN_POINT('Ctrl Pts',(1.52616256504467,89.7971047842489,10.1087303766691));
#65379=CARTESIAN_POINT('Ctrl Pts',(3.21140767063859,90.0858783146224,11.9293218383111));
#65380=CARTESIAN_POINT('Ctrl Pts',(3.30323743242567,90.3626559668299,14.276240933303));
#65381=CARTESIAN_POINT('Ctrl Pts',(1.98789207577699,90.627200204105,16.0898027557638));
#65382=CARTESIAN_POINT('Ctrl Pts',(0.0241974623197764,90.86830082554,16.6489912297625));
#65383=CARTESIAN_POINT('Ctrl Pts',(-1.69368084010089,91.0861200642671,16.1049922105906));
#65384=CARTESIAN_POINT('Ctrl Pts',(-2.81033338844852,91.2809643968551,14.9452095342079));
#65385=CARTESIAN_POINT('Ctrl Pts',(-3.23146979160152,91.4744780596263,13.4011379073283));
#65386=CARTESIAN_POINT('Ctrl Pts',(-2.86407265519059,91.6665312140481,11.8566330885878));
#65387=CARTESIAN_POINT('Ctrl Pts',(-1.80990108569908,91.8569947753109,10.6866444426581));
#65388=CARTESIAN_POINT('Ctrl Pts',(-0.337754813899104,92.0457495597246,
10.1687628870289));
#65389=CARTESIAN_POINT('Ctrl Pts',(1.18763110189629,92.2326830579912,10.4178406020297));
#65390=CARTESIAN_POINT('Ctrl Pts',(2.39508588402732,92.4176866578788,11.3569396665519));
#65391=CARTESIAN_POINT('Ctrl Pts',(2.99846077048866,92.6006617408029,12.7442190178643));
#65392=CARTESIAN_POINT('Ctrl Pts',(2.86406492662596,92.7815187653892,14.2338326625746));
#65393=CARTESIAN_POINT('Ctrl Pts',(2.04358132087385,92.9601718455146,15.4619408054085));
#65394=CARTESIAN_POINT('Ctrl Pts',(0.751296929799555,93.1365472418599,16.1382458662903));
#65395=CARTESIAN_POINT('Ctrl Pts',(-0.687290894650869,93.3105782793599,
16.1133154333185));
#65396=CARTESIAN_POINT('Ctrl Pts',(-1.92137415892804,93.4822078008889,15.4121948543585));
#65397=CARTESIAN_POINT('Ctrl Pts',(-2.65731745584422,93.6513873028849,14.2229713817855));
#65398=CARTESIAN_POINT('Ctrl Pts',(-2.72467523247443,93.7995574197688,12.9993478101219));
#65399=CARTESIAN_POINT('Ctrl Pts',(-2.35680632127026,93.9275748885119,12.0272037600701));
#65400=CARTESIAN_POINT('Ctrl Pts',(-1.60700565797264,94.072380504393,11.1189899717487));
#65401=CARTESIAN_POINT('Ctrl Pts',(-0.203446123334107,94.2505639771652,
10.5658090747328));
#65402=CARTESIAN_POINT('Ctrl Pts',(1.49575309669785,94.4598530632153,11.0726893252092));
#65403=CARTESIAN_POINT('Ctrl Pts',(2.49678227792913,94.6646318210984,12.4902982018984));
#65404=CARTESIAN_POINT('Ctrl Pts',(2.42399981467692,94.831561367221,13.9024753634234));
#65405=CARTESIAN_POINT('Ctrl Pts',(1.93577122333525,94.9464973222074,14.6988423857405));
#65406=CARTESIAN_POINT('Ctrl Pts',(1.60855744696839,95.003490707163,15.0199806827984));
#65407=CARTESIAN_POINT('Ctrl Pts',(1.40135621667452,95.0359246481305,15.1765886648261));
#65408=CARTESIAN_POINT('Ctrl Pts',(0.635078339402144,95.1491319775694,15.6724562054475));
#65409=CARTESIAN_POINT('Ctrl Pts',(-0.720559162425314,95.3000177856171,
15.6863625542683));
#65410=CARTESIAN_POINT('Ctrl Pts',(-1.8708747810453,95.4860536506094,14.6538899840269));
#65411=CARTESIAN_POINT('Ctrl Pts',(-2.16058008250562,95.5890455651222,13.8568424348098));
#65412=CARTESIAN_POINT('Ctrl Pts',(-2.17993256337463,95.6570456913322,13.3104242948812));
#65413=CARTESIAN_POINT('Ctrl Pts',(-2.1480847252082,95.702204137361,12.9493357867975));
#65414=CARTESIAN_POINT('Ctrl Pts',(-2.02450479564091,95.7583256112684,12.5130496666982));
#65415=CARTESIAN_POINT('Ctrl Pts',(-1.75360435091691,95.8251694120019,12.0460412039888));
#65416=CARTESIAN_POINT('Ctrl Pts',(-1.37849074783188,95.8915126624859,11.6632242622581));
#65417=CARTESIAN_POINT('Ctrl Pts',(-0.923748479397676,95.9573798229221,
11.387018956129));
#65418=CARTESIAN_POINT('Ctrl Pts',(-0.418445576848205,96.0227717513124,
11.2327055835173));
#65419=CARTESIAN_POINT('Ctrl Pts',(0.105520528106774,96.0877139012382,11.2084459531777));
#65420=CARTESIAN_POINT('Ctrl Pts',(0.786338536997495,96.1737086069401,11.3479552873821));
#65421=CARTESIAN_POINT('Ctrl Pts',(1.52303500717221,96.2801377489088,11.8291464763594));
#65422=CARTESIAN_POINT('Ctrl Pts',(2.01715667209892,96.4062625436115,12.7482521021039));
#65423=CARTESIAN_POINT('Ctrl Pts',(2.01045790345397,96.5309261038632,13.7793624143205));
#65424=CARTESIAN_POINT('Ctrl Pts',(1.51637800664929,96.6542580992801,14.6719798136283));
#65425=CARTESIAN_POINT('Ctrl Pts',(0.663888543978092,96.7763970615423,15.2136124389558));
#65426=CARTESIAN_POINT('Ctrl Pts',(-0.336049672007484,96.8974833143649,
15.2806088470557));
#65427=CARTESIAN_POINT('Ctrl Pts',(-1.23702901529549,97.0176655564635,14.8631858266175));
#65428=CARTESIAN_POINT('Ctrl Pts',(-1.89420479903932,97.1503580247946,13.982436534616));
#65429=CARTESIAN_POINT('Ctrl Pts',(-1.96193864187616,97.2954556790466,12.7556076580179));
#65430=CARTESIAN_POINT('Ctrl Pts',(-1.19721912475719,97.4530355758608,11.6597400684424));
#65431=CARTESIAN_POINT('Ctrl Pts',(-0.0281587723358688,97.5971720203736,
11.306636794884));
#65432=CARTESIAN_POINT('Ctrl Pts',(1.01129169438915,97.7282311720686,11.6161391384085));
#65433=CARTESIAN_POINT('Ctrl Pts',(1.70064661125628,97.8463613303911,12.3082123810528));
#65434=CARTESIAN_POINT('Ctrl Pts',(1.97428043926036,97.9648262448885,13.249425353759));
#65435=CARTESIAN_POINT('Ctrl Pts',(1.76313138826258,98.0837817071748,14.2102217464921));
#65436=CARTESIAN_POINT('Ctrl Pts',(1.11322929763875,98.203378013067,14.956581570516));
#65437=CARTESIAN_POINT('Ctrl Pts',(0.257678298166416,98.3137402058402,15.2727661476035));
#65438=CARTESIAN_POINT('Ctrl Pts',(-0.728874592332793,98.4349564865196,
15.191430874777));
#65439=CARTESIAN_POINT('Ctrl Pts',(-1.58805687481121,98.5572254947863,14.6275712205838));
#65440=CARTESIAN_POINT('Ctrl Pts',(-2.044720159798,98.6911826223687,13.6163889972621));
#65441=CARTESIAN_POINT('Ctrl Pts',(-1.98673559372465,98.7849432279802,12.8437627048067));
#65442=CARTESIAN_POINT('Ctrl Pts',(-1.73073495584116,98.8689105869503,12.2196452596691));
#65443=CARTESIAN_POINT('Ctrl Pts',(-1.32097441252665,98.9533854474619,11.6654502341919));
#65444=CARTESIAN_POINT('Ctrl Pts',(-0.660793794475513,99.0441439765671,
11.3083813226462));
#65445=CARTESIAN_POINT('Ctrl Pts',(-0.0598969890390443,99.1195820525141,
11.218007253297));
#65446=CARTESIAN_POINT('Ctrl Pts',(0.462847266033453,99.1845785155341,11.2370733537587));
#65447=CARTESIAN_POINT('Ctrl Pts',(1.09828510826303,99.2664639660505,11.4455188681155));
#65448=CARTESIAN_POINT('Ctrl Pts',(1.72023525244675,99.3657958818357,11.9636756035441));
#65449=CARTESIAN_POINT('Ctrl Pts',(2.25134488151769,99.4997248277813,12.9196203077091));
#65450=CARTESIAN_POINT('Ctrl Pts',(2.16906732596622,99.6700195549317,14.380884605866));
#65451=CARTESIAN_POINT('Ctrl Pts',(1.2485647484992,99.818254361804,15.2625087202804));
#65452=CARTESIAN_POINT('Ctrl Pts',(0.444576618744897,99.9243407315245,15.5426355963576));
#65453=CARTESIAN_POINT('Ctrl Pts',(-0.124650265136175,99.9954998612222,
15.6294832306231));
#65454=CARTESIAN_POINT('Ctrl Pts',(-0.918737021005253,100.094399188943,
15.4865591877427));
#65455=CARTESIAN_POINT('Ctrl Pts',(-1.67679364799143,100.203632794597,15.0184860900645));
#65456=CARTESIAN_POINT('Ctrl Pts',(-2.12728633876912,100.295798559161,14.4164680057849));
#65457=CARTESIAN_POINT('Ctrl Pts',(-2.44385567388375,100.407434629731,13.5761810060226));
#65458=CARTESIAN_POINT('Ctrl Pts',(-2.43349609112601,100.558140077718,12.3181762302894));
#65459=CARTESIAN_POINT('Ctrl Pts',(-1.71815741033316,100.692891281568,11.40887510621));
#65460=CARTESIAN_POINT('Ctrl Pts',(-1.17713165256918,100.770845395039,11.0964290332353));
#65461=CARTESIAN_POINT('Ctrl Pts',(2.90276395212938,88.0589545760158,13.0875997250314));
#65462=CARTESIAN_POINT('Ctrl Pts',(2.95627977768387,88.1495677453682,13.8115623287023));
#65463=CARTESIAN_POINT('Ctrl Pts',(2.49516168027059,88.330846998084,15.3000193606636));
#65464=CARTESIAN_POINT('Ctrl Pts',(0.465788387492445,88.6026204963471,16.4588062976629));
#65465=CARTESIAN_POINT('Ctrl Pts',(-1.80476146413435,88.8739729860722,15.9279676833003));
#65466=CARTESIAN_POINT('Ctrl Pts',(-3.10155536278043,89.1446181204072,13.9957909307606));
#65467=CARTESIAN_POINT('Ctrl Pts',(-2.73404191397397,89.4142810240402,11.7062879228243));
#65468=CARTESIAN_POINT('Ctrl Pts',(-0.915092544492909,89.682695115903,10.2891619118715));
#65469=CARTESIAN_POINT('Ctrl Pts',(1.37353687594359,89.949600710797,10.486936929915));
#65470=CARTESIAN_POINT('Ctrl Pts',(2.83987558909873,90.2049373800204,12.1177004430502));
#65471=CARTESIAN_POINT('Ctrl Pts',(2.89136847089987,90.4487224978189,14.1852973727042));
#65472=CARTESIAN_POINT('Ctrl Pts',(1.71420211019153,90.6810455124534,15.7611841780058));
#65473=CARTESIAN_POINT('Ctrl Pts',(-0.0128299371654484,90.8923117455707,
16.2269021591063));
#65474=CARTESIAN_POINT('Ctrl Pts',(-1.5090788482888,91.0829321788154,15.7301039900146));
#65475=CARTESIAN_POINT('Ctrl Pts',(-2.4712190066523,91.2533322525557,14.7025505955179));
#65476=CARTESIAN_POINT('Ctrl Pts',(-2.82047005478047,91.4225304385253,13.347796228399));
#65477=CARTESIAN_POINT('Ctrl Pts',(-2.48034860101448,91.590488555968,12.0020035560574));
#65478=CARTESIAN_POINT('Ctrl Pts',(-1.54368559506711,91.7571719060457,10.9914121456071));
#65479=CARTESIAN_POINT('Ctrl Pts',(-0.247851535959068,91.9225516418578,
10.5560764938838));
#65480=CARTESIAN_POINT('Ctrl Pts',(1.08726220401839,92.0866038825379,10.793671671954));
#65481=CARTESIAN_POINT('Ctrl Pts',(2.13696021870783,92.2493092899283,11.6345510627664));
#65482=CARTESIAN_POINT('Ctrl Pts',(2.65109720927979,92.4106541005746,12.8651154167332));
#65483=CARTESIAN_POINT('Ctrl Pts',(2.51299220078441,92.5706298715948,14.1805581643091));
#65484=CARTESIAN_POINT('Ctrl Pts',(1.76873005652531,92.7292329498877,15.2596809574676));
#65485=CARTESIAN_POINT('Ctrl Pts',(0.60811066872096,92.8864652975645,15.845136786697));
#65486=CARTESIAN_POINT('Ctrl Pts',(-0.679516057648502,93.042333919981,15.8032945622656));
#65487=CARTESIAN_POINT('Ctrl Pts',(-1.78042322221891,93.1968512659859,15.1552720996806));
#65488=CARTESIAN_POINT('Ctrl Pts',(-2.42972444918458,93.3500347148581,14.0685141712926));
#65489=CARTESIAN_POINT('Ctrl Pts',(-2.47342502433508,93.485032308027,12.9531599654245));
#65490=CARTESIAN_POINT('Ctrl Pts',(-2.12173691667042,93.6023232400316,12.0683988477808));
#65491=CARTESIAN_POINT('Ctrl Pts',(-1.41794563352187,93.7356222147801,11.2443833855659));
#65492=CARTESIAN_POINT('Ctrl Pts',(-0.108651400054405,93.900868814998,10.7521591008224));
#65493=CARTESIAN_POINT('Ctrl Pts',(1.47580000963189,94.0970547503915,11.2528212630621));
#65494=CARTESIAN_POINT('Ctrl Pts',(2.40245789704906,94.291241610282,12.6122252108601));
#65495=CARTESIAN_POINT('Ctrl Pts',(2.30958675223246,94.451495797935,13.9661845313665));
#65496=CARTESIAN_POINT('Ctrl Pts',(1.82188265588916,94.5629134950966,14.7288928580851));
#65497=CARTESIAN_POINT('Ctrl Pts',(1.49719096913084,94.6184378224292,15.0352973716418));
#65498=CARTESIAN_POINT('Ctrl Pts',(1.29186658376209,94.6501156878609,15.1841493917124));
#65499=CARTESIAN_POINT('Ctrl Pts',(0.533511913404019,94.7608712055693,15.654143026697));
#65500=CARTESIAN_POINT('Ctrl Pts',(-0.808074592779245,94.9101512303414,
15.6464877011121));
#65501=CARTESIAN_POINT('Ctrl Pts',(-1.94420320187033,95.0971904649237,14.5863988238769));
#65502=CARTESIAN_POINT('Ctrl Pts',(-2.22188224409465,95.2018810288088,13.7706870299644));
#65503=CARTESIAN_POINT('Ctrl Pts',(-2.22955039463141,95.2714832059397,13.2113581250775));
#65504=CARTESIAN_POINT('Ctrl Pts',(-2.18876276415898,95.3178348388426,12.8417215097046));
#65505=CARTESIAN_POINT('Ctrl Pts',(-2.05167672673761,95.375681883697,12.3951255440082));
#65506=CARTESIAN_POINT('Ctrl Pts',(-1.76041900544877,95.4449678022735,11.9175965276771));
#65507=CARTESIAN_POINT('Ctrl Pts',(-1.36080955808199,95.5141241472378,11.5275545479325));
#65508=CARTESIAN_POINT('Ctrl Pts',(-0.877970487401089,95.5831702281511,
11.2489614525707));
#65509=CARTESIAN_POINT('Ctrl Pts',(-0.342000986324222,95.6521067193162,
11.0985126748453));
#65510=CARTESIAN_POINT('Ctrl Pts',(0.213623207064906,95.720952651231,11.0855717915074));
#65511=CARTESIAN_POINT('Ctrl Pts',(0.93535872538529,95.812630073061,11.2509739490936));
#65512=CARTESIAN_POINT('Ctrl Pts',(1.71507243567299,95.9270440274078,11.7856963334004));
#65513=CARTESIAN_POINT('Ctrl Pts',(2.22879898544115,96.064126183288,12.7961234832359));
#65514=CARTESIAN_POINT('Ctrl Pts',(2.19496889611997,96.201080189433,13.927792625613));
#65515=CARTESIAN_POINT('Ctrl Pts',(1.62336777189102,96.3379891415667,14.9047555231163));
#65516=CARTESIAN_POINT('Ctrl Pts',(0.653637378996546,96.4749390978704,15.4883450793425));
#65517=CARTESIAN_POINT('Ctrl Pts',(-0.479183597507465,96.6120140716515,
15.5362569140024));
#65518=CARTESIAN_POINT('Ctrl Pts',(-1.49550380827525,96.7493002509423,15.0340431944611));
#65519=CARTESIAN_POINT('Ctrl Pts',(-2.22617634409563,96.902165163245,14.001312148663));
#65520=CARTESIAN_POINT('Ctrl Pts',(-2.26912391360259,97.0708521378234,12.5743617552715));
#65521=CARTESIAN_POINT('Ctrl Pts',(-1.34012118721779,97.2557343745632,11.3126762919694));
#65522=CARTESIAN_POINT('Ctrl Pts',(0.0517192767727834,97.4261669198471,
10.9312737951385));
#65523=CARTESIAN_POINT('Ctrl Pts',(1.27666129064818,97.5819976087186,11.331693969795));
#65524=CARTESIAN_POINT('Ctrl Pts',(2.07664831716534,97.7230050544256,12.178854656779));
#65525=CARTESIAN_POINT('Ctrl Pts',(2.3738396568357,97.8648420439373,13.3133439150153));
#65526=CARTESIAN_POINT('Ctrl Pts',(2.08993730325257,98.0075746833811,14.4582197611074));
#65527=CARTESIAN_POINT('Ctrl Pts',(1.28596236049746,98.1512642776317,15.3331498015845));
#65528=CARTESIAN_POINT('Ctrl Pts',(0.248580457378911,98.2839133694417,15.6853991648919));
#65529=CARTESIAN_POINT('Ctrl Pts',(-0.933019279072089,98.4295580310931,
15.5563383436846));
#65530=CARTESIAN_POINT('Ctrl Pts',(-1.94528147010697,98.5763136628078,14.8529360099437));
#65531=CARTESIAN_POINT('Ctrl Pts',(-2.45982197643258,98.7367255305564,13.6289096816955));
#65532=CARTESIAN_POINT('Ctrl Pts',(-2.36668773663634,98.848688246541,12.7090141811426));
#65533=CARTESIAN_POINT('Ctrl Pts',(-2.04306609875493,98.9487318029496,11.9738450868454));
#65534=CARTESIAN_POINT('Ctrl Pts',(-1.53940292542878,99.0491943457798,11.3277821125564));
#65535=CARTESIAN_POINT('Ctrl Pts',(-0.747158491221365,99.1567306174659,
10.9250034101893));
#65536=CARTESIAN_POINT('Ctrl Pts',(-0.0355768373076844,99.2458149990659,
10.8359274483637));
#65537=CARTESIAN_POINT('Ctrl Pts',(0.579456403249374,99.322420701784,10.8735010914224));
#65538=CARTESIAN_POINT('Ctrl Pts',(1.31947344673593,99.4186441904899,11.1366691296655));
#65539=CARTESIAN_POINT('Ctrl Pts',(2.03176253387087,99.5348675172455,11.7600543420649));
#65540=CARTESIAN_POINT('Ctrl Pts',(2.62304119418394,99.6908473899985,12.8875930599719));
#65541=CARTESIAN_POINT('Ctrl Pts',(2.48567427465143,99.8877397945851,14.5730938352413));
#65542=CARTESIAN_POINT('Ctrl Pts',(1.40893999897151,100.057286246309,15.5547480034218));
#65543=CARTESIAN_POINT('Ctrl Pts',(0.489040922673266,100.177833295425,15.8525318981432));
#65544=CARTESIAN_POINT('Ctrl Pts',(-0.157644488075177,100.258454146333,
15.9365107147818));
#65545=CARTESIAN_POINT('Ctrl Pts',(-1.04840784317475,100.369923284926,15.7556200306154));
#65546=CARTESIAN_POINT('Ctrl Pts',(-1.88548202700648,100.492288158336,15.2130321561939));
#65547=CARTESIAN_POINT('Ctrl Pts',(-2.37213571326726,100.594888104147,14.5324827913111));
#65548=CARTESIAN_POINT('Ctrl Pts',(-2.70319266626553,100.718569100259,13.5947914370014));
#65549=CARTESIAN_POINT('Ctrl Pts',(-2.66142717358176,100.88446549619,12.2109455348121));
#65550=CARTESIAN_POINT('Ctrl Pts',(-1.86143294901679,101.0311095758,11.2394258266373));
#65551=CARTESIAN_POINT('Ctrl Pts',(-1.27034543602034,101.115370990615,10.9133596760187));
#65552=CARTESIAN_POINT('Ctrl Pts',(2.6982717955234,88.403566445568,13.1056746312321));
#65553=CARTESIAN_POINT('Ctrl Pts',(2.73677823189285,88.4878761639066,13.7800071944845));
#65554=CARTESIAN_POINT('Ctrl Pts',(2.28425210318142,88.6555720116245,15.1486253494134));
#65555=CARTESIAN_POINT('Ctrl Pts',(0.407881201053683,88.904226976665,16.1734842624281));
#65556=CARTESIAN_POINT('Ctrl Pts',(-1.63846080224287,89.1499107750029,15.654110428655));
#65557=CARTESIAN_POINT('Ctrl Pts',(-2.76815376800513,89.3925605881487,13.9001090618085));
#65558=CARTESIAN_POINT('Ctrl Pts',(-2.40326272296852,89.6321427493135,11.8725688627051));
#65559=CARTESIAN_POINT('Ctrl Pts',(-0.777267600718407,89.8686482498881,
10.6543421289767));
#65560=CARTESIAN_POINT('Ctrl Pts',(1.2209111868425,90.1020966373451,10.8651434831607));
#65561=CARTESIAN_POINT('Ctrl Pts',(2.46834350755888,90.3239964454185,12.3060790477895));
#65562=CARTESIAN_POINT('Ctrl Pts',(2.47949950937406,90.534789028808,14.0943538121054));
#65563=CARTESIAN_POINT('Ctrl Pts',(1.44051214460606,90.7348908208017,15.4325656002478));
#65564=CARTESIAN_POINT('Ctrl Pts',(-0.0498573366506787,90.9163226656018,
15.8048130884501));
#65565=CARTESIAN_POINT('Ctrl Pts',(-1.32447685647671,91.0797442933639,15.3552157694385));
#65566=CARTESIAN_POINT('Ctrl Pts',(-2.13210462485608,91.2257001082563,14.4598916568282));
#65567=CARTESIAN_POINT('Ctrl Pts',(-2.40947031795943,91.3705828174244,13.2944545494697));
#65568=CARTESIAN_POINT('Ctrl Pts',(-2.09662454683838,91.514445897888,12.1473740235271));
#65569=CARTESIAN_POINT('Ctrl Pts',(-1.27747010443514,91.6573490367806,11.2961798485563));
#65570=CARTESIAN_POINT('Ctrl Pts',(-0.15794825801904,91.7993537239909,10.9433901007385));
#65571=CARTESIAN_POINT('Ctrl Pts',(0.986893306140469,91.9405247070845,11.1695027418782));
#65572=CARTESIAN_POINT('Ctrl Pts',(1.87883455338834,92.080931921978,11.9121624589809));
#65573=CARTESIAN_POINT('Ctrl Pts',(2.30373364807092,92.2206464603464,12.986011815602));
#65574=CARTESIAN_POINT('Ctrl Pts',(2.16191947494285,92.3597409778006,14.1272836660435));
#65575=CARTESIAN_POINT('Ctrl Pts',(1.49387879217675,92.4982940542609,15.0574211095268));
#65576=CARTESIAN_POINT('Ctrl Pts',(0.464924407642362,92.6363833532689,15.5520277071038));
#65577=CARTESIAN_POINT('Ctrl Pts',(-0.671741220646141,92.7740895606021,
15.4932736912129));
#65578=CARTESIAN_POINT('Ctrl Pts',(-1.63947228550976,92.9114947310828,14.898349345003));
#65579=CARTESIAN_POINT('Ctrl Pts',(-2.20213144252492,93.0486821268315,13.9140569607997));
#65580=CARTESIAN_POINT('Ctrl Pts',(-2.22217481619574,93.170507196285,12.906972120727));
#65581=CARTESIAN_POINT('Ctrl Pts',(-1.88666751207057,93.2770715915512,12.1095939354917));
#65582=CARTESIAN_POINT('Ctrl Pts',(-1.22888560907111,93.3988639251671,11.3697767993831));
#65583=CARTESIAN_POINT('Ctrl Pts',(-0.0138566767747093,93.5511736528308,
10.938509126912));
#65584=CARTESIAN_POINT('Ctrl Pts',(1.45584692256595,93.7342564375675,11.432953200915));
#65585=CARTESIAN_POINT('Ctrl Pts',(2.30813351616898,93.9178513994656,12.7341522198219));
#65586=CARTESIAN_POINT('Ctrl Pts',(2.19517368978801,94.0714302286491,14.0298936993096));
#65587=CARTESIAN_POINT('Ctrl Pts',(1.70799408844307,94.1793296679858,14.7589433304297));
#65588=CARTESIAN_POINT('Ctrl Pts',(1.38582449129328,94.2333849376954,15.050614060485));
#65589=CARTESIAN_POINT('Ctrl Pts',(1.18237695084966,94.2643067275912,15.1917101185989));
#65590=CARTESIAN_POINT('Ctrl Pts',(0.431945487405895,94.3726104335691,15.6358298479467));
#65591=CARTESIAN_POINT('Ctrl Pts',(-0.895590023133178,94.5202846750657,
15.6066128479558));
#65592=CARTESIAN_POINT('Ctrl Pts',(-2.01753162269537,94.7083272792382,14.5189076637268));
#65593=CARTESIAN_POINT('Ctrl Pts',(-2.28318440568369,94.8147164924953,13.6845316251193));
#65594=CARTESIAN_POINT('Ctrl Pts',(-2.27916822588818,94.8859207205472,13.1122919552739));
#65595=CARTESIAN_POINT('Ctrl Pts',(-2.22944080310975,94.9334655403241,12.7341072326119));
#65596=CARTESIAN_POINT('Ctrl Pts',(-2.07884865783431,94.9930381561256,12.2772014213181));
#65597=CARTESIAN_POINT('Ctrl Pts',(-1.76723365998065,95.0647661925447,11.7891518513653));
#65598=CARTESIAN_POINT('Ctrl Pts',(-1.34312836833211,95.1367356319896,11.3918848336069));
#65599=CARTESIAN_POINT('Ctrl Pts',(-0.832192495404496,95.2089606333801,
11.1109039490121));
#65600=CARTESIAN_POINT('Ctrl Pts',(-0.265556395800235,95.2814416873198,
10.9643197661734));
#65601=CARTESIAN_POINT('Ctrl Pts',(0.321725886023046,95.3541914012238,10.9626976298369));
#65602=CARTESIAN_POINT('Ctrl Pts',(1.08437891377309,95.4515515391821,11.1539926108051));
#65603=CARTESIAN_POINT('Ctrl Pts',(1.90710986417378,95.5739503059066,11.7422461904413));
#65604=CARTESIAN_POINT('Ctrl Pts',(2.4404412987834,95.7219898229644,12.843994864368));
#65605=CARTESIAN_POINT('Ctrl Pts',(2.379479888786,95.8712342750027,14.0762228369055));
#65606=CARTESIAN_POINT('Ctrl Pts',(1.73035753713278,96.0217201838532,15.1375312326044));
#65607=CARTESIAN_POINT('Ctrl Pts',(0.643386214015007,96.1734811341986,15.7630777197292));
#65608=CARTESIAN_POINT('Ctrl Pts',(-0.622317523007441,96.3265448289381,
15.7919049809492));
#65609=CARTESIAN_POINT('Ctrl Pts',(-1.75397860125501,96.480934945421,15.2049005623045));
#65610=CARTESIAN_POINT('Ctrl Pts',(-2.55814788915194,96.6539723016953,14.02018776271));
#65611=CARTESIAN_POINT('Ctrl Pts',(-2.57630918532901,96.8462485966002,12.393115852525));
#65612=CARTESIAN_POINT('Ctrl Pts',(-1.48302324967836,97.0584331732658,10.9656125154963));
#65613=CARTESIAN_POINT('Ctrl Pts',(0.131597325881443,97.2551618193207,10.555910795393));
#65614=CARTESIAN_POINT('Ctrl Pts',(1.54203088690724,97.4357640453685,11.0472488011817));
#65615=CARTESIAN_POINT('Ctrl Pts',(2.45265002307442,97.5996487784601,12.0494969325054));
#65616=CARTESIAN_POINT('Ctrl Pts',(2.77339887441105,97.764857842986,13.3772624762716));
#65617=CARTESIAN_POINT('Ctrl Pts',(2.41674321824258,97.9313676595873,14.7062177757228));
#65618=CARTESIAN_POINT('Ctrl Pts',(1.45869542335619,98.0991505421964,15.7097180326528));
#65619=CARTESIAN_POINT('Ctrl Pts',(0.239482616591414,98.2540865330431,16.0980321821802));
#65620=CARTESIAN_POINT('Ctrl Pts',(-1.13716396581138,98.4241595756667,15.9212458125922));
#65621=CARTESIAN_POINT('Ctrl Pts',(-2.30250606540272,98.5954018308291,15.0783007993036));
#65622=CARTESIAN_POINT('Ctrl Pts',(-2.87492379306717,98.7822684387443,13.641430366129));
#65623=CARTESIAN_POINT('Ctrl Pts',(-2.74663987954804,98.9124332651019,12.5742656574783));
#65624=CARTESIAN_POINT('Ctrl Pts',(-2.35539724166868,99.0285530189489,11.7280449140218));
#65625=CARTESIAN_POINT('Ctrl Pts',(-1.75783143833091,99.1450032440976,10.9901139909209));
#65626=CARTESIAN_POINT('Ctrl Pts',(-0.833523187967213,99.2693172583649,
10.5416254977322));
#65627=CARTESIAN_POINT('Ctrl Pts',(-0.0112566855763176,99.3720479456177,
10.4538476434305));
#65628=CARTESIAN_POINT('Ctrl Pts',(0.696065540465303,99.4602628880338,10.5099288290863));
#65629=CARTESIAN_POINT('Ctrl Pts',(1.54066178520884,99.5708244149292,10.8278193912155));
#65630=CARTESIAN_POINT('Ctrl Pts',(2.34328981529501,99.7039391526554,11.5564330805856));
#65631=CARTESIAN_POINT('Ctrl Pts',(2.99473750685021,99.8819699522155,12.8555658122346));
#65632=CARTESIAN_POINT('Ctrl Pts',(2.80228122333666,100.105460034239,14.7653030646166));
#65633=CARTESIAN_POINT('Ctrl Pts',(1.56931524944386,100.296318130813,15.8469872865633));
#65634=CARTESIAN_POINT('Ctrl Pts',(0.533505226601642,100.431325859326,16.1624281999286));
#65635=CARTESIAN_POINT('Ctrl Pts',(-0.190638711014172,100.521408431442,
16.2435381989408));
#65636=CARTESIAN_POINT('Ctrl Pts',(-1.17807866534425,100.645447380912,16.024680873488));
#65637=CARTESIAN_POINT('Ctrl Pts',(-2.09417040602153,100.780943522073,15.4075782223232));
#65638=CARTESIAN_POINT('Ctrl Pts',(-2.6169850877654,100.893977649135,14.6484975768373));
#65639=CARTESIAN_POINT('Ctrl Pts',(-2.96252965864728,101.029703570786,13.6134018679802));
#65640=CARTESIAN_POINT('Ctrl Pts',(-2.8893582560375,101.210790914664,12.1037148393349));
#65641=CARTESIAN_POINT('Ctrl Pts',(-2.00470848770043,101.369327870032,11.0699765470644));
#65642=CARTESIAN_POINT('Ctrl Pts',(-1.3635592194715,101.45989658619,10.730290318802));
#65643=CARTESIAN_POINT('Ctrl Pts',(2.49377963891743,88.7481783151202,13.1237495374328));
#65644=CARTESIAN_POINT('Ctrl Pts',(2.51727668610183,88.826184582445,13.7484520602668));
#65645=CARTESIAN_POINT('Ctrl Pts',(2.07334252609224,88.9802970251652,14.9972313381631));
#65646=CARTESIAN_POINT('Ctrl Pts',(0.349974014614918,89.2058334569828,15.8881622271935));
#65647=CARTESIAN_POINT('Ctrl Pts',(-1.4721601403514,89.4258485639336,15.3802531740095));
#65648=CARTESIAN_POINT('Ctrl Pts',(-2.43475217322985,89.6405030558901,13.8044271928562));
#65649=CARTESIAN_POINT('Ctrl Pts',(-2.07248353196307,89.8500044745869,12.0388498025858));
#65650=CARTESIAN_POINT('Ctrl Pts',(-0.639442656943906,90.0546013838731,
11.0195223460819));
#65651=CARTESIAN_POINT('Ctrl Pts',(1.06828549774142,90.2545925638933,11.2433500364064));
#65652=CARTESIAN_POINT('Ctrl Pts',(2.09681142601901,90.4430555108166,12.4944576525287));
#65653=CARTESIAN_POINT('Ctrl Pts',(2.06763054784826,90.6208555597969,14.0034102515066));
#65654=CARTESIAN_POINT('Ctrl Pts',(1.1668221790206,90.78873612915,15.1039470224899));
#65655=CARTESIAN_POINT('Ctrl Pts',(-0.0868847361359067,90.9403335856326,
15.3827240177938));
#65656=CARTESIAN_POINT('Ctrl Pts',(-1.13987486466463,91.0765564079124,14.9803275488623));
#65657=CARTESIAN_POINT('Ctrl Pts',(-1.79299024305986,91.1980679639569,14.2172327181384));
#65658=CARTESIAN_POINT('Ctrl Pts',(-1.99847058113838,91.3186351963235,13.2411128705403));
#65659=CARTESIAN_POINT('Ctrl Pts',(-1.71290049266228,91.438403239808,12.2927444909967));
#65660=CARTESIAN_POINT('Ctrl Pts',(-1.01125461380317,91.5575261675155,11.6009475515055));
#65661=CARTESIAN_POINT('Ctrl Pts',(-0.0680449800790074,91.6761558061239,
11.3307037075934));
#65662=CARTESIAN_POINT('Ctrl Pts',(0.886524408262558,91.7944455316312,11.5453338118024));
#65663=CARTESIAN_POINT('Ctrl Pts',(1.62070888806884,91.9125545540277,12.1897738551953));
#65664=CARTESIAN_POINT('Ctrl Pts',(1.95637008686205,92.0306388201183,13.1069082144709));
#65665=CARTESIAN_POINT('Ctrl Pts',(1.81084674910129,92.1488520840062,14.0740091677779));
#65666=CARTESIAN_POINT('Ctrl Pts',(1.21902752782821,92.2673551586341,14.855161261586));
#65667=CARTESIAN_POINT('Ctrl Pts',(0.321738146563767,92.3863014089734,15.2589186275106));
#65668=CARTESIAN_POINT('Ctrl Pts',(-0.663966383643774,92.5058452012233,
15.1832528201601));
#65669=CARTESIAN_POINT('Ctrl Pts',(-1.49852134880062,92.6261381961799,14.6414265903252));
#65670=CARTESIAN_POINT('Ctrl Pts',(-1.97453843586526,92.7473295388048,13.7595997503068));
#65671=CARTESIAN_POINT('Ctrl Pts',(-1.97092460805639,92.8559820845432,12.8607842760296));
#65672=CARTESIAN_POINT('Ctrl Pts',(-1.65159810747073,92.9518199430708,12.1507890232025));
#65673=CARTESIAN_POINT('Ctrl Pts',(-1.03982558462033,93.0621056355542,11.4951702132003));
#65674=CARTESIAN_POINT('Ctrl Pts',(0.0809380465049925,93.2014784906635,
11.1248591530016));
#65675=CARTESIAN_POINT('Ctrl Pts',(1.4358938355,93.3714581247436,11.6130851387679));
#65676=CARTESIAN_POINT('Ctrl Pts',(2.21380913528891,93.5444611886493,12.8560792287835));
#65677=CARTESIAN_POINT('Ctrl Pts',(2.08076062734356,93.6913646593632,14.0936028672527));
#65678=CARTESIAN_POINT('Ctrl Pts',(1.59410552099699,93.7957458408751,14.7889938027743));
#65679=CARTESIAN_POINT('Ctrl Pts',(1.27445801345573,93.8483320529615,15.0659307493282));
#65680=CARTESIAN_POINT('Ctrl Pts',(1.07288731793725,93.8784977673215,15.1992708454853));
#65681=CARTESIAN_POINT('Ctrl Pts',(0.330379061407773,93.9843496615688,15.6175166691962));
#65682=CARTESIAN_POINT('Ctrl Pts',(-0.983105453487106,94.1304181197899,
15.5667379947997));
#65683=CARTESIAN_POINT('Ctrl Pts',(-2.09086004352039,94.3194640935526,14.4514165035768));
#65684=CARTESIAN_POINT('Ctrl Pts',(-2.34448656727271,94.4275519561817,13.598376220274));
#65685=CARTESIAN_POINT('Ctrl Pts',(-2.32878605714495,94.5003582351546,13.0132257854703));
#65686=CARTESIAN_POINT('Ctrl Pts',(-2.27011884206053,94.5490962418056,12.6264929555191));
#65687=CARTESIAN_POINT('Ctrl Pts',(-2.106020588931,94.6103944285541,12.1592772986281));
#65688=CARTESIAN_POINT('Ctrl Pts',(-1.77404831451251,94.6845645828161,11.6607071750535));
#65689=CARTESIAN_POINT('Ctrl Pts',(-1.32544717858223,94.7593471167414,11.2562151192812));
#65690=CARTESIAN_POINT('Ctrl Pts',(-0.786414503407905,94.8347510386092,
10.9728464454538));
#65691=CARTESIAN_POINT('Ctrl Pts',(-0.189111805276248,94.9107766553234,
10.8301268575013));
#65692=CARTESIAN_POINT('Ctrl Pts',(0.429828564981183,94.9874301512166,10.8398234681666));
#65693=CARTESIAN_POINT('Ctrl Pts',(1.23339910216089,95.090473005303,11.0570112725166));
#65694=CARTESIAN_POINT('Ctrl Pts',(2.09914729267456,95.2208565844055,11.6987960474823));
#65695=CARTESIAN_POINT('Ctrl Pts',(2.65208361212563,95.3798534626408,12.8918662454998));
#65696=CARTESIAN_POINT('Ctrl Pts',(2.56399088145202,95.5413883605725,14.224653048198));
#65697=CARTESIAN_POINT('Ctrl Pts',(1.83734730237453,95.7054512261398,15.3703069420924));
#65698=CARTESIAN_POINT('Ctrl Pts',(0.633135049033465,95.8720231705268,16.0378103601158));
#65699=CARTESIAN_POINT('Ctrl Pts',(-0.76545144850742,96.0410755862248,16.0475530478959));
#65700=CARTESIAN_POINT('Ctrl Pts',(-2.01245339423477,96.2125696398999,15.375757930148));
#65701=CARTESIAN_POINT('Ctrl Pts',(-2.89011943420824,96.4057794401457,14.0390633767572));
#65702=CARTESIAN_POINT('Ctrl Pts',(-2.88349445705544,96.6216450553769,12.2118699497786));
#65703=CARTESIAN_POINT('Ctrl Pts',(-1.62592531213895,96.8611319719683,10.6185487390233));
#65704=CARTESIAN_POINT('Ctrl Pts',(0.211475374990095,97.0841567187942,10.1805477956475));
#65705=CARTESIAN_POINT('Ctrl Pts',(1.80740048316628,97.2895304820185,10.7628036325681));
#65706=CARTESIAN_POINT('Ctrl Pts',(2.82865172898348,97.4762925024945,11.9201392082317));
#65707=CARTESIAN_POINT('Ctrl Pts',(3.17295809198639,97.6648736420349,13.4411810375279));
#65708=CARTESIAN_POINT('Ctrl Pts',(2.74354913323257,97.8551606357935,14.9542157903382));
#65709=CARTESIAN_POINT('Ctrl Pts',(1.63142848621491,98.0470368067611,16.0862862637212));
#65710=CARTESIAN_POINT('Ctrl Pts',(0.230384775803907,98.2242596966446,16.5106651994685));
#65711=CARTESIAN_POINT('Ctrl Pts',(-1.34130865255068,98.4187611202403,16.2861532814996));
#65712=CARTESIAN_POINT('Ctrl Pts',(-2.65973066069848,98.6144899988505,15.3036655886634));
#65713=CARTESIAN_POINT('Ctrl Pts',(-3.29002560970176,98.8278113469321,13.6539510505623));
#65714=CARTESIAN_POINT('Ctrl Pts',(-3.12659202245975,98.9761782836627,12.4395171338142));
#65715=CARTESIAN_POINT('Ctrl Pts',(-2.66772838458244,99.1083742349483,11.482244741198));
#65716=CARTESIAN_POINT('Ctrl Pts',(-1.97625995123304,99.2408121424155,10.6524458692854));
#65717=CARTESIAN_POINT('Ctrl Pts',(-0.919887884713065,99.3819038992638,
10.1582475852753));
#65718=CARTESIAN_POINT('Ctrl Pts',(0.0130634661550411,99.4982808921694,
10.0717678384972));
#65719=CARTESIAN_POINT('Ctrl Pts',(0.812674677681222,99.5981050742835,10.14635656675));
#65720=CARTESIAN_POINT('Ctrl Pts',(1.76185012368174,99.7230046393686,10.5189696527654));
#65721=CARTESIAN_POINT('Ctrl Pts',(2.65481709671915,99.8730107880652,11.3528118191064));
#65722=CARTESIAN_POINT('Ctrl Pts',(3.36643381951645,100.073092514433,12.8235385644975));
#65723=CARTESIAN_POINT('Ctrl Pts',(3.11888817202187,100.323180273892,14.9575122939919));
#65724=CARTESIAN_POINT('Ctrl Pts',(1.72969049991617,100.535350015318,16.1392265697048));
#65725=CARTESIAN_POINT('Ctrl Pts',(0.57796953053001,100.684818423227,16.4723245017141));
#65726=CARTESIAN_POINT('Ctrl Pts',(-0.223632933953175,100.784362716553,
16.5505656830996));
#65727=CARTESIAN_POINT('Ctrl Pts',(-1.30774948751375,100.920971476897,16.2937417163607));
#65728=CARTESIAN_POINT('Ctrl Pts',(-2.30285878503657,101.069598885813,15.6021242884526));
#65729=CARTESIAN_POINT('Ctrl Pts',(-2.86183446226353,101.193067194121,14.7645123623634));
#65730=CARTESIAN_POINT('Ctrl Pts',(-3.22186665102905,101.340838041313,13.632012298959));
#65731=CARTESIAN_POINT('Ctrl Pts',(-3.11728933849324,101.537116333136,11.9964841438576));
#65732=CARTESIAN_POINT('Ctrl Pts',(-2.14798402638407,101.707546164264,10.9005272674917));
#65733=CARTESIAN_POINT('Ctrl Pts',(-1.45677300292266,101.804422181766,10.5472209615853));
#65734=CARTESIAN_POINT('Ctrl Pts',(2.49380022861477,88.7482468790765,13.1242986243742));
#65735=CARTESIAN_POINT('Ctrl Pts',(2.51714660453923,88.8262297351317,13.7488179208904));
#65736=CARTESIAN_POINT('Ctrl Pts',(2.07317421855453,88.980319051494,14.9973183482153));
#65737=CARTESIAN_POINT('Ctrl Pts',(0.349974014614918,89.2058334569828,15.8881622271935));
#65738=CARTESIAN_POINT('Ctrl Pts',(-1.4721601403514,89.4258485639336,15.3802531740095));
#65739=CARTESIAN_POINT('Ctrl Pts',(-2.43475217322985,89.6405030558901,13.8044271928562));
#65740=CARTESIAN_POINT('Ctrl Pts',(-2.07248353196307,89.8500044745869,12.0388498025858));
#65741=CARTESIAN_POINT('Ctrl Pts',(-0.639442656943906,90.0546013838731,
11.0195223460819));
#65742=CARTESIAN_POINT('Ctrl Pts',(1.06828549774142,90.2545925638933,11.2433500364064));
#65743=CARTESIAN_POINT('Ctrl Pts',(2.09681142601901,90.4430555108166,12.4944576525287));
#65744=CARTESIAN_POINT('Ctrl Pts',(2.06763054784826,90.6208555597969,14.0034102515066));
#65745=CARTESIAN_POINT('Ctrl Pts',(1.1668221790206,90.78873612915,15.1039470224899));
#65746=CARTESIAN_POINT('Ctrl Pts',(-0.0868847361359067,90.9403335856326,
15.3827240177938));
#65747=CARTESIAN_POINT('Ctrl Pts',(-1.13987486466463,91.0765564079124,14.9803275488623));
#65748=CARTESIAN_POINT('Ctrl Pts',(-1.79299024305986,91.1980679639569,14.2172327181384));
#65749=CARTESIAN_POINT('Ctrl Pts',(-1.99847058113838,91.3186351963235,13.2411128705403));
#65750=CARTESIAN_POINT('Ctrl Pts',(-1.71290049266228,91.438403239808,12.2927444909967));
#65751=CARTESIAN_POINT('Ctrl Pts',(-1.01125461380317,91.5575261675155,11.6009475515055));
#65752=CARTESIAN_POINT('Ctrl Pts',(-0.0680449800790074,91.6761558061239,
11.3307037075934));
#65753=CARTESIAN_POINT('Ctrl Pts',(0.886524408262558,91.7944455316312,11.5453338118024));
#65754=CARTESIAN_POINT('Ctrl Pts',(1.62070888806884,91.9125545540277,12.1897738551953));
#65755=CARTESIAN_POINT('Ctrl Pts',(1.95637008686205,92.0306388201183,13.1069082144709));
#65756=CARTESIAN_POINT('Ctrl Pts',(1.81084674910129,92.1488520840062,14.0740091677779));
#65757=CARTESIAN_POINT('Ctrl Pts',(1.21902752782821,92.2673551586341,14.855161261586));
#65758=CARTESIAN_POINT('Ctrl Pts',(0.321738146563767,92.3863014089734,15.2589186275106));
#65759=CARTESIAN_POINT('Ctrl Pts',(-0.663966383643774,92.5058452012233,
15.1832528201601));
#65760=CARTESIAN_POINT('Ctrl Pts',(-1.49852134880062,92.6261381961799,14.6414265903252));
#65761=CARTESIAN_POINT('Ctrl Pts',(-1.97453843586526,92.7473295388048,13.7595997503068));
#65762=CARTESIAN_POINT('Ctrl Pts',(-1.97092460805639,92.8559820845432,12.8607842760296));
#65763=CARTESIAN_POINT('Ctrl Pts',(-1.65159810747073,92.9518199430708,12.1507890232025));
#65764=CARTESIAN_POINT('Ctrl Pts',(-1.03982558462033,93.0621056355542,11.4951702132003));
#65765=CARTESIAN_POINT('Ctrl Pts',(0.0809380465049925,93.2014784906635,
11.1248591530016));
#65766=CARTESIAN_POINT('Ctrl Pts',(1.4358938355,93.3714581247436,11.6130851387679));
#65767=CARTESIAN_POINT('Ctrl Pts',(2.21380913528891,93.5444611886493,12.8560792287835));
#65768=CARTESIAN_POINT('Ctrl Pts',(2.08076062734356,93.6913646593632,14.0936028672527));
#65769=CARTESIAN_POINT('Ctrl Pts',(1.59410552099699,93.7957458408751,14.7889938027743));
#65770=CARTESIAN_POINT('Ctrl Pts',(1.27445801345573,93.8483320529615,15.0659307493282));
#65771=CARTESIAN_POINT('Ctrl Pts',(1.07288731793725,93.8784977673215,15.1992708454853));
#65772=CARTESIAN_POINT('Ctrl Pts',(0.330379061407773,93.9843496615688,15.6175166691962));
#65773=CARTESIAN_POINT('Ctrl Pts',(-0.983105453487106,94.1304181197899,
15.5667379947997));
#65774=CARTESIAN_POINT('Ctrl Pts',(-2.09086004352039,94.3194640935526,14.4514165035768));
#65775=CARTESIAN_POINT('Ctrl Pts',(-2.34448656727271,94.4275519561817,13.598376220274));
#65776=CARTESIAN_POINT('Ctrl Pts',(-2.32878605714495,94.5003582351546,13.0132257854703));
#65777=CARTESIAN_POINT('Ctrl Pts',(-2.27011884206053,94.5490962418056,12.6264929555191));
#65778=CARTESIAN_POINT('Ctrl Pts',(-2.106020588931,94.6103944285541,12.1592772986281));
#65779=CARTESIAN_POINT('Ctrl Pts',(-1.77404831451251,94.6845645828161,11.6607071750535));
#65780=CARTESIAN_POINT('Ctrl Pts',(-1.32544717858223,94.7593471167414,11.2562151192812));
#65781=CARTESIAN_POINT('Ctrl Pts',(-0.786414503407905,94.8347510386092,
10.9728464454538));
#65782=CARTESIAN_POINT('Ctrl Pts',(-0.189111805276248,94.9107766553234,
10.8301268575013));
#65783=CARTESIAN_POINT('Ctrl Pts',(0.429828564981183,94.9874301512166,10.8398234681666));
#65784=CARTESIAN_POINT('Ctrl Pts',(0.91716227398176,95.049921561671,10.9715392707581));
#65785=CARTESIAN_POINT('Ctrl Pts',(1.18480262056273,95.0868664053839,11.0991467172034));
#65786=CARTESIAN_POINT('Ctrl Pts',(1.26263430499969,95.0979194610116,11.1414618660017));
#65787=CARTESIAN_POINT('Ctrl Pts',(2.60841185759868,116.632148017263,14.370680154362));
#65788=CARTESIAN_POINT('Ctrl Pts',(2.30778866091531,116.727031067497,15.0690888853187));
#65789=CARTESIAN_POINT('Ctrl Pts',(1.12445764834896,116.913723744564,16.1810188066154));
#65790=CARTESIAN_POINT('Ctrl Pts',(-1.25555818790042,117.188688965645,16.0635810015158));
#65791=CARTESIAN_POINT('Ctrl Pts',(-2.81220088569084,117.457618540921,14.3232511812366));
#65792=CARTESIAN_POINT('Ctrl Pts',(-2.64998973991795,117.722051177067,12.0374368167346));
#65793=CARTESIAN_POINT('Ctrl Pts',(-0.941586509937382,117.981899992631,
10.5634534644126));
#65794=CARTESIAN_POINT('Ctrl Pts',(0.899999153910539,118.194538963125,10.741903484399));
#65795=CARTESIAN_POINT('Ctrl Pts',(1.96699814475253,118.36389001071,11.6130329988365));
#65796=CARTESIAN_POINT('Ctrl Pts',(2.28309757924212,118.448491912406,12.2112327280851));
#65797=CARTESIAN_POINT('Ctrl Pts',(2.38806140485046,118.491549366035,12.5616587240347));
#65798=CARTESIAN_POINT('Ctrl Pts',(2.51630021877766,116.733680406233,14.3148119822871));
#65799=CARTESIAN_POINT('Ctrl Pts',(2.22738125818649,116.825032510427,14.9874533144481));
#65800=CARTESIAN_POINT('Ctrl Pts',(1.09057470294181,117.004399481502,16.0555743277148));
#65801=CARTESIAN_POINT('Ctrl Pts',(-1.18668210243013,117.267494666309,15.9429969544623));
#65802=CARTESIAN_POINT('Ctrl Pts',(-2.67031536555362,117.523876159038,14.2838674933955));
#65803=CARTESIAN_POINT('Ctrl Pts',(-2.51623040664612,117.77508338085,12.1121781733781));
#65804=CARTESIAN_POINT('Ctrl Pts',(-0.897653230639775,118.021236678474,
10.7165287022644));
#65805=CARTESIAN_POINT('Ctrl Pts',(0.841225402353136,118.221999068804,10.8845158308112));
#65806=CARTESIAN_POINT('Ctrl Pts',(1.84905875074838,118.381935657463,11.7068661177474));
#65807=CARTESIAN_POINT('Ctrl Pts',(2.1458150030417,118.461333441716,12.2682356637141));
#65808=CARTESIAN_POINT('Ctrl Pts',(2.245862133833,118.502288008538,12.6013801594841));
#65809=CARTESIAN_POINT('Ctrl Pts',(2.42418857995666,116.835212795203,14.2589438102121));
#65810=CARTESIAN_POINT('Ctrl Pts',(2.14697385545769,116.923033953355,14.9058177435774));
#65811=CARTESIAN_POINT('Ctrl Pts',(1.05669175753469,117.095075218441,15.9301298488143));
#65812=CARTESIAN_POINT('Ctrl Pts',(-1.11780601695983,117.346300366974,15.8224129074088));
#65813=CARTESIAN_POINT('Ctrl Pts',(-2.52842984541641,117.590133777157,14.2444838055542));
#65814=CARTESIAN_POINT('Ctrl Pts',(-2.38247107337429,117.828115584635,12.1869195300215));
#65815=CARTESIAN_POINT('Ctrl Pts',(-0.853719951342167,118.06057336432,10.869603940116));
#65816=CARTESIAN_POINT('Ctrl Pts',(0.782451650795737,118.249459174483,11.0271281772233));
#65817=CARTESIAN_POINT('Ctrl Pts',(1.73111935674423,118.399981304216,11.8006992366585));
#65818=CARTESIAN_POINT('Ctrl Pts',(2.00853242684129,118.474174971026,12.3252385993429));
#65819=CARTESIAN_POINT('Ctrl Pts',(2.10366286281553,118.513026651041,12.6411015949336));
#65820=CARTESIAN_POINT('Ctrl Pts',(2.33207694113565,116.936745184174,14.2030756381372));
#65821=CARTESIAN_POINT('Ctrl Pts',(2.06656645272888,117.021035396283,14.8241821727068));
#65822=CARTESIAN_POINT('Ctrl Pts',(1.02280881212754,117.185750955378,15.8046853699137));
#65823=CARTESIAN_POINT('Ctrl Pts',(-1.04892993148955,117.425106067638,15.7018288603554));
#65824=CARTESIAN_POINT('Ctrl Pts',(-2.38654432527919,117.656391395274,14.2051001177131));
#65825=CARTESIAN_POINT('Ctrl Pts',(-2.24871174010246,117.881147788418,12.2616608866649));
#65826=CARTESIAN_POINT('Ctrl Pts',(-0.809786672044562,118.099910050163,
11.0226791779678));
#65827=CARTESIAN_POINT('Ctrl Pts',(0.723677899238335,118.276919280162,11.1697405236356));
#65828=CARTESIAN_POINT('Ctrl Pts',(1.61317996274009,118.418026950969,11.8945323555693));
#65829=CARTESIAN_POINT('Ctrl Pts',(1.87124985064086,118.487016500336,12.3822415349717));
#65830=CARTESIAN_POINT('Ctrl Pts',(1.96146359179807,118.523765293543,12.680823030383));
#65831=CARTESIAN_POINT('Ctrl Pts',(2.85508310539628,22.7016051911778,13.3));
#65832=CARTESIAN_POINT('Ctrl Pts',(2.84040985303552,22.7610702599433,13.7953362626623));
#65833=CARTESIAN_POINT('Ctrl Pts',(2.57005469369539,22.8818105286997,14.7182643754022));
#65834=CARTESIAN_POINT('Ctrl Pts',(1.18387003193848,23.1175816758084,16.1251408416108));
#65835=CARTESIAN_POINT('Ctrl Pts',(-1.44635846823727,23.4073653880304,16.1636979204723));
#65836=CARTESIAN_POINT('Ctrl Pts',(-3.10207688975974,23.7441121923493,13.5585336200215));
#65837=CARTESIAN_POINT('Ctrl Pts',(-1.93931411699474,24.0343451755729,11.1893587933123));
#65838=CARTESIAN_POINT('Ctrl Pts',(0.0883386693549116,24.2813382692206,
10.6296561281468));
#65839=CARTESIAN_POINT('Ctrl Pts',(1.70144742269104,24.4884076529068,11.3202189090701));
#65840=CARTESIAN_POINT('Ctrl Pts',(2.44259794298568,24.6739869579023,12.7117540199086));
#65841=CARTESIAN_POINT('Ctrl Pts',(2.29730552460407,24.8394118737477,14.0742850221851));
#65842=CARTESIAN_POINT('Ctrl Pts',(1.60135946438255,24.9858059086488,15.065894901695));
#65843=CARTESIAN_POINT('Ctrl Pts',(0.527454597690121,25.1297760483933,15.5827695470996));
#65844=CARTESIAN_POINT('Ctrl Pts',(-0.773691505026583,25.2871272558827,
15.5063423998538));
#65845=CARTESIAN_POINT('Ctrl Pts',(-1.91735749878862,25.4569723948024,14.6292447253925));
#65846=CARTESIAN_POINT('Ctrl Pts',(-2.2807995761954,25.6384274211836,13.1312382095964));
#65847=CARTESIAN_POINT('Ctrl Pts',(-1.63447911169001,25.8163001873567,11.7658051165269));
#65848=CARTESIAN_POINT('Ctrl Pts',(-0.30166668820052,25.9908519237952,11.118090048511));
#65849=CARTESIAN_POINT('Ctrl Pts',(1.11827404154826,26.1623781939067,11.4471128168816));
#65850=CARTESIAN_POINT('Ctrl Pts',(2.00298722537565,26.3311895429685,12.5747319143883));
#65851=CARTESIAN_POINT('Ctrl Pts',(1.98502979276238,26.4976150162961,13.9880823206758));
#65852=CARTESIAN_POINT('Ctrl Pts',(1.09529607704403,26.6620054275366,15.0639864439094));
#65853=CARTESIAN_POINT('Ctrl Pts',(-0.258208853904818,26.8247233802242,
15.3408406941205));
#65854=CARTESIAN_POINT('Ctrl Pts',(-1.47752555552934,26.9861415626953,14.7145503488409));
#65855=CARTESIAN_POINT('Ctrl Pts',(-2.02847081070307,27.1466444125973,13.4669408700617));
#65856=CARTESIAN_POINT('Ctrl Pts',(-1.7064364111904,27.2932881153463,12.2648907963243));
#65857=CARTESIAN_POINT('Ctrl Pts',(-0.874436327135088,27.4265029451041,
11.54040839076));
#65858=CARTESIAN_POINT('Ctrl Pts',(0.0984990014798181,27.5464882437543,
11.3336290315483));
#65859=CARTESIAN_POINT('Ctrl Pts',(1.0464095846472,27.6667307527874,11.627693502193));
#65860=CARTESIAN_POINT('Ctrl Pts',(1.97802584892726,27.8276185888103,12.5894195007116));
#65861=CARTESIAN_POINT('Ctrl Pts',(1.9827636101529,27.9896718678958,14.052696341479));
#65862=CARTESIAN_POINT('Ctrl Pts',(1.0366379049331,28.1535448779212,15.0355576473949));
#65863=CARTESIAN_POINT('Ctrl Pts',(0.0602149397180628,28.2775076356642,
15.3404992503449));
#65864=CARTESIAN_POINT('Ctrl Pts',(-0.955566674000275,28.4026811174227,
15.128424970176));
#65865=CARTESIAN_POINT('Ctrl Pts',(-1.74698128488437,28.5292091514289,14.4420850463022));
#65866=CARTESIAN_POINT('Ctrl Pts',(-2.1084540663241,28.657232610625,13.4461169760093));
#65867=CARTESIAN_POINT('Ctrl Pts',(-1.92196705962975,28.8012916705864,12.2675635904411));
#65868=CARTESIAN_POINT('Ctrl Pts',(-0.988491269521039,28.962263576584,11.2671245863818));
#65869=CARTESIAN_POINT('Ctrl Pts',(0.51289185285495,29.1412742662328,11.0539213646967));
#65870=CARTESIAN_POINT('Ctrl Pts',(2.07965481981169,29.3543978617751,11.967943201084));
#65871=CARTESIAN_POINT('Ctrl Pts',(2.52905815177238,29.6044782263651,14.196116432258));
#65872=CARTESIAN_POINT('Ctrl Pts',(0.579839355331495,29.8952708304772,16.0125676359185));
#65873=CARTESIAN_POINT('Ctrl Pts',(-1.6163097135127,30.1459120270744,15.4054900459629));
#65874=CARTESIAN_POINT('Ctrl Pts',(-2.48042034327965,30.3515915572706,13.9303609021762));
#65875=CARTESIAN_POINT('Ctrl Pts',(-2.50691056537359,30.4561722031845,13.068345948761));
#65876=CARTESIAN_POINT('Ctrl Pts',(-2.41159217086306,30.5089016104533,12.65665943316));
#65877=CARTESIAN_POINT('Ctrl Pts',(2.53672207026418,22.6010701274518,13.3));
#65878=CARTESIAN_POINT('Ctrl Pts',(2.52386596814846,22.6547808871083,13.7475472389172));
#65879=CARTESIAN_POINT('Ctrl Pts',(2.28516242108258,22.7614097926142,14.5627020551058));
#65880=CARTESIAN_POINT('Ctrl Pts',(1.04821201701013,22.9723630473711,15.8230970362253));
#65881=CARTESIAN_POINT('Ctrl Pts',(-1.30163826043596,23.2309895404828,15.8589868213865));
#65882=CARTESIAN_POINT('Ctrl Pts',(-2.79650367489345,23.533893960578,13.5229554773338));
#65883=CARTESIAN_POINT('Ctrl Pts',(-1.75020632631818,23.7966890553668,11.3727757526931));
#65884=CARTESIAN_POINT('Ctrl Pts',(0.100026788420263,24.0222658657341,10.8566282676066));
#65885=CARTESIAN_POINT('Ctrl Pts',(1.58596911863261,24.2127607413429,11.4874877813099));
#65886=CARTESIAN_POINT('Ctrl Pts',(2.27784118097466,24.3849371468287,12.7759298186652));
#65887=CARTESIAN_POINT('Ctrl Pts',(2.14599261285379,24.5396549455458,14.0506824690678));
#65888=CARTESIAN_POINT('Ctrl Pts',(1.49342098412511,24.6776008543935,14.9871469796318));
#65889=CARTESIAN_POINT('Ctrl Pts',(0.475385173604076,24.814339074427,15.4817553369712));
#65890=CARTESIAN_POINT('Ctrl Pts',(-0.770842812967098,24.9650411471909,
15.413615855556));
#65891=CARTESIAN_POINT('Ctrl Pts',(-1.8816802076409,25.1293818886154,14.570924124473));
#65892=CARTESIAN_POINT('Ctrl Pts',(-2.24621461637246,25.3071361639334,13.1059467520125));
#65893=CARTESIAN_POINT('Ctrl Pts',(-1.61366325932767,25.4836327911446,11.747168499655));
#65894=CARTESIAN_POINT('Ctrl Pts',(-0.278378180266116,25.6591480325535,
11.0868932263985));
#65895=CARTESIAN_POINT('Ctrl Pts',(1.17095166640344,25.8339657612004,11.4113524729003));
#65896=CARTESIAN_POINT('Ctrl Pts',(2.09391508043506,26.0083762241633,12.5688636664693));
#65897=CARTESIAN_POINT('Ctrl Pts',(2.0874158269108,26.1826680912139,14.0486955369498));
#65898=CARTESIAN_POINT('Ctrl Pts',(1.15336459345638,26.3571369042277,15.1984251330648));
#65899=CARTESIAN_POINT('Ctrl Pts',(-0.298634256840866,26.5320736766806,
15.5091115507522));
#65900=CARTESIAN_POINT('Ctrl Pts',(-1.63160944640033,26.7077658150152,14.8401215472852));
#65901=CARTESIAN_POINT('Ctrl Pts',(-2.25131622058411,26.8844963732798,13.4725419062569));
#65902=CARTESIAN_POINT('Ctrl Pts',(-1.9059670914065,27.0477020505508,12.1316352867466));
#65903=CARTESIAN_POINT('Ctrl Pts',(-0.979854205581052,27.1972220957301,
11.3101474584682));
#65904=CARTESIAN_POINT('Ctrl Pts',(0.116931174873669,27.3327865136187,11.0664240469857));
#65905=CARTESIAN_POINT('Ctrl Pts',(1.19700060462999,27.4694517064889,11.3906384812928));
#65906=CARTESIAN_POINT('Ctrl Pts',(2.27146199137299,27.6532725125067,12.4789085973207));
#65907=CARTESIAN_POINT('Ctrl Pts',(2.2944534071564,27.8396822715647,14.1613568274049));
#65908=CARTESIAN_POINT('Ctrl Pts',(1.21188254212424,28.0290394905166,15.3070004216219));
#65909=CARTESIAN_POINT('Ctrl Pts',(0.0845872396768884,28.1726048993493,
15.6701949854082));
#65910=CARTESIAN_POINT('Ctrl Pts',(-1.09545910495886,28.3177922830621,15.4348199567659));
#65911=CARTESIAN_POINT('Ctrl Pts',(-2.02084877192932,28.4646665841871,14.6463384527996));
#65912=CARTESIAN_POINT('Ctrl Pts',(-2.45024610790034,28.6132878065287,13.494059057564));
#65913=CARTESIAN_POINT('Ctrl Pts',(-2.24537056320646,28.7804215714648,12.1252219559702));
#65914=CARTESIAN_POINT('Ctrl Pts',(-1.17335673448093,28.966899793215,10.9580237712631));
#65915=CARTESIAN_POINT('Ctrl Pts',(0.558777587586121,29.1736969761794,10.6986804799736));
#65916=CARTESIAN_POINT('Ctrl Pts',(2.36919813842405,29.418962526061,11.7378175469893));
#65917=CARTESIAN_POINT('Ctrl Pts',(2.89725560020412,29.7050532180518,14.2840477585018));
#65918=CARTESIAN_POINT('Ctrl Pts',(0.696448044363527,30.0347471463454,16.3532177295756));
#65919=CARTESIAN_POINT('Ctrl Pts',(-1.76982090953937,30.3159478043037,15.6816271858541));
#65920=CARTESIAN_POINT('Ctrl Pts',(-2.73900717504778,30.5446729887148,14.046826392024));
#65921=CARTESIAN_POINT('Ctrl Pts',(-2.77339105257539,30.6602644219914,13.0943059059134));
#65922=CARTESIAN_POINT('Ctrl Pts',(-2.6710485091933,30.7183585763046,12.640190198649));
#65923=CARTESIAN_POINT('Ctrl Pts',(2.2183610351321,22.5005350637259,13.3));
#65924=CARTESIAN_POINT('Ctrl Pts',(2.20732208326138,22.5484915142731,13.699758215172));
#65925=CARTESIAN_POINT('Ctrl Pts',(2.00027014846976,22.6410090565288,14.4071397348093));
#65926=CARTESIAN_POINT('Ctrl Pts',(0.912554002081777,22.8271444189337,15.5210532308397));
#65927=CARTESIAN_POINT('Ctrl Pts',(-1.15691805263464,23.0546136929354,15.5542757223008));
#65928=CARTESIAN_POINT('Ctrl Pts',(-2.49093046002719,23.3236757288067,13.4873773346461));
#65929=CARTESIAN_POINT('Ctrl Pts',(-1.56109853564162,23.5590329351607,11.5561927120739));
#65930=CARTESIAN_POINT('Ctrl Pts',(0.111714907485613,23.7631934622475,11.0836004070663));
#65931=CARTESIAN_POINT('Ctrl Pts',(1.47049081457418,23.937113829779,11.6547566535498));
#65932=CARTESIAN_POINT('Ctrl Pts',(2.11308441896366,24.0958873357551,12.8401056174219));
#65933=CARTESIAN_POINT('Ctrl Pts',(1.99467970110352,24.239898017344,14.0270799159506));
#65934=CARTESIAN_POINT('Ctrl Pts',(1.38548250386768,24.3693958001383,14.9083990575687));
#65935=CARTESIAN_POINT('Ctrl Pts',(0.423315749518031,24.4989021004607,15.3807411268428));
#65936=CARTESIAN_POINT('Ctrl Pts',(-0.76799412090761,24.6429550384991,15.3208893112581));
#65937=CARTESIAN_POINT('Ctrl Pts',(-1.84600291649318,24.8017913824285,14.5126035235537));
#65938=CARTESIAN_POINT('Ctrl Pts',(-2.21162965654954,24.9758449066832,13.0806552944285));
#65939=CARTESIAN_POINT('Ctrl Pts',(-1.59284740696533,25.1509653949324,11.7285318827829));
#65940=CARTESIAN_POINT('Ctrl Pts',(-0.255089672331717,25.3274441413117,
11.055696404286));
#65941=CARTESIAN_POINT('Ctrl Pts',(1.22362929125862,25.5055533284942,11.375592128919));
#65942=CARTESIAN_POINT('Ctrl Pts',(2.18484293549448,25.685562905358,12.5629954185504));
#65943=CARTESIAN_POINT('Ctrl Pts',(2.18980186105923,25.8677211661319,14.1093087532237));
#65944=CARTESIAN_POINT('Ctrl Pts',(1.21143310986873,26.0522683809189,15.3328638222202));
#65945=CARTESIAN_POINT('Ctrl Pts',(-0.339059659776909,26.239423973137,15.6773824073839));
#65946=CARTESIAN_POINT('Ctrl Pts',(-1.78569333727131,26.4293900673351,14.9656927457296));
#65947=CARTESIAN_POINT('Ctrl Pts',(-2.47416163046515,26.6223483339623,13.4781429424522));
#65948=CARTESIAN_POINT('Ctrl Pts',(-2.10549777162261,26.8021159857552,11.9983797771691));
#65949=CARTESIAN_POINT('Ctrl Pts',(-1.08527208402701,26.9679412463559,11.0798865261764));
#65950=CARTESIAN_POINT('Ctrl Pts',(0.13536334826752,27.1190847834831,10.7992190624231));
#65951=CARTESIAN_POINT('Ctrl Pts',(1.34759162461277,27.2721726601904,11.1535834603927));
#65952=CARTESIAN_POINT('Ctrl Pts',(2.56489813381872,27.4789264362032,12.3683976939296));
#65953=CARTESIAN_POINT('Ctrl Pts',(2.6061432041599,27.6896926752336,14.2700173133308));
#65954=CARTESIAN_POINT('Ctrl Pts',(1.38712717931538,27.904534103112,15.5784431958487));
#65955=CARTESIAN_POINT('Ctrl Pts',(0.10895953963572,28.0677021630343,15.9998907204716));
#65956=CARTESIAN_POINT('Ctrl Pts',(-1.23535153591744,28.2329034487015,15.7412149433557));
#65957=CARTESIAN_POINT('Ctrl Pts',(-2.29471625897426,28.4001240169453,14.8505918592972));
#65958=CARTESIAN_POINT('Ctrl Pts',(-2.79203814947656,28.5693430024324,13.5420011391188));
#65959=CARTESIAN_POINT('Ctrl Pts',(-2.56877406678316,28.7595514723432,11.9828803214993));
#65960=CARTESIAN_POINT('Ctrl Pts',(-1.35822219944082,28.9715360098461,10.6489229561444));
#65961=CARTESIAN_POINT('Ctrl Pts',(0.604663322317292,29.2061196861259,10.3434395952506));
#65962=CARTESIAN_POINT('Ctrl Pts',(2.65874145703642,29.483527190347,11.5076918928945));
#65963=CARTESIAN_POINT('Ctrl Pts',(3.26545304863587,29.8056282097385,14.3719790847457));
#65964=CARTESIAN_POINT('Ctrl Pts',(0.813056733395563,30.1742234622136,16.6938678232326));
#65965=CARTESIAN_POINT('Ctrl Pts',(-1.92333210556604,30.4859835815331,15.9577643257455));
#65966=CARTESIAN_POINT('Ctrl Pts',(-2.9975940068159,30.737754420159,14.1632918818718));
#65967=CARTESIAN_POINT('Ctrl Pts',(-3.0398715397772,30.8643566407983,13.1202658630658));
#65968=CARTESIAN_POINT('Ctrl Pts',(-2.93050484752353,30.9278155421559,12.623720964138));
#65969=CARTESIAN_POINT('Ctrl Pts',(1.9,22.4,13.3));
#65970=CARTESIAN_POINT('Ctrl Pts',(1.89077819837431,22.4422021414379,13.6519691914269));
#65971=CARTESIAN_POINT('Ctrl Pts',(1.71537787585695,22.5206083204434,14.2515774145128));
#65972=CARTESIAN_POINT('Ctrl Pts',(0.776895987153429,22.6819257904964,15.2190094254541));
#65973=CARTESIAN_POINT('Ctrl Pts',(-1.01219784483332,22.8782378453878,15.2495646232149));
#65974=CARTESIAN_POINT('Ctrl Pts',(-2.18535724516091,23.1134574970354,13.4517991919584));
#65975=CARTESIAN_POINT('Ctrl Pts',(-1.37199074496505,23.3213768149546,11.7396096714547));
#65976=CARTESIAN_POINT('Ctrl Pts',(0.123403026550972,23.504121058761,11.3105725465261));
#65977=CARTESIAN_POINT('Ctrl Pts',(1.35501251051576,23.661466918215,11.8220255257895));
#65978=CARTESIAN_POINT('Ctrl Pts',(1.94832765695265,23.8068375246815,12.9042814161785));
#65979=CARTESIAN_POINT('Ctrl Pts',(1.84336678935325,23.9401410891422,14.0034773628334));
#65980=CARTESIAN_POINT('Ctrl Pts',(1.27754402361024,24.0611907458831,14.8296511355055));
#65981=CARTESIAN_POINT('Ctrl Pts',(0.371246325431991,24.1834651264945,15.2797269167144));
#65982=CARTESIAN_POINT('Ctrl Pts',(-0.765145428848119,24.3208689298072,
15.2281627669602));
#65983=CARTESIAN_POINT('Ctrl Pts',(-1.81032562534546,24.4742008762416,14.4542829226342));
#65984=CARTESIAN_POINT('Ctrl Pts',(-2.17704469672661,24.6445536494329,13.0553638368446));
#65985=CARTESIAN_POINT('Ctrl Pts',(-1.57203155460298,24.8182979987203,11.709895265911));
#65986=CARTESIAN_POINT('Ctrl Pts',(-0.23180116439731,24.99574025007,11.0244995821736));
#65987=CARTESIAN_POINT('Ctrl Pts',(1.27630691611381,25.1771408957878,11.3398317849377));
#65988=CARTESIAN_POINT('Ctrl Pts',(2.27577079055389,25.3627495865527,12.5571271706314));
#65989=CARTESIAN_POINT('Ctrl Pts',(2.29218789520766,25.5527742410498,14.1699219694977));
#65990=CARTESIAN_POINT('Ctrl Pts',(1.26950162628108,25.74739985761,15.4673025113756));
#65991=CARTESIAN_POINT('Ctrl Pts',(-0.379485062712953,25.9467742695935,
15.8456532640155));
#65992=CARTESIAN_POINT('Ctrl Pts',(-1.93977722814229,26.1510143196549,15.0912639441738));
#65993=CARTESIAN_POINT('Ctrl Pts',(-2.69700704034618,26.3602002946448,13.4837439786473));
#65994=CARTESIAN_POINT('Ctrl Pts',(-2.30502845183871,26.5565299209596,11.8651242675914));
#65995=CARTESIAN_POINT('Ctrl Pts',(-1.19068996247298,26.7386603969818,10.8496255938845));
#65996=CARTESIAN_POINT('Ctrl Pts',(0.153795521661376,26.9053830533475,10.5320140778605));
#65997=CARTESIAN_POINT('Ctrl Pts',(1.49818264459556,27.0748936138919,10.9165284394926));
#65998=CARTESIAN_POINT('Ctrl Pts',(2.85833427626445,27.3045803598996,12.2578867905387));
#65999=CARTESIAN_POINT('Ctrl Pts',(2.9178330011634,27.5397030789025,14.3786777992568));
#66000=CARTESIAN_POINT('Ctrl Pts',(1.56237181650653,27.7800287157075,15.8498859700755));
#66001=CARTESIAN_POINT('Ctrl Pts',(0.13333183959455,27.9627994267194,16.3295864555349));
#66002=CARTESIAN_POINT('Ctrl Pts',(-1.37524396687603,28.148014614341,16.0476099299455));
#66003=CARTESIAN_POINT('Ctrl Pts',(-2.5685837460192,28.3355814497034,15.0548452657946));
#66004=CARTESIAN_POINT('Ctrl Pts',(-3.13383019105279,28.5253981983361,13.5899432206735));
#66005=CARTESIAN_POINT('Ctrl Pts',(-2.89217757035986,28.7386813732216,11.8405386870284));
#66006=CARTESIAN_POINT('Ctrl Pts',(-1.54308766440071,28.9761722264772,10.3398221410258));
#66007=CARTESIAN_POINT('Ctrl Pts',(0.650549057048467,29.2385423960724,9.98819871052755));
#66008=CARTESIAN_POINT('Ctrl Pts',(2.94828477564879,29.548091854633,11.2775662387998));
#66009=CARTESIAN_POINT('Ctrl Pts',(3.63365049706761,29.9062032014252,14.4599104109895));
#66010=CARTESIAN_POINT('Ctrl Pts',(0.929665422427599,30.3136997780818,17.0345179168896));
#66011=CARTESIAN_POINT('Ctrl Pts',(-2.07684330159272,30.6560193587624,16.2339014656368));
#66012=CARTESIAN_POINT('Ctrl Pts',(-3.25618083858403,30.9308358516032,14.2797573717195));
#66013=CARTESIAN_POINT('Ctrl Pts',(-3.306352026979,31.0684488596052,13.1462258202182));
#66014=CARTESIAN_POINT('Ctrl Pts',(-3.18996118585377,31.1372725080072,12.6072517296268));
#66015=CARTESIAN_POINT('',(2.85,22.7,13.3));
#66016=CARTESIAN_POINT('Ctrl Pts',(-0.969619743608971,35.5250590498763,
10.2301745864681));
#66017=CARTESIAN_POINT('Ctrl Pts',(-0.293405597888406,35.6135359928547,
10.017227865461));
#66018=CARTESIAN_POINT('Ctrl Pts',(1.20310012018456,35.7904514013391,10.0572891405987));
#66019=CARTESIAN_POINT('Ctrl Pts',(2.93390863505459,36.0553071829586,11.48394067231));
#66020=CARTESIAN_POINT('Ctrl Pts',(3.41758282565779,36.319305470682,13.6665663047758));
#66021=CARTESIAN_POINT('Ctrl Pts',(2.45975719166707,36.5820762567064,15.6749533869058));
#66022=CARTESIAN_POINT('Ctrl Pts',(0.481163202010952,36.8432697896237,16.6627535697665));
#66023=CARTESIAN_POINT('Ctrl Pts',(-1.67190062807935,37.1025582194331,16.2252409039492));
#66024=CARTESIAN_POINT('Ctrl Pts',(-3.08306248478425,37.359605173675,14.572269215861));
#66025=CARTESIAN_POINT('Ctrl Pts',(-3.19643759372744,37.6423848448201,12.1766162167722));
#66026=CARTESIAN_POINT('Ctrl Pts',(-1.38811732008393,37.9493821651013,10.154502174276));
#66027=CARTESIAN_POINT('Ctrl Pts',(1.03278567716216,38.2237370964296,10.2682868731901));
#66028=CARTESIAN_POINT('Ctrl Pts',(2.3809218660535,38.4400825676405,11.4276672457298));
#66029=CARTESIAN_POINT('Ctrl Pts',(2.92531221614793,38.6007121886329,12.628817144057));
#66030=CARTESIAN_POINT('Ctrl Pts',(2.89919394194952,38.7596516023286,13.9328342740706));
#66031=CARTESIAN_POINT('Ctrl Pts',(2.1402434917003,38.9692434239079,15.4825527531054));
#66032=CARTESIAN_POINT('Ctrl Pts',(0.0844388902172162,39.2267424133018,
16.4533543876597));
#66033=CARTESIAN_POINT('Ctrl Pts',(-2.12137754341091,39.5031047174653,15.4071077046148));
#66034=CARTESIAN_POINT('Ctrl Pts',(-2.84263724025941,39.7486842815273,13.4542134019695));
#66035=CARTESIAN_POINT('Ctrl Pts',(-2.29285373611436,39.9652776471272,11.7066022813769));
#66036=CARTESIAN_POINT('Ctrl Pts',(-0.809367529129827,40.177402665634,10.6913151614677));
#66037=CARTESIAN_POINT('Ctrl Pts',(0.505559239349309,40.333140300507,10.7738392885579));
#66038=CARTESIAN_POINT('Ctrl Pts',(1.23843792453526,40.4355732287232,11.1503985996136));
#66039=CARTESIAN_POINT('Ctrl Pts',(1.67669838949815,40.5034925168063,11.475947565662));
#66040=CARTESIAN_POINT('Ctrl Pts',(2.28287603261652,40.6213815738627,12.2188580969849));
#66041=CARTESIAN_POINT('Ctrl Pts',(2.53798439367783,40.7870458540183,13.5975998584707));
#66042=CARTESIAN_POINT('Ctrl Pts',(1.77492212034956,40.9815214196383,15.0584075661407));
#66043=CARTESIAN_POINT('Ctrl Pts',(0.307669421971351,41.1717923357691,15.7241021006855));
#66044=CARTESIAN_POINT('Ctrl Pts',(-1.22506403825479,41.3579933663104,15.3538045685215));
#66045=CARTESIAN_POINT('Ctrl Pts',(-2.18442835856201,41.540291349872,14.1430778842092));
#66046=CARTESIAN_POINT('Ctrl Pts',(-2.19211575387567,41.6891193359005,12.8837149285007));
#66047=CARTESIAN_POINT('Ctrl Pts',(-1.79903872344835,41.7917680008934,12.1474870326954));
#66048=CARTESIAN_POINT('Ctrl Pts',(-1.48461936224863,41.8500065969429,11.8006059047461));
#66049=CARTESIAN_POINT('Ctrl Pts',(-0.936263451520069,41.9369461449212,
11.3661693008175));
#66050=CARTESIAN_POINT('Ctrl Pts',(0.120072761527529,42.0658359418734,11.0942972486871));
#66051=CARTESIAN_POINT('Ctrl Pts',(1.43243517464226,42.234704644183,11.6660157935677));
#66052=CARTESIAN_POINT('Ctrl Pts',(2.10042667241831,42.4008672345781,12.9032804607227));
#66053=CARTESIAN_POINT('Ctrl Pts',(1.84785783997348,42.5828304210762,14.4264829178442));
#66054=CARTESIAN_POINT('Ctrl Pts',(0.44228534019957,42.7800073483584,15.4529020688146));
#66055=CARTESIAN_POINT('Ctrl Pts',(-1.37655749427508,42.9922179535626,14.9849431781379));
#66056=CARTESIAN_POINT('Ctrl Pts',(-2.15418937753764,43.2023326687039,13.295902856596));
#66057=CARTESIAN_POINT('Ctrl Pts',(-1.3568352207939,43.4112150248688,11.6324213557684));
#66058=CARTESIAN_POINT('Ctrl Pts',(0.440098590354474,43.6197411074281,11.197323805629));
#66059=CARTESIAN_POINT('Ctrl Pts',(1.6666239589875,43.7939276913608,12.1238487379755));
#66060=CARTESIAN_POINT('Ctrl Pts',(1.96028188226055,43.9339647282883,13.2369884585598));
#66061=CARTESIAN_POINT('Ctrl Pts',(1.76057565116699,44.0745948763178,14.3753735947725));
#66062=CARTESIAN_POINT('Ctrl Pts',(0.601463815507247,44.2517749140429,15.4227810305552));
#66063=CARTESIAN_POINT('Ctrl Pts',(-1.29162186703593,44.4674365769801,15.1369988331886));
#66064=CARTESIAN_POINT('Ctrl Pts',(-2.16357425753909,44.6625228061157,13.6556127826875));
#66065=CARTESIAN_POINT('Ctrl Pts',(-1.87153826486548,44.8361904377402,12.2281811299447));
#66066=CARTESIAN_POINT('Ctrl Pts',(-1.124208757008,44.9620959723648,11.4873485185699));
#66067=CARTESIAN_POINT('Ctrl Pts',(-0.344208843748469,45.0640384861851,
11.2133990437453));
#66068=CARTESIAN_POINT('Ctrl Pts',(0.305542062754602,45.1443340519541,11.1837221225817));
#66069=CARTESIAN_POINT('Ctrl Pts',(0.965600074924294,45.2285945750684,11.3652955927471));
#66070=CARTESIAN_POINT('Ctrl Pts',(1.75770762590764,45.3464019646695,11.9033594103926));
#66071=CARTESIAN_POINT('Ctrl Pts',(2.34064770972088,45.4958733909137,13.0257905767835));
#66072=CARTESIAN_POINT('Ctrl Pts',(2.05691682344594,45.6789904927352,14.5511095312853));
#66073=CARTESIAN_POINT('Ctrl Pts',(0.871285117834535,45.8660473054438,15.6011188018465));
#66074=CARTESIAN_POINT('Ctrl Pts',(-0.744178145769051,46.0572040445543,
15.702809222116));
#66075=CARTESIAN_POINT('Ctrl Pts',(-2.11039561200266,46.2525955949688,14.7696884134947));
#66076=CARTESIAN_POINT('Ctrl Pts',(-2.62495996595091,46.4523253192325,13.1583436840268));
#66077=CARTESIAN_POINT('Ctrl Pts',(-2.22701969031422,46.5884211851561,12.0776096121419));
#66078=CARTESIAN_POINT('Ctrl Pts',(-1.87713189663534,46.657212827205,11.6515692922621));
#66079=CARTESIAN_POINT('Ctrl Pts',(-0.928524254695599,35.7529573111631,
10.4693566435768));
#66080=CARTESIAN_POINT('Ctrl Pts',(-0.302351448403887,35.8349249624316,
10.2712100694345));
#66081=CARTESIAN_POINT('Ctrl Pts',(1.07964142130674,35.9983042873203,10.3077443607092));
#66082=CARTESIAN_POINT('Ctrl Pts',(2.66892271900442,36.2414530879768,11.6170450699432));
#66083=CARTESIAN_POINT('Ctrl Pts',(3.1109355193755,36.4824792190626,13.6096159864436));
#66084=CARTESIAN_POINT('Ctrl Pts',(2.2412653402876,36.7211720735862,15.4341158566646));
#66085=CARTESIAN_POINT('Ctrl Pts',(0.452404820286235,36.9573452503665,16.3276102496121));
#66086=CARTESIAN_POINT('Ctrl Pts',(-1.48645903874779,37.1908337232594,15.9340132840584));
#66087=CARTESIAN_POINT('Ctrl Pts',(-2.75303462194856,37.4214809426201,14.4511194819745));
#66088=CARTESIAN_POINT('Ctrl Pts',(-2.85492986041186,37.6744542905615,12.3079979573691));
#66089=CARTESIAN_POINT('Ctrl Pts',(-1.24193668279672,37.9483231609776,10.5039796610413));
#66090=CARTESIAN_POINT('Ctrl Pts',(0.913112028660612,38.1925516538795,10.604645079803));
#66091=CARTESIAN_POINT('Ctrl Pts',(2.11300131054057,38.3850155279473,11.63525163892));
#66092=CARTESIAN_POINT('Ctrl Pts',(2.59791237230024,38.5278949222772,12.7033537235139));
#66093=CARTESIAN_POINT('Ctrl Pts',(2.57545282267576,38.6692982128313,13.8634999863281));
#66094=CARTESIAN_POINT('Ctrl Pts',(1.90093268976562,38.8558656519239,15.2433560739298));
#66095=CARTESIAN_POINT('Ctrl Pts',(0.0696743896235553,39.0853830840031,
16.1109546339611));
#66096=CARTESIAN_POINT('Ctrl Pts',(-1.90410487343739,39.3324996979054,15.1787107387759));
#66097=CARTESIAN_POINT('Ctrl Pts',(-2.55456593756854,39.5529976676009,13.4263717799337));
#66098=CARTESIAN_POINT('Ctrl Pts',(-2.06165747168906,39.748327985643,11.8495201010784));
#66099=CARTESIAN_POINT('Ctrl Pts',(-0.718798232809231,39.9406424887904,
10.9261681097463));
#66100=CARTESIAN_POINT('Ctrl Pts',(0.48085385964531,40.0827133731717,10.9984774691904));
#66101=CARTESIAN_POINT('Ctrl Pts',(1.15291310828357,40.1765676975719,11.3424147239867));
#66102=CARTESIAN_POINT('Ctrl Pts',(1.555680829885,40.2389142093674,11.6405819896993));
#66103=CARTESIAN_POINT('Ctrl Pts',(2.11498582008125,40.3474355071447,12.3232392027595));
#66104=CARTESIAN_POINT('Ctrl Pts',(2.35530702507243,40.5008571269339,13.5991552068882));
#66105=CARTESIAN_POINT('Ctrl Pts',(1.6475116476446,40.6825591967348,14.9664523143975));
#66106=CARTESIAN_POINT('Ctrl Pts',(0.266043325204939,40.8620650218924,15.6000893188088));
#66107=CARTESIAN_POINT('Ctrl Pts',(-1.19652997111221,41.0395781865116,15.2538100228942));
#66108=CARTESIAN_POINT('Ctrl Pts',(-2.1272252638981,41.2153253649343,14.0915006276765));
#66109=CARTESIAN_POINT('Ctrl Pts',(-2.14149232020009,41.360512507773,12.8631716507578));
#66110=CARTESIAN_POINT('Ctrl Pts',(-1.7577029360263,41.4615792510597,12.136583923261));
#66111=CARTESIAN_POINT('Ctrl Pts',(-1.44811693946317,41.519191370033,11.7921953718333));
#66112=CARTESIAN_POINT('Ctrl Pts',(-0.905905233845331,41.6054687313099,
11.358829834061));
#66113=CARTESIAN_POINT('Ctrl Pts',(0.148783283224247,41.7344084333373,11.080034544991));
#66114=CARTESIAN_POINT('Ctrl Pts',(1.48264268622566,41.905567866661,11.6498940810064));
#66115=CARTESIAN_POINT('Ctrl Pts',(2.17804706649762,42.0762312421305,12.9152113329992));
#66116=CARTESIAN_POINT('Ctrl Pts',(1.9281502881629,42.2656152135407,14.5019643907221));
#66117=CARTESIAN_POINT('Ctrl Pts',(0.454206047228391,42.4740014059576,15.6010773688966));
#66118=CARTESIAN_POINT('Ctrl Pts',(-1.50492058521437,42.7020851652482,15.1190889953041));
#66119=CARTESIAN_POINT('Ctrl Pts',(-2.37393678440876,42.9315346015318,13.2844054826429));
#66120=CARTESIAN_POINT('Ctrl Pts',(-1.51093073900629,43.1629797347666,11.4325359425679));
#66121=CARTESIAN_POINT('Ctrl Pts',(0.499870888212584,43.397023065096,10.9221304640026));
#66122=CARTESIAN_POINT('Ctrl Pts',(1.90249455419702,43.5946859167395,11.9584394585814));
#66123=CARTESIAN_POINT('Ctrl Pts',(2.24947803672872,43.7546603065521,13.226802610543));
#66124=CARTESIAN_POINT('Ctrl Pts',(2.03249683098778,43.9159410443849,14.5338782293896));
#66125=CARTESIAN_POINT('Ctrl Pts',(0.709081435241008,44.1201506791162,15.7540073459432));
#66126=CARTESIAN_POINT('Ctrl Pts',(-1.48517107917157,44.3698059824277,15.4441339572982));
#66127=CARTESIAN_POINT('Ctrl Pts',(-2.51179701745175,44.5961435788324,13.7348300181415));
#66128=CARTESIAN_POINT('Ctrl Pts',(-2.18702749691963,44.7976270138815,12.0762756711685));
#66129=CARTESIAN_POINT('Ctrl Pts',(-1.32803235969944,44.9435697167804,11.210705134577));
#66130=CARTESIAN_POINT('Ctrl Pts',(-0.427955672068899,45.0615747648806,
10.8863098737508));
#66131=CARTESIAN_POINT('Ctrl Pts',(0.322903160144552,45.1544230560825,10.8459404674635));
#66132=CARTESIAN_POINT('Ctrl Pts',(1.08654236719346,45.2517202654121,11.049522088885));
#66133=CARTESIAN_POINT('Ctrl Pts',(2.00430019963811,45.3875248410472,11.6625506339721));
#66134=CARTESIAN_POINT('Ctrl Pts',(2.68332056852154,45.5593334049225,12.9477790937394));
#66135=CARTESIAN_POINT('Ctrl Pts',(2.37029763305347,45.7688203617572,14.6946173751069));
#66136=CARTESIAN_POINT('Ctrl Pts',(1.02903008263469,45.9816339492315,15.8973953661167));
#66137=CARTESIAN_POINT('Ctrl Pts',(-0.79656024254013,46.1977617860478,16.0229620984205));
#66138=CARTESIAN_POINT('Ctrl Pts',(-2.33618804037084,46.4171691651988,14.9835519669358));
#66139=CARTESIAN_POINT('Ctrl Pts',(-2.91868728668747,46.6397983888878,13.190566256523));
#66140=CARTESIAN_POINT('Ctrl Pts',(-2.48421628078386,46.7903156144816,11.9933694045403));
#66141=CARTESIAN_POINT('Ctrl Pts',(-2.10165986920628,46.8660802928157,11.5219695835744));
#66142=CARTESIAN_POINT('Ctrl Pts',(-0.887428765782225,35.9808555724499,
10.7085387006856));
#66143=CARTESIAN_POINT('Ctrl Pts',(-0.311297298919368,36.0563139320087,
10.5251922734079));
#66144=CARTESIAN_POINT('Ctrl Pts',(0.956182722428914,36.2061571733015,10.5581995808197));
#66145=CARTESIAN_POINT('Ctrl Pts',(2.40393680295423,36.427598992995,11.7501494675763));
#66146=CARTESIAN_POINT('Ctrl Pts',(2.8042882130932,36.6456529674432,13.5526656681114));
#66147=CARTESIAN_POINT('Ctrl Pts',(2.02277348890814,36.8602678904659,15.1932783264235));
#66148=CARTESIAN_POINT('Ctrl Pts',(0.42364643856152,37.0714207111093,15.9924669294578));
#66149=CARTESIAN_POINT('Ctrl Pts',(-1.30101744941622,37.2791092270855,15.6427856641674));
#66150=CARTESIAN_POINT('Ctrl Pts',(-2.42300675911287,37.4833567115649,14.3299697480881));
#66151=CARTESIAN_POINT('Ctrl Pts',(-2.51342212709626,37.7065237363028,12.4393796979659));
#66152=CARTESIAN_POINT('Ctrl Pts',(-1.09575604550953,37.947264156854,10.8534571478067));
#66153=CARTESIAN_POINT('Ctrl Pts',(0.793438380159059,38.1613662113293,10.9410032864159));
#66154=CARTESIAN_POINT('Ctrl Pts',(1.84508075502765,38.3299484882543,11.8428360321102));
#66155=CARTESIAN_POINT('Ctrl Pts',(2.27051252845255,38.4550776559217,12.7778903029709));
#66156=CARTESIAN_POINT('Ctrl Pts',(2.251711703402,38.578944823334,13.7941656985855));
#66157=CARTESIAN_POINT('Ctrl Pts',(1.66162188783096,38.74248787994,15.0041593947542));
#66158=CARTESIAN_POINT('Ctrl Pts',(0.0549098890299007,38.9440237547044,
15.7685548802624));
#66159=CARTESIAN_POINT('Ctrl Pts',(-1.68683220346387,39.1618946783455,14.9503137729369));
#66160=CARTESIAN_POINT('Ctrl Pts',(-2.26649463487766,39.3573110536744,13.3985301578978));
#66161=CARTESIAN_POINT('Ctrl Pts',(-1.83046120726377,39.5313783241587,11.9924379207797));
#66162=CARTESIAN_POINT('Ctrl Pts',(-0.628228936488634,39.703882311947,11.1610210580248));
#66163=CARTESIAN_POINT('Ctrl Pts',(0.456148479941315,39.8322864458366,11.2231156498228));
#66164=CARTESIAN_POINT('Ctrl Pts',(1.06738829203189,39.9175621664208,11.5344308483598));
#66165=CARTESIAN_POINT('Ctrl Pts',(1.43466327027188,39.9743359019283,11.8052164137364));
#66166=CARTESIAN_POINT('Ctrl Pts',(1.94709560754598,40.0734894404267,12.4276203085341));
#66167=CARTESIAN_POINT('Ctrl Pts',(2.17262965646704,40.2146683998495,13.6007105553058));
#66168=CARTESIAN_POINT('Ctrl Pts',(1.52010117493962,40.3835969738312,14.8744970626542));
#66169=CARTESIAN_POINT('Ctrl Pts',(0.224417228438533,40.5523377080158,15.4760765369319));
#66170=CARTESIAN_POINT('Ctrl Pts',(-1.16799590396964,40.7211630067128,15.1538154772671));
#66171=CARTESIAN_POINT('Ctrl Pts',(-2.07002216923418,40.8903593799966,14.039923371144));
#66172=CARTESIAN_POINT('Ctrl Pts',(-2.09086888652449,41.0319056796453,12.8426283730148));
#66173=CARTESIAN_POINT('Ctrl Pts',(-1.71636714860424,41.131390501226,12.1256808138265));
#66174=CARTESIAN_POINT('Ctrl Pts',(-1.41161451667769,41.188376143123,11.7837848389202));
#66175=CARTESIAN_POINT('Ctrl Pts',(-0.875547016170588,41.2739913176985,
11.3514903673047));
#66176=CARTESIAN_POINT('Ctrl Pts',(0.177493804920967,41.4029809248012,11.0657718412948));
#66177=CARTESIAN_POINT('Ctrl Pts',(1.53285019780908,41.576431089139,11.633772368445));
#66178=CARTESIAN_POINT('Ctrl Pts',(2.25566746057696,41.751595249683,12.9271422052756));
#66179=CARTESIAN_POINT('Ctrl Pts',(2.00844273635235,41.9484000060053,14.5774458636001));
#66180=CARTESIAN_POINT('Ctrl Pts',(0.466126754257215,42.1679954635567,15.7492526689788));
#66181=CARTESIAN_POINT('Ctrl Pts',(-1.63328367615364,42.4119523769338,15.25323481247));
#66182=CARTESIAN_POINT('Ctrl Pts',(-2.5936841912799,42.6607365343597,13.2729081086898));
#66183=CARTESIAN_POINT('Ctrl Pts',(-1.66502625721867,42.9147444446644,11.2326505293673));
#66184=CARTESIAN_POINT('Ctrl Pts',(0.559643186070704,43.1743050227638,10.6469371223761));
#66185=CARTESIAN_POINT('Ctrl Pts',(2.13836514940656,43.3954441421182,11.7930301791872));
#66186=CARTESIAN_POINT('Ctrl Pts',(2.53867419119688,43.5753558848156,13.2166167625263));
#66187=CARTESIAN_POINT('Ctrl Pts',(2.30441801080858,43.7572872124519,14.6923828640066));
#66188=CARTESIAN_POINT('Ctrl Pts',(0.816699054974774,43.9885264441894,16.0852336613315));
#66189=CARTESIAN_POINT('Ctrl Pts',(-1.67872029130721,44.2721753878753,15.7512690814078));
#66190=CARTESIAN_POINT('Ctrl Pts',(-2.86001977736444,44.5297643515489,13.8140472535956));
#66191=CARTESIAN_POINT('Ctrl Pts',(-2.5025167289738,44.7590635900227,11.9243702123924));
#66192=CARTESIAN_POINT('Ctrl Pts',(-1.53185596239088,44.9250434611961,10.9340617505841));
#66193=CARTESIAN_POINT('Ctrl Pts',(-0.511702500389332,45.0591110435762,
10.5592207037563));
#66194=CARTESIAN_POINT('Ctrl Pts',(0.340264257534502,45.1645120602108,10.5081588123451));
#66195=CARTESIAN_POINT('Ctrl Pts',(1.20748465946262,45.2748459557558,10.733748585023));
#66196=CARTESIAN_POINT('Ctrl Pts',(2.25089277336859,45.428647717425,11.4217418575516));
#66197=CARTESIAN_POINT('Ctrl Pts',(3.02599342732222,45.6227934189313,12.8697676106951));
#66198=CARTESIAN_POINT('Ctrl Pts',(2.683678442661,45.8586502307792,14.8381252189284));
#66199=CARTESIAN_POINT('Ctrl Pts',(1.18677504743485,46.0972205930193,16.1936719303867));
#66200=CARTESIAN_POINT('Ctrl Pts',(-0.848942339311207,46.3383195275414,
16.3431149747252));
#66201=CARTESIAN_POINT('Ctrl Pts',(-2.56198046873903,46.5817427354286,15.197415520377));
#66202=CARTESIAN_POINT('Ctrl Pts',(-3.21241460742404,46.827271458543,13.2227888290192));
#66203=CARTESIAN_POINT('Ctrl Pts',(-2.74141287125351,46.992210043807,11.9091291969388));
#66204=CARTESIAN_POINT('Ctrl Pts',(-2.32618784177721,47.0749477584263,11.3923698748866));
#66205=CARTESIAN_POINT('Ctrl Pts',(-0.846333276868852,36.2087538337368,
10.9477207577944));
#66206=CARTESIAN_POINT('Ctrl Pts',(-0.32024314943485,36.2777029015855,10.7791744773813));
#66207=CARTESIAN_POINT('Ctrl Pts',(0.832724023551092,36.4140100592826,10.8086548009301));
#66208=CARTESIAN_POINT('Ctrl Pts',(2.13895088690405,36.6137448980134,11.8832538652094));
#66209=CARTESIAN_POINT('Ctrl Pts',(2.49764090681091,36.8088267158237,13.4957153497792));
#66210=CARTESIAN_POINT('Ctrl Pts',(1.80428163752868,36.9993637073457,14.9524407961822));
#66211=CARTESIAN_POINT('Ctrl Pts',(0.394888056836802,37.1854961718521,15.6573236093034));
#66212=CARTESIAN_POINT('Ctrl Pts',(-1.11557586008467,37.3673847309119,15.3515580442764));
#66213=CARTESIAN_POINT('Ctrl Pts',(-2.09297889627718,37.5452324805099,14.2088200142016));
#66214=CARTESIAN_POINT('Ctrl Pts',(-2.17191439378068,37.7385931820442,12.5707614385627));
#66215=CARTESIAN_POINT('Ctrl Pts',(-0.949575408222315,37.9462051527305,
11.202934634572));
#66216=CARTESIAN_POINT('Ctrl Pts',(0.673764731657505,38.1301807687792,11.2773614930289));
#66217=CARTESIAN_POINT('Ctrl Pts',(1.57716019951472,38.2748814485611,12.0504204253005));
#66218=CARTESIAN_POINT('Ctrl Pts',(1.94311268460486,38.382260389566,12.8524268824278));
#66219=CARTESIAN_POINT('Ctrl Pts',(1.92797058412824,38.4885914338368,13.724831410843));
#66220=CARTESIAN_POINT('Ctrl Pts',(1.42231108589628,38.6291101079561,14.7649627155785));
#66221=CARTESIAN_POINT('Ctrl Pts',(0.0401453884362414,38.8026644254056,
15.4261551265637));
#66222=CARTESIAN_POINT('Ctrl Pts',(-1.46955953349035,38.9912896587856,14.721916807098));
#66223=CARTESIAN_POINT('Ctrl Pts',(-1.97842333218679,39.161624439748,13.3706885358619));
#66224=CARTESIAN_POINT('Ctrl Pts',(-1.59926494283846,39.3144286626745,12.1353557404812));
#66225=CARTESIAN_POINT('Ctrl Pts',(-0.537659640168033,39.4671221351034,
11.3958740063034));
#66226=CARTESIAN_POINT('Ctrl Pts',(0.431443100237323,39.5818595185013,11.4477538304553));
#66227=CARTESIAN_POINT('Ctrl Pts',(0.981863475780215,39.6585566352696,11.7264469727329));
#66228=CARTESIAN_POINT('Ctrl Pts',(1.31364571065875,39.7097575944895,11.9698508377737));
#66229=CARTESIAN_POINT('Ctrl Pts',(1.77920539501069,39.7995433737088,12.5320014143087));
#66230=CARTESIAN_POINT('Ctrl Pts',(1.98995228786165,39.9284796727651,13.6022659037234));
#66231=CARTESIAN_POINT('Ctrl Pts',(1.39269070223466,40.0846347509277,14.782541810911));
#66232=CARTESIAN_POINT('Ctrl Pts',(0.182791131672126,40.2426103941391,15.3520637550552));
#66233=CARTESIAN_POINT('Ctrl Pts',(-1.13946183682706,40.402747826914,15.0538209316398));
#66234=CARTESIAN_POINT('Ctrl Pts',(-2.01281907457026,40.5653933950589,13.9883461146112));
#66235=CARTESIAN_POINT('Ctrl Pts',(-2.0402454528489,40.7032988515178,12.8220850952719));
#66236=CARTESIAN_POINT('Ctrl Pts',(-1.6750313611822,40.8012017513922,12.1147777043921));
#66237=CARTESIAN_POINT('Ctrl Pts',(-1.37511209389223,40.8575609162131,11.7753743060073));
#66238=CARTESIAN_POINT('Ctrl Pts',(-0.845188798495847,40.9425139040871,
11.3441509005482));
#66239=CARTESIAN_POINT('Ctrl Pts',(0.206204326617689,41.071553416265,11.0515091375987));
#66240=CARTESIAN_POINT('Ctrl Pts',(1.58305770939249,41.2472943116171,11.6176506558837));
#66241=CARTESIAN_POINT('Ctrl Pts',(2.33328785465628,41.4269592572355,12.9390730775521));
#66242=CARTESIAN_POINT('Ctrl Pts',(2.08873518454178,41.63118479847,14.652927336478));
#66243=CARTESIAN_POINT('Ctrl Pts',(0.478047461286037,41.8619895211559,15.8974279690608));
#66244=CARTESIAN_POINT('Ctrl Pts',(-1.76164676709294,42.1218195886195,15.3873806296362));
#66245=CARTESIAN_POINT('Ctrl Pts',(-2.81343159815104,42.3899384671876,13.2614107347368));
#66246=CARTESIAN_POINT('Ctrl Pts',(-1.81912177543106,42.6665091545622,11.0327651161668));
#66247=CARTESIAN_POINT('Ctrl Pts',(0.619415483928814,42.9515869804317,10.3717437807498));
#66248=CARTESIAN_POINT('Ctrl Pts',(2.37423574461608,43.196202367497,11.6276208997929));
#66249=CARTESIAN_POINT('Ctrl Pts',(2.82787034566504,43.3960514630793,13.2064309145094));
#66250=CARTESIAN_POINT('Ctrl Pts',(2.57633919062938,43.598633380519,14.8508874986237));
#66251=CARTESIAN_POINT('Ctrl Pts',(0.924316674708532,43.8569022092627,16.4164599767195));
#66252=CARTESIAN_POINT('Ctrl Pts',(-1.87226950344286,44.1745447933228,16.0584042055174));
#66253=CARTESIAN_POINT('Ctrl Pts',(-3.20824253727711,44.4633851242655,13.8932644890496));
#66254=CARTESIAN_POINT('Ctrl Pts',(-2.81800596102796,44.720500166164,11.7724647536162));
#66255=CARTESIAN_POINT('Ctrl Pts',(-1.73567956508233,44.9065172056118,10.6574183665911));
#66256=CARTESIAN_POINT('Ctrl Pts',(-0.595449328709767,45.0566473222717,
10.2321315337616));
#66257=CARTESIAN_POINT('Ctrl Pts',(0.357625354924448,45.1746010643391,10.1703771572269));
#66258=CARTESIAN_POINT('Ctrl Pts',(1.32842695173177,45.2979716460994,10.417975081161));
#66259=CARTESIAN_POINT('Ctrl Pts',(2.49748534709905,45.4697705938028,11.1809330811311));
#66260=CARTESIAN_POINT('Ctrl Pts',(3.36866628612287,45.68625343294,12.791756127651));
#66261=CARTESIAN_POINT('Ctrl Pts',(2.99705925226852,45.9484800998012,14.98163306275));
#66262=CARTESIAN_POINT('Ctrl Pts',(1.344520012235,46.2128072368071,16.4899484946569));
#66263=CARTESIAN_POINT('Ctrl Pts',(-0.901324436082288,46.4788772690349,
16.6632678510297));
#66264=CARTESIAN_POINT('Ctrl Pts',(-2.78777289710721,46.7463163056586,15.4112790738181));
#66265=CARTESIAN_POINT('Ctrl Pts',(-3.50614192816061,47.0147445281983,13.2550114015154));
#66266=CARTESIAN_POINT('Ctrl Pts',(-2.99860946172314,47.1941044731325,11.8248889893372));
#66267=CARTESIAN_POINT('Ctrl Pts',(-2.55071581434815,47.283815224037,11.2627701661989));
#66268=CARTESIAN_POINT('Ctrl Pts',(0.445846264208625,51.6658477063225,10.1121426167274));
#66269=CARTESIAN_POINT('Ctrl Pts',(1.16404206559057,51.7563468451642,10.2127508125863));
#66270=CARTESIAN_POINT('Ctrl Pts',(2.51084538435324,51.9352746543126,10.9131244582453));
#66271=CARTESIAN_POINT('Ctrl Pts',(3.43546172194773,52.2021181550985,12.9752067851171));
#66272=CARTESIAN_POINT('Ctrl Pts',(2.90016583811925,52.4660706907587,15.1448692652158));
#66273=CARTESIAN_POINT('Ctrl Pts',(1.15108978739344,52.7287973130357,16.5189201188617));
#66274=CARTESIAN_POINT('Ctrl Pts',(-1.05986975257263,52.9899432723208,16.5244632521564));
#66275=CARTESIAN_POINT('Ctrl Pts',(-2.79299924630602,53.2491804520227,15.1779379934512));
#66276=CARTESIAN_POINT('Ctrl Pts',(-3.32480009112557,53.5061795791808,13.0668764085995));
#66277=CARTESIAN_POINT('Ctrl Pts',(-2.48609575586124,53.7512036302333,11.1706159064391));
#66278=CARTESIAN_POINT('Ctrl Pts',(-0.797770401081796,53.9843201289036,
10.185651493995));
#66279=CARTESIAN_POINT('Ctrl Pts',(1.04695880052775,54.2056729305981,10.3005443775845));
#66280=CARTESIAN_POINT('Ctrl Pts',(2.75732496495255,54.4608671974974,11.5896407034103));
#66281=CARTESIAN_POINT('Ctrl Pts',(3.21092349295627,54.7478772279226,14.0799057085922));
#66282=CARTESIAN_POINT('Ctrl Pts',(1.40221873075584,55.0639890763963,16.2154026564162));
#66283=CARTESIAN_POINT('Ctrl Pts',(-1.32826248154208,55.3729279006118,16.1639039679761));
#66284=CARTESIAN_POINT('Ctrl Pts',(-2.46324596201939,55.5801574022457,14.7299387087418));
#66285=CARTESIAN_POINT('Ctrl Pts',(-2.6435839192479,55.6916462498041,13.8546566050136));
#66286=CARTESIAN_POINT('Ctrl Pts',(-2.67320101458777,55.7163812827006,13.6585635500232));
#66287=CARTESIAN_POINT('Ctrl Pts',(-2.68950031358046,55.7472242652351,13.4116438102883));
#66288=CARTESIAN_POINT('Ctrl Pts',(-2.67654859278463,55.7841138257671,13.1156583788531));
#66289=CARTESIAN_POINT('Ctrl Pts',(-2.58516892110096,55.8576484167926,12.5333589951533));
#66290=CARTESIAN_POINT('Ctrl Pts',(-2.04824134124429,56.015649313113,11.3456205112857));
#66291=CARTESIAN_POINT('Ctrl Pts',(-0.173069692310768,56.2537881248067,
10.397914739607));
#66292=CARTESIAN_POINT('Ctrl Pts',(1.88964734427024,56.5084479913319,11.2989850846241));
#66293=CARTESIAN_POINT('Ctrl Pts',(2.60142242705677,56.7341868214723,13.0778682424338));
#66294=CARTESIAN_POINT('Ctrl Pts',(2.14212645018905,56.9329559190759,14.6937475450074));
#66295=CARTESIAN_POINT('Ctrl Pts',(0.809504952860645,57.1274072773428,15.6643722638487));
#66296=CARTESIAN_POINT('Ctrl Pts',(-0.800286605823953,57.3176571401586,
15.6088479390479));
#66297=CARTESIAN_POINT('Ctrl Pts',(-2.00925065186011,57.5038425162973,14.5962951303551));
#66298=CARTESIAN_POINT('Ctrl Pts',(-2.33089364379664,57.6861283245531,13.0859315767866));
#66299=CARTESIAN_POINT('Ctrl Pts',(-1.66868325190088,57.8647115917552,11.7262435341493));
#66300=CARTESIAN_POINT('Ctrl Pts',(-0.335405361119072,58.0398094756416,
11.0746722341866));
#66301=CARTESIAN_POINT('Ctrl Pts',(1.08777266255173,58.2116592038884,11.3777316224606));
#66302=CARTESIAN_POINT('Ctrl Pts',(2.00844471935908,58.3805310808016,12.4732448226105));
#66303=CARTESIAN_POINT('Ctrl Pts',(2.04589361782153,58.505161388625,13.5272553458206));
#66304=CARTESIAN_POINT('Ctrl Pts',(1.80162355774204,58.5874976800848,14.1431016224888));
#66305=CARTESIAN_POINT('Ctrl Pts',(1.57462652991566,58.6421964556724,14.5194599162909));
#66306=CARTESIAN_POINT('Ctrl Pts',(0.921284375875408,58.7555706101121,15.1716196737154));
#66307=CARTESIAN_POINT('Ctrl Pts',(-0.559323486541137,58.9258795698348,
15.4251265913212));
#66308=CARTESIAN_POINT('Ctrl Pts',(-1.98161722775831,59.1381198537348,14.1989325529882));
#66309=CARTESIAN_POINT('Ctrl Pts',(-1.92830754970155,59.3482717047087,12.3391872739581));
#66310=CARTESIAN_POINT('Ctrl Pts',(-0.474337152083153,59.5571963003103,
11.2027925785685));
#66311=CARTESIAN_POINT('Ctrl Pts',(1.32802077288509,59.7657739417265,11.6099790789725));
#66312=CARTESIAN_POINT('Ctrl Pts',(2.15772795610831,59.9748521182681,13.2614463248672));
#66313=CARTESIAN_POINT('Ctrl Pts',(1.40689670059518,60.1852962987321,14.9632314121181));
#66314=CARTESIAN_POINT('Ctrl Pts',(-0.407278733503049,60.3979740857096,
15.468739419225));
#66315=CARTESIAN_POINT('Ctrl Pts',(-1.70421135728494,60.5777470442394,14.5561329060626));
#66316=CARTESIAN_POINT('Ctrl Pts',(-2.04852498716468,60.7234716717298,13.408246526714));
#66317=CARTESIAN_POINT('Ctrl Pts',(-1.90436246834392,60.8460742215266,12.412420236595));
#66318=CARTESIAN_POINT('Ctrl Pts',(-1.42619810349544,60.9391411294724,11.7972487198612));
#66319=CARTESIAN_POINT('Ctrl Pts',(-1.00545093965125,61.0017050399128,11.5236867403454));
#66320=CARTESIAN_POINT('Ctrl Pts',(-0.653343800533873,61.0518521649572,
11.329343969651));
#66321=CARTESIAN_POINT('Ctrl Pts',(0.099998629121662,61.146503828448,11.1375368016581));
#66322=CARTESIAN_POINT('Ctrl Pts',(1.28912570182539,61.2936681364074,11.4604593570168));
#66323=CARTESIAN_POINT('Ctrl Pts',(2.19138559292769,61.4630318554624,12.5750982685794));
#66324=CARTESIAN_POINT('Ctrl Pts',(2.21879758576631,61.642449074206,14.0945176467641));
#66325=CARTESIAN_POINT('Ctrl Pts',(1.28772112801874,61.8256164694219,15.3348576439151));
#66326=CARTESIAN_POINT('Ctrl Pts',(-0.241443755623096,62.0127224705213,
15.7495969807645));
#66327=CARTESIAN_POINT('Ctrl Pts',(-1.73425307349269,62.2039267452204,15.1230719503154));
#66328=CARTESIAN_POINT('Ctrl Pts',(-2.54423592511502,62.3993640676977,13.6800226513326));
#66329=CARTESIAN_POINT('Ctrl Pts',(-2.28296970228244,62.6043950170162,11.9633098075878));
#66330=CARTESIAN_POINT('Ctrl Pts',(-1.38591243097158,62.7460124560898,11.1534718409885));
#66331=CARTESIAN_POINT('Ctrl Pts',(-0.829611386823436,62.8203761132634,
10.9386484300407));
#66332=CARTESIAN_POINT('Ctrl Pts',(0.38002601593105,51.894132922063,10.3452258592843));
#66333=CARTESIAN_POINT('Ctrl Pts',(1.04561055735909,51.9779870683912,10.4375209418931));
#66334=CARTESIAN_POINT('Ctrl Pts',(2.28959663373971,52.1432373900973,11.0839834026683));
#66335=CARTESIAN_POINT('Ctrl Pts',(3.1389126194169,52.3882134746617,12.9768465067893));
#66336=CARTESIAN_POINT('Ctrl Pts',(2.65062121395832,52.6292008894566,14.9578142951044));
#66337=CARTESIAN_POINT('Ctrl Pts',(1.06206603561794,52.8678552946214,16.2062727884347));
#66338=CARTESIAN_POINT('Ctrl Pts',(-0.937078411997912,53.1039875153361,
16.2116698916617));
#66339=CARTESIAN_POINT('Ctrl Pts',(-2.49800482308679,53.3374328297761,14.9994365287431));
#66340=CARTESIAN_POINT('Ctrl Pts',(-2.97559942988575,53.568037876535,13.105315068351));
#66341=CARTESIAN_POINT('Ctrl Pts',(-2.22576011261648,53.7872381782223,11.4087407820391));
#66342=CARTESIAN_POINT('Ctrl Pts',(-0.719211151907584,53.9953106016391,
10.5290335875151));
#66343=CARTESIAN_POINT('Ctrl Pts',(0.924657178006765,54.1925572595333,10.6306634839183));
#66344=CARTESIAN_POINT('Ctrl Pts',(2.44751583241136,54.4197001537148,11.7773150632063));
#66345=CARTESIAN_POINT('Ctrl Pts',(2.85222472287848,54.6749694417843,13.9918788858764));
#66346=CARTESIAN_POINT('Ctrl Pts',(1.24466783780811,54.956241155142,15.8932578850828));
#66347=CARTESIAN_POINT('Ctrl Pts',(-1.18899616424661,55.2316068648696,15.8504376842965));
#66348=CARTESIAN_POINT('Ctrl Pts',(-2.20587709721319,55.4169082924069,14.5699720254287));
#66349=CARTESIAN_POINT('Ctrl Pts',(-2.36822651153772,55.516847918831,13.7855025636774));
#66350=CARTESIAN_POINT('Ctrl Pts',(-2.39493674542547,55.539027045757,13.6097011178693));
#66351=CARTESIAN_POINT('Ctrl Pts',(-2.40975768379484,55.5666954993779,13.3882119714191));
#66352=CARTESIAN_POINT('Ctrl Pts',(-2.39838198229458,55.5998097611757,13.122516874998));
#66353=CARTESIAN_POINT('Ctrl Pts',(-2.3167775359425,55.6658631764742,12.5993804450098));
#66354=CARTESIAN_POINT('Ctrl Pts',(-1.83523332892062,55.8080304714487,11.530273157802));
#66355=CARTESIAN_POINT('Ctrl Pts',(-0.142248222083035,56.0233232803886,
10.6689858858619));
#66356=CARTESIAN_POINT('Ctrl Pts',(1.73948903769928,56.2553659901608,11.4838300332593));
#66357=CARTESIAN_POINT('Ctrl Pts',(2.39836936022397,56.4627627807999,13.1161972427045));
#66358=CARTESIAN_POINT('Ctrl Pts',(1.9777870995906,56.64684408314,14.6138748628466));
#66359=CARTESIAN_POINT('Ctrl Pts',(0.736254230871711,56.8285256399016,15.5252124467261));
#66360=CARTESIAN_POINT('Ctrl Pts',(-0.782492003945809,57.008012802175,15.4791022171478));
#66361=CARTESIAN_POINT('Ctrl Pts',(-1.93927405337162,57.1855130743989,14.5192215493128));
#66362=CARTESIAN_POINT('Ctrl Pts',(-2.25669900564292,57.3612496887774,13.0649459223754));
#66363=CARTESIAN_POINT('Ctrl Pts',(-1.61818130107,57.5354648773718,11.7351894938078));
#66364=CARTESIAN_POINT('Ctrl Pts',(-0.305549112424641,57.7084045570741,
11.0837620750159));
#66365=CARTESIAN_POINT('Ctrl Pts',(1.11991210009554,57.8803206864588,11.3775497551447));
#66366=CARTESIAN_POINT('Ctrl Pts',(2.06072059219382,58.0514829670831,12.4810414041313));
#66367=CARTESIAN_POINT('Ctrl Pts',(2.10725865009378,58.1794875676566,13.5630161536499));
#66368=CARTESIAN_POINT('Ctrl Pts',(1.85801322786466,58.2647543577404,14.2021700051929));
#66369=CARTESIAN_POINT('Ctrl Pts',(1.62445737768668,58.3215872081488,14.5945059340594));
#66370=CARTESIAN_POINT('Ctrl Pts',(0.94710368745052,58.439968768518,15.2795932435486));
#66371=CARTESIAN_POINT('Ctrl Pts',(-0.614371771197201,58.6199556753514,
15.5629719319932));
#66372=CARTESIAN_POINT('Ctrl Pts',(-2.15600600757443,58.8480648658049,14.2620100689544));
#66373=CARTESIAN_POINT('Ctrl Pts',(-2.11995695792847,59.0775462281663,12.2311772197443));
#66374=CARTESIAN_POINT('Ctrl Pts',(-0.523423431696986,59.3090277093448,
10.9551827677584));
#66375=CARTESIAN_POINT('Ctrl Pts',(1.50367428801177,59.5431148830245,11.3898078095394));
#66376=CARTESIAN_POINT('Ctrl Pts',(2.46495145155469,59.780356498564,13.2530761359036));
#66377=CARTESIAN_POINT('Ctrl Pts',(1.62594816896165,60.0212828002207,15.2097164770404));
#66378=CARTESIAN_POINT('Ctrl Pts',(-0.458508601026925,60.2663874533731,
15.813091542949));
#66379=CARTESIAN_POINT('Ctrl Pts',(-1.96939148720944,60.4744806514749,14.7711547587735));
#66380=CARTESIAN_POINT('Ctrl Pts',(-2.3801743425067,60.6434428231889,13.4440484551771));
#66381=CARTESIAN_POINT('Ctrl Pts',(-2.22297758285063,60.7856732537224,12.2876999672974));
#66382=CARTESIAN_POINT('Ctrl Pts',(-1.67447145664554,60.8936360758271,11.5695545665826));
#66383=CARTESIAN_POINT('Ctrl Pts',(-1.18941724923096,60.9661799395199,11.2483368299688));
#66384=CARTESIAN_POINT('Ctrl Pts',(-0.783218346752186,61.024317361992,11.0196557639951));
#66385=CARTESIAN_POINT('Ctrl Pts',(0.0876819560510596,61.1339957656059,
10.7902562013244));
#66386=CARTESIAN_POINT('Ctrl Pts',(1.46612917475685,61.3042633158441,11.1529481660207));
#66387=CARTESIAN_POINT('Ctrl Pts',(2.51651255753311,61.4996775639743,12.4310524210908));
#66388=CARTESIAN_POINT('Ctrl Pts',(2.56024916794277,61.7058918118971,14.1768777154794));
#66389=CARTESIAN_POINT('Ctrl Pts',(1.50471339889892,61.915422008706,15.6025313116502));
#66390=CARTESIAN_POINT('Ctrl Pts',(-0.23171713912405,62.128277794586,16.085063349869));
#66391=CARTESIAN_POINT('Ctrl Pts',(-1.92331879578128,62.3444465989242,15.3866180607013));
#66392=CARTESIAN_POINT('Ctrl Pts',(-2.84145203577105,62.5638933635446,13.7713782437873));
#66393=CARTESIAN_POINT('Ctrl Pts',(-2.55987100019197,62.7924197557714,11.8567130657939));
#66394=CARTESIAN_POINT('Ctrl Pts',(-1.5721280846574,62.9489892365689,10.9569442928862));
#66395=CARTESIAN_POINT('Ctrl Pts',(-0.961374574518973,63.0308340001136,
10.7170354018271));
#66396=CARTESIAN_POINT('Ctrl Pts',(0.314205767653474,52.1224181378033,10.5783091018412));
#66397=CARTESIAN_POINT('Ctrl Pts',(0.927179049127616,52.1996272916182,10.6622910711999));
#66398=CARTESIAN_POINT('Ctrl Pts',(2.06834788312619,52.3512001258821,11.2548423470911));
#66399=CARTESIAN_POINT('Ctrl Pts',(2.84236351688607,52.574308794225,12.9784862284615));
#66400=CARTESIAN_POINT('Ctrl Pts',(2.40107658979739,52.7923310881545,14.770759324993));
#66401=CARTESIAN_POINT('Ctrl Pts',(0.973042283842452,53.0069132762071,15.8936254580078));
#66402=CARTESIAN_POINT('Ctrl Pts',(-0.814287071423194,53.2180317583515,
15.8988765311669));
#66403=CARTESIAN_POINT('Ctrl Pts',(-2.20301039986756,53.4256852075293,14.820935064035));
#66404=CARTESIAN_POINT('Ctrl Pts',(-2.62639876864594,53.6298961738894,13.1437537281026));
#66405=CARTESIAN_POINT('Ctrl Pts',(-1.96542446937171,53.8232727262112,11.6468656576391));
#66406=CARTESIAN_POINT('Ctrl Pts',(-0.640651902733371,54.0063010743747,
10.872415681035));
#66407=CARTESIAN_POINT('Ctrl Pts',(0.802355555485791,54.1794415884684,10.9607825902522));
#66408=CARTESIAN_POINT('Ctrl Pts',(2.13770669987019,54.3785331099324,11.9649894230023));
#66409=CARTESIAN_POINT('Ctrl Pts',(2.49352595280071,54.602061655646,13.9038520631604));
#66410=CARTESIAN_POINT('Ctrl Pts',(1.08711694486039,54.8484932338877,15.5711131137492));
#66411=CARTESIAN_POINT('Ctrl Pts',(-1.04972984695112,55.0902858291273,15.536971400617));
#66412=CARTESIAN_POINT('Ctrl Pts',(-1.94850823240697,55.2536591825681,14.4100053421157));
#66413=CARTESIAN_POINT('Ctrl Pts',(-2.09286910382753,55.3420495878578,13.7163485223411));
#66414=CARTESIAN_POINT('Ctrl Pts',(-2.11667247626317,55.3616728088132,13.5608386857155));
#66415=CARTESIAN_POINT('Ctrl Pts',(-2.13001505400921,55.3861667335208,13.36478013255));
#66416=CARTESIAN_POINT('Ctrl Pts',(-2.12021537180453,55.4155056965844,13.129375371143));
#66417=CARTESIAN_POINT('Ctrl Pts',(-2.04838615078405,55.4740779361559,12.6654018948664));
#66418=CARTESIAN_POINT('Ctrl Pts',(-1.62222531659694,55.6004116297843,11.7149258043184));
#66419=CARTESIAN_POINT('Ctrl Pts',(-0.111426751855292,55.7928584359703,
10.9400570321169));
#66420=CARTESIAN_POINT('Ctrl Pts',(1.58933073112833,56.0022839889897,11.6686749818947));
#66421=CARTESIAN_POINT('Ctrl Pts',(2.19531629339118,56.1913387401275,13.1545262429752));
#66422=CARTESIAN_POINT('Ctrl Pts',(1.81344774899216,56.3607322472041,14.5340021806857));
#66423=CARTESIAN_POINT('Ctrl Pts',(0.663003508882794,56.5296440024604,15.3860526296035));
#66424=CARTESIAN_POINT('Ctrl Pts',(-0.76469740206766,56.6983684641913,15.3493564952476));
#66425=CARTESIAN_POINT('Ctrl Pts',(-1.86929745488312,56.8671836325004,14.4421479682705));
#66426=CARTESIAN_POINT('Ctrl Pts',(-2.1825043674892,57.0363710530016,13.0439602679641));
#66427=CARTESIAN_POINT('Ctrl Pts',(-1.56767935023913,57.2062181629884,11.7441354534662));
#66428=CARTESIAN_POINT('Ctrl Pts',(-0.275692863730203,57.3769996385065,
11.0928519158453));
#66429=CARTESIAN_POINT('Ctrl Pts',(1.15205153763939,57.5489821690291,11.3773678878289));
#66430=CARTESIAN_POINT('Ctrl Pts',(2.11299646502858,57.7224348533646,12.4888379856522));
#66431=CARTESIAN_POINT('Ctrl Pts',(2.16862368236604,57.8538137466882,13.5987769614792));
#66432=CARTESIAN_POINT('Ctrl Pts',(1.91440289798728,57.9420110353959,14.2612383878969));
#66433=CARTESIAN_POINT('Ctrl Pts',(1.67428822545771,58.0009779606252,14.6695519518278));
#66434=CARTESIAN_POINT('Ctrl Pts',(0.972922999025649,58.1243669269237,15.3875668133818));
#66435=CARTESIAN_POINT('Ctrl Pts',(-0.669420055853256,58.314031780868,15.7008172726651));
#66436=CARTESIAN_POINT('Ctrl Pts',(-2.33039478739054,58.5580098778749,14.3250875849206));
#66437=CARTESIAN_POINT('Ctrl Pts',(-2.31160636615539,58.8068207516239,12.1231671655305));
#66438=CARTESIAN_POINT('Ctrl Pts',(-0.572509711310807,59.0608591183793,
10.7075729569483));
#66439=CARTESIAN_POINT('Ctrl Pts',(1.67932780313847,59.3204558243225,11.1696365401063));
#66440=CARTESIAN_POINT('Ctrl Pts',(2.77217494700108,59.5858608788598,13.2447059469399));
#66441=CARTESIAN_POINT('Ctrl Pts',(1.84499963732813,59.8572693017093,15.4562015419629));
#66442=CARTESIAN_POINT('Ctrl Pts',(-0.509738468550788,60.1348008210364,
16.1574436666731));
#66443=CARTESIAN_POINT('Ctrl Pts',(-2.23457161713394,60.3712142587102,14.9861766114844));
#66444=CARTESIAN_POINT('Ctrl Pts',(-2.71182369784871,60.563413974648,13.4798503836404));
#66445=CARTESIAN_POINT('Ctrl Pts',(-2.54159269735736,60.7252722859181,12.1629796979999));
#66446=CARTESIAN_POINT('Ctrl Pts',(-1.92274480979564,60.8481310221818,11.3418604133041));
#66447=CARTESIAN_POINT('Ctrl Pts',(-1.37338355881068,60.930654839127,10.9729869195923));
#66448=CARTESIAN_POINT('Ctrl Pts',(-0.913092892970496,60.9967825590269,
10.7099675583393));
#66449=CARTESIAN_POINT('Ctrl Pts',(0.0753652829804603,61.1214877027638,
10.4429756009906));
#66450=CARTESIAN_POINT('Ctrl Pts',(1.6431326476883,61.3148584952808,10.8454369750245));
#66451=CARTESIAN_POINT('Ctrl Pts',(2.84163952213855,61.5363232724862,12.2870065736023));
#66452=CARTESIAN_POINT('Ctrl Pts',(2.90170075011925,61.7693345495881,14.2592377841948));
#66453=CARTESIAN_POINT('Ctrl Pts',(1.72170566977911,62.0052275479901,15.8702049793853));
#66454=CARTESIAN_POINT('Ctrl Pts',(-0.221990522625003,62.2438331186507,
16.4205297189735));
#66455=CARTESIAN_POINT('Ctrl Pts',(-2.11238451806987,62.484966452628,15.6501641710872));
#66456=CARTESIAN_POINT('Ctrl Pts',(-3.13866814642708,62.7284226593914,13.8627338362421));
#66457=CARTESIAN_POINT('Ctrl Pts',(-2.83677229810149,62.9804444945266,11.7501163239999));
#66458=CARTESIAN_POINT('Ctrl Pts',(-1.75834373834323,63.1519660170479,10.7604167447839));
#66459=CARTESIAN_POINT('Ctrl Pts',(-1.09313776221452,63.2412918869638,10.4954223736136));
#66460=CARTESIAN_POINT('Ctrl Pts',(0.248385519375899,52.3507033535437,10.8113923443982));
#66461=CARTESIAN_POINT('Ctrl Pts',(0.80874754089614,52.4212675148452,10.8870612005067));
#66462=CARTESIAN_POINT('Ctrl Pts',(1.84709913251267,52.5591628616668,11.4257012915141));
#66463=CARTESIAN_POINT('Ctrl Pts',(2.54581441435525,52.7604041137883,12.9801259501337));
#66464=CARTESIAN_POINT('Ctrl Pts',(2.15153196563645,52.9554612868524,14.5837043548816));
#66465=CARTESIAN_POINT('Ctrl Pts',(0.884018532066958,53.1459712577928,15.5809781275808));
#66466=CARTESIAN_POINT('Ctrl Pts',(-0.69149573084848,53.3320760013669,15.5860831706721));
#66467=CARTESIAN_POINT('Ctrl Pts',(-1.90801597664832,53.5139375852825,14.642433599327));
#66468=CARTESIAN_POINT('Ctrl Pts',(-2.27719810740612,53.6917544712438,13.1821923878542));
#66469=CARTESIAN_POINT('Ctrl Pts',(-1.70508882612695,53.8593072742,11.8849905332391));
#66470=CARTESIAN_POINT('Ctrl Pts',(-0.562092653559157,54.0172915471103,
11.215797774555));
#66471=CARTESIAN_POINT('Ctrl Pts',(0.680053932964807,54.1663259174035,11.290901696586));
#66472=CARTESIAN_POINT('Ctrl Pts',(1.82789756732901,54.3373660661498,12.1526637827982));
#66473=CARTESIAN_POINT('Ctrl Pts',(2.13482718272291,54.5291538695076,13.8158252404444));
#66474=CARTESIAN_POINT('Ctrl Pts',(0.929566051912647,54.7407453126335,15.2489683424158));
#66475=CARTESIAN_POINT('Ctrl Pts',(-0.910463529655639,54.948964793385,15.2235051169375));
#66476=CARTESIAN_POINT('Ctrl Pts',(-1.69113936760076,55.0904100727293,14.2500386588026));
#66477=CARTESIAN_POINT('Ctrl Pts',(-1.81751169611734,55.1672512568847,13.6471944810048));
#66478=CARTESIAN_POINT('Ctrl Pts',(-1.83840820710088,55.1843185718696,13.5119762535616));
#66479=CARTESIAN_POINT('Ctrl Pts',(-1.85027242422358,55.2056379676637,13.3413482936807));
#66480=CARTESIAN_POINT('Ctrl Pts',(-1.84204876131448,55.231201631993,13.1362338672878));
#66481=CARTESIAN_POINT('Ctrl Pts',(-1.77999476562559,55.2822926958375,12.7314233447229));
#66482=CARTESIAN_POINT('Ctrl Pts',(-1.40921730427326,55.3927927881198,11.8995784508347));
#66483=CARTESIAN_POINT('Ctrl Pts',(-0.0806052816275569,55.5623935915521,
11.2111281783718));
#66484=CARTESIAN_POINT('Ctrl Pts',(1.43917242455737,55.7492019878187,11.8535199305299));
#66485=CARTESIAN_POINT('Ctrl Pts',(1.99226322655837,55.9199146994551,13.1928552432458));
#66486=CARTESIAN_POINT('Ctrl Pts',(1.64910839839372,56.0746204112681,14.4541294985246));
#66487=CARTESIAN_POINT('Ctrl Pts',(0.589752786893861,56.2307623650192,15.2468928124809));
#66488=CARTESIAN_POINT('Ctrl Pts',(-0.746902800189516,56.3887241262077,
15.2196107733473));
#66489=CARTESIAN_POINT('Ctrl Pts',(-1.79932085639463,56.548854190602,14.3650743872282));
#66490=CARTESIAN_POINT('Ctrl Pts',(-2.10830972933549,56.7114924172259,13.0229746135528));
#66491=CARTESIAN_POINT('Ctrl Pts',(-1.51717739940825,56.876971448605,11.7530814131246));
#66492=CARTESIAN_POINT('Ctrl Pts',(-0.245836615035774,57.0455947199389,
11.1019417566746));
#66493=CARTESIAN_POINT('Ctrl Pts',(1.18419097518321,57.2176436515995,11.377186020513));
#66494=CARTESIAN_POINT('Ctrl Pts',(2.16527233786333,57.393386739646,12.4966345671731));
#66495=CARTESIAN_POINT('Ctrl Pts',(2.22998871463829,57.5281399257198,13.6345377693084));
#66496=CARTESIAN_POINT('Ctrl Pts',(1.97079256810989,57.6192677130515,14.3203067706008));
#66497=CARTESIAN_POINT('Ctrl Pts',(1.72411907322871,57.6803687131016,14.7445979695963));
#66498=CARTESIAN_POINT('Ctrl Pts',(0.998742310600759,57.8087650853294,15.495540383215));
#66499=CARTESIAN_POINT('Ctrl Pts',(-0.724468340509324,58.0081078863845,
15.8386626133371));
#66500=CARTESIAN_POINT('Ctrl Pts',(-2.50478356720666,58.2679548899448,14.3881651008867));
#66501=CARTESIAN_POINT('Ctrl Pts',(-2.50325577438232,58.5360952750815,12.0151571113168));
#66502=CARTESIAN_POINT('Ctrl Pts',(-0.621595990924646,58.8126905274138,
10.4599631461383));
#66503=CARTESIAN_POINT('Ctrl Pts',(1.85498131826514,59.0977967656205,10.9494652706732));
#66504=CARTESIAN_POINT('Ctrl Pts',(3.07939844244746,59.3913652591555,13.2363357579762));
#66505=CARTESIAN_POINT('Ctrl Pts',(2.0640511056946,59.6932558031979,15.7026866068853));
#66506=CARTESIAN_POINT('Ctrl Pts',(-0.56096833607467,60.0032141886998,16.5017957903972));
#66507=CARTESIAN_POINT('Ctrl Pts',(-2.49975174705845,60.2679478659456,15.2011984641953));
#66508=CARTESIAN_POINT('Ctrl Pts',(-3.04347305319073,60.4833851261072,13.5156523121035));
#66509=CARTESIAN_POINT('Ctrl Pts',(-2.86020781186409,60.6648713181137,12.0382594287024));
#66510=CARTESIAN_POINT('Ctrl Pts',(-2.17101816294575,60.8026259685364,11.1141662600256));
#66511=CARTESIAN_POINT('Ctrl Pts',(-1.55734986839041,60.8951297387342,10.6976370092157));
#66512=CARTESIAN_POINT('Ctrl Pts',(-1.04296743918883,60.9692477560618,10.4002793526834));
#66513=CARTESIAN_POINT('Ctrl Pts',(0.0630486099098471,61.1089796399216,
10.0956950006568));
#66514=CARTESIAN_POINT('Ctrl Pts',(1.82013612061974,61.3254536747173,10.5379257840283));
#66515=CARTESIAN_POINT('Ctrl Pts',(3.16676648674395,61.572968980998,12.1429607261137));
#66516=CARTESIAN_POINT('Ctrl Pts',(3.24315233229571,61.8327772872792,14.3415978529102));
#66517=CARTESIAN_POINT('Ctrl Pts',(1.93869794065929,62.0950330872743,16.1378786471204));
#66518=CARTESIAN_POINT('Ctrl Pts',(-0.212263906125961,62.3593884427155,
16.7559960880779));
#66519=CARTESIAN_POINT('Ctrl Pts',(-2.30145024035847,62.6254863063319,15.9137102814732));
#66520=CARTESIAN_POINT('Ctrl Pts',(-3.43588425708311,62.8929519552382,13.9540894286967));
#66521=CARTESIAN_POINT('Ctrl Pts',(-3.11367359601103,63.1684692332818,11.643519582206));
#66522=CARTESIAN_POINT('Ctrl Pts',(-1.94455939202906,63.3549427975269,10.5638891966816));
#66523=CARTESIAN_POINT('Ctrl Pts',(-1.22490094991005,63.4517497738138,10.2738093454001));
#66524=CARTESIAN_POINT('Ctrl Pts',(1.85670933670314,67.8162814825949,10.6678728949504));
#66525=CARTESIAN_POINT('Ctrl Pts',(2.43602197966479,67.9048067130758,11.0772117886178));
#66526=CARTESIAN_POINT('Ctrl Pts',(3.31138477419987,68.0818237056135,12.2930394731503));
#66527=CARTESIAN_POINT('Ctrl Pts',(3.22470059147693,68.3468414640187,14.5358665053979));
#66528=CARTESIAN_POINT('Ctrl Pts',(1.78035101801571,68.6110053286756,16.2437005675216));
#66529=CARTESIAN_POINT('Ctrl Pts',(-0.398931224427797,68.87395706305,16.6986682402629));
#66530=CARTESIAN_POINT('Ctrl Pts',(-2.3843464145878,69.1353372445261,15.7211359742319));
#66531=CARTESIAN_POINT('Ctrl Pts',(-3.34029854038271,69.3948123372156,13.7432675526659));
#66532=CARTESIAN_POINT('Ctrl Pts',(-2.87920489104697,69.652058213363,11.6138171811909));
#66533=CARTESIAN_POINT('Ctrl Pts',(-1.28405859028018,69.8973232110643,10.2856759717977));
#66534=CARTESIAN_POINT('Ctrl Pts',(0.667327379030212,70.1306721384216,10.1534794027043));
#66535=CARTESIAN_POINT('Ctrl Pts',(2.27325538581328,70.3522534623988,11.0739567043829));
#66536=CARTESIAN_POINT('Ctrl Pts',(3.23327615711246,70.6077079139465,12.99126474038));
#66537=CARTESIAN_POINT('Ctrl Pts',(2.53340867575295,70.8950134973084,15.4265265382553));
#66538=CARTESIAN_POINT('Ctrl Pts',(-0.0387874535395751,71.2114494314392,
16.537589845118));
#66539=CARTESIAN_POINT('Ctrl Pts',(-2.46488681075965,71.5207018511086,15.2793708579856));
#66540=CARTESIAN_POINT('Ctrl Pts',(-3.0194423980344,71.822422717759,12.6713480466428));
#66541=CARTESIAN_POINT('Ctrl Pts',(-1.38798471805984,72.1163679385386,10.6399663599959));
#66542=CARTESIAN_POINT('Ctrl Pts',(0.502791661670317,72.3308848888959,10.6231415412111));
#66543=CARTESIAN_POINT('Ctrl Pts',(1.47389601290199,72.4714016735426,11.2093038867376));
#66544=CARTESIAN_POINT('Ctrl Pts',(1.88316787655009,72.5411621865908,11.5944131847211));
#66545=CARTESIAN_POINT('Ctrl Pts',(2.19405691725845,72.6104243783894,12.0586074280405));
#66546=CARTESIAN_POINT('Ctrl Pts',(2.53070804850737,72.7250336026109,12.9195308779709));
#66547=CARTESIAN_POINT('Ctrl Pts',(2.43170974236522,72.883170223474,14.2545730359041));
#66548=CARTESIAN_POINT('Ctrl Pts',(1.29763738145591,73.0820761708995,15.5011320023063));
#66549=CARTESIAN_POINT('Ctrl Pts',(-0.326434740095091,73.2766468129717,
15.7785554159035));
#66550=CARTESIAN_POINT('Ctrl Pts',(-1.7457431520839,73.466995830727,15.0140013277268));
#66551=CARTESIAN_POINT('Ctrl Pts',(-2.37915175472792,73.6532626901171,13.5691967259924));
#66552=CARTESIAN_POINT('Ctrl Pts',(-1.99682535493553,73.8356096858057,12.0728221880452));
#66553=CARTESIAN_POINT('Ctrl Pts',(-0.799077803009128,74.01423239441,11.1483727982448));
#66554=CARTESIAN_POINT('Ctrl Pts',(0.684242025495391,74.1893507431627,11.157075878773));
#66555=CARTESIAN_POINT('Ctrl Pts',(1.82618961641565,74.3612004242115,12.0600879660341));
#66556=CARTESIAN_POINT('Ctrl Pts',(2.16567416243771,74.5300528254682,13.4492130447806));
#66557=CARTESIAN_POINT('Ctrl Pts',(1.58618759125941,74.696183100623,14.73214214359));
#66558=CARTESIAN_POINT('Ctrl Pts',(0.357063385623933,74.8598981792545,15.3762725490012));
#66559=CARTESIAN_POINT('Ctrl Pts',(-0.986547124399861,75.0215158702681,
15.1328704254147));
#66560=CARTESIAN_POINT('Ctrl Pts',(-1.99665026629802,75.1991266012217,14.008047190742));
#66561=CARTESIAN_POINT('Ctrl Pts',(-1.93314910690999,75.3573224550387,12.6189681599128));
#66562=CARTESIAN_POINT('Ctrl Pts',(-1.08666427933318,75.5145655987107,11.63650588873));
#66563=CARTESIAN_POINT('Ctrl Pts',(0.0310153359284624,75.6538155156279,
11.2735856755919));
#66564=CARTESIAN_POINT('Ctrl Pts',(1.2767819779433,75.8101327231011,11.7298773561435));
#66565=CARTESIAN_POINT('Ctrl Pts',(1.97616391758332,75.9664765024184,12.8535243090815));
#66566=CARTESIAN_POINT('Ctrl Pts',(1.83728075366513,76.1232123129657,14.1740596869939));
#66567=CARTESIAN_POINT('Ctrl Pts',(0.911576562100944,76.2807155795881,15.1345764081083));
#66568=CARTESIAN_POINT('Ctrl Pts',(-0.419740331737157,76.4393345343032,
15.3238994606443));
#66569=CARTESIAN_POINT('Ctrl Pts',(-1.59340498562502,76.5994257148169,14.6502009434244));
#66570=CARTESIAN_POINT('Ctrl Pts',(-2.17724646289294,76.7793301999848,13.23842029717));
#66571=CARTESIAN_POINT('Ctrl Pts',(-1.51301420837496,76.9802742295743,11.5954783371621));
#66572=CARTESIAN_POINT('Ctrl Pts',(0.372263544000895,77.2040586660941,10.993031354742));
#66573=CARTESIAN_POINT('Ctrl Pts',(1.71371613042439,77.3853767161158,11.8693209754832));
#66574=CARTESIAN_POINT('Ctrl Pts',(2.07812199344447,77.5067673998192,12.787549358819));
#66575=CARTESIAN_POINT('Ctrl Pts',(2.14159723430654,77.5654598619418,13.254921766966));
#66576=CARTESIAN_POINT('Ctrl Pts',(2.12669180036108,77.6244463050604,13.7293760541241));
#66577=CARTESIAN_POINT('Ctrl Pts',(1.96007099854122,77.698728531597,14.3090748515968));
#66578=CARTESIAN_POINT('Ctrl Pts',(1.40225955808634,77.8188007585235,15.1102220024261));
#66579=CARTESIAN_POINT('Ctrl Pts',(0.250892231981857,77.9712350172198,15.6915466425755));
#66580=CARTESIAN_POINT('Ctrl Pts',(-1.30233550994055,78.1581011855988,15.3843152222005));
#66581=CARTESIAN_POINT('Ctrl Pts',(-2.36017044749241,78.3490726374534,14.1617211117542));
#66582=CARTESIAN_POINT('Ctrl Pts',(-2.44529326530541,78.5442859556217,12.5110277849349));
#66583=CARTESIAN_POINT('Ctrl Pts',(-1.47548070536812,78.7438463495833,11.1269582907925));
#66584=CARTESIAN_POINT('Ctrl Pts',(-0.375471582425882,78.8798352338376,
10.7894481836038));
#66585=CARTESIAN_POINT('Ctrl Pts',(0.175037137306408,78.9485750961381,10.8098385013603));
#66586=CARTESIAN_POINT('Ctrl Pts',(1.6908637574071,68.0447466494469,10.8458773711862));
#66587=CARTESIAN_POINT('Ctrl Pts',(2.22798671957131,68.1267463690719,11.2242837835917));
#66588=CARTESIAN_POINT('Ctrl Pts',(3.03658819127134,68.2901931069568,12.3466170372939));
#66589=CARTESIAN_POINT('Ctrl Pts',(2.95754503485996,68.5334493293176,14.4052783886444));
#66590=CARTESIAN_POINT('Ctrl Pts',(1.63946032851273,68.7745858162928,15.9644933705822));
#66591=CARTESIAN_POINT('Ctrl Pts',(-0.339666919821582,69.01339855444,16.3780848913055));
#66592=CARTESIAN_POINT('Ctrl Pts',(-2.13469030133651,69.2496953306187,15.494721729799));
#66593=CARTESIAN_POINT('Ctrl Pts',(-2.99571041460629,69.4833086246055,13.714185366764));
#66594=CARTESIAN_POINT('Ctrl Pts',(-2.58248382224423,69.7140871144928,11.80376017475));
#66595=CARTESIAN_POINT('Ctrl Pts',(-1.15610395069001,69.9334567944685,10.6154883664123));
#66596=CARTESIAN_POINT('Ctrl Pts',(0.585165556796055,70.1416931193554,10.496838092407));
#66597=CARTESIAN_POINT('Ctrl Pts',(2.01625356645349,70.3390990857319,11.3162524642622));
#66598=CARTESIAN_POINT('Ctrl Pts',(2.87134270658542,70.5664254649136,13.0219942174795));
#66599=CARTESIAN_POINT('Ctrl Pts',(2.25028856230078,70.821902835782,15.1877697105361));
#66600=CARTESIAN_POINT('Ctrl Pts',(-0.0368840815874874,71.1034026808018,
16.178102643529));
#66601=CARTESIAN_POINT('Ctrl Pts',(-2.20012627605475,71.3789882022379,15.0596346097378));
#66602=CARTESIAN_POINT('Ctrl Pts',(-2.6997469456442,71.6487263265457,12.7291745761339));
#66603=CARTESIAN_POINT('Ctrl Pts',(-1.23851386451774,71.9127606817029,10.9014114004134));
#66604=CARTESIAN_POINT('Ctrl Pts',(0.47036207186609,72.1066567862411,10.8817739166415));
#66605=CARTESIAN_POINT('Ctrl Pts',(1.35329158177082,72.2342881946177,11.4129403636492));
#66606=CARTESIAN_POINT('Ctrl Pts',(1.7262508293604,72.2977828683341,11.7629106708839));
#66607=CARTESIAN_POINT('Ctrl Pts',(2.01047124602242,72.3609591527076,12.1858815356422));
#66608=CARTESIAN_POINT('Ctrl Pts',(2.31945641328146,72.4657375867817,12.9723889777793));
#66609=CARTESIAN_POINT('Ctrl Pts',(2.23199454505765,72.6109978916266,14.1988498760847));
#66610=CARTESIAN_POINT('Ctrl Pts',(1.18579312871404,72.7951763476163,15.3563986803355));
#66611=CARTESIAN_POINT('Ctrl Pts',(-0.330275915687068,72.9769418543322,
15.621117764498));
#66612=CARTESIAN_POINT('Ctrl Pts',(-1.67189963570851,73.1564980205229,14.9055500254477));
#66613=CARTESIAN_POINT('Ctrl Pts',(-2.2819418968461,73.334056048206,13.5312995370621));
#66614=CARTESIAN_POINT('Ctrl Pts',(-1.92079877016408,73.509835767522,12.087200469746));
#66615=CARTESIAN_POINT('Ctrl Pts',(-0.757702727053409,73.6840781414891,
11.1790774296483));
#66616=CARTESIAN_POINT('Ctrl Pts',(0.706999028706615,73.8570324079774,11.1787549573379));
#66617=CARTESIAN_POINT('Ctrl Pts',(1.85507178555875,74.0289485500747,12.0743780146905));
#66618=CARTESIAN_POINT('Ctrl Pts',(2.20897506698,74.2000975019401,13.4795202611282));
#66619=CARTESIAN_POINT('Ctrl Pts',(1.6239403103936,74.3707393203612,14.8014365791305));
#66620=CARTESIAN_POINT('Ctrl Pts',(0.350151449131357,74.5411503549865,15.4820174971789));
#66621=CARTESIAN_POINT('Ctrl Pts',(-1.06847454630527,74.7116031039766,15.2371502021208));
#66622=CARTESIAN_POINT('Ctrl Pts',(-2.15809908045976,74.901341833707,14.0458318361661));
#66623=CARTESIAN_POINT('Ctrl Pts',(-2.10481117645329,75.0727931302178,12.5402712220382));
#66624=CARTESIAN_POINT('Ctrl Pts',(-1.18620856045404,75.2451808363801,11.4552688564583));
#66625=CARTESIAN_POINT('Ctrl Pts',(0.046045271720834,75.3992393285853,11.0423615123174));
#66626=CARTESIAN_POINT('Ctrl Pts',(1.44263668058336,75.573922910794,11.5384046732556));
#66627=CARTESIAN_POINT('Ctrl Pts',(2.24340518791338,75.750216614577,12.7973762745375));
#66628=CARTESIAN_POINT('Ctrl Pts',(2.10025705293841,75.9283527132405,14.2992105770565));
#66629=CARTESIAN_POINT('Ctrl Pts',(1.05214770800895,76.1085583193164,15.4081463814273));
#66630=CARTESIAN_POINT('Ctrl Pts',(-0.476886486902698,76.2910335636422,
15.6405602731496));
#66631=CARTESIAN_POINT('Ctrl Pts',(-1.8395781310858,76.4759732412606,14.875277590802));
#66632=CARTESIAN_POINT('Ctrl Pts',(-2.5309286729142,76.684398089858,13.2463448599704));
#66633=CARTESIAN_POINT('Ctrl Pts',(-1.77709762854491,76.9176501442953,11.3328365937584));
#66634=CARTESIAN_POINT('Ctrl Pts',(0.405025589060511,77.1774085192071,10.615426790541));
#66635=CARTESIAN_POINT('Ctrl Pts',(1.96644435451936,77.3874472951319,11.6184892768977));
#66636=CARTESIAN_POINT('Ctrl Pts',(2.3956515391194,77.52768729193,12.6756599141739));
#66637=CARTESIAN_POINT('Ctrl Pts',(2.47317674299433,77.5954091950267,13.2142138706979));
#66638=CARTESIAN_POINT('Ctrl Pts',(2.46030531838649,77.6634044766836,13.7611362800532));
#66639=CARTESIAN_POINT('Ctrl Pts',(2.27368042992308,77.7489112471484,14.4297292960393));
#66640=CARTESIAN_POINT('Ctrl Pts',(1.64001466463188,77.8868236335093,15.354563799779));
#66641=CARTESIAN_POINT('Ctrl Pts',(0.326891597429018,78.0612879022827,16.0285818285653));
#66642=CARTESIAN_POINT('Ctrl Pts',(-1.44289062624411,78.2739747921973,15.6899474839444));
#66643=CARTESIAN_POINT('Ctrl Pts',(-2.6472907269544,78.4899797904215,14.3142674428346));
#66644=CARTESIAN_POINT('Ctrl Pts',(-2.75296903649539,78.7092691128502,12.4607241288402));
#66645=CARTESIAN_POINT('Ctrl Pts',(-1.67950205787869,78.9317853940746,10.9121973695958));
#66646=CARTESIAN_POINT('Ctrl Pts',(-0.464434207018058,79.0822315596954,
10.5331333222611));
#66647=CARTESIAN_POINT('Ctrl Pts',(0.142094012249548,79.1579621925517,10.5520430852575));
#66648=CARTESIAN_POINT('Ctrl Pts',(1.52501817811105,68.2732118162988,11.0238818474219));
#66649=CARTESIAN_POINT('Ctrl Pts',(2.01995145947785,68.348686025068,11.3713557785656));
#66650=CARTESIAN_POINT('Ctrl Pts',(2.76179160834279,68.4985625083001,12.4001946014373));
#66651=CARTESIAN_POINT('Ctrl Pts',(2.69038947824299,68.7200571946162,14.2746902718909));
#66652=CARTESIAN_POINT('Ctrl Pts',(1.49856963900974,68.9381663039099,15.6852861736429));
#66653=CARTESIAN_POINT('Ctrl Pts',(-0.280402615215369,69.1528400458299,
16.0575015423482));
#66654=CARTESIAN_POINT('Ctrl Pts',(-1.88503418808523,69.3640534167114,15.2683074853659));
#66655=CARTESIAN_POINT('Ctrl Pts',(-2.6511222888299,69.5718049119957,13.6851031808621));
#66656=CARTESIAN_POINT('Ctrl Pts',(-2.28576275344152,69.7761160156225,11.9937031683093));
#66657=CARTESIAN_POINT('Ctrl Pts',(-1.02814931109985,69.969590377873,10.9453007610268));
#66658=CARTESIAN_POINT('Ctrl Pts',(0.50300373456189,70.152714100289,10.8401967821098));
#66659=CARTESIAN_POINT('Ctrl Pts',(1.7592517470937,70.3259447090649,11.5585482241415));
#66660=CARTESIAN_POINT('Ctrl Pts',(2.50940925605836,70.5251430158805,13.0527236945793));
#66661=CARTESIAN_POINT('Ctrl Pts',(1.9671684488486,70.7487921742557,14.9490128828172));
#66662=CARTESIAN_POINT('Ctrl Pts',(-0.0349807096354077,70.9953559301642,
15.8186154419401));
#66663=CARTESIAN_POINT('Ctrl Pts',(-1.93536574134987,71.237274553367,14.8398983614901));
#66664=CARTESIAN_POINT('Ctrl Pts',(-2.38005149325401,71.4750299353324,12.7870011056248));
#66665=CARTESIAN_POINT('Ctrl Pts',(-1.08904301097566,71.7091534248672,11.1628564408311));
#66666=CARTESIAN_POINT('Ctrl Pts',(0.437932482061858,71.8824286835865,11.1404062920719));
#66667=CARTESIAN_POINT('Ctrl Pts',(1.23268715063964,71.9971747156927,11.616576840561));
#66668=CARTESIAN_POINT('Ctrl Pts',(1.56933378217072,72.0544035500773,11.9314081570468));
#66669=CARTESIAN_POINT('Ctrl Pts',(1.82688557478638,72.1114939270255,12.3131556432439));
#66670=CARTESIAN_POINT('Ctrl Pts',(2.10820477805556,72.2064415709525,13.0252470775877));
#66671=CARTESIAN_POINT('Ctrl Pts',(2.0322793477501,72.3388255597791,14.1431267162651));
#66672=CARTESIAN_POINT('Ctrl Pts',(1.07394887597216,72.5082765243333,15.2116653583646));
#66673=CARTESIAN_POINT('Ctrl Pts',(-0.33411709127905,72.6772368956925,15.4636801130925));
#66674=CARTESIAN_POINT('Ctrl Pts',(-1.59805611933312,72.8460002103187,14.7970987231688));
#66675=CARTESIAN_POINT('Ctrl Pts',(-2.1847320389643,73.014849406295,13.4934023481318));
#66676=CARTESIAN_POINT('Ctrl Pts',(-1.84477218539263,73.1840618492383,12.1015787514466));
#66677=CARTESIAN_POINT('Ctrl Pts',(-0.716327651097694,73.3539238885679,
11.2097820610519));
#66678=CARTESIAN_POINT('Ctrl Pts',(0.729756031917838,73.524714072792,11.200434035903));
#66679=CARTESIAN_POINT('Ctrl Pts',(1.88395395470186,73.696696675938,12.0886680633468));
#66680=CARTESIAN_POINT('Ctrl Pts',(2.2522759715223,73.8701421784118,13.5098274774756));
#66681=CARTESIAN_POINT('Ctrl Pts',(1.66169302952779,74.0452955400992,14.8707310146709));
#66682=CARTESIAN_POINT('Ctrl Pts',(0.343239512638783,74.2224025307185,15.5877624453568));
#66683=CARTESIAN_POINT('Ctrl Pts',(-1.1504019682107,74.4016903376851,15.341429978827));
#66684=CARTESIAN_POINT('Ctrl Pts',(-2.3195478946215,74.6035570661924,14.0836164815903));
#66685=CARTESIAN_POINT('Ctrl Pts',(-2.2764732459966,74.7882638053972,12.4615742841636));
#66686=CARTESIAN_POINT('Ctrl Pts',(-1.2857528415749,74.9757960740495,11.2740318241866));
#66687=CARTESIAN_POINT('Ctrl Pts',(0.0610752075132027,75.1446631415427,
10.811137349043));
#66688=CARTESIAN_POINT('Ctrl Pts',(1.60849138322342,75.3377130984868,11.3469319903676));
#66689=CARTESIAN_POINT('Ctrl Pts',(2.51064645824345,75.5339567267357,12.7412282399934));
#66690=CARTESIAN_POINT('Ctrl Pts',(2.3632333522117,75.7334931135155,14.4243614671191));
#66691=CARTESIAN_POINT('Ctrl Pts',(1.19271885391695,75.9364010590447,15.6817163547461));
#66692=CARTESIAN_POINT('Ctrl Pts',(-0.534032642068244,76.1427325929813,
15.957221085655));
#66693=CARTESIAN_POINT('Ctrl Pts',(-2.08575127654658,76.3525207677044,15.1003542381797));
#66694=CARTESIAN_POINT('Ctrl Pts',(-2.88461088293549,76.5894659797311,13.2542694227708));
#66695=CARTESIAN_POINT('Ctrl Pts',(-2.04118104871486,76.8550260590165,11.0701948503547));
#66696=CARTESIAN_POINT('Ctrl Pts',(0.437787634120127,77.1507583723203,10.23782222634));
#66697=CARTESIAN_POINT('Ctrl Pts',(2.21917257861433,77.389517874148,11.3676575783123));
#66698=CARTESIAN_POINT('Ctrl Pts',(2.7131810847943,77.5486071840408,12.5637704695288));
#66699=CARTESIAN_POINT('Ctrl Pts',(2.80475625168213,77.6253585281116,13.1735059744297));
#66700=CARTESIAN_POINT('Ctrl Pts',(2.79391883641191,77.7023626483069,13.7928965059823));
#66701=CARTESIAN_POINT('Ctrl Pts',(2.58728986130495,77.7990939626997,14.5503837404819));
#66702=CARTESIAN_POINT('Ctrl Pts',(1.87776977117742,77.9548465084949,15.5989055971319));
#66703=CARTESIAN_POINT('Ctrl Pts',(0.402890962876184,78.1513407873456,16.3656170145551));
#66704=CARTESIAN_POINT('Ctrl Pts',(-1.58344574254767,78.389848398796,15.9955797456884));
#66705=CARTESIAN_POINT('Ctrl Pts',(-2.9344110064164,78.6308869433896,14.4668137739148));
#66706=CARTESIAN_POINT('Ctrl Pts',(-3.06064480768539,78.8742522700789,12.4104204727457));
#66707=CARTESIAN_POINT('Ctrl Pts',(-1.88352341038926,79.1197244385656,10.6974364483992));
#66708=CARTESIAN_POINT('Ctrl Pts',(-0.553396831610237,79.2846278855533,
10.2768184609184));
#66709=CARTESIAN_POINT('Ctrl Pts',(0.109150887192687,79.3673492889653,10.2942476691546));
#66710=CARTESIAN_POINT('Ctrl Pts',(1.35917259881499,68.5016769831508,11.2018863236575));
#66711=CARTESIAN_POINT('Ctrl Pts',(1.81191619938438,68.5706256810641,11.5184277735395));
#66712=CARTESIAN_POINT('Ctrl Pts',(2.48699502541424,68.7069319096434,12.4537721655809));
#66713=CARTESIAN_POINT('Ctrl Pts',(2.42323392162601,68.906665059915,14.1441021551374));
#66714=CARTESIAN_POINT('Ctrl Pts',(1.35767894950677,69.1017467915271,15.4060789767035));
#66715=CARTESIAN_POINT('Ctrl Pts',(-0.221138310609155,69.2922815372198,
15.7369181933908));
#66716=CARTESIAN_POINT('Ctrl Pts',(-1.63537807483394,69.4784115028039,15.0418932409329));
#66717=CARTESIAN_POINT('Ctrl Pts',(-2.3065341630535,69.6603011993856,13.6560209949601));
#66718=CARTESIAN_POINT('Ctrl Pts',(-1.98904168463877,69.8381449167524,12.1836461618684));
#66719=CARTESIAN_POINT('Ctrl Pts',(-0.900194671509688,70.0057239612773,
11.2751131556414));
#66720=CARTESIAN_POINT('Ctrl Pts',(0.420841912327732,70.1637350812228,11.1835554718125));
#66721=CARTESIAN_POINT('Ctrl Pts',(1.5022499277339,70.312790332398,11.8008439840208));
#66722=CARTESIAN_POINT('Ctrl Pts',(2.14747580553131,70.4838605668475,13.0834531716788));
#66723=CARTESIAN_POINT('Ctrl Pts',(1.68404833539643,70.6756815127292,14.7102560550982));
#66724=CARTESIAN_POINT('Ctrl Pts',(-0.0330773376833198,70.8873091795266,
15.4591282403512));
#66725=CARTESIAN_POINT('Ctrl Pts',(-1.67060520664496,71.0955609044962,14.6201621132424));
#66726=CARTESIAN_POINT('Ctrl Pts',(-2.0603560408638,71.3013335441192,12.8448276351158));
#66727=CARTESIAN_POINT('Ctrl Pts',(-0.93957215743358,71.5055461680315,11.4243014812485));
#66728=CARTESIAN_POINT('Ctrl Pts',(0.40550289225763,71.6582005809317,11.3990386675022));
#66729=CARTESIAN_POINT('Ctrl Pts',(1.11208271950847,71.7600612367677,11.8202133174726));
#66730=CARTESIAN_POINT('Ctrl Pts',(1.41241673498102,71.8110242318205,12.0999056432097));
#66731=CARTESIAN_POINT('Ctrl Pts',(1.64329990355035,71.8620287013435,12.4404297508457));
#66732=CARTESIAN_POINT('Ctrl Pts',(1.89695314282964,71.9471455551232,13.0781051773961));
#66733=CARTESIAN_POINT('Ctrl Pts',(1.83256415044253,72.0666532279316,14.0874035564457));
#66734=CARTESIAN_POINT('Ctrl Pts',(0.962104623230294,72.2213767010501,15.0669320363937));
#66735=CARTESIAN_POINT('Ctrl Pts',(-0.337958266871026,72.377531937053,15.3062424616871));
#66736=CARTESIAN_POINT('Ctrl Pts',(-1.52421260295774,72.5355024001146,14.6886474208897));
#66737=CARTESIAN_POINT('Ctrl Pts',(-2.08752218108247,72.6956427643839,13.4555051592014));
#66738=CARTESIAN_POINT('Ctrl Pts',(-1.76874560062118,72.8582879309545,12.1159570331473));
#66739=CARTESIAN_POINT('Ctrl Pts',(-0.674952575141974,73.0237696356469,
11.2404866924554));
#66740=CARTESIAN_POINT('Ctrl Pts',(0.752513035129063,73.1923957376067,11.2221131144679));
#66741=CARTESIAN_POINT('Ctrl Pts',(1.91283612384496,73.3644448018013,12.1029581120033));
#66742=CARTESIAN_POINT('Ctrl Pts',(2.29557687606458,73.5401868548836,13.540134693823));
#66743=CARTESIAN_POINT('Ctrl Pts',(1.69944574866197,73.7198517598374,14.9400254502113));
#66744=CARTESIAN_POINT('Ctrl Pts',(0.336327576146208,73.9036547064504,15.6935073935344));
#66745=CARTESIAN_POINT('Ctrl Pts',(-1.2323293901161,74.0917775713935,15.4457097555331));
#66746=CARTESIAN_POINT('Ctrl Pts',(-2.48099670878324,74.3057722986777,14.1214011270144));
#66747=CARTESIAN_POINT('Ctrl Pts',(-2.44813531553989,74.5037344805762,12.382877346289));
#66748=CARTESIAN_POINT('Ctrl Pts',(-1.38529712269576,74.7064113117189,11.0927947919148));
#66749=CARTESIAN_POINT('Ctrl Pts',(0.0761051433055752,74.8900869545002,
10.5799131857687));
#66750=CARTESIAN_POINT('Ctrl Pts',(1.77434608586349,75.1015032861798,11.1554593074796));
#66751=CARTESIAN_POINT('Ctrl Pts',(2.77788772857351,75.3176968388944,12.6850802054493));
#66752=CARTESIAN_POINT('Ctrl Pts',(2.62620965148495,75.5386335137904,14.5495123571817));
#66753=CARTESIAN_POINT('Ctrl Pts',(1.33328999982496,75.7642437987729,15.955286328065));
#66754=CARTESIAN_POINT('Ctrl Pts',(-0.591178797233786,75.9944316223205,
16.2738818981605));
#66755=CARTESIAN_POINT('Ctrl Pts',(-2.33192442200736,76.2290682941482,15.3254308855573));
#66756=CARTESIAN_POINT('Ctrl Pts',(-3.23829309295676,76.4945338696043,13.2621939855711));
#66757=CARTESIAN_POINT('Ctrl Pts',(-2.30526446888481,76.7924019737375,10.8075531069511));
#66758=CARTESIAN_POINT('Ctrl Pts',(0.470549679179745,77.1241082254333,9.86021766213912));
#66759=CARTESIAN_POINT('Ctrl Pts',(2.4719008027093,77.3915884531642,11.1168258797268));
#66760=CARTESIAN_POINT('Ctrl Pts',(3.03071063046922,77.5695270761517,12.4518810248836));
#66761=CARTESIAN_POINT('Ctrl Pts',(3.13633576036993,77.6553078611967,13.1327980781616));
#66762=CARTESIAN_POINT('Ctrl Pts',(3.12753235443733,77.74132081993,13.8246567319115));
#66763=CARTESIAN_POINT('Ctrl Pts',(2.90089929268681,77.8492766782512,14.6710381849245));
#66764=CARTESIAN_POINT('Ctrl Pts',(2.11552487772295,78.0228693834808,15.8432473944847));
#66765=CARTESIAN_POINT('Ctrl Pts',(0.478890328323348,78.2413936724085,16.7026522005448));
#66766=CARTESIAN_POINT('Ctrl Pts',(-1.72400085885123,78.5057220053945,16.3012120074322));
#66767=CARTESIAN_POINT('Ctrl Pts',(-3.22153128587838,78.7717940963577,14.6193601049952));
#66768=CARTESIAN_POINT('Ctrl Pts',(-3.36832057887537,79.0392354273075,12.360116816651));
#66769=CARTESIAN_POINT('Ctrl Pts',(-2.08754476289982,79.3076634830567,10.4826755272027));
#66770=CARTESIAN_POINT('Ctrl Pts',(-0.642359456202413,79.4870242114111,
10.0205035995757));
#66771=CARTESIAN_POINT('Ctrl Pts',(0.0762077621358257,79.576736385379,10.0364522530518));
#66772=CARTESIAN_POINT('Ctrl Pts',(2.81131480190565,83.9588917569221,11.7304854175133));
#66773=CARTESIAN_POINT('Ctrl Pts',(3.1634734059473,84.0490914904875,12.3617083701036));
#66774=CARTESIAN_POINT('Ctrl Pts',(3.41927311572191,84.2277460141943,13.8547319648058));
#66775=CARTESIAN_POINT('Ctrl Pts',(2.33912418555997,84.4943504633577,15.8372825840002));
#66776=CARTESIAN_POINT('Ctrl Pts',(0.287239187875634,84.7583831881601,16.7254887171579));
#66777=CARTESIAN_POINT('Ctrl Pts',(-1.86632053509874,85.0211986207285,16.1651191296993));
#66778=CARTESIAN_POINT('Ctrl Pts',(-3.21132830161042,85.2824397306322,14.4088646646408));
#66779=CARTESIAN_POINT('Ctrl Pts',(-3.18862357503074,85.5417678794362,12.2116117870217));
#66780=CARTESIAN_POINT('Ctrl Pts',(-1.83388297336382,85.7988641651152,10.5121773355353));
#66781=CARTESIAN_POINT('Ctrl Pts',(0.501237119890374,86.0816969064778,9.94806983576265));
#66782=CARTESIAN_POINT('Ctrl Pts',(2.3976931384394,86.3329225326326,11.0853724677802));
#66783=CARTESIAN_POINT('Ctrl Pts',(3.04292942468987,86.5533961798783,12.7795112871806));
#66784=CARTESIAN_POINT('Ctrl Pts',(2.92206733122934,86.7718730917204,14.5706524524003));
#66785=CARTESIAN_POINT('Ctrl Pts',(1.32567383401337,87.041052574509,16.3290287773339));
#66786=CARTESIAN_POINT('Ctrl Pts',(-1.47145643355607,87.3572972781939,16.1899578223516));
#66787=CARTESIAN_POINT('Ctrl Pts',(-3.08216932414845,87.6663565997973,13.9789898804522));
#66788=CARTESIAN_POINT('Ctrl Pts',(-2.47216016580187,87.942769012737,11.6185629897703));
#66789=CARTESIAN_POINT('Ctrl Pts',(-0.690694897967686,88.1883927916437,
10.5383284001373));
#66790=CARTESIAN_POINT('Ctrl Pts',(1.13002648557816,88.4050238387048,10.747872608232));
#66791=CARTESIAN_POINT('Ctrl Pts',(2.40770993731236,88.6171836897901,12.0115089895042));
#66792=CARTESIAN_POINT('Ctrl Pts',(2.63267941973996,88.8248658396074,13.7554790818738));
#66793=CARTESIAN_POINT('Ctrl Pts',(1.75537245676262,89.0280911225172,15.2362829583177));
#66794=CARTESIAN_POINT('Ctrl Pts',(0.186729728072551,89.2269139728645,15.8489582981416));
#66795=CARTESIAN_POINT('Ctrl Pts',(-1.39147934974809,89.4214132646649,15.3763700465788));
#66796=CARTESIAN_POINT('Ctrl Pts',(-2.32347814117571,89.6117006625855,14.0612378074417));
#66797=CARTESIAN_POINT('Ctrl Pts',(-2.24973188901709,89.7979186483429,12.4855872732891));
#66798=CARTESIAN_POINT('Ctrl Pts',(-1.24305608263045,89.9802295684301,11.3145613956799));
#66799=CARTESIAN_POINT('Ctrl Pts',(0.240233047129281,90.1588265301917,11.0178176751031));
#66800=CARTESIAN_POINT('Ctrl Pts',(1.56532538871952,90.3339330312789,11.6840101966434));
#66801=CARTESIAN_POINT('Ctrl Pts',(2.18729149046849,90.505783787506,12.9997555342965));
#66802=CARTESIAN_POINT('Ctrl Pts',(1.87494079047942,90.6746486932259,14.395446589982));
#66803=CARTESIAN_POINT('Ctrl Pts',(0.784888113405734,90.8408045247825,15.2867363064573));
#66804=CARTESIAN_POINT('Ctrl Pts',(-0.600743943724048,91.0045575052185,
15.3198072369973));
#66805=CARTESIAN_POINT('Ctrl Pts',(-1.70177211459418,91.1662251260324,14.5004567628948));
#66806=CARTESIAN_POINT('Ctrl Pts',(-2.01714312898682,91.3083684314537,13.3429961213115));
#66807=CARTESIAN_POINT('Ctrl Pts',(-1.65649172539696,91.467107854453,12.0840708518216));
#66808=CARTESIAN_POINT('Ctrl Pts',(-0.532550109112778,91.6246713686028,
11.2747192128877));
#66809=CARTESIAN_POINT('Ctrl Pts',(0.932547456212629,91.7988368784177,11.4993881399202));
#66810=CARTESIAN_POINT('Ctrl Pts',(1.84228482993564,91.9552567777171,12.4572187451289));
#66811=CARTESIAN_POINT('Ctrl Pts',(1.9721115764305,92.111714941055,13.7771894871907));
#66812=CARTESIAN_POINT('Ctrl Pts',(1.25989227087951,92.2685707605075,14.8984729993988));
#66813=CARTESIAN_POINT('Ctrl Pts',(0.00333932959659818,92.4262004921002,
15.348492069359));
#66814=CARTESIAN_POINT('Ctrl Pts',(-1.2749231585388,92.5849565243759,14.9263720564591));
#66815=CARTESIAN_POINT('Ctrl Pts',(-2.02797557135136,92.7451870109718,13.7999461577328));
#66816=CARTESIAN_POINT('Ctrl Pts',(-1.92439385153347,92.9252507192101,12.2749837865247));
#66817=CARTESIAN_POINT('Ctrl Pts',(-0.598169095806888,93.1263804160157,
11.0929087972298));
#66818=CARTESIAN_POINT('Ctrl Pts',(1.36056420078383,93.3503628519224,11.4015256735229));
#66819=CARTESIAN_POINT('Ctrl Pts',(2.30107078704159,93.560499426661,12.9987178470627));
#66820=CARTESIAN_POINT('Ctrl Pts',(1.90268123985577,93.7558063742613,14.6070907964034));
#66821=CARTESIAN_POINT('Ctrl Pts',(0.712823826060705,93.9351257409999,15.5472965779981));
#66822=CARTESIAN_POINT('Ctrl Pts',(-0.838406291108695,94.1181965624792,
15.5576480364145));
#66823=CARTESIAN_POINT('Ctrl Pts',(-2.09367889856679,94.3052082155816,14.5919591474277));
#66824=CARTESIAN_POINT('Ctrl Pts',(-2.49940843490071,94.4963211079793,13.0251281454885));
#66825=CARTESIAN_POINT('Ctrl Pts',(-1.84207682216284,94.6916699268768,11.5069054891674));
#66826=CARTESIAN_POINT('Ctrl Pts',(-0.324467363129059,94.8958280351608,
10.67837767433));
#66827=CARTESIAN_POINT('Ctrl Pts',(0.854984362619392,95.0365675621011,10.8955737776502));
#66828=CARTESIAN_POINT('Ctrl Pts',(1.35943926359463,95.1100701719084,11.2003610085549));
#66829=CARTESIAN_POINT('Ctrl Pts',(2.5854520276638,84.1873662167992,11.8188762531224));
#66830=CARTESIAN_POINT('Ctrl Pts',(2.91253206383163,84.2709353426817,12.4032348828803));
#66831=CARTESIAN_POINT('Ctrl Pts',(3.14915586599972,84.4359195989222,13.7819068115739));
#66832=CARTESIAN_POINT('Ctrl Pts',(2.15807315015206,84.6806566806843,15.6020916097792));
#66833=CARTESIAN_POINT('Ctrl Pts',(0.285068220968175,84.9216996807521,16.413348807361));
#66834=CARTESIAN_POINT('Ctrl Pts',(-1.67109844695777,85.160415163267,15.9047677567488));
#66835=CARTESIAN_POINT('Ctrl Pts',(-2.88744692882538,85.396612122941,14.3171209916001));
#66836=CARTESIAN_POINT('Ctrl Pts',(-2.86740715724632,85.6301207841428,12.3386894762662));
#66837=CARTESIAN_POINT('Ctrl Pts',(-1.65225590824352,85.860792556601,10.8136250694661));
#66838=CARTESIAN_POINT('Ctrl Pts',(0.436403417431028,86.1137925878981,10.3085700292359));
#66839=CARTESIAN_POINT('Ctrl Pts',(2.12820626833387,86.3378901386587,11.3228458190353));
#66840=CARTESIAN_POINT('Ctrl Pts',(2.70362696673639,86.5342434618883,12.8312527502471));
#66841=CARTESIAN_POINT('Ctrl Pts',(2.5969382753804,86.7286734444469,14.4252978231867));
#66842=CARTESIAN_POINT('Ctrl Pts',(1.17810109142946,86.9680636529594,15.9898183410281));
#66843=CARTESIAN_POINT('Ctrl Pts',(-1.31035803152768,87.2494235126238,15.8682322153034));
#66844=CARTESIAN_POINT('Ctrl Pts',(-2.74839274372567,87.5248733235881,13.899654818273));
#66845=CARTESIAN_POINT('Ctrl Pts',(-2.20647747994194,87.7720165816171,11.7883563528541));
#66846=CARTESIAN_POINT('Ctrl Pts',(-0.608731181166276,87.9925368752317,
10.8159473053283));
#66847=CARTESIAN_POINT('Ctrl Pts',(1.03336076441061,88.1878849652216,11.0018719634053));
#66848=CARTESIAN_POINT('Ctrl Pts',(2.19404375918698,88.3802174652576,12.1448397907251));
#66849=CARTESIAN_POINT('Ctrl Pts',(2.40320971567541,88.5696601920862,13.7349977865651));
#66850=CARTESIAN_POINT('Ctrl Pts',(1.60121716602805,88.756357255753,15.097533337494));
#66851=CARTESIAN_POINT('Ctrl Pts',(0.150600329632758,88.9404760425103,15.6695519202184));
#66852=CARTESIAN_POINT('Ctrl Pts',(-1.32532063886921,89.1221914699639,15.2334970850425));
#66853=CARTESIAN_POINT('Ctrl Pts',(-2.20954062082533,89.3017028467093,13.9966386823743));
#66854=CARTESIAN_POINT('Ctrl Pts',(-2.14615455673499,89.4792262135844,12.4944725429736));
#66855=CARTESIAN_POINT('Ctrl Pts',(-1.18159272372089,89.6549805577111,11.3608275948985));
#66856=CARTESIAN_POINT('Ctrl Pts',(0.263464546250137,89.8292040840662,11.0633309231916));
#66857=CARTESIAN_POINT('Ctrl Pts',(1.57592204643969,90.002150022639,11.7131990761825));
#66858=CARTESIAN_POINT('Ctrl Pts',(2.2066228743119,90.174067094111,13.0250484964761));
#66859=CARTESIAN_POINT('Ctrl Pts',(1.90011809253171,90.3452248620228,14.441461025335));
#66860=CARTESIAN_POINT('Ctrl Pts',(0.787690164230864,90.5158848987094,15.3651514375489));
#66861=CARTESIAN_POINT('Ctrl Pts',(-0.65374675169598,90.6863230737345,15.4110429139321));
#66862=CARTESIAN_POINT('Ctrl Pts',(-1.82192680704175,90.8568112840542,14.557063743915));
#66863=CARTESIAN_POINT('Ctrl Pts',(-2.16924526933698,91.0086416664991,13.3239025695316));
#66864=CARTESIAN_POINT('Ctrl Pts',(-1.79137319025143,91.1799469073033,11.9627293492403));
#66865=CARTESIAN_POINT('Ctrl Pts',(-0.573590439104622,91.3520233928302,
11.06642807203));
#66866=CARTESIAN_POINT('Ctrl Pts',(1.04905466587743,91.544670528724,11.2989185145622));
#66867=CARTESIAN_POINT('Ctrl Pts',(2.07539198860986,91.7194272837472,12.3590436946813));
#66868=CARTESIAN_POINT('Ctrl Pts',(2.23623694555617,91.8958025280184,13.8450315151429));
#66869=CARTESIAN_POINT('Ctrl Pts',(1.43969013104392,92.0740242729069,15.1265597720918));
#66870=CARTESIAN_POINT('Ctrl Pts',(0.00790787849180596,92.2543203617113,
15.6550412764804));
#66871=CARTESIAN_POINT('Ctrl Pts',(-1.4663543163428,92.4368930058903,15.183803995202));
#66872=CARTESIAN_POINT('Ctrl Pts',(-2.3478777074049,92.6219321531392,13.8915311332495));
#66873=CARTESIAN_POINT('Ctrl Pts',(-2.24421352307133,92.8304711337829,12.1247829321979));
#66874=CARTESIAN_POINT('Ctrl Pts',(-0.717840456061674,93.0638544450115,
10.7397389347576));
#66875=CARTESIAN_POINT('Ctrl Pts',(1.55753455888578,93.3237562683135,11.0790571099927));
#66876=CARTESIAN_POINT('Ctrl Pts',(2.66050638885144,93.5670930898916,12.9199648922052));
#66877=CARTESIAN_POINT('Ctrl Pts',(2.21453464333129,93.7924946455065,14.7791660858403));
#66878=CARTESIAN_POINT('Ctrl Pts',(0.85454209279392,93.998641329072,15.8694668344574));
#66879=CARTESIAN_POINT('Ctrl Pts',(-0.919977059355176,94.208104937822,15.8930508439885));
#66880=CARTESIAN_POINT('Ctrl Pts',(-2.35489039484447,94.420895720329,14.8032782782973));
#66881=CARTESIAN_POINT('Ctrl Pts',(-2.82392567654851,94.6370014294129,13.0344450229515));
#66882=CARTESIAN_POINT('Ctrl Pts',(-2.09501575230247,94.8563877686733,11.3256031638159));
#66883=CARTESIAN_POINT('Ctrl Pts',(-0.40807524298053,95.0839772241254,10.3935981604164));
#66884=CARTESIAN_POINT('Ctrl Pts',(0.897190420009427,95.2396054419005,10.6278613760455));
#66885=CARTESIAN_POINT('Ctrl Pts',(1.45434235785663,95.3205220683781,10.9601002251437));
#66886=CARTESIAN_POINT('Ctrl Pts',(2.35958925342194,84.4158406766762,11.9072670887315));
#66887=CARTESIAN_POINT('Ctrl Pts',(2.66159072171595,84.4927791948759,12.444761395657));
#66888=CARTESIAN_POINT('Ctrl Pts',(2.87903861627751,84.6440931836499,13.7090816583421));
#66889=CARTESIAN_POINT('Ctrl Pts',(1.97702211474414,84.866962898011,15.3669006355582));
#66890=CARTESIAN_POINT('Ctrl Pts',(0.282897254060713,85.0850161733442,16.1012088975638));
#66891=CARTESIAN_POINT('Ctrl Pts',(-1.47587635881681,85.2996317058054,15.6444163837983));
#66892=CARTESIAN_POINT('Ctrl Pts',(-2.56356555604033,85.5107845152498,14.2253773185593));
#66893=CARTESIAN_POINT('Ctrl Pts',(-2.5461907394619,85.7184736888495,12.4657671655105));
#66894=CARTESIAN_POINT('Ctrl Pts',(-1.47062884312324,85.9227209480869,11.1150728033969));
#66895=CARTESIAN_POINT('Ctrl Pts',(0.371569714971683,86.1458882693185,10.6690702227092));
#66896=CARTESIAN_POINT('Ctrl Pts',(1.85871939822834,86.3428577446849,11.5603191702903));
#66897=CARTESIAN_POINT('Ctrl Pts',(2.36432450878294,86.5150907438982,12.8829942133133));
#66898=CARTESIAN_POINT('Ctrl Pts',(2.27180921953146,86.6854737971734,14.2799431939731));
#66899=CARTESIAN_POINT('Ctrl Pts',(1.03052834884555,86.8950747314099,15.6506079047223));
#66900=CARTESIAN_POINT('Ctrl Pts',(-1.14925962949929,87.1415497470537,15.5465066082551));
#66901=CARTESIAN_POINT('Ctrl Pts',(-2.41461616330291,87.383390047379,13.8203197560938));
#66902=CARTESIAN_POINT('Ctrl Pts',(-1.94079479408201,87.6012641504972,11.9581497159379));
#66903=CARTESIAN_POINT('Ctrl Pts',(-0.526767464364877,87.7966809588198,
11.0935662105192));
#66904=CARTESIAN_POINT('Ctrl Pts',(0.936695043243057,87.9707460917385,11.2558713185787));
#66905=CARTESIAN_POINT('Ctrl Pts',(1.98037758106161,88.1432512407249,12.2781705919459));
#66906=CARTESIAN_POINT('Ctrl Pts',(2.17374001161086,88.3144545445653,13.7145164912566));
#66907=CARTESIAN_POINT('Ctrl Pts',(1.44706187529347,88.4846233889889,14.9587837166703));
#66908=CARTESIAN_POINT('Ctrl Pts',(0.114470931192956,88.654038112156,15.490145542295));
#66909=CARTESIAN_POINT('Ctrl Pts',(-1.25916192799034,88.822969675263,15.0906241235063));
#66910=CARTESIAN_POINT('Ctrl Pts',(-2.09560310047496,88.9917050308331,13.9320395573069));
#66911=CARTESIAN_POINT('Ctrl Pts',(-2.04257722445289,89.1605337788261,12.5033578126581));
#66912=CARTESIAN_POINT('Ctrl Pts',(-1.12012936481134,89.3297315469923,11.4070937941172));
#66913=CARTESIAN_POINT('Ctrl Pts',(0.286696045370998,89.4995816379407,11.1088441712803));
#66914=CARTESIAN_POINT('Ctrl Pts',(1.58651870415989,89.6703670139991,11.7423879557218));
#66915=CARTESIAN_POINT('Ctrl Pts',(2.22595425815534,89.842350400716,13.0503414586556));
#66916=CARTESIAN_POINT('Ctrl Pts',(1.92529539458401,90.0158010308196,14.4874754606883));
#66917=CARTESIAN_POINT('Ctrl Pts',(0.790492215056007,90.1909652726362,15.4435665686406));
#66918=CARTESIAN_POINT('Ctrl Pts',(-0.706749559667907,90.3680886422505,
15.5022785908669));
#66919=CARTESIAN_POINT('Ctrl Pts',(-1.94208149948933,90.5473974420758,14.6136707249352));
#66920=CARTESIAN_POINT('Ctrl Pts',(-2.32134740968715,90.7089149015442,13.3048090177519));
#66921=CARTESIAN_POINT('Ctrl Pts',(-1.92625465510593,90.8927859601538,11.8413878466589));
#66922=CARTESIAN_POINT('Ctrl Pts',(-0.614630769096463,91.0793754170575,
10.8581369311724));
#66923=CARTESIAN_POINT('Ctrl Pts',(1.16556187554226,91.2905041790304,11.0984488892043));
#66924=CARTESIAN_POINT('Ctrl Pts',(2.30849914728408,91.4835977897773,12.2608686442338));
#66925=CARTESIAN_POINT('Ctrl Pts',(2.50036231468186,91.6798901149816,13.9128735430949));
#66926=CARTESIAN_POINT('Ctrl Pts',(1.61948799120833,91.8794777853063,15.3546465447847));
#66927=CARTESIAN_POINT('Ctrl Pts',(0.0124764273870137,92.0824402313226,
15.9615904836018));
#66928=CARTESIAN_POINT('Ctrl Pts',(-1.65778547414679,92.2888294874047,15.4412359339448));
#66929=CARTESIAN_POINT('Ctrl Pts',(-2.66777984345844,92.4986772953065,13.9831161087662));
#66930=CARTESIAN_POINT('Ctrl Pts',(-2.56403319460919,92.7356915483555,11.9745820778711));
#66931=CARTESIAN_POINT('Ctrl Pts',(-0.83751181631646,93.0013284740074,10.3865690722854));
#66932=CARTESIAN_POINT('Ctrl Pts',(1.75450491698771,93.2971496847048,10.7565885464627));
#66933=CARTESIAN_POINT('Ctrl Pts',(3.01994199066127,93.5736867531223,12.8412119373476));
#66934=CARTESIAN_POINT('Ctrl Pts',(2.52638804680682,93.8291829167515,14.9512413752771));
#66935=CARTESIAN_POINT('Ctrl Pts',(0.996260359527135,94.0621569171439,16.1916370909168));
#66936=CARTESIAN_POINT('Ctrl Pts',(-1.00154782760166,94.298013313165,16.2284536515627));
#66937=CARTESIAN_POINT('Ctrl Pts',(-2.61610189112216,94.5365832250761,15.0145974091672));
#66938=CARTESIAN_POINT('Ctrl Pts',(-3.14844291819632,94.7776817508467,13.0437619004143));
#66939=CARTESIAN_POINT('Ctrl Pts',(-2.34795468244211,95.0211056104699,11.1443008384644));
#66940=CARTESIAN_POINT('Ctrl Pts',(-0.491683122832005,95.2721264130899,
10.1088186465028));
#66941=CARTESIAN_POINT('Ctrl Pts',(0.939396477399463,95.4426433216997,10.3601489744408));
#66942=CARTESIAN_POINT('Ctrl Pts',(1.54924545211863,95.5309739648478,10.7198394417325));
#66943=CARTESIAN_POINT('Ctrl Pts',(2.1337264791801,84.6443151365533,11.9956579243407));
#66944=CARTESIAN_POINT('Ctrl Pts',(2.41064937960028,84.7146230470702,12.4862879084337));
#66945=CARTESIAN_POINT('Ctrl Pts',(2.60892136655532,84.8522667683779,13.6362565051101));
#66946=CARTESIAN_POINT('Ctrl Pts',(1.79597107933622,85.0532691153375,15.1317096613373));
#66947=CARTESIAN_POINT('Ctrl Pts',(0.280726287153252,85.2483326659362,15.7890689877668));
#66948=CARTESIAN_POINT('Ctrl Pts',(-1.28065427067585,85.4388482483439,15.3840650108478));
#66949=CARTESIAN_POINT('Ctrl Pts',(-2.23968418325529,85.6249569075585,14.1336336455185));
#66950=CARTESIAN_POINT('Ctrl Pts',(-2.2249743216775,85.8068265935561,12.5928448547549));
#66951=CARTESIAN_POINT('Ctrl Pts',(-1.28900177800295,85.9846493395728,11.4165205373277));
#66952=CARTESIAN_POINT('Ctrl Pts',(0.306736012512332,86.1779839507388,11.0295704161824));
#66953=CARTESIAN_POINT('Ctrl Pts',(1.5892325281228,86.347825350711,11.7977925215452));
#66954=CARTESIAN_POINT('Ctrl Pts',(2.02502205082946,86.4959380259083,12.9347356763797));
#66955=CARTESIAN_POINT('Ctrl Pts',(1.94668016368254,86.6422741499,14.1345885647596));
#66956=CARTESIAN_POINT('Ctrl Pts',(0.882955606261628,86.8220858098603,15.3113974684164));
#66957=CARTESIAN_POINT('Ctrl Pts',(-0.988161227470902,87.0336759814836,
15.2247810012068));
#66958=CARTESIAN_POINT('Ctrl Pts',(-2.08083958288015,87.2419067711699,13.7409846939147));
#66959=CARTESIAN_POINT('Ctrl Pts',(-1.67511210822208,87.4305117193772,12.1279430790217));
#66960=CARTESIAN_POINT('Ctrl Pts',(-0.444803747563472,87.6008250424078,
11.3711851157103));
#66961=CARTESIAN_POINT('Ctrl Pts',(0.840029322075505,87.7536072182553,11.5098706737521));
#66962=CARTESIAN_POINT('Ctrl Pts',(1.76671140293624,87.9062850161924,12.4115013931666));
#66963=CARTESIAN_POINT('Ctrl Pts',(1.9442703075463,88.0592488970441,13.6940351959479));
#66964=CARTESIAN_POINT('Ctrl Pts',(1.2929065845589,88.2128895222246,14.8200340958466));
#66965=CARTESIAN_POINT('Ctrl Pts',(0.078341532753162,88.3676001818018,15.3107391643716));
#66966=CARTESIAN_POINT('Ctrl Pts',(-1.19300321711147,88.5237478805622,14.9477511619699));
#66967=CARTESIAN_POINT('Ctrl Pts',(-1.98166558012459,88.6817072149568,13.8674404322395));
#66968=CARTESIAN_POINT('Ctrl Pts',(-1.93899989217078,88.8418413440677,12.5122430823426));
#66969=CARTESIAN_POINT('Ctrl Pts',(-1.05866600590178,89.0044825362734,11.4533599933358));
#66970=CARTESIAN_POINT('Ctrl Pts',(0.309927544491852,89.1699591918152,11.1543574193689));
#66971=CARTESIAN_POINT('Ctrl Pts',(1.59711536188005,89.3385840053592,11.7715768352609));
#66972=CARTESIAN_POINT('Ctrl Pts',(2.24528564199875,89.5106337073209,13.0756344208351));
#66973=CARTESIAN_POINT('Ctrl Pts',(1.9504726966363,89.6863771996163,14.5334898960415));
#66974=CARTESIAN_POINT('Ctrl Pts',(0.793294265881137,89.866045646563,15.5219816997322));
#66975=CARTESIAN_POINT('Ctrl Pts',(-0.759752367639839,90.0498542107665,
15.5935142678018));
#66976=CARTESIAN_POINT('Ctrl Pts',(-2.0622361919369,90.2379836000976,14.6702777059554));
#66977=CARTESIAN_POINT('Ctrl Pts',(-2.4734495500373,90.4091881365894,13.2857154659721));
#66978=CARTESIAN_POINT('Ctrl Pts',(-2.06113611996042,90.6056250130043,11.7200463440775));
#66979=CARTESIAN_POINT('Ctrl Pts',(-0.655671099088308,90.8067274412847,
10.6498457903147));
#66980=CARTESIAN_POINT('Ctrl Pts',(1.28206908520706,91.0363378293367,10.8979792638463));
#66981=CARTESIAN_POINT('Ctrl Pts',(2.5416063059583,91.2477682958074,12.1626935937863));
#66982=CARTESIAN_POINT('Ctrl Pts',(2.76448768380754,91.4639777019449,13.9807155710471));
#66983=CARTESIAN_POINT('Ctrl Pts',(1.79928585137275,91.6849312977057,15.5827333174776));
#66984=CARTESIAN_POINT('Ctrl Pts',(0.0170449762822211,91.9105601009339,
16.2681396907231));
#66985=CARTESIAN_POINT('Ctrl Pts',(-1.84921663195079,92.1407659689192,15.6986678726876));
#66986=CARTESIAN_POINT('Ctrl Pts',(-2.98768197951198,92.3754224374738,14.0747010842829));
#66987=CARTESIAN_POINT('Ctrl Pts',(-2.88385286614705,92.640911962928,11.8243812235443));
#66988=CARTESIAN_POINT('Ctrl Pts',(-0.957183176571245,92.9388025030031,
10.0333992098132));
#66989=CARTESIAN_POINT('Ctrl Pts',(1.95147527508967,93.2705431010961,10.4341199829326));
#66990=CARTESIAN_POINT('Ctrl Pts',(3.3793775924711,93.5802804163528,12.7624589824902));
#66991=CARTESIAN_POINT('Ctrl Pts',(2.83824145028234,93.8658711879965,15.123316664714));
#66992=CARTESIAN_POINT('Ctrl Pts',(1.13797862626035,94.1256725052158,16.5138073473761));
#66993=CARTESIAN_POINT('Ctrl Pts',(-1.08311859584813,94.3879216885077,16.5638564591368));
#66994=CARTESIAN_POINT('Ctrl Pts',(-2.87731338739983,94.6522707298234,15.225916540037));
#66995=CARTESIAN_POINT('Ctrl Pts',(-3.47296015984411,94.9183620722804,13.0530787778772));
#66996=CARTESIAN_POINT('Ctrl Pts',(-2.60089361258174,95.1858234522663,10.9629985131129));
#66997=CARTESIAN_POINT('Ctrl Pts',(-0.575291002683476,95.4602756020544,
9.8240391325891));
#66998=CARTESIAN_POINT('Ctrl Pts',(0.981602534789498,95.645681201499,10.0924365728361));
#66999=CARTESIAN_POINT('Ctrl Pts',(1.64414854638063,95.7414258613175,10.4795786583213));
#67000=CARTESIAN_POINT('Ctrl Pts',(2.32926620539106,98.3820905511788,11.315870744573));
#67001=CARTESIAN_POINT('Ctrl Pts',(2.69493995777859,98.4541857528228,11.7630352306204));
#67002=CARTESIAN_POINT('Ctrl Pts',(3.15450211047238,98.5959918188983,12.8524682974727));
#67003=CARTESIAN_POINT('Ctrl Pts',(2.8728678713054,98.8053526764308,14.5732971974836));
#67004=CARTESIAN_POINT('Ctrl Pts',(1.7489436325344,99.0105003412595,15.8596457798458));
#67005=CARTESIAN_POINT('Ctrl Pts',(0.137401383018491,99.2128414252949,16.3532340115199));
#67006=CARTESIAN_POINT('Ctrl Pts',(-1.20008932127566,99.3790185028937,15.9985498101805));
#67007=CARTESIAN_POINT('Ctrl Pts',(-2.0298458980374,99.5104422645353,15.3341208557355));
#67008=CARTESIAN_POINT('Ctrl Pts',(-2.64371113418118,99.6408387621566,14.4754288465473));
#67009=CARTESIAN_POINT('Ctrl Pts',(-2.91077650132971,99.801879403758,13.1629053944612));
#67010=CARTESIAN_POINT('Ctrl Pts',(-2.30193793452482,100.013038207241,11.5098151807535));
#67011=CARTESIAN_POINT('Ctrl Pts',(-0.653860747579426,100.240650037961,
10.4643285577639));
#67012=CARTESIAN_POINT('Ctrl Pts',(1.39652630140739,100.483036430519,10.827076812383));
#67013=CARTESIAN_POINT('Ctrl Pts',(2.52533114927779,100.699746357258,12.3030925980515));
#67014=CARTESIAN_POINT('Ctrl Pts',(2.53500450171196,100.892395386792,13.9085733567948));
#67015=CARTESIAN_POINT('Ctrl Pts',(1.79773017141689,101.062432504713,15.1162732471124));
#67016=CARTESIAN_POINT('Ctrl Pts',(0.557534924579458,101.229155089766,15.7422279973987));
#67017=CARTESIAN_POINT('Ctrl Pts',(-0.571837703131487,101.365366721425,
15.6410180425175));
#67018=CARTESIAN_POINT('Ctrl Pts',(-1.33230934740187,101.47273570082,15.2210687872799));
#67019=CARTESIAN_POINT('Ctrl Pts',(-1.79058153699214,101.552468988986,14.7671787687757));
#67020=CARTESIAN_POINT('Ctrl Pts',(-2.10298870045688,101.631423318044,14.2100248929845));
#67021=CARTESIAN_POINT('Ctrl Pts',(-2.29941666157641,101.73566621192,13.3899123585956));
#67022=CARTESIAN_POINT('Ctrl Pts',(-2.10340034761895,101.864076701832,12.3374498456843));
#67023=CARTESIAN_POINT('Ctrl Pts',(-1.34801811984108,101.998445948856,11.5143857513643));
#67024=CARTESIAN_POINT('Ctrl Pts',(-0.214963331132888,102.147276247187,
11.07378096596));
#67025=CARTESIAN_POINT('Ctrl Pts',(1.0134066427486,102.29338793081,11.3094928437476));
#67026=CARTESIAN_POINT('Ctrl Pts',(1.898888574248,102.452466354268,12.2994347933101));
#67027=CARTESIAN_POINT('Ctrl Pts',(2.10849282477825,102.5932690289,13.4503728680158));
#67028=CARTESIAN_POINT('Ctrl Pts',(1.68169428198145,102.731883915474,14.5250971334327));
#67029=CARTESIAN_POINT('Ctrl Pts',(0.870570209303794,102.853302183626,15.1256434184298));
#67030=CARTESIAN_POINT('Ctrl Pts',(-0.21524462154583,102.988381671201,15.3203822425943));
#67031=CARTESIAN_POINT('Ctrl Pts',(-1.09816815381474,103.099539973989,14.9672230150072));
#67032=CARTESIAN_POINT('Ctrl Pts',(-1.62082829575769,103.202274108003,14.3196850878211));
#67033=CARTESIAN_POINT('Ctrl Pts',(-1.90109061114495,103.28989800875,13.6687113972404));
#67034=CARTESIAN_POINT('Ctrl Pts',(-1.89160665090365,103.376916014849,12.9440991525659));
#67035=CARTESIAN_POINT('Ctrl Pts',(-1.59953921394162,103.463444601711,12.3078190182658));
#67036=CARTESIAN_POINT('Ctrl Pts',(-1.14734301614179,103.549679693028,11.7763926106062));
#67037=CARTESIAN_POINT('Ctrl Pts',(-0.341801890305038,103.656998696664,
11.389519255861));
#67038=CARTESIAN_POINT('Ctrl Pts',(0.720330453089296,103.785246069805,11.5049339932187));
#67039=CARTESIAN_POINT('Ctrl Pts',(1.55977130459687,103.913188765162,12.1608445039213));
#67040=CARTESIAN_POINT('Ctrl Pts',(1.92756435851514,104.041056120166,13.1606287698491));
#67041=CARTESIAN_POINT('Ctrl Pts',(1.73609916594073,104.154858394614,14.0885033980296));
#67042=CARTESIAN_POINT('Ctrl Pts',(1.23283508114643,104.254681708604,14.7283130870023));
#67043=CARTESIAN_POINT('Ctrl Pts',(0.731674204292337,104.32618975619,15.0256034889539));
#67044=CARTESIAN_POINT('Ctrl Pts',(0.285162600187898,104.383544486588,15.1427637986439));
#67045=CARTESIAN_POINT('Ctrl Pts',(-0.176137074242099,104.441018582419,
15.1763120810118));
#67046=CARTESIAN_POINT('Ctrl Pts',(-0.751264634096996,104.51309058961,15.0567985842817));
#67047=CARTESIAN_POINT('Ctrl Pts',(-1.24688257511855,104.58553341317,14.7354388218607));
#67048=CARTESIAN_POINT('Ctrl Pts',(-1.55441023882616,104.643735615231,14.3823236486075));
#67049=CARTESIAN_POINT('Ctrl Pts',(-1.91377889489559,104.731316081866,13.7757375195179));
#67050=CARTESIAN_POINT('Ctrl Pts',(-1.99664443357858,104.863745532147,12.6438805035126));
#67051=CARTESIAN_POINT('Ctrl Pts',(-1.04309428332082,105.043102190833,11.4328977755217));
#67052=CARTESIAN_POINT('Ctrl Pts',(0.244197832177701,105.195270638501,11.2225120094968));
#67053=CARTESIAN_POINT('Ctrl Pts',(1.17430485409628,105.31885632517,11.6120647990092));
#67054=CARTESIAN_POINT('Ctrl Pts',(1.78711054085387,105.422926774664,12.1977614975811));
#67055=CARTESIAN_POINT('Ctrl Pts',(2.13921750944901,105.53887239286,13.0889544092712));
#67056=CARTESIAN_POINT('Ctrl Pts',(2.01431169320179,105.667297712427,14.1421503743038));
#67057=CARTESIAN_POINT('Ctrl Pts',(1.3711465398885,105.803211209963,15.0627365372946));
#67058=CARTESIAN_POINT('Ctrl Pts',(0.286102187432918,105.947032839628,15.5691851440355));
#67059=CARTESIAN_POINT('Ctrl Pts',(-0.973013580671568,106.099235761022,
15.4189649577865));
#67060=CARTESIAN_POINT('Ctrl Pts',(-1.98293771020574,106.25440520203,14.6132612144251));
#67061=CARTESIAN_POINT('Ctrl Pts',(-2.42540130933238,106.41264225971,13.3718877473894));
#67062=CARTESIAN_POINT('Ctrl Pts',(-2.14159152551099,106.574035260974,12.05824585642));
#67063=CARTESIAN_POINT('Ctrl Pts',(-1.18955423369878,106.738656846882,11.0719338039678));
#67064=CARTESIAN_POINT('Ctrl Pts',(0.219166308238618,106.913130725917,10.7155127352073));
#67065=CARTESIAN_POINT('Ctrl Pts',(1.17828412266602,107.03412190253,11.0517911283707));
#67066=CARTESIAN_POINT('Ctrl Pts',(1.58874560978865,107.098668256655,11.3669222244684));
#67067=CARTESIAN_POINT('Ctrl Pts',(2.16507776278379,98.4487062429102,11.4115576670062));
#67068=CARTESIAN_POINT('Ctrl Pts',(2.51172315852272,98.5164451800714,11.8291290167757));
#67069=CARTESIAN_POINT('Ctrl Pts',(2.9501904150609,98.6495211739876,12.8483188307114));
#67070=CARTESIAN_POINT('Ctrl Pts',(2.69810460566407,98.8455618367907,14.4613815118639));
#67071=CARTESIAN_POINT('Ctrl Pts',(1.65666157345432,99.0372836109927,15.671090461532));
#67072=CARTESIAN_POINT('Ctrl Pts',(0.156784680815158,99.2260577432743,16.1427198977121));
#67073=CARTESIAN_POINT('Ctrl Pts',(-1.09154198223851,99.3808653102375,15.8218016783094));
#67074=CARTESIAN_POINT('Ctrl Pts',(-1.86857646175828,99.5031875405753,15.2095054230858));
#67075=CARTESIAN_POINT('Ctrl Pts',(-2.44585043467083,99.6244894116808,14.4152909674852));
#67076=CARTESIAN_POINT('Ctrl Pts',(-2.70372853688371,99.77419436994,13.1972753456789));
#67077=CARTESIAN_POINT('Ctrl Pts',(-2.1505549898306,99.9703691734479,11.6571577300591));
#67078=CARTESIAN_POINT('Ctrl Pts',(-0.628257391422791,100.181757318978,
10.673676255501));
#67079=CARTESIAN_POINT('Ctrl Pts',(1.27892157899806,100.406914176573,10.9941873969971));
#67080=CARTESIAN_POINT('Ctrl Pts',(2.34048410598568,100.608394905306,12.3568259937458));
#67081=CARTESIAN_POINT('Ctrl Pts',(2.36315036799856,100.787749485407,13.851171738007));
#67082=CARTESIAN_POINT('Ctrl Pts',(1.68633892577243,100.946302723298,14.9835439965474));
#67083=CARTESIAN_POINT('Ctrl Pts',(0.533450727153234,101.102076850792,15.5794325826145));
#67084=CARTESIAN_POINT('Ctrl Pts',(-0.525066618352268,101.229653703928,
15.4951216475083));
#67085=CARTESIAN_POINT('Ctrl Pts',(-1.24261559725032,101.330433895234,15.1079982740459));
#67086=CARTESIAN_POINT('Ctrl Pts',(-1.67756889910168,101.405389363526,14.6856544196782));
#67087=CARTESIAN_POINT('Ctrl Pts',(-1.97695860024531,101.479737598154,14.1640433477083));
#67088=CARTESIAN_POINT('Ctrl Pts',(-2.17005146414342,101.57807228972,13.3924623469577));
#67089=CARTESIAN_POINT('Ctrl Pts',(-1.99538196912404,101.69955164982,12.3950488160063));
#67090=CARTESIAN_POINT('Ctrl Pts',(-1.28647863191238,101.827206737331,11.605377727602));
#67091=CARTESIAN_POINT('Ctrl Pts',(-0.210783711347632,101.969150612895,
11.1734303992142));
#67092=CARTESIAN_POINT('Ctrl Pts',(0.968980110784211,102.109197430349,11.3851065206294));
#67093=CARTESIAN_POINT('Ctrl Pts',(1.83449204726866,102.262652988264,12.329588887239));
#67094=CARTESIAN_POINT('Ctrl Pts',(2.05136790923078,102.399278256329,13.4435900836687));
#67095=CARTESIAN_POINT('Ctrl Pts',(1.6479272701096,102.534620253491,14.4978847248409));
#67096=CARTESIAN_POINT('Ctrl Pts',(0.858482367728352,102.653945955347,15.0980434272643));
#67097=CARTESIAN_POINT('Ctrl Pts',(-0.211879256810604,102.787446772081,
15.3038835430309));
#67098=CARTESIAN_POINT('Ctrl Pts',(-1.09508607595738,102.898069112918,14.9646832330691));
#67099=CARTESIAN_POINT('Ctrl Pts',(-1.6267785734138,103.000973018449,14.3228560151164));
#67100=CARTESIAN_POINT('Ctrl Pts',(-1.91674678972689,103.089055190921,13.6722937375774));
#67101=CARTESIAN_POINT('Ctrl Pts',(-1.91714874007563,103.177000200415,12.9400669685551));
#67102=CARTESIAN_POINT('Ctrl Pts',(-1.62887128498662,103.264921017815,12.2898310562481));
#67103=CARTESIAN_POINT('Ctrl Pts',(-1.17501187054071,103.352856902418,11.7420751853729));
#67104=CARTESIAN_POINT('Ctrl Pts',(-0.354999662671231,103.462876607181,
11.3341085134853));
#67105=CARTESIAN_POINT('Ctrl Pts',(0.742794669808538,103.595269319499,11.4378314328122));
#67106=CARTESIAN_POINT('Ctrl Pts',(1.6245574524756,103.728242056865,12.1070383547486));
#67107=CARTESIAN_POINT('Ctrl Pts',(2.0239406035163,103.862000653388,13.1471298237393));
#67108=CARTESIAN_POINT('Ctrl Pts',(1.83622631795286,103.981779730254,14.1262977461567));
#67109=CARTESIAN_POINT('Ctrl Pts',(1.3133416807573,104.087352933003,14.8100338655519));
#67110=CARTESIAN_POINT('Ctrl Pts',(0.785834080040622,104.163255187635,15.132724277827));
#67111=CARTESIAN_POINT('Ctrl Pts',(0.312439097394648,104.22429356955,15.2637142130627));
#67112=CARTESIAN_POINT('Ctrl Pts',(-0.178671074865471,104.285559869038,
15.3060159702618));
#67113=CARTESIAN_POINT('Ctrl Pts',(-0.794786296770833,104.362574759393,
15.1866477277048));
#67114=CARTESIAN_POINT('Ctrl Pts',(-1.330469273762,104.440218336155,14.8494644185806));
#67115=CARTESIAN_POINT('Ctrl Pts',(-1.66568812591068,104.502730747048,14.474658333133));
#67116=CARTESIAN_POINT('Ctrl Pts',(-2.06065477599685,104.596919873498,13.8276155705839));
#67117=CARTESIAN_POINT('Ctrl Pts',(-2.16697226106977,104.739796149952,12.6080465029953));
#67118=CARTESIAN_POINT('Ctrl Pts',(-1.15199041777266,104.934097470161,11.2824363581431));
#67119=CARTESIAN_POINT('Ctrl Pts',(0.243658765030482,105.099464035666,11.0354787111077));
#67120=CARTESIAN_POINT('Ctrl Pts',(1.26119383106488,105.233986560599,11.4466899111251));
#67121=CARTESIAN_POINT('Ctrl Pts',(1.9365604370268,105.347363371189,12.0763001234226));
#67122=CARTESIAN_POINT('Ctrl Pts',(2.33228516036666,105.473765523175,13.0429364538209));
#67123=CARTESIAN_POINT('Ctrl Pts',(2.20993278665595,105.613831408377,14.1929931475162));
#67124=CARTESIAN_POINT('Ctrl Pts',(1.52047758571895,105.762065900799,15.2051331481097));
#67125=CARTESIAN_POINT('Ctrl Pts',(0.344098514121134,105.91886873789,15.7708592678365));
#67126=CARTESIAN_POINT('Ctrl Pts',(-1.02912827537185,106.084671343671,15.6227001010336));
#67127=CARTESIAN_POINT('Ctrl Pts',(-2.13736931842044,106.253494995048,14.75831771187));
#67128=CARTESIAN_POINT('Ctrl Pts',(-2.63234926916575,106.42537687195,13.4152597750011));
#67129=CARTESIAN_POINT('Ctrl Pts',(-2.3395791441654,106.600340436149,11.9881676930327));
#67130=CARTESIAN_POINT('Ctrl Pts',(-1.32084832213294,106.778394314994,10.9110647073382));
#67131=CARTESIAN_POINT('Ctrl Pts',(0.194853311955219,106.966615675196,10.5115694226002));
#67132=CARTESIAN_POINT('Ctrl Pts',(1.22978840410585,107.096747140189,10.8633655039387));
#67133=CARTESIAN_POINT('Ctrl Pts',(1.67374240970349,107.166046927473,11.1972689795355));
#67134=CARTESIAN_POINT('Ctrl Pts',(2.00088932017653,98.5153219346416,11.5072445894395));
#67135=CARTESIAN_POINT('Ctrl Pts',(2.32850635926684,98.57870460732,11.8952228029309));
#67136=CARTESIAN_POINT('Ctrl Pts',(2.74587871964942,98.7030505290768,12.8441693639504));
#67137=CARTESIAN_POINT('Ctrl Pts',(2.52334134002275,98.8857709971507,14.3494658262441));
#67138=CARTESIAN_POINT('Ctrl Pts',(1.56437951437425,99.0640668807258,15.4825351432181));
#67139=CARTESIAN_POINT('Ctrl Pts',(0.176167978611816,99.2392740612538,15.9322057839043));
#67140=CARTESIAN_POINT('Ctrl Pts',(-0.982994643201375,99.3827121175813,
15.6450535464384));
#67141=CARTESIAN_POINT('Ctrl Pts',(-1.70730702547919,99.4959328166154,15.0848899904361));
#67142=CARTESIAN_POINT('Ctrl Pts',(-2.2479897351605,99.6081400612049,14.355153088423));
#67143=CARTESIAN_POINT('Ctrl Pts',(-2.49668057243772,99.7465093361221,13.2316452968967));
#67144=CARTESIAN_POINT('Ctrl Pts',(-1.99917204513637,99.9277001396536,11.8045002793647));
#67145=CARTESIAN_POINT('Ctrl Pts',(-0.602654035266162,100.122864599995,
10.883023953238));
#67146=CARTESIAN_POINT('Ctrl Pts',(1.16131685658873,100.330791922626,11.1612979816114));
#67147=CARTESIAN_POINT('Ctrl Pts',(2.15563706269356,100.517043453353,12.4105593894401));
#67148=CARTESIAN_POINT('Ctrl Pts',(2.19129623428519,100.683103584022,13.7937701192192));
#67149=CARTESIAN_POINT('Ctrl Pts',(1.57494768012797,100.830172941884,14.8508147459825));
#67150=CARTESIAN_POINT('Ctrl Pts',(0.509366529727014,100.974998611821,15.4166371678302));
#67151=CARTESIAN_POINT('Ctrl Pts',(-0.478295533573054,101.093940686429,
15.349225252499));
#67152=CARTESIAN_POINT('Ctrl Pts',(-1.15292184709877,101.188132089647,14.9949277608119));
#67153=CARTESIAN_POINT('Ctrl Pts',(-1.56455626121122,101.258309738068,14.6041300705805));
#67154=CARTESIAN_POINT('Ctrl Pts',(-1.85092850003376,101.328051878265,14.1180618024322));
#67155=CARTESIAN_POINT('Ctrl Pts',(-2.04068626671044,101.420478367521,13.39501233532));
#67156=CARTESIAN_POINT('Ctrl Pts',(-1.88736359062915,101.53502659781,12.4526477863286));
#67157=CARTESIAN_POINT('Ctrl Pts',(-1.22493914398367,101.655967525809,11.6963697038397));
#67158=CARTESIAN_POINT('Ctrl Pts',(-0.206604091562376,101.791024978605,
11.2730798324683));
#67159=CARTESIAN_POINT('Ctrl Pts',(0.924553578819829,101.925006929887,11.4607201975114));
#67160=CARTESIAN_POINT('Ctrl Pts',(1.77009552028933,102.072839622259,12.3597429811677));
#67161=CARTESIAN_POINT('Ctrl Pts',(1.99424299368331,102.205287483758,13.4368072993216));
#67162=CARTESIAN_POINT('Ctrl Pts',(1.61416025823776,102.337356591508,14.4706723162492));
#67163=CARTESIAN_POINT('Ctrl Pts',(0.846394526152918,102.454589727069,15.0704434360988));
#67164=CARTESIAN_POINT('Ctrl Pts',(-0.208513892075373,102.586511872962,
15.2873848434675));
#67165=CARTESIAN_POINT('Ctrl Pts',(-1.09200399810003,102.696598251846,14.9621434511312));
#67166=CARTESIAN_POINT('Ctrl Pts',(-1.63272885106989,102.799671928898,14.3260269424118));
#67167=CARTESIAN_POINT('Ctrl Pts',(-1.93240296830881,102.888212373092,13.6758760779144));
#67168=CARTESIAN_POINT('Ctrl Pts',(-1.94269082924761,102.977084385981,12.9360347845444));
#67169=CARTESIAN_POINT('Ctrl Pts',(-1.65820335603162,103.06639743392,12.2718430942304));
#67170=CARTESIAN_POINT('Ctrl Pts',(-1.20268072493963,103.156034111808,11.7077577601396));
#67171=CARTESIAN_POINT('Ctrl Pts',(-0.368197435037411,103.268754517698,
11.2786977711096));
#67172=CARTESIAN_POINT('Ctrl Pts',(0.765258886527789,103.405292569193,11.3707288724057));
#67173=CARTESIAN_POINT('Ctrl Pts',(1.68934360035434,103.543295348571,12.0532322055757));
#67174=CARTESIAN_POINT('Ctrl Pts',(2.12031684851748,103.682945186611,13.1336308776294));
#67175=CARTESIAN_POINT('Ctrl Pts',(1.93635346996498,103.808701065892,14.1640920942839));
#67176=CARTESIAN_POINT('Ctrl Pts',(1.39384828036816,103.920024157402,14.8917546441016));
#67177=CARTESIAN_POINT('Ctrl Pts',(0.839993955788918,104.000320619079,15.2398450667002));
#67178=CARTESIAN_POINT('Ctrl Pts',(0.339715594601406,104.065042652514,15.3846646274813));
#67179=CARTESIAN_POINT('Ctrl Pts',(-0.181205075488834,104.130101155658,
15.4357198595116));
#67180=CARTESIAN_POINT('Ctrl Pts',(-0.838307959444663,104.212058929177,
15.3164968711279));
#67181=CARTESIAN_POINT('Ctrl Pts',(-1.41405597240546,104.294903259141,14.9634900153004));
#67182=CARTESIAN_POINT('Ctrl Pts',(-1.77696601299519,104.361725878863,14.5669930176586));
#67183=CARTESIAN_POINT('Ctrl Pts',(-2.2075306570981,104.46252366513,13.8794936216499));
#67184=CARTESIAN_POINT('Ctrl Pts',(-2.33730008856093,104.615846767758,12.5722125024781));
#67185=CARTESIAN_POINT('Ctrl Pts',(-1.2608865522245,104.825092749488,11.1319749407646));
#67186=CARTESIAN_POINT('Ctrl Pts',(0.243119697883272,105.003657432829,10.8484454127187));
#67187=CARTESIAN_POINT('Ctrl Pts',(1.34808280803351,105.149116796028,11.2813150232408));
#67188=CARTESIAN_POINT('Ctrl Pts',(2.08601033319973,105.271799967715,11.9548387492641));
#67189=CARTESIAN_POINT('Ctrl Pts',(2.52535281128431,105.40865865349,12.9969184983707));
#67190=CARTESIAN_POINT('Ctrl Pts',(2.4055538801101,105.560365104324,14.2438359207287));
#67191=CARTESIAN_POINT('Ctrl Pts',(1.66980863154941,105.720920591636,15.3475297589247));
#67192=CARTESIAN_POINT('Ctrl Pts',(0.402094840809354,105.890704636152,15.9725333916377));
#67193=CARTESIAN_POINT('Ctrl Pts',(-1.08524297007214,106.070106926321,15.8264352442804));
#67194=CARTESIAN_POINT('Ctrl Pts',(-2.29180092663514,106.252584788068,14.9033742093148));
#67195=CARTESIAN_POINT('Ctrl Pts',(-2.83929722899912,106.438111484187,13.4586318026127));
#67196=CARTESIAN_POINT('Ctrl Pts',(-2.53756676281984,106.626645611325,11.9180895296454));
#67197=CARTESIAN_POINT('Ctrl Pts',(-1.45214241056707,106.818131783107,10.7501956107087));
#67198=CARTESIAN_POINT('Ctrl Pts',(0.170540315671819,107.020100624473,10.3076261099931));
#67199=CARTESIAN_POINT('Ctrl Pts',(1.28129268554569,107.159372377849,10.6749398795065));
#67200=CARTESIAN_POINT('Ctrl Pts',(1.75873920961835,107.233425598291,11.0276157346027));
#67201=CARTESIAN_POINT('Ctrl Pts',(1.83670087756925,98.5819376263729,11.6029315118727));
#67202=CARTESIAN_POINT('Ctrl Pts',(2.14528956001096,98.6409640345686,11.9613165890863));
#67203=CARTESIAN_POINT('Ctrl Pts',(2.54156702423794,98.7565798841661,12.8400198971892));
#67204=CARTESIAN_POINT('Ctrl Pts',(2.34857807438143,98.9259801575108,14.2375501406243));
#67205=CARTESIAN_POINT('Ctrl Pts',(1.47209745529416,99.0908501504588,15.2939798249042));
#67206=CARTESIAN_POINT('Ctrl Pts',(0.19555127640848,99.2524903792333,15.7216916700965));
#67207=CARTESIAN_POINT('Ctrl Pts',(-0.874447304164229,99.3845589249252,
15.4683054145673));
#67208=CARTESIAN_POINT('Ctrl Pts',(-1.54603758920007,99.4886780926552,14.9602745577865));
#67209=CARTESIAN_POINT('Ctrl Pts',(-2.05012903565016,99.591790710729,14.2950152093608));
#67210=CARTESIAN_POINT('Ctrl Pts',(-2.28963260799172,99.7188243023042,13.2660152481144));
#67211=CARTESIAN_POINT('Ctrl Pts',(-1.84778910044215,99.8850311058594,11.9518428286703));
#67212=CARTESIAN_POINT('Ctrl Pts',(-0.577050679109529,100.063971881012,
11.0923716509751));
#67213=CARTESIAN_POINT('Ctrl Pts',(1.04371213417939,100.25466966868,11.3284085662256));
#67214=CARTESIAN_POINT('Ctrl Pts',(1.97079001940144,100.425692001399,12.4642927851344));
#67215=CARTESIAN_POINT('Ctrl Pts',(2.01944210057179,100.578457682636,13.7363685004315));
#67216=CARTESIAN_POINT('Ctrl Pts',(1.46355643448351,100.71404316047,14.7180854954176));
#67217=CARTESIAN_POINT('Ctrl Pts',(0.485282332300793,100.847920372847,15.2538417530459));
#67218=CARTESIAN_POINT('Ctrl Pts',(-0.431524448793835,100.958227668931,
15.2033288574897));
#67219=CARTESIAN_POINT('Ctrl Pts',(-1.06322809694722,101.045830284061,14.8818572475778));
#67220=CARTESIAN_POINT('Ctrl Pts',(-1.45154362332076,101.111230112609,14.5226057214829));
#67221=CARTESIAN_POINT('Ctrl Pts',(-1.72489839982219,101.176366158375,14.072080257156));
#67222=CARTESIAN_POINT('Ctrl Pts',(-1.91132106927746,101.262884445321,13.3975623236822));
#67223=CARTESIAN_POINT('Ctrl Pts',(-1.77934521213425,101.370501545798,12.5102467566506));
#67224=CARTESIAN_POINT('Ctrl Pts',(-1.16339965605497,101.484728314285,11.7873616800774));
#67225=CARTESIAN_POINT('Ctrl Pts',(-0.202424471777119,101.612899344313,
11.3727292657226));
#67226=CARTESIAN_POINT('Ctrl Pts',(0.880127046855447,101.740816429424,11.5363338743933));
#67227=CARTESIAN_POINT('Ctrl Pts',(1.70569899331,101.883026256255,12.3898970750966));
#67228=CARTESIAN_POINT('Ctrl Pts',(1.93711807813584,102.011296711186,13.4300245149745));
#67229=CARTESIAN_POINT('Ctrl Pts',(1.58039324636591,102.140092929525,14.4434599076574));
#67230=CARTESIAN_POINT('Ctrl Pts',(0.834306684577478,102.25523349879,15.0428434449332));
#67231=CARTESIAN_POINT('Ctrl Pts',(-0.205148527340144,102.385576973841,
15.270886143904));
#67232=CARTESIAN_POINT('Ctrl Pts',(-1.08892192024266,102.495127390775,14.9596036691931));
#67233=CARTESIAN_POINT('Ctrl Pts',(-1.638679128726,102.598370839346,14.3291978697072));
#67234=CARTESIAN_POINT('Ctrl Pts',(-1.94805914689074,102.687369555263,13.6794584182514));
#67235=CARTESIAN_POINT('Ctrl Pts',(-1.9682329184196,102.777168571547,12.9320026005336));
#67236=CARTESIAN_POINT('Ctrl Pts',(-1.68753542707662,102.867873850023,12.2538551322126));
#67237=CARTESIAN_POINT('Ctrl Pts',(-1.23034957933855,102.959211321198,11.6734403349063));
#67238=CARTESIAN_POINT('Ctrl Pts',(-0.381395207403597,103.074632428216,
11.2232870287339));
#67239=CARTESIAN_POINT('Ctrl Pts',(0.787723103247037,103.215315818886,11.3036263119991));
#67240=CARTESIAN_POINT('Ctrl Pts',(1.75412974823307,103.358348640276,11.9994260564029));
#67241=CARTESIAN_POINT('Ctrl Pts',(2.21669309351866,103.503889719833,13.1201319315196));
#67242=CARTESIAN_POINT('Ctrl Pts',(2.03648062197711,103.635622401532,14.201886442411));
#67243=CARTESIAN_POINT('Ctrl Pts',(1.47435487997904,103.752695381801,14.9734754226512));
#67244=CARTESIAN_POINT('Ctrl Pts',(0.894153831537209,103.837386050524,15.3469658555734));
#67245=CARTESIAN_POINT('Ctrl Pts',(0.366992091808162,103.905791735478,15.5056150418999));
#67246=CARTESIAN_POINT('Ctrl Pts',(-0.183739076112201,103.974642442278,
15.5654237487616));
#67247=CARTESIAN_POINT('Ctrl Pts',(-0.881829622118494,104.06154309896,15.446346014551));
#67248=CARTESIAN_POINT('Ctrl Pts',(-1.49764267104891,104.149588182126,15.0775156120203));
#67249=CARTESIAN_POINT('Ctrl Pts',(-1.88824390007971,104.22072101068,14.6593277021841));
#67250=CARTESIAN_POINT('Ctrl Pts',(-2.35440653819935,104.328127456763,13.9313716727161));
#67251=CARTESIAN_POINT('Ctrl Pts',(-2.50762791605212,104.491897385563,12.5363785019609));
#67252=CARTESIAN_POINT('Ctrl Pts',(-1.36978268667635,104.716088028814,10.9815135233859));
#67253=CARTESIAN_POINT('Ctrl Pts',(0.242580630736055,104.907850829993,10.6614121143297));
#67254=CARTESIAN_POINT('Ctrl Pts',(1.43497178500211,105.064247031457,11.1159401353568));
#67255=CARTESIAN_POINT('Ctrl Pts',(2.23546022937266,105.196236564241,11.8333773751057));
#67256=CARTESIAN_POINT('Ctrl Pts',(2.71842046220195,105.343551783805,12.9509005429204));
#67257=CARTESIAN_POINT('Ctrl Pts',(2.60117497356426,105.506898800274,14.2946786939413));
#67258=CARTESIAN_POINT('Ctrl Pts',(1.81913967737985,105.679775282475,15.4899263697399));
#67259=CARTESIAN_POINT('Ctrl Pts',(0.460091167497574,105.862540534413,16.1742075154388));
#67260=CARTESIAN_POINT('Ctrl Pts',(-1.14135766477241,106.055542508971,16.0301703875275));
#67261=CARTESIAN_POINT('Ctrl Pts',(-2.44623253484984,106.251674581087,15.0484307067596));
#67262=CARTESIAN_POINT('Ctrl Pts',(-3.04624518883249,106.450846096425,13.5020038302243));
#67263=CARTESIAN_POINT('Ctrl Pts',(-2.73555438147426,106.6529507865,11.8480113662582));
#67264=CARTESIAN_POINT('Ctrl Pts',(-1.58343649900123,106.857869251219,10.589326514079));
#67265=CARTESIAN_POINT('Ctrl Pts',(0.14622731938842,107.073585573753,10.1036827973861));
#67266=CARTESIAN_POINT('Ctrl Pts',(1.33279696698552,107.221997615509,10.4865142550742));
#67267=CARTESIAN_POINT('Ctrl Pts',(1.8437360095332,107.300804269109,10.8579624896698));
#67268=CARTESIAN_POINT('Ctrl Pts',(2.49284186651808,100.7945130522,13.1110770588995));
#67269=CARTESIAN_POINT('Ctrl Pts',(2.51510269440366,100.863453425796,13.6629870657637));
#67270=CARTESIAN_POINT('Ctrl Pts',(2.17961349497895,100.999754830071,14.7663896380711));
#67271=CARTESIAN_POINT('Ctrl Pts',(0.795914331805827,101.1994864983,15.7392516655857));
#67272=CARTESIAN_POINT('Ctrl Pts',(-0.853766209202168,101.394579343051,
15.6554435518708));
#67273=CARTESIAN_POINT('Ctrl Pts',(-2.07338251428329,101.585126420958,14.5992895565228));
#67274=CARTESIAN_POINT('Ctrl Pts',(-2.3769033064482,101.771265881478,13.0525813475902));
#67275=CARTESIAN_POINT('Ctrl Pts',(-1.68070836712873,101.953168845295,11.6790615543513));
#67276=CARTESIAN_POINT('Ctrl Pts',(-0.316585819691275,102.131026046402,
11.0391790038355));
#67277=CARTESIAN_POINT('Ctrl Pts',(0.95913378208078,102.285723454486,11.3318051599028));
#67278=CARTESIAN_POINT('Ctrl Pts',(1.7385263897513,102.418771549116,12.0978996555273));
#67279=CARTESIAN_POINT('Ctrl Pts',(2.05900879000914,102.53130516533,12.9642472996834));
#67280=CARTESIAN_POINT('Ctrl Pts',(1.99140764775307,102.623895737268,13.7215605251988));
#67281=CARTESIAN_POINT('Ctrl Pts',(1.7505100490346,102.697301489324,14.2621652806589));
#67282=CARTESIAN_POINT('Ctrl Pts',(1.48692355688233,102.752034803086,14.6158543164599));
#67283=CARTESIAN_POINT('Ctrl Pts',(0.932904994664702,102.842734592139,15.0934843577826));
#67284=CARTESIAN_POINT('Ctrl Pts',(-0.0914144687160896,102.968333415228,
15.3762721980933));
#67285=CARTESIAN_POINT('Ctrl Pts',(-1.33485789371615,103.127446017604,14.853019541222));
#67286=CARTESIAN_POINT('Ctrl Pts',(-1.9848419465324,103.284558264171,13.6933545546193));
#67287=CARTESIAN_POINT('Ctrl Pts',(-1.7859198054212,103.440023723922,12.3916974239502));
#67288=CARTESIAN_POINT('Ctrl Pts',(-0.836554893827291,103.594221052691,
11.4959387949505));
#67289=CARTESIAN_POINT('Ctrl Pts',(0.456174919648817,103.747531635336,11.3738488107031));
#67290=CARTESIAN_POINT('Ctrl Pts',(1.3638147823984,103.874871679777,11.9549038831241));
#67291=CARTESIAN_POINT('Ctrl Pts',(1.76271423183761,103.976693557164,12.6795595279847));
#67292=CARTESIAN_POINT('Ctrl Pts',(1.90810598694439,104.078542102711,13.4945344024168));
#67293=CARTESIAN_POINT('Ctrl Pts',(1.65790918644532,104.17203697728,14.2442552014034));
#67294=CARTESIAN_POINT('Ctrl Pts',(1.18092989180617,104.257276104356,14.7396737469657));
#67295=CARTESIAN_POINT('Ctrl Pts',(0.836952047812147,104.308512974323,14.9680700673282));
#67296=CARTESIAN_POINT('Ctrl Pts',(0.450100297839354,104.359851063443,15.1155674993526));
#67297=CARTESIAN_POINT('Ctrl Pts',(0.0395872801241101,104.411306853854,
15.1750254409463));
#67298=CARTESIAN_POINT('Ctrl Pts',(-0.375108892402885,104.462898554674,
15.1429069972814));
#67299=CARTESIAN_POINT('Ctrl Pts',(-0.840313267844409,104.523254297577,
15.0001497606756));
#67300=CARTESIAN_POINT('Ctrl Pts',(-1.31270319649571,104.592502929932,14.6948548388226));
#67301=CARTESIAN_POINT('Ctrl Pts',(-1.70591154338413,104.670811240362,14.1946222164672));
#67302=CARTESIAN_POINT('Ctrl Pts',(-1.91536791775402,104.749572649424,13.5901594840855));
#67303=CARTESIAN_POINT('Ctrl Pts',(-1.92018868414222,104.85525116503,12.7322430362218));
#67304=CARTESIAN_POINT('Ctrl Pts',(-1.38717216919487,104.98870517941,11.7334940060542));
#67305=CARTESIAN_POINT('Ctrl Pts',(-0.270060311200083,105.13328337949,11.2421101980971));
#67306=CARTESIAN_POINT('Ctrl Pts',(1.07762575349443,105.29829144771,11.4226004121413));
#67307=CARTESIAN_POINT('Ctrl Pts',(1.94172923493356,105.438337213777,12.2957565076881));
#67308=CARTESIAN_POINT('Ctrl Pts',(2.11223738347851,105.571487979555,13.3693963868629));
#67309=CARTESIAN_POINT('Ctrl Pts',(1.96016494784412,105.686803188369,14.291952220544));
#67310=CARTESIAN_POINT('Ctrl Pts',(1.35126081272394,105.803960330811,15.0753078389932));
#67311=CARTESIAN_POINT('Ctrl Pts',(0.573346440079449,105.908193804669,15.4114252004776));
#67312=CARTESIAN_POINT('Ctrl Pts',(0.156498882992677,105.96074884795,15.4795852197261));
#67313=CARTESIAN_POINT('Ctrl Pts',(-0.0852434104585933,105.99090946777,
15.4884288797639));
#67314=CARTESIAN_POINT('Ctrl Pts',(-0.690982562143647,106.066524384947,
15.4613152548541));
#67315=CARTESIAN_POINT('Ctrl Pts',(-1.69935828633558,106.196714378299,15.0178602255304));
#67316=CARTESIAN_POINT('Ctrl Pts',(-2.45487748272796,106.384833620489,13.6157127030245));
#67317=CARTESIAN_POINT('Ctrl Pts',(-2.18187137791978,106.577424396135,12.0086256405781));
#67318=CARTESIAN_POINT('Ctrl Pts',(-0.948900392360805,106.774611627066,
10.8830013639477));
#67319=CARTESIAN_POINT('Ctrl Pts',(0.233539243349673,106.914804888263,10.7911776881976));
#67320=CARTESIAN_POINT('Ctrl Pts',(0.823185956938756,106.991473315452,10.9644105236304));
#67321=CARTESIAN_POINT('Ctrl Pts',(0.909520965425754,107.002848116697,10.9936163144232));
#67322=CARTESIAN_POINT('Ctrl Pts',(1.03788710524578,107.019926828246,11.0410609823112));
#67323=CARTESIAN_POINT('Ctrl Pts',(1.22456730925336,107.045442868801,11.1251201833512));
#67324=CARTESIAN_POINT('Ctrl Pts',(1.3818642775407,107.068192490325,11.2177754657732));
#67325=CARTESIAN_POINT('Ctrl Pts',(1.45735612640718,107.079506406801,11.2679629878995));
#67326=CARTESIAN_POINT('Ctrl Pts',(3.21941318832154,100.108785057528,13.1833163433551));
#67327=CARTESIAN_POINT('Ctrl Pts',(3.24455523314204,100.197321287997,13.8923045368011));
#67328=CARTESIAN_POINT('Ctrl Pts',(2.80713176742478,100.374361485089,15.3250956794238));
#67329=CARTESIAN_POINT('Ctrl Pts',(0.969614502742895,100.639422025843,16.6144421993269));
#67330=CARTESIAN_POINT('Ctrl Pts',(-1.26454957428976,100.903625125234,16.4990836728105));
#67331=CARTESIAN_POINT('Ctrl Pts',(-2.94684780441473,101.166617778622,15.0400296462461));
#67332=CARTESIAN_POINT('Ctrl Pts',(-3.37158210295618,101.428047309056,12.8672526496821));
#67333=CARTESIAN_POINT('Ctrl Pts',(-2.37673874171828,101.687566346648,10.9082910923444));
#67334=CARTESIAN_POINT('Ctrl Pts',(-0.402489017164984,101.944858172735,
9.98417551291717));
#67335=CARTESIAN_POINT('Ctrl Pts',(1.46456479582327,102.171301975291,10.4145590099485));
#67336=CARTESIAN_POINT('Ctrl Pts',(2.61231259502638,102.367597713274,11.5473339970204));
#67337=CARTESIAN_POINT('Ctrl Pts',(3.08497142042482,102.534508032253,12.8333323454061));
#67338=CARTESIAN_POINT('Ctrl Pts',(2.98184891257021,102.672415521047,13.961120190847));
#67339=CARTESIAN_POINT('Ctrl Pts',(2.62024973410492,102.781992635605,14.7672819481499));
#67340=CARTESIAN_POINT('Ctrl Pts',(2.22499652586286,102.86379154855,15.294913342711));
#67341=CARTESIAN_POINT('Ctrl Pts',(1.39445192806024,102.999473850705,16.0074493521681));
#67342=CARTESIAN_POINT('Ctrl Pts',(-0.140565850136767,103.187553708594,
16.4272206062621));
#67343=CARTESIAN_POINT('Ctrl Pts',(-1.9985595677167,103.425570942461,15.6387475870579));
#67344=CARTESIAN_POINT('Ctrl Pts',(-2.96048320986048,103.659593451464,13.9075444527093));
#67345=CARTESIAN_POINT('Ctrl Pts',(-2.65787738048873,103.889471146227,11.9838453444094));
#67346=CARTESIAN_POINT('Ctrl Pts',(-1.26176999230344,104.115073879095,10.6802078223776));
#67347=CARTESIAN_POINT('Ctrl Pts',(0.605124317383043,104.336304043699,10.5154870563486));
#67348=CARTESIAN_POINT('Ctrl Pts',(1.88707072683939,104.516961487962,11.3489400854149));
#67349=CARTESIAN_POINT('Ctrl Pts',(2.43904296713747,104.659246682307,12.3644427552886));
#67350=CARTESIAN_POINT('Ctrl Pts',(2.63371417310203,104.800036629377,13.4925391037022));
#67351=CARTESIAN_POINT('Ctrl Pts',(2.28458834892654,104.92703642919,14.5080554840302));
#67352=CARTESIAN_POINT('Ctrl Pts',(1.64371035343149,105.040835090016,15.165413844503));
#67353=CARTESIAN_POINT('Ctrl Pts',(1.18664880104888,105.108620123374,15.4647724792534));
#67354=CARTESIAN_POINT('Ctrl Pts',(0.678233264625506,105.17591182741,15.6547340548872));
#67355=CARTESIAN_POINT('Ctrl Pts',(0.144674432748567,105.242712965019,15.7282656905062));
#67356=CARTESIAN_POINT('Ctrl Pts',(-0.388137622843626,105.309026834882,
15.6831454939067));
#67357=CARTESIAN_POINT('Ctrl Pts',(-0.978854928122067,105.385826316907,
15.4970265683964));
#67358=CARTESIAN_POINT('Ctrl Pts',(-1.56896826791722,105.472795189938,15.1084644066728));
#67359=CARTESIAN_POINT('Ctrl Pts',(-2.04938088700793,105.569563993684,14.4857050331616));
#67360=CARTESIAN_POINT('Ctrl Pts',(-2.29698114254584,105.665276579509,13.7487193482343));
#67361=CARTESIAN_POINT('Ctrl Pts',(-2.29251479802894,105.79150776619,12.7231693556636));
#67362=CARTESIAN_POINT('Ctrl Pts',(-1.65421308374222,105.9467435063,11.5707423061279));
#67363=CARTESIAN_POINT('Ctrl Pts',(-0.392842510617309,106.108841018637,
11.0395975521201));
#67364=CARTESIAN_POINT('Ctrl Pts',(1.06923407512284,106.288091924768,11.2574218887874));
#67365=CARTESIAN_POINT('Ctrl Pts',(1.95337222561244,106.434482360356,12.1908952611499));
#67366=CARTESIAN_POINT('Ctrl Pts',(2.1082466558304,106.568779458601,13.2756411100311));
#67367=CARTESIAN_POINT('Ctrl Pts',(1.94421267177165,106.682846004844,14.1866454226411));
#67368=CARTESIAN_POINT('Ctrl Pts',(1.34330259058895,106.79540736939,14.9275804835321));
#67369=CARTESIAN_POINT('Ctrl Pts',(0.61200668180574,106.892712422958,15.2291155882341));
#67370=CARTESIAN_POINT('Ctrl Pts',(0.227225315900298,106.941080281224,15.2858774481804));
#67371=CARTESIAN_POINT('Ctrl Pts',(0.00613214032702904,106.968643257595,
15.2905083201661));
#67372=CARTESIAN_POINT('Ctrl Pts',(-0.54471342419038,107.037421791256,15.2571654833285));
#67373=CARTESIAN_POINT('Ctrl Pts',(-1.43438208415316,107.153376225102,14.8421645711519));
#67374=CARTESIAN_POINT('Ctrl Pts',(-2.05603692064065,107.314978655579,13.6223386293409));
#67375=CARTESIAN_POINT('Ctrl Pts',(-1.79818201528118,107.474811222724,12.2935478036575));
#67376=CARTESIAN_POINT('Ctrl Pts',(-0.786014398068314,107.6332147514,11.4126594286765));
#67377=CARTESIAN_POINT('Ctrl Pts',(0.137534125330372,107.742482326453,11.3631447251376));
#67378=CARTESIAN_POINT('Ctrl Pts',(0.587677173117342,107.801336393184,11.5049815654278));
#67379=CARTESIAN_POINT('Ctrl Pts',(0.653425842901073,107.810053434367,11.5286618432418));
#67380=CARTESIAN_POINT('Ctrl Pts',(0.75100760781322,107.823126728322,11.5669103329402));
#67381=CARTESIAN_POINT('Ctrl Pts',(0.956389857350736,107.851441476637,11.6642964257376));
#67382=CARTESIAN_POINT('Ctrl Pts',(1.35986455640331,107.912367400845,11.9449080491776));
#67383=CARTESIAN_POINT('Ctrl Pts',(1.78122114059743,107.999272471419,12.521010802963));
#67384=CARTESIAN_POINT('Ctrl Pts',(1.94192063122901,108.103466225824,13.3620056610018));
#67385=CARTESIAN_POINT('Ctrl Pts',(1.76390438783843,108.190300974208,14.0525436062148));
#67386=CARTESIAN_POINT('Ctrl Pts',(1.51226222511977,108.246795981566,14.4325824089464));
#67387=CARTESIAN_POINT('Ctrl Pts',(1.37402659897863,108.272882024984,14.5895751776131));
#67388=CARTESIAN_POINT('Ctrl Pts',(1.27618860602231,108.290276554284,14.6890093996381));
#67389=CARTESIAN_POINT('Ctrl Pts',(1.14383757110516,108.312027478503,14.8029233156905));
#67390=CARTESIAN_POINT('Ctrl Pts',(0.970805900348634,108.338144302769,14.9213825185975));
#67391=CARTESIAN_POINT('Ctrl Pts',(0.723945101066349,108.372989395592,15.0529453341035));
#67392=CARTESIAN_POINT('Ctrl Pts',(0.257373367219668,108.43402285334,15.2102168710372));
#67393=CARTESIAN_POINT('Ctrl Pts',(-0.460529247412758,108.521432115362,
15.2051861304357));
#67394=CARTESIAN_POINT('Ctrl Pts',(-1.24039994542318,108.626762875932,14.8304636360463));
#67395=CARTESIAN_POINT('Ctrl Pts',(-1.78791423789818,108.732648358347,14.1546113404499));
#67396=CARTESIAN_POINT('Ctrl Pts',(-1.99545953699991,108.839181926111,13.3045066713905));
#67397=CARTESIAN_POINT('Ctrl Pts',(-1.81861916546087,108.946473201078,12.4412539227986));
#67398=CARTESIAN_POINT('Ctrl Pts',(-1.2855418969239,109.054621381307,11.7304303379646));
#67399=CARTESIAN_POINT('Ctrl Pts',(-0.493259060560167,109.16372418882,11.3125997973087));
#67400=CARTESIAN_POINT('Ctrl Pts',(0.511368579472583,109.286110722847,11.2667175254659));
#67401=CARTESIAN_POINT('Ctrl Pts',(1.52783037367081,109.422363220256,11.7834151903454));
#67402=CARTESIAN_POINT('Ctrl Pts',(2.04447062716034,109.548086024133,12.7001566610426));
#67403=CARTESIAN_POINT('Ctrl Pts',(2.09991900669706,109.649879979524,13.5233406882324));
#67404=CARTESIAN_POINT('Ctrl Pts',(1.90500107311737,109.758925662751,14.3851318524273));
#67405=CARTESIAN_POINT('Ctrl Pts',(1.12516702783843,109.901988919277,15.311513234486));
#67406=CARTESIAN_POINT('Ctrl Pts',(-0.359505704859066,110.081107404553,
15.6254905457));
#67407=CARTESIAN_POINT('Ctrl Pts',(-1.75137860208549,110.2639827875,14.9469903243404));
#67408=CARTESIAN_POINT('Ctrl Pts',(-2.4471099510444,110.450802616763,13.5261006325578));
#67409=CARTESIAN_POINT('Ctrl Pts',(-2.11498461487842,110.641730113627,11.9439348554511));
#67410=CARTESIAN_POINT('Ctrl Pts',(-0.853141999308173,110.836900028849,
10.8768689052287));
#67411=CARTESIAN_POINT('Ctrl Pts',(0.866788744668601,111.040141111079,10.8090293100212));
#67412=CARTESIAN_POINT('Ctrl Pts',(1.82218329954828,111.179993228394,11.5191862896573));
#67413=CARTESIAN_POINT('Ctrl Pts',(2.13896789330312,111.252654201251,12.0080759845444));
#67414=CARTESIAN_POINT('Ctrl Pts',(2.97721912554466,100.337349853617,13.1591469020712));
#67415=CARTESIAN_POINT('Ctrl Pts',(3.0014225553287,100.41935795199,13.815805619725));
#67416=CARTESIAN_POINT('Ctrl Pts',(2.59798398913854,100.582822327766,15.138842769738));
#67417=CARTESIAN_POINT('Ctrl Pts',(0.911714445763874,100.826110183329,16.3227120214131));
#67418=CARTESIAN_POINT('Ctrl Pts',(-1.12762178592724,101.067276531172,16.2178702991639));
#67419=CARTESIAN_POINT('Ctrl Pts',(-2.65569270770424,101.306120659401,14.893116283005));
#67420=CARTESIAN_POINT('Ctrl Pts',(-3.04002250412019,101.542453499864,12.9290288823181));
#67421=CARTESIAN_POINT('Ctrl Pts',(-2.1447286168551,101.776100512864,11.16521457968));
#67422=CARTESIAN_POINT('Ctrl Pts',(-0.373854618007078,102.006914130624,
10.3358433432232));
#67423=CARTESIAN_POINT('Ctrl Pts',(1.29608779124244,102.209442468357,10.7203077266));
#67424=CARTESIAN_POINT('Ctrl Pts',(2.32105052660134,102.384655658554,11.7308558831893));
#67425=CARTESIAN_POINT('Ctrl Pts',(2.74298387695292,102.533440409946,12.8769706634986));
#67426=CARTESIAN_POINT('Ctrl Pts',(2.65170182429782,102.656242259788,13.8812669689642));
#67427=CARTESIAN_POINT('Ctrl Pts',(2.33033650574815,102.753762253511,14.598909725653));
#67428=CARTESIAN_POINT('Ctrl Pts',(1.97897220286934,102.826539300063,15.0685603339605));
#67429=CARTESIAN_POINT('Ctrl Pts',(1.24060295026172,102.947227431183,15.7027943540395));
#67430=CARTESIAN_POINT('Ctrl Pts',(-0.124182056329873,103.114480277472,
16.0769044702059));
#67431=CARTESIAN_POINT('Ctrl Pts',(-1.77732567638319,103.326195967508,15.3768382384458));
#67432=CARTESIAN_POINT('Ctrl Pts',(-2.63526945541779,103.534581722366,13.8361478200127));
#67433=CARTESIAN_POINT('Ctrl Pts',(-2.36722485546621,103.739655338792,12.1197960375897));
#67434=CARTESIAN_POINT('Ctrl Pts',(-1.12003162614473,103.941456270294,10.9521181465686));
#67435=CARTESIAN_POINT('Ctrl Pts',(0.555474518138305,104.140046574245,10.8016076411335));
#67436=CARTESIAN_POINT('Ctrl Pts',(1.71265207869239,104.3029315519,11.5509280179846));
#67437=CARTESIAN_POINT('Ctrl Pts',(2.21360005537086,104.431728973927,12.4694816795206));
#67438=CARTESIAN_POINT('Ctrl Pts',(2.39184477771615,104.559538453822,13.4932042032737));
#67439=CARTESIAN_POINT('Ctrl Pts',(2.07569529476612,104.675369945219,14.420122056488));
#67440=CARTESIAN_POINT('Ctrl Pts',(1.48945019955638,104.779648761463,15.0235004786572));
#67441=CARTESIAN_POINT('Ctrl Pts',(1.07008321663664,104.841917740357,15.2992050086116));
#67442=CARTESIAN_POINT('Ctrl Pts',(0.602188942363458,104.903891572755,15.475011869709));
#67443=CARTESIAN_POINT('Ctrl Pts',(0.109645381873752,104.965577594631,15.5438522739862));
#67444=CARTESIAN_POINT('Ctrl Pts',(-0.383794712696708,105.026984074812,
15.5030659950316));
#67445=CARTESIAN_POINT('Ctrl Pts',(-0.932674374696177,105.098302310464,
15.3314009658229));
#67446=CARTESIAN_POINT('Ctrl Pts',(-1.48354657744338,105.179364436602,14.9705945507227));
#67447=CARTESIAN_POINT('Ctrl Pts',(-1.93489110579998,105.269979742577,14.3886774275969));
#67448=CARTESIAN_POINT('Ctrl Pts',(-2.16977673428189,105.360041936148,13.6958660601848));
#67449=CARTESIAN_POINT('Ctrl Pts',(-2.16840609340003,105.47942223247,12.7261939158498));
#67450=CARTESIAN_POINT('Ctrl Pts',(-1.56519944555977,105.627397397336,11.62499287277));
#67451=CARTESIAN_POINT('Ctrl Pts',(-0.351915110811561,105.783655138921,
11.1071017674458));
#67452=CARTESIAN_POINT('Ctrl Pts',(1.07203130124671,105.958158432415,11.312481396572));
#67453=CARTESIAN_POINT('Ctrl Pts',(1.94949122871948,106.102433978162,12.225849009996));
#67454=CARTESIAN_POINT('Ctrl Pts',(2.10957689837978,106.236348965585,13.306892868975));
#67455=CARTESIAN_POINT('Ctrl Pts',(1.94953009712914,106.350831732687,14.2217476886087));
#67456=CARTESIAN_POINT('Ctrl Pts',(1.34595533130063,106.464925023196,14.9768229353525));
#67457=CARTESIAN_POINT('Ctrl Pts',(0.599119934563651,106.564539550196,15.289885458982));
#67458=CARTESIAN_POINT('Ctrl Pts',(0.203649838264434,106.614303136798,15.3504467053623));
#67459=CARTESIAN_POINT('Ctrl Pts',(-0.0243263766015025,106.64273199432,
15.356481840032));
#67460=CARTESIAN_POINT('Ctrl Pts',(-0.593469803508126,106.713789322486,
15.3252154071703));
#67461=CARTESIAN_POINT('Ctrl Pts',(-1.52270748488062,106.834488942835,14.9007297892781));
#67462=CARTESIAN_POINT('Ctrl Pts',(-2.18898377466974,107.004930310548,13.6201299872355));
#67463=CARTESIAN_POINT('Ctrl Pts',(-1.92607846949404,107.175682280527,12.1985737492977));
#67464=CARTESIAN_POINT('Ctrl Pts',(-0.840309729499128,107.347013709955,
11.2361067404336));
#67465=CARTESIAN_POINT('Ctrl Pts',(0.169535831336823,107.466589847056,11.1724890461576));
#67466=CARTESIAN_POINT('Ctrl Pts',(0.666180101057831,107.531382033941,11.324791218162));
#67467=CARTESIAN_POINT('Ctrl Pts',(0.738790883742652,107.540984995144,11.3503133336356));
#67468=CARTESIAN_POINT('Ctrl Pts',(0.846634106957426,107.555393428296,11.3916272160638));
#67469=CARTESIAN_POINT('Ctrl Pts',(1.07401648099589,107.586634405511,11.4972844068827));
#67470=CARTESIAN_POINT('Ctrl Pts',(1.52273373306752,107.654037196072,11.804042311152));
#67471=CARTESIAN_POINT('Ctrl Pts',(1.9967268298589,107.750680601562,12.4403935395825));
#67472=CARTESIAN_POINT('Ctrl Pts',(2.18490022917524,107.867299542099,13.3797933847505));
#67473=CARTESIAN_POINT('Ctrl Pts',(1.99148579757452,107.965076000406,14.1588828236315));
#67474=CARTESIAN_POINT('Ctrl Pts',(1.71074153044894,108.028951655748,14.590898884757));
#67475=CARTESIAN_POINT('Ctrl Pts',(1.55574190339104,108.058495319469,14.769973722537));
#67476=CARTESIAN_POINT('Ctrl Pts',(1.44585607606784,108.078208256583,14.8835704792628));
#67477=CARTESIAN_POINT('Ctrl Pts',(1.29687288352194,108.102881966276,15.0140356843413));
#67478=CARTESIAN_POINT('Ctrl Pts',(1.10156630049055,108.132544513271,15.1502224385089));
#67479=CARTESIAN_POINT('Ctrl Pts',(0.822227619337672,108.172167789794,15.3021958157975));
#67480=CARTESIAN_POINT('Ctrl Pts',(0.292462013639442,108.241697602338,15.4859538200435));
#67481=CARTESIAN_POINT('Ctrl Pts',(-0.527870899667793,108.341603780246,
15.4877029851746));
#67482=CARTESIAN_POINT('Ctrl Pts',(-1.42639530611788,108.462467618126,15.0660623239948));
#67483=CARTESIAN_POINT('Ctrl Pts',(-2.06365860953833,108.584372632003,14.2939479126033));
#67484=CARTESIAN_POINT('Ctrl Pts',(-2.31212380606438,108.707368925733,13.3149675711768));
#67485=CARTESIAN_POINT('Ctrl Pts',(-2.11658312055525,108.831513517464,12.3145741411436));
#67486=CARTESIAN_POINT('Ctrl Pts',(-1.50630007764062,108.956855261822,11.4854580477888));
#67487=CARTESIAN_POINT('Ctrl Pts',(-0.591603229966188,109.083440171806,
10.9926973044355));
#67488=CARTESIAN_POINT('Ctrl Pts',(0.573863165244347,109.225516128066,10.9292815651746));
#67489=CARTESIAN_POINT('Ctrl Pts',(1.75863530343156,109.383687562582,11.5189168345029));
#67490=CARTESIAN_POINT('Ctrl Pts',(2.36645968899241,109.529504991381,12.5769886842501));
#67491=CARTESIAN_POINT('Ctrl Pts',(2.43848095796253,109.647408968564,13.5296536457081));
#67492=CARTESIAN_POINT('Ctrl Pts',(2.22110617041835,109.773575853537,14.5283583099813));
#67493=CARTESIAN_POINT('Ctrl Pts',(1.32892436585788,109.93875195499,15.6044418360144));
#67494=CARTESIAN_POINT('Ctrl Pts',(-0.375735547519591,110.144754052652,
15.9775159621844));
#67495=CARTESIAN_POINT('Ctrl Pts',(-1.9737793652605,110.354075777694,15.2116037190409));
#67496=CARTESIAN_POINT('Ctrl Pts',(-2.77568014980066,110.566727843583,13.5994221513611));
#67497=CARTESIAN_POINT('Ctrl Pts',(-2.41047606829342,110.782699052213,11.8077710606813));
#67498=CARTESIAN_POINT('Ctrl Pts',(-0.999571941372368,111.001956153692,
10.6014571112487));
#67499=CARTESIAN_POINT('Ctrl Pts',(0.917719561938274,111.228591161885,10.5161593504357));
#67500=CARTESIAN_POINT('Ctrl Pts',(1.97805596779178,111.383286307474,11.2968351135459));
#67501=CARTESIAN_POINT('Ctrl Pts',(2.32997171279836,111.463304468483,11.833078989016));
#67502=CARTESIAN_POINT('Ctrl Pts',(2.7350250627678,100.565914649707,13.1349774607871));
#67503=CARTESIAN_POINT('Ctrl Pts',(2.75828987751536,100.641394615982,13.7393067026489));
#67504=CARTESIAN_POINT('Ctrl Pts',(2.38883621085233,100.791283170442,14.9525898600523));
#67505=CARTESIAN_POINT('Ctrl Pts',(0.853814388784849,101.012798340815,16.0309818434995));
#67506=CARTESIAN_POINT('Ctrl Pts',(-0.990693997564699,101.230927937112,
15.9366569255174));
#67507=CARTESIAN_POINT('Ctrl Pts',(-2.36453761099378,101.445623540179,14.7462029197638));
#67508=CARTESIAN_POINT('Ctrl Pts',(-2.70846290528419,101.656859690671,12.9908051149541));
#67509=CARTESIAN_POINT('Ctrl Pts',(-1.91271849199191,101.864634679079,11.4221380670157));
#67510=CARTESIAN_POINT('Ctrl Pts',(-0.345220218849182,102.068970088513,
10.6875111735294));
#67511=CARTESIAN_POINT('Ctrl Pts',(1.12761078666161,102.247582961421,11.0260564432514));
#67512=CARTESIAN_POINT('Ctrl Pts',(2.02978845817633,102.401713603836,11.9143777693584));
#67513=CARTESIAN_POINT('Ctrl Pts',(2.40099633348103,102.532372787637,12.9206089815911));
#67514=CARTESIAN_POINT('Ctrl Pts',(2.32155473602545,102.640068998527,13.8014137470815));
#67515=CARTESIAN_POINT('Ctrl Pts',(2.04042327739136,102.725531871417,14.4305375031559));
#67516=CARTESIAN_POINT('Ctrl Pts',(1.73294787987584,102.789287051574,14.8422073252102));
#67517=CARTESIAN_POINT('Ctrl Pts',(1.08675397246322,102.894981011661,15.3981393559111));
#67518=CARTESIAN_POINT('Ctrl Pts',(-0.107798262522985,103.041406846351,
15.7265883341495));
#67519=CARTESIAN_POINT('Ctrl Pts',(-1.55609178504967,103.226820992556,15.114928889834));
#67520=CARTESIAN_POINT('Ctrl Pts',(-2.3100557009751,103.409569993268,13.764751187316));
#67521=CARTESIAN_POINT('Ctrl Pts',(-2.07657233044371,103.589839531357,12.25574673077));
#67522=CARTESIAN_POINT('Ctrl Pts',(-0.978293259986012,103.767838661493,
11.2240284707595));
#67523=CARTESIAN_POINT('Ctrl Pts',(0.505824718893558,103.94378910479,11.0877282259183));
#67524=CARTESIAN_POINT('Ctrl Pts',(1.53823343054539,104.088901615839,11.7529159505543));
#67525=CARTESIAN_POINT('Ctrl Pts',(1.98815714360423,104.204211265545,12.5745206037526));
#67526=CARTESIAN_POINT('Ctrl Pts',(2.14997538233027,104.319040278266,13.4938693028453));
#67527=CARTESIAN_POINT('Ctrl Pts',(1.86680224060572,104.423703461249,14.3321886289457));
#67528=CARTESIAN_POINT('Ctrl Pts',(1.33519004568128,104.518462432909,14.8815871128114));
#67529=CARTESIAN_POINT('Ctrl Pts',(0.953517632224392,104.57521535734,15.1336375379699));
#67530=CARTESIAN_POINT('Ctrl Pts',(0.526144620101407,104.631871318099,15.2952896845308));
#67531=CARTESIAN_POINT('Ctrl Pts',(0.0746163309989309,104.688442224242,
15.3594388574662));
#67532=CARTESIAN_POINT('Ctrl Pts',(-0.379451802549797,104.744941314744,
15.3229864961564));
#67533=CARTESIAN_POINT('Ctrl Pts',(-0.886493821270294,104.81077830402,15.1657753632491));
#67534=CARTESIAN_POINT('Ctrl Pts',(-1.39812488696955,104.885933683268,14.8327246947727));
#67535=CARTESIAN_POINT('Ctrl Pts',(-1.82040132459206,104.97039549147,14.291649822032));
#67536=CARTESIAN_POINT('Ctrl Pts',(-2.04257232601797,105.054807292785,13.6430127721351));
#67537=CARTESIAN_POINT('Ctrl Pts',(-2.04429738877112,105.16733669875,12.7292184760357));
#67538=CARTESIAN_POINT('Ctrl Pts',(-1.47618580737732,105.308051288373,11.6792434394121));
#67539=CARTESIAN_POINT('Ctrl Pts',(-0.310987711005822,105.458469259206,
11.1746059827715));
#67540=CARTESIAN_POINT('Ctrl Pts',(1.07482852737057,105.628224940062,11.3675409043566));
#67541=CARTESIAN_POINT('Ctrl Pts',(1.94561023182653,105.77038559597,12.260802758842));
#67542=CARTESIAN_POINT('Ctrl Pts',(2.11090714092915,105.90391847257,13.338144627919));
#67543=CARTESIAN_POINT('Ctrl Pts',(1.95484752248664,106.018817460528,14.2568499545763));
#67544=CARTESIAN_POINT('Ctrl Pts',(1.34860807201228,106.134442677004,15.0260653871728));
#67545=CARTESIAN_POINT('Ctrl Pts',(0.586233187321556,106.236366677432,15.3506553297297));
#67546=CARTESIAN_POINT('Ctrl Pts',(0.18007436062856,106.287525992374,15.4150159625443));
#67547=CARTESIAN_POINT('Ctrl Pts',(-0.0547848935300436,106.316820731045,
15.4224553598979));
#67548=CARTESIAN_POINT('Ctrl Pts',(-0.642226182825883,106.390156853716,
15.3932653310122));
#67549=CARTESIAN_POINT('Ctrl Pts',(-1.6110328856081,106.515601660566,14.9592950074042));
#67550=CARTESIAN_POINT('Ctrl Pts',(-2.32193062869885,106.694881965519,13.6179213451299));
#67551=CARTESIAN_POINT('Ctrl Pts',(-2.0539749237069,106.876553338331,12.1035996949379));
#67552=CARTESIAN_POINT('Ctrl Pts',(-0.89460506092996,107.060812668511,11.0595540521907));
#67553=CARTESIAN_POINT('Ctrl Pts',(0.201537537343257,107.190697367659,10.9818333671775));
#67554=CARTESIAN_POINT('Ctrl Pts',(0.744683028998303,107.261427674696,11.1446008708961));
#67555=CARTESIAN_POINT('Ctrl Pts',(0.824155924584212,107.27191655592,11.1719648240295));
#67556=CARTESIAN_POINT('Ctrl Pts',(0.942260606101615,107.287660128272,11.2163440991875));
#67557=CARTESIAN_POINT('Ctrl Pts',(1.191643104641,107.321827334384,11.3302723880277));
#67558=CARTESIAN_POINT('Ctrl Pts',(1.68560290973175,107.395706991298,11.6631765731265));
#67559=CARTESIAN_POINT('Ctrl Pts',(2.21223251912034,107.502088731704,12.3597762762018));
#67560=CARTESIAN_POINT('Ctrl Pts',(2.42787982712146,107.631132858374,13.3975811084991));
#67561=CARTESIAN_POINT('Ctrl Pts',(2.2190672073106,107.739851026604,14.265222041048));
#67562=CARTESIAN_POINT('Ctrl Pts',(1.90922083577811,107.811107329933,14.7492153605674));
#67563=CARTESIAN_POINT('Ctrl Pts',(1.73745720780343,107.844108613953,14.9503722674611));
#67564=CARTESIAN_POINT('Ctrl Pts',(1.61552354611335,107.866139958883,15.0781315588876));
#67565=CARTESIAN_POINT('Ctrl Pts',(1.44990819593871,107.893736454049,15.225148052992));
#67566=CARTESIAN_POINT('Ctrl Pts',(1.23232670063248,107.926944723774,15.3790623584201));
#67567=CARTESIAN_POINT('Ctrl Pts',(0.920510137608981,107.971346183998,15.5514462974916));
#67568=CARTESIAN_POINT('Ctrl Pts',(0.327550660059198,108.049372351337,15.76169076905));
#67569=CARTESIAN_POINT('Ctrl Pts',(-0.595212551922845,108.161775445127,
15.7702198399133));
#67570=CARTESIAN_POINT('Ctrl Pts',(-1.61239066681261,108.298172360322,15.3016610119433));
#67571=CARTESIAN_POINT('Ctrl Pts',(-2.33940298117849,108.436096905661,14.4332844847565));
#67572=CARTESIAN_POINT('Ctrl Pts',(-2.62878807512887,108.575555925357,13.325428470963));
#67573=CARTESIAN_POINT('Ctrl Pts',(-2.41454707564966,108.716553833851,12.1878943594883));
#67574=CARTESIAN_POINT('Ctrl Pts',(-1.72705825835735,108.859089142338,11.2404857576132));
#67575=CARTESIAN_POINT('Ctrl Pts',(-0.689947399372223,109.003156154794,
10.6727948115623));
#67576=CARTESIAN_POINT('Ctrl Pts',(0.6363577510161,109.164921533284,10.5918456048832));
#67577=CARTESIAN_POINT('Ctrl Pts',(1.98944023319231,109.345011904906,11.2544184786604));
#67578=CARTESIAN_POINT('Ctrl Pts',(2.68844875082447,109.510923958626,12.4538207074574));
#67579=CARTESIAN_POINT('Ctrl Pts',(2.777042909228,109.644937957605,13.5359666031841));
#67580=CARTESIAN_POINT('Ctrl Pts',(2.5372112677193,109.788226044324,14.6715847675353));
#67581=CARTESIAN_POINT('Ctrl Pts',(1.53268170387733,109.975514990703,15.8973704375427));
#67582=CARTESIAN_POINT('Ctrl Pts',(-0.391965390180126,110.20840070075,16.3295413786689));
#67583=CARTESIAN_POINT('Ctrl Pts',(-2.19618012843552,110.444168767888,15.4762171137414));
#67584=CARTESIAN_POINT('Ctrl Pts',(-3.10425034855693,110.682653070405,13.6727436701643));
#67585=CARTESIAN_POINT('Ctrl Pts',(-2.70596752170842,110.9236679908,11.6716072659118));
#67586=CARTESIAN_POINT('Ctrl Pts',(-1.14600188343656,111.167012278533,10.3260453172688));
#67587=CARTESIAN_POINT('Ctrl Pts',(0.968650379207943,111.417041212691,10.2232893908503));
#67588=CARTESIAN_POINT('Ctrl Pts',(2.13392863603529,111.586579386555,11.0744839374344));
#67589=CARTESIAN_POINT('Ctrl Pts',(2.52097553229361,111.673954735715,11.6580819934878));
#67590=CARTESIAN_POINT('Ctrl Pts',(2.49283099999093,100.794479445797,13.1108080195032));
#67591=CARTESIAN_POINT('Ctrl Pts',(2.51515719970202,100.863431279975,13.6628077855728));
#67592=CARTESIAN_POINT('Ctrl Pts',(2.17968843256609,100.999744013118,14.7663369503664));
#67593=CARTESIAN_POINT('Ctrl Pts',(0.795914331805827,101.1994864983,15.7392516655857));
#67594=CARTESIAN_POINT('Ctrl Pts',(-0.853766209202168,101.394579343051,
15.6554435518708));
#67595=CARTESIAN_POINT('Ctrl Pts',(-2.07338251428329,101.585126420958,14.5992895565228));
#67596=CARTESIAN_POINT('Ctrl Pts',(-2.3769033064482,101.771265881478,13.0525813475902));
#67597=CARTESIAN_POINT('Ctrl Pts',(-1.68070836712873,101.953168845295,11.6790615543513));
#67598=CARTESIAN_POINT('Ctrl Pts',(-0.316585819691275,102.131026046402,
11.0391790038355));
#67599=CARTESIAN_POINT('Ctrl Pts',(0.95913378208078,102.285723454486,11.3318051599028));
#67600=CARTESIAN_POINT('Ctrl Pts',(1.7385263897513,102.418771549116,12.0978996555273));
#67601=CARTESIAN_POINT('Ctrl Pts',(2.05900879000914,102.53130516533,12.9642472996834));
#67602=CARTESIAN_POINT('Ctrl Pts',(1.99140764775307,102.623895737268,13.7215605251988));
#67603=CARTESIAN_POINT('Ctrl Pts',(1.7505100490346,102.697301489324,14.2621652806589));
#67604=CARTESIAN_POINT('Ctrl Pts',(1.48692355688233,102.752034803086,14.6158543164599));
#67605=CARTESIAN_POINT('Ctrl Pts',(0.932904994664702,102.842734592139,15.0934843577826));
#67606=CARTESIAN_POINT('Ctrl Pts',(-0.0914144687160896,102.968333415228,
15.3762721980933));
#67607=CARTESIAN_POINT('Ctrl Pts',(-1.33485789371615,103.127446017604,14.853019541222));
#67608=CARTESIAN_POINT('Ctrl Pts',(-1.9848419465324,103.284558264171,13.6933545546193));
#67609=CARTESIAN_POINT('Ctrl Pts',(-1.7859198054212,103.440023723922,12.3916974239502));
#67610=CARTESIAN_POINT('Ctrl Pts',(-0.836554893827291,103.594221052691,
11.4959387949505));
#67611=CARTESIAN_POINT('Ctrl Pts',(0.456174919648817,103.747531635336,11.3738488107031));
#67612=CARTESIAN_POINT('Ctrl Pts',(1.3638147823984,103.874871679777,11.9549038831241));
#67613=CARTESIAN_POINT('Ctrl Pts',(1.76271423183761,103.976693557164,12.6795595279847));
#67614=CARTESIAN_POINT('Ctrl Pts',(1.90810598694439,104.078542102711,13.4945344024168));
#67615=CARTESIAN_POINT('Ctrl Pts',(1.65790918644532,104.17203697728,14.2442552014034));
#67616=CARTESIAN_POINT('Ctrl Pts',(1.18092989180617,104.257276104356,14.7396737469657));
#67617=CARTESIAN_POINT('Ctrl Pts',(0.836952047812147,104.308512974323,14.9680700673282));
#67618=CARTESIAN_POINT('Ctrl Pts',(0.450100297839354,104.359851063443,15.1155674993526));
#67619=CARTESIAN_POINT('Ctrl Pts',(0.0395872801241101,104.411306853854,
15.1750254409463));
#67620=CARTESIAN_POINT('Ctrl Pts',(-0.375108892402885,104.462898554674,
15.1429069972814));
#67621=CARTESIAN_POINT('Ctrl Pts',(-0.840313267844409,104.523254297577,
15.0001497606756));
#67622=CARTESIAN_POINT('Ctrl Pts',(-1.31270319649571,104.592502929932,14.6948548388226));
#67623=CARTESIAN_POINT('Ctrl Pts',(-1.70591154338413,104.670811240362,14.1946222164672));
#67624=CARTESIAN_POINT('Ctrl Pts',(-1.91536791775402,104.749572649424,13.5901594840855));
#67625=CARTESIAN_POINT('Ctrl Pts',(-1.92018868414222,104.85525116503,12.7322430362218));
#67626=CARTESIAN_POINT('Ctrl Pts',(-1.38717216919487,104.98870517941,11.7334940060542));
#67627=CARTESIAN_POINT('Ctrl Pts',(-0.270060311200083,105.13328337949,11.2421101980971));
#67628=CARTESIAN_POINT('Ctrl Pts',(1.07762575349443,105.29829144771,11.4226004121413));
#67629=CARTESIAN_POINT('Ctrl Pts',(1.94172923493356,105.438337213777,12.2957565076881));
#67630=CARTESIAN_POINT('Ctrl Pts',(2.11223738347851,105.571487979555,13.3693963868629));
#67631=CARTESIAN_POINT('Ctrl Pts',(1.96016494784412,105.686803188369,14.291952220544));
#67632=CARTESIAN_POINT('Ctrl Pts',(1.35126081272394,105.803960330811,15.0753078389932));
#67633=CARTESIAN_POINT('Ctrl Pts',(0.573346440079449,105.908193804669,15.4114252004776));
#67634=CARTESIAN_POINT('Ctrl Pts',(0.156498882992677,105.96074884795,15.4795852197261));
#67635=CARTESIAN_POINT('Ctrl Pts',(-0.0852434104585933,105.99090946777,
15.4884288797639));
#67636=CARTESIAN_POINT('Ctrl Pts',(-0.690982562143647,106.066524384947,
15.4613152548541));
#67637=CARTESIAN_POINT('Ctrl Pts',(-1.69935828633558,106.196714378299,15.0178602255304));
#67638=CARTESIAN_POINT('Ctrl Pts',(-2.45487748272796,106.384833620489,13.6157127030245));
#67639=CARTESIAN_POINT('Ctrl Pts',(-2.18187137791978,106.577424396135,12.0086256405781));
#67640=CARTESIAN_POINT('Ctrl Pts',(-0.948900392360805,106.774611627066,
10.8830013639477));
#67641=CARTESIAN_POINT('Ctrl Pts',(0.233539243349673,106.914804888263,10.7911776881976));
#67642=CARTESIAN_POINT('Ctrl Pts',(0.823185956938756,106.991473315452,10.9644105236304));
#67643=CARTESIAN_POINT('Ctrl Pts',(0.909520965425754,107.002848116697,10.9936163144232));
#67644=CARTESIAN_POINT('Ctrl Pts',(1.03788710524578,107.019926828246,11.0410609823112));
#67645=CARTESIAN_POINT('Ctrl Pts',(1.30926972828611,107.057020263259,11.1632603691728));
#67646=CARTESIAN_POINT('Ctrl Pts',(1.84847208639594,107.137376786525,11.5223108351008));
#67647=CARTESIAN_POINT('Ctrl Pts',(2.42773820838176,107.253496861847,12.2791590128213));
#67648=CARTESIAN_POINT('Ctrl Pts',(2.67085942506765,107.394966174649,13.4153688322477));
#67649=CARTESIAN_POINT('Ctrl Pts',(2.44664861704666,107.514626052802,14.3715612584646));
#67650=CARTESIAN_POINT('Ctrl Pts',(2.10770014110726,107.593263004116,14.907531836378));
#67651=CARTESIAN_POINT('Ctrl Pts',(1.9191725122158,107.629721908436,15.1307708123851));
#67652=CARTESIAN_POINT('Ctrl Pts',(1.78519101615885,107.654071661183,15.2726926385123));
#67653=CARTESIAN_POINT('Ctrl Pts',(1.60294350835546,107.684590941821,15.4362604216428));
#67654=CARTESIAN_POINT('Ctrl Pts',(1.36308710077436,107.721344934276,15.6079022783315));
#67655=CARTESIAN_POINT('Ctrl Pts',(1.01879265588027,107.770524578201,15.8006967791856));
#67656=CARTESIAN_POINT('Ctrl Pts',(0.362639306478935,107.857047100334,16.0374277180563));
#67657=CARTESIAN_POINT('Ctrl Pts',(-0.662554204177914,107.981947110009,
16.052736694652));
#67658=CARTESIAN_POINT('Ctrl Pts',(-1.79838602750735,108.133877102516,15.5372596998919));
#67659=CARTESIAN_POINT('Ctrl Pts',(-2.61514735281868,108.287821179317,14.5726210569098));
#67660=CARTESIAN_POINT('Ctrl Pts',(-2.94545234419337,108.443742924981,13.3358893707492));
#67661=CARTESIAN_POINT('Ctrl Pts',(-2.71251103074408,108.601594150237,12.0612145778331));
#67662=CARTESIAN_POINT('Ctrl Pts',(-1.94781643907409,108.761323022852,10.9955134674375));
#67663=CARTESIAN_POINT('Ctrl Pts',(-0.788291568778272,108.922872137781,
10.3528923186892));
#67664=CARTESIAN_POINT('Ctrl Pts',(0.698852336787839,109.104326938504,10.2544096445917));
#67665=CARTESIAN_POINT('Ctrl Pts',(2.22024516295304,109.306336247231,10.9899201228179));
#67666=CARTESIAN_POINT('Ctrl Pts',(3.01043781265651,109.492342925873,12.3306527306649));
#67667=CARTESIAN_POINT('Ctrl Pts',(3.11560486049346,109.642466946645,13.5422795606599));
#67668=CARTESIAN_POINT('Ctrl Pts',(2.85331636502024,109.80287623511,14.8148112250893));
#67669=CARTESIAN_POINT('Ctrl Pts',(1.73643904189676,110.012278026417,16.190299039071));
#67670=CARTESIAN_POINT('Ctrl Pts',(-0.408195232840666,110.272047348849,
16.6815667951534));
#67671=CARTESIAN_POINT('Ctrl Pts',(-2.41858089161053,110.534261758082,15.7408305084419));
#67672=CARTESIAN_POINT('Ctrl Pts',(-3.43282054731318,110.798578297227,13.7460651889675));
#67673=CARTESIAN_POINT('Ctrl Pts',(-3.00145897512342,111.064636929387,11.5354434711421));
#67674=CARTESIAN_POINT('Ctrl Pts',(-1.29243182550077,111.332068403376,10.0506335232888));
#67675=CARTESIAN_POINT('Ctrl Pts',(1.01958119647761,111.605491263496,9.93041943126484));
#67676=CARTESIAN_POINT('Ctrl Pts',(2.2898013042788,111.789872465636,10.8521327613231));
#67677=CARTESIAN_POINT('Ctrl Pts',(2.71197935178886,111.884605002945,11.4830849979595));
#67678=CARTESIAN_POINT('Ctrl Pts',(2.31220144791066,104.895136985459,14.2499282950331));
#67679=CARTESIAN_POINT('Ctrl Pts',(2.27420039961476,104.906599180693,14.3345491847664));
#67680=CARTESIAN_POINT('Ctrl Pts',(2.23140315805251,104.917892748149,14.4168838347965));
#67681=CARTESIAN_POINT('Ctrl Pts',(2.18421017770141,104.92913510024,14.4964371151384));
#67682=CARTESIAN_POINT('Ctrl Pts',(2.15840306163429,104.935282893473,14.5399402108113));
#67683=CARTESIAN_POINT('Ctrl Pts',(2.13128235315898,104.941415302853,14.5826113449346));
#67684=CARTESIAN_POINT('Ctrl Pts',(2.1029200134062,104.947551014578,14.6243685072651));
#67685=CARTESIAN_POINT('Ctrl Pts',(2.07259601784244,104.954111097306,14.6690137663058));
#67686=CARTESIAN_POINT('Ctrl Pts',(2.04084876730712,104.9606764644,14.7126201487188));
#67687=CARTESIAN_POINT('Ctrl Pts',(2.00775362174451,104.967273385227,14.7551051400211));
#67688=CARTESIAN_POINT('Ctrl Pts',(1.92026468474914,104.984712728088,14.867416678892));
#67689=CARTESIAN_POINT('Ctrl Pts',(1.82334397601601,105.002375722057,14.9719076479643));
#67690=CARTESIAN_POINT('Ctrl Pts',(1.71867319953035,105.020116808472,15.0672745496425));
#67691=CARTESIAN_POINT('Ctrl Pts',(1.68902870082,105.025141378185,15.0942840368053));
#67692=CARTESIAN_POINT('Ctrl Pts',(1.65876324929722,105.030172047059,15.1205608831828));
#67693=CARTESIAN_POINT('Ctrl Pts',(1.62791693994719,105.035205272825,15.1460740158455));
#67694=CARTESIAN_POINT('Ctrl Pts',(1.52002140916941,105.052810703653,15.2353149347254));
#67695=CARTESIAN_POINT('Ctrl Pts',(1.40501478746162,105.070451758976,15.3152168018034));
#67696=CARTESIAN_POINT('Ctrl Pts',(1.28446866836278,105.088008386665,15.3845447744751));
#67697=CARTESIAN_POINT('Ctrl Pts',(1.24873987207963,105.093212014777,15.4050929682356));
#67698=CARTESIAN_POINT('Ctrl Pts',(1.2125249485834,105.098407899999,15.4247118951434));
#67699=CARTESIAN_POINT('Ctrl Pts',(1.17586637806379,105.103592191453,15.4433687062027));
#67700=CARTESIAN_POINT('Ctrl Pts',(1.12459789858549,105.110842630742,15.4694610038937));
#67701=CARTESIAN_POINT('Ctrl Pts',(1.07246073447628,105.118070378548,15.4936716081275));
#67702=CARTESIAN_POINT('Ctrl Pts',(1.01958922738601,105.125241585622,15.5159221619009));
#67703=CARTESIAN_POINT('Ctrl Pts',(1.01956424715919,105.125244973806,15.5159326746309));
#67704=CARTESIAN_POINT('Ctrl Pts',(1.01953926676833,105.125248361977,15.5159431869236));
#67705=CARTESIAN_POINT('Ctrl Pts',(1.01951428621352,105.125251750135,15.5159536987788));
#67706=CARTESIAN_POINT('Ctrl Pts',(0.937462525771387,105.136380581006,15.5504812036761));
#67707=CARTESIAN_POINT('Ctrl Pts',(0.853515168959687,105.147382834861,15.580345047422));
#67708=CARTESIAN_POINT('Ctrl Pts',(0.768280266695011,105.158332912142,15.6054595511352));
#67709=CARTESIAN_POINT('Ctrl Pts',(0.736515636026395,105.162413695381,15.6148190143795));
#67710=CARTESIAN_POINT('Ctrl Pts',(0.704572600040203,105.166487200638,15.6235191907505));
#67711=CARTESIAN_POINT('Ctrl Pts',(0.672484017712271,105.170557164629,15.6315568484486));
#67712=CARTESIAN_POINT('Ctrl Pts',(0.543653859675258,105.186897372456,15.6638266664454));
#67713=CARTESIAN_POINT('Ctrl Pts',(0.412461897545337,105.203187832181,15.6854181899435));
#67714=CARTESIAN_POINT('Ctrl Pts',(0.280754984522898,105.219568177955,15.6963245673514));
#67715=CARTESIAN_POINT('Ctrl Pts',(0.235205809239355,105.225233114015,15.7000964004683));
#67716=CARTESIAN_POINT('Ctrl Pts',(0.189594149019697,105.23090875347,15.7025904915425));
#67717=CARTESIAN_POINT('Ctrl Pts',(0.143993589047487,105.236600494221,15.7038067337658));
#67718=CARTESIAN_POINT('Ctrl Pts',(0.0214336593638503,105.251898099046,
15.7070756094429));
#67719=CARTESIAN_POINT('Ctrl Pts',(-0.101053045992834,105.26731534126,15.7011142175678));
#67720=CARTESIAN_POINT('Ctrl Pts',(-0.222054613535675,105.282761645719,
15.6860517097815));
#67721=CARTESIAN_POINT('Ctrl Pts',(-0.231879006231722,105.284015766338,
15.6848287504886));
#67722=CARTESIAN_POINT('Ctrl Pts',(-0.241693629493812,105.285270081524,
15.683545775842));
#67723=CARTESIAN_POINT('Ctrl Pts',(-0.251497738146157,105.286524544392,
15.6822028442612));
#67724=CARTESIAN_POINT('Ctrl Pts',(-0.295773122662273,105.292189702523,
15.6761381611544));
#67725=CARTESIAN_POINT('Ctrl Pts',(-0.339832900064291,105.297857415166,
15.6688511049375));
#67726=CARTESIAN_POINT('Ctrl Pts',(-0.383605439801159,105.303522213605,
15.6603482858131));
#67727=CARTESIAN_POINT('Ctrl Pts',(-0.474632834078136,105.31530247228,15.642666207653));
#67728=CARTESIAN_POINT('Ctrl Pts',(-0.564428333984754,105.327071019503,
15.6197226781248));
#67729=CARTESIAN_POINT('Ctrl Pts',(-0.652325899701623,105.338715235235,
15.5916425343705));
#67730=CARTESIAN_POINT('Ctrl Pts',(-0.683819847232622,105.342887390815,
15.581581339082));
#67731=CARTESIAN_POINT('Ctrl Pts',(-0.715070591587191,105.347043635564,
15.5708608561379));
#67732=CARTESIAN_POINT('Ctrl Pts',(-0.746049078785308,105.35117896166,15.5594872212166));
#67733=CARTESIAN_POINT('Ctrl Pts',(-0.746050762019458,105.351179186355,
15.5594866032235));
#67734=CARTESIAN_POINT('Ctrl Pts',(-0.746052445252847,105.35117941105,15.5594859852285));
#67735=CARTESIAN_POINT('Ctrl Pts',(-0.746054128485389,105.351179635746,
15.5594853672316));
#67736=CARTESIAN_POINT('Ctrl Pts',(-0.793086767511783,105.357458037176,
15.542217386672));
#67737=CARTESIAN_POINT('Ctrl Pts',(-0.839532451831011,105.36369197631,15.5234300496359));
#67738=CARTESIAN_POINT('Ctrl Pts',(-0.88529182882496,105.369902005009,15.503181560758));
#67739=CARTESIAN_POINT('Ctrl Pts',(-0.982641150680751,105.383113331785,
15.4601045612367));
#67740=CARTESIAN_POINT('Ctrl Pts',(-1.07687862515342,105.396215416679,15.4104165331654));
#67741=CARTESIAN_POINT('Ctrl Pts',(-1.16722703977509,105.409290524897,15.3547778569735));
#67742=CARTESIAN_POINT('Ctrl Pts',(-1.19234182397621,105.412925104681,15.3393115828651));
#67743=CARTESIAN_POINT('Ctrl Pts',(-1.21715597278025,105.416557568954,15.3233857783956));
#67744=CARTESIAN_POINT('Ctrl Pts',(-1.24165254843071,105.420189612386,15.3070152965456));
#67745=CARTESIAN_POINT('Ctrl Pts',(-1.33468628106446,105.433983481476,15.2448430544639));
#67746=CARTESIAN_POINT('Ctrl Pts',(-1.42314424358298,105.447773826133,15.1762536441637));
#67747=CARTESIAN_POINT('Ctrl Pts',(-1.50617387261965,105.461660206449,15.1020104225316));
#67748=CARTESIAN_POINT('Ctrl Pts',(-1.51634606224985,105.463361465331,15.0929146799881));
#67749=CARTESIAN_POINT('Ctrl Pts',(-1.52643671658802,105.465064157184,15.0837341006866));
#67750=CARTESIAN_POINT('Ctrl Pts',(-1.53644421913697,105.466768457951,15.0744701109921));
#67751=CARTESIAN_POINT('Ctrl Pts',(-1.61677973838047,105.480449782181,15.0001031629209));
#67752=CARTESIAN_POINT('Ctrl Pts',(-1.6917708061302,105.494237643618,14.9203492168783));
#67753=CARTESIAN_POINT('Ctrl Pts',(-1.76073527650109,105.508034423551,14.8360397261554));
#67754=CARTESIAN_POINT('Ctrl Pts',(-1.77675949669865,105.511240170488,14.8164500180518));
#67755=CARTESIAN_POINT('Ctrl Pts',(-1.79245844556267,105.514446426784,14.7966141639437));
#67756=CARTESIAN_POINT('Ctrl Pts',(-1.80782371518128,105.517652018906,14.7765422221908));
#67757=CARTESIAN_POINT('Ctrl Pts',(-1.86879426141414,105.530372049695,14.6968952467062));
#67758=CARTESIAN_POINT('Ctrl Pts',(-1.92450788267108,105.543079431336,14.6135337054796));
#67759=CARTESIAN_POINT('Ctrl Pts',(-1.97441075903152,105.555687562119,14.5271518064505));
#67760=CARTESIAN_POINT('Ctrl Pts',(-1.98624318030295,105.558677063441,14.5066698804758));
#67761=CARTESIAN_POINT('Ctrl Pts',(-1.99774912755194,105.561661009207,14.4860180562287));
#67762=CARTESIAN_POINT('Ctrl Pts',(-2.00892160078681,105.564638290794,14.4652053898462));
#67763=CARTESIAN_POINT('Ctrl Pts',(-2.01763154882185,105.566959349647,14.448980043958));
#67764=CARTESIAN_POINT('Ctrl Pts',(-2.02613860509512,105.569276332924,14.4326572761255));
#67765=CARTESIAN_POINT('Ctrl Pts',(-2.03444811357903,105.571579479006,14.4162461873535));
#67766=CARTESIAN_POINT('Ctrl Pts',(-2.03446150325956,105.571583190223,14.4162197430414));
#67767=CARTESIAN_POINT('Ctrl Pts',(-2.03447489240929,105.571586901433,14.4161932984712));
#67768=CARTESIAN_POINT('Ctrl Pts',(-2.03448828102828,105.571590612637,14.4161668536429));
#67769=CARTESIAN_POINT('Ctrl Pts',(-2.07648480457982,105.583231668721,14.3332164869913));
#67770=CARTESIAN_POINT('Ctrl Pts',(-2.1132550838095,105.594807933288,14.2477244678497));
#67771=CARTESIAN_POINT('Ctrl Pts',(-2.14472416620306,105.606305480878,14.1604491939523));
#67772=CARTESIAN_POINT('Ctrl Pts',(-2.1564212796263,105.610579139594,14.1280088207297));
#67773=CARTESIAN_POINT('Ctrl Pts',(-2.16738644906337,105.614841927265,14.0953222879995));
#67774=CARTESIAN_POINT('Ctrl Pts',(-2.17761752864817,105.619093145075,14.0624291555584));
#67775=CARTESIAN_POINT('Ctrl Pts',(-2.20744654807204,105.631487698118,13.9665282412546));
#67776=CARTESIAN_POINT('Ctrl Pts',(-2.23099406701571,105.643826754511,13.8688475741174));
#67777=CARTESIAN_POINT('Ctrl Pts',(-2.24813593865129,105.656199546234,13.7702733671563));
#67778=CARTESIAN_POINT('Ctrl Pts',(-2.249751117528,105.657365362445,13.7609852928867));
#67779=CARTESIAN_POINT('Ctrl Pts',(-2.2513094271258,105.658531473181,13.7516893235597));
#67780=CARTESIAN_POINT('Ctrl Pts',(-2.25281076541762,105.659697949965,13.7423862242467));
#67781=CARTESIAN_POINT('Ctrl Pts',(-2.27308663248914,105.675451446922,13.6167460497098));
#67782=CARTESIAN_POINT('Ctrl Pts',(-2.28297344172099,105.691275271019,13.4897921642673));
#67783=CARTESIAN_POINT('Ctrl Pts',(-2.28243769111326,105.707173664902,13.3633101936904));
#67784=CARTESIAN_POINT('Ctrl Pts',(-2.28204297258892,105.718886933132,13.2701235951838));
#67785=CARTESIAN_POINT('Ctrl Pts',(-2.27598992932626,105.73064025116,13.177196942669));
#67786=CARTESIAN_POINT('Ctrl Pts',(-2.2643692664422,105.742346446779,13.0852252627368));
#67787=CARTESIAN_POINT('Ctrl Pts',(-2.26025649785685,105.746489486988,13.0526747757515));
#67788=CARTESIAN_POINT('Ctrl Pts',(-2.255446294118,105.750626683126,13.02024343671));
#67789=CARTESIAN_POINT('Ctrl Pts',(-2.24994239248223,105.754754364393,12.9879605246861));
#67790=CARTESIAN_POINT('Ctrl Pts',(-2.23586841052012,105.765309224481,12.9054101537717));
#67791=CARTESIAN_POINT('Ctrl Pts',(-2.21733181160476,105.77574347324,12.8238073247741));
#67792=CARTESIAN_POINT('Ctrl Pts',(-2.1941782950671,105.786163606793,12.7436717166253));
#67793=CARTESIAN_POINT('Ctrl Pts',(-2.19415222754999,105.786175338359,12.7435814954991));
#67794=CARTESIAN_POINT('Ctrl Pts',(-2.19412615413402,105.786187069927,12.7434912760791));
#67795=CARTESIAN_POINT('Ctrl Pts',(-2.19410007481906,105.786198801498,12.7434010583658));
#67796=CARTESIAN_POINT('Ctrl Pts',(-2.17084996842585,105.796657675197,12.6629705932076));
#67797=CARTESIAN_POINT('Ctrl Pts',(-2.14290692946814,105.807118255861,12.5838976670209));
#67798=CARTESIAN_POINT('Ctrl Pts',(-2.11062188922789,105.817566777419,12.5066962471183));
#67799=CARTESIAN_POINT('Ctrl Pts',(-2.09218205364603,105.823534526511,12.4626020945604));
#67800=CARTESIAN_POINT('Ctrl Pts',(-2.07232676388679,105.82949834534,12.419118288576));
#67801=CARTESIAN_POINT('Ctrl Pts',(-2.05112860949134,105.835455698038,12.3763382896272));
#67802=CARTESIAN_POINT('Ctrl Pts',(-2.01005570878195,105.846998483854,12.2934490618013));
#67803=CARTESIAN_POINT('Ctrl Pts',(-1.96394352830422,105.858516221837,12.2132085252751));
#67804=CARTESIAN_POINT('Ctrl Pts',(-1.91337228647697,105.869950662046,12.1361612675599));
#67805=CARTESIAN_POINT('Ctrl Pts',(-1.88610183507187,105.876116663409,12.0946136720985));
#67806=CARTESIAN_POINT('Ctrl Pts',(-1.85753493633608,105.882258518483,12.0539937768536));
#67807=CARTESIAN_POINT('Ctrl Pts',(-1.82776294759618,105.88836763039,12.0143806935106));
#67808=CARTESIAN_POINT('Ctrl Pts',(-1.77363839518428,105.899473806416,11.9423653362456));
#67809=CARTESIAN_POINT('Ctrl Pts',(-1.71541761572262,105.91056647888,11.8737411495443));
#67810=CARTESIAN_POINT('Ctrl Pts',(-1.65346856418764,105.921727293805,11.8090617901708));
#67811=CARTESIAN_POINT('Ctrl Pts',(-1.62305798741109,105.927206099546,11.7773109146473));
#67812=CARTESIAN_POINT('Ctrl Pts',(-1.59174923650817,105.932701220555,11.7465114045834));
#67813=CARTESIAN_POINT('Ctrl Pts',(-1.55958800014773,105.938221698182,11.7167327888761));
#67814=CARTESIAN_POINT('Ctrl Pts',(-1.5543975039448,105.939112647082,11.7119268233956));
#67815=CARTESIAN_POINT('Ctrl Pts',(-1.54918476732884,105.940004254391,11.7071473973373));
#67816=CARTESIAN_POINT('Ctrl Pts',(-1.54394998157397,105.940896547551,11.7023947818719));
#67817=CARTESIAN_POINT('Ctrl Pts',(-1.47945933338536,105.951889273317,11.6438442955078));
#67818=CARTESIAN_POINT('Ctrl Pts',(-1.41180652123641,105.962801288623,11.5891520869799));
#67819=CARTESIAN_POINT('Ctrl Pts',(-1.34129713765614,105.973662939573,11.5387351859745));
#67820=CARTESIAN_POINT('Ctrl Pts',(-1.30255702088344,105.979630678968,11.5110345235507));
#67821=CARTESIAN_POINT('Ctrl Pts',(-1.26295418549131,105.985583188231,11.4846252713274));
#67822=CARTESIAN_POINT('Ctrl Pts',(-1.22253722997851,105.99152530639,11.459583012843));
#67823=CARTESIAN_POINT('Ctrl Pts',(-1.21331913596365,105.992880554531,11.4538715016685));
#67824=CARTESIAN_POINT('Ctrl Pts',(-1.20405865225382,105.99423566561,11.4482319331064));
#67825=CARTESIAN_POINT('Ctrl Pts',(-1.19475662808346,105.995590629736,11.4426653275844));
#67826=CARTESIAN_POINT('Ctrl Pts',(-1.19467046260739,105.995603180889,11.4426137636231));
#67827=CARTESIAN_POINT('Ctrl Pts',(-1.19458429352618,105.995615732036,11.4425622058978));
#67828=CARTESIAN_POINT('Ctrl Pts',(-1.19449812084045,105.995628283176,11.4425106544095));
#67829=CARTESIAN_POINT('Ctrl Pts',(-1.11827078254639,106.006730872859,11.3969088177554));
#67830=CARTESIAN_POINT('Ctrl Pts',(-1.03922131389124,106.017828090831,11.3561914637407));
#67831=CARTESIAN_POINT('Ctrl Pts',(-0.958079564117482,106.02889315763,11.320463658687));
#67832=CARTESIAN_POINT('Ctrl Pts',(-0.87496204969569,106.040227653765,11.2838658978538));
#67833=CARTESIAN_POINT('Ctrl Pts',(-0.789650234395092,106.051528405288,
11.25250371516));
#67834=CARTESIAN_POINT('Ctrl Pts',(-0.702939310861689,106.062768405711,
11.226437420213));
#67835=CARTESIAN_POINT('Ctrl Pts',(-0.691972596945212,106.064189978265,
11.2231407006315));
#67836=CARTESIAN_POINT('Ctrl Pts',(-0.680983503790746,106.065610581433,
11.2199286246592));
#67837=CARTESIAN_POINT('Ctrl Pts',(-0.669973637772597,106.067030162643,
11.2168012554285));
#67838=CARTESIAN_POINT('Ctrl Pts',(-0.596242281793452,106.076536876656,
11.1958577513349));
#67839=CARTESIAN_POINT('Ctrl Pts',(-0.521594012127566,106.0859592265,11.1786470542945));
#67840=CARTESIAN_POINT('Ctrl Pts',(-0.446378319094508,106.095374568071,
11.1653006883884));
#67841=CARTESIAN_POINT('Ctrl Pts',(-0.373298020979768,106.104522605417,
11.1523332296064));
#67842=CARTESIAN_POINT('Ctrl Pts',(-0.299681807214974,106.113664005035,
11.1430146279782));
#67843=CARTESIAN_POINT('Ctrl Pts',(-0.225891105797696,106.122863974629,
11.1374884678137));
#67844=CARTESIAN_POINT('Ctrl Pts',(-0.14339479848619,106.133149329076,11.131310347828));
#67845=CARTESIAN_POINT('Ctrl Pts',(-0.0606540173709518,106.143508255438,
11.129867656258));
#67846=CARTESIAN_POINT('Ctrl Pts',(0.0217462257417332,106.153870595193,
11.1331027964363));
#67847=CARTESIAN_POINT('Ctrl Pts',(0.0996101080729353,106.163662459547,
11.1361598332199));
#67848=CARTESIAN_POINT('Ctrl Pts',(0.177170135376786,106.173457417067,11.143392939204));
#67849=CARTESIAN_POINT('Ctrl Pts',(0.253974465255779,106.18320170211,11.1547455584407));
#67850=CARTESIAN_POINT('Ctrl Pts',(0.290109610774734,106.187786224344,11.1600867748641));
#67851=CARTESIAN_POINT('Ctrl Pts',(0.326074151320781,106.192359440177,11.1663399787423));
#67852=CARTESIAN_POINT('Ctrl Pts',(0.361817298262778,106.19691615701,11.1734987980242));
#67853=CARTESIAN_POINT('Ctrl Pts',(0.369752224482258,106.197927741467,11.1750880454095));
#67854=CARTESIAN_POINT('Ctrl Pts',(0.377676219185207,106.19893845325,11.1767218047798));
#67855=CARTESIAN_POINT('Ctrl Pts',(0.385589320558754,106.199948416309,11.1784003272889));
#67856=CARTESIAN_POINT('Ctrl Pts',(0.399726235083881,106.201752735597,11.1813990414618));
#67857=CARTESIAN_POINT('Ctrl Pts',(0.413828388402745,106.203554665579,11.1845406098083));
#67858=CARTESIAN_POINT('Ctrl Pts',(0.427896328510184,106.205354908042,11.1878248239191));
#67859=CARTESIAN_POINT('Ctrl Pts',(0.496011645924629,106.21407147108,11.2037266037749));
#67860=CARTESIAN_POINT('Ctrl Pts',(0.563283685263166,106.22274484046,11.2229683911427));
#67861=CARTESIAN_POINT('Ctrl Pts',(0.629330603489222,106.231430431946,11.2454761241329));
#67862=CARTESIAN_POINT('Ctrl Pts',(0.658079077638241,106.235211039868,11.2552731441514));
#67863=CARTESIAN_POINT('Ctrl Pts',(0.686594926239551,106.238993888204,11.265688514558));
#67864=CARTESIAN_POINT('Ctrl Pts',(0.71484446174108,106.24278319748,11.2767139852148));
#67865=CARTESIAN_POINT('Ctrl Pts',(0.781986129750496,106.25178938257,11.302918610436));
#67866=CARTESIAN_POINT('Ctrl Pts',(0.847631645539037,106.260835618038,11.3325764984433));
#67867=CARTESIAN_POINT('Ctrl Pts',(0.911534058805369,106.26986322064,11.3653742253422));
#67868=CARTESIAN_POINT('Ctrl Pts',(0.935902949783958,106.273305855313,11.3778814874359));
#67869=CARTESIAN_POINT('Ctrl Pts',(0.960018798076461,106.276745844659,11.390845656331));
#67870=CARTESIAN_POINT('Ctrl Pts',(0.983869475843969,106.280180173273,11.40425056808));
#67871=CARTESIAN_POINT('Ctrl Pts',(1.03153578423814,106.287043783961,11.4310406938641));
#67872=CARTESIAN_POINT('Ctrl Pts',(1.07817034688009,106.293853057527,11.4595298036398));
#67873=CARTESIAN_POINT('Ctrl Pts',(1.12360386288074,106.300656487286,11.489727866128));
#67874=CARTESIAN_POINT('Ctrl Pts',(1.12365926278775,106.30066478313,11.4897646885005));
#67875=CARTESIAN_POINT('Ctrl Pts',(1.12371466089045,106.300673078963,11.489801513403));
#67876=CARTESIAN_POINT('Ctrl Pts',(1.12377005718842,106.300681374784,11.4898383408353));
#67877=CARTESIAN_POINT('Ctrl Pts',(1.21883652868225,106.314917966604,11.5530384852764));
#67878=CARTESIAN_POINT('Ctrl Pts',(1.30859016660072,106.329121033484,11.6236870039346));
#67879=CARTESIAN_POINT('Ctrl Pts',(1.39204457833629,106.343297376238,11.7008037116028));
#67880=CARTESIAN_POINT('Ctrl Pts',(1.46712375098319,106.356051022965,11.7701812135056));
#67881=CARTESIAN_POINT('Ctrl Pts',(1.53710150328638,106.368782762367,11.8447941298811));
#67882=CARTESIAN_POINT('Ctrl Pts',(1.60122042459052,106.381492453046,11.9239052235944));
#67883=CARTESIAN_POINT('Ctrl Pts',(1.63008654138185,106.387214311868,11.9595207645948));
#67884=CARTESIAN_POINT('Ctrl Pts',(1.65776174908389,106.392931095069,11.9960444184693));
#67885=CARTESIAN_POINT('Ctrl Pts',(1.68433499070737,106.398561331456,12.0332820906798));
#67886=CARTESIAN_POINT('Ctrl Pts',(1.68656466909823,106.399033747151,12.0364065884069));
#67887=CARTESIAN_POINT('Ctrl Pts',(1.68878661000094,106.399505557261,12.0395361349704));
#67888=CARTESIAN_POINT('Ctrl Pts',(1.6910008771225,106.399976715713,12.0426706279985));
#67889=CARTESIAN_POINT('Ctrl Pts',(1.69101435879028,106.399979584383,12.0426897125043));
#67890=CARTESIAN_POINT('Ctrl Pts',(1.69102784015037,106.399982453044,12.0427087972224));
#67891=CARTESIAN_POINT('Ctrl Pts',(1.69104132120274,106.399985321697,12.0427278821528));
#67892=CARTESIAN_POINT('Ctrl Pts',(1.7281760628828,106.407887277476,12.0952989975656));
#67893=CARTESIAN_POINT('Ctrl Pts',(1.76297760691431,106.41572430273,12.1494850633351));
#67894=CARTESIAN_POINT('Ctrl Pts',(1.79522323258318,106.423548761793,12.2050923605098));
#67895=CARTESIAN_POINT('Ctrl Pts',(1.8086376653189,106.426803798022,12.2282254314952));
#67896=CARTESIAN_POINT('Ctrl Pts',(1.82160954051176,106.430056585454,12.2516038884278));
#67897=CARTESIAN_POINT('Ctrl Pts',(1.83412204242246,106.433310576039,12.2752112597003));
#67898=CARTESIAN_POINT('Ctrl Pts',(1.8673563186388,106.441953453592,12.337914458726));
#67899=CARTESIAN_POINT('Ctrl Pts',(1.89734992033821,106.450606035702,12.4022367996933));
#67900=CARTESIAN_POINT('Ctrl Pts',(1.92385711591667,106.459314064612,12.4678661360404));
#67901=CARTESIAN_POINT('Ctrl Pts',(1.93077581557633,106.461586965813,12.4849961891124));
#67902=CARTESIAN_POINT('Ctrl Pts',(1.93745688799951,106.463863609922,12.5022150326731));
#67903=CARTESIAN_POINT('Ctrl Pts',(1.94389576434339,106.466144737025,12.5195165694771));
#67904=CARTESIAN_POINT('Ctrl Pts',(1.95278245464122,106.469293061205,12.543395487326));
#67905=CARTESIAN_POINT('Ctrl Pts',(1.9612083840792,106.472449947364,12.5674327080015));
#67906=CARTESIAN_POINT('Ctrl Pts',(1.9691626354976,106.475617239892,12.5916133493029));
#67907=CARTESIAN_POINT('Ctrl Pts',(1.98702336922665,106.482729181105,12.6459093443581));
#67908=CARTESIAN_POINT('Ctrl Pts',(2.00250551225335,106.48989358909,12.7009289184984));
#67909=CARTESIAN_POINT('Ctrl Pts',(2.01563081321039,106.497072068049,12.756432926117));
#67910=CARTESIAN_POINT('Ctrl Pts',(2.01566999108625,106.497093495181,12.7565986007273));
#67911=CARTESIAN_POINT('Ctrl Pts',(2.01570914797441,106.497114922442,12.7567642796745));
#67912=CARTESIAN_POINT('Ctrl Pts',(2.01574828387691,106.497136349829,12.7569299629524));
#67913=CARTESIAN_POINT('Ctrl Pts',(2.03315128913704,106.506664709131,12.8306062236724));
#67914=CARTESIAN_POINT('Ctrl Pts',(2.04640392038463,106.516212173606,12.9051065380258));
#67915=CARTESIAN_POINT('Ctrl Pts',(2.05560223298109,106.52573997703,12.9799745305667));
#67916=CARTESIAN_POINT('Ctrl Pts',(2.05720372334514,106.527398834045,12.9930095701321));
#67917=CARTESIAN_POINT('Ctrl Pts',(2.05868231642198,106.529057110534,13.0060558820584));
#67918=CARTESIAN_POINT('Ctrl Pts',(2.0600385150921,106.530714621495,13.0191112181));
#67919=CARTESIAN_POINT('Ctrl Pts',(2.06827633959412,106.540782677678,13.0984119647347));
#67920=CARTESIAN_POINT('Ctrl Pts',(2.07199787975471,106.550821575886,13.1780405372738));
#67921=CARTESIAN_POINT('Ctrl Pts',(2.07128305867051,106.560796196022,13.2574603773354));
#67922=CARTESIAN_POINT('Ctrl Pts',(2.07123384373994,106.561482941627,13.2629283776508));
#67923=CARTESIAN_POINT('Ctrl Pts',(2.07116360377587,106.562169384997,13.2683954084505));
#67924=CARTESIAN_POINT('Ctrl Pts',(2.07107236646904,106.562855515764,13.2738613035474));
#67925=CARTESIAN_POINT('Ctrl Pts',(2.06962589105825,106.573733426536,13.3605175533834));
#67926=CARTESIAN_POINT('Ctrl Pts',(2.06290110218543,106.584533555568,13.4468827845573));
#67927=CARTESIAN_POINT('Ctrl Pts',(2.05089935882075,106.595255300884,13.5324077362176));
#67928=CARTESIAN_POINT('Ctrl Pts',(2.050892248048,106.595261653286,13.5324584078973));
#67929=CARTESIAN_POINT('Ctrl Pts',(2.05088513542134,106.59526800566,13.5325090792829));
#67930=CARTESIAN_POINT('Ctrl Pts',(2.05087802094089,106.595274358007,13.532559750374));
#67931=CARTESIAN_POINT('Ctrl Pts',(2.04173028718651,106.603442147344,13.5977121748083));
#67932=CARTESIAN_POINT('Ctrl Pts',(2.02952069130434,106.61156211999,13.66236009784));
#67933=CARTESIAN_POINT('Ctrl Pts',(2.01426416762495,106.61967394276,13.7262096654756));
#67934=CARTESIAN_POINT('Ctrl Pts',(2.00512022408077,106.624535735067,13.7644776781664));
#67935=CARTESIAN_POINT('Ctrl Pts',(1.99488198236352,106.629394475103,13.8024579322979));
#67936=CARTESIAN_POINT('Ctrl Pts',(1.98355572954919,106.634257578248,13.8400787879328));
#67937=CARTESIAN_POINT('Ctrl Pts',(1.97289374012445,106.638835469556,13.8754932512601));
#67938=CARTESIAN_POINT('Ctrl Pts',(1.96126697018555,106.64341757991,13.9105922964225));
#67939=CARTESIAN_POINT('Ctrl Pts',(1.94868017937678,106.64801030961,13.9453213261371));
#67940=CARTESIAN_POINT('Ctrl Pts',(1.92112627961522,106.65806431112,14.0213470755208));
#67941=CARTESIAN_POINT('Ctrl Pts',(1.88896804748103,106.66817039956,14.0956017957832));
#67942=CARTESIAN_POINT('Ctrl Pts',(1.85259474927175,106.678296263071,14.1676207893657));
#67943=CARTESIAN_POINT('Ctrl Pts',(1.84190082487254,106.681273315585,14.1887947194352));
#67944=CARTESIAN_POINT('Ctrl Pts',(1.83084237860993,106.68425212139,14.2097756887979));
#67945=CARTESIAN_POINT('Ctrl Pts',(1.81942881751468,106.687231969321,14.2305525822634));
#67946=CARTESIAN_POINT('Ctrl Pts',(1.78237298048731,106.696906492321,14.298007881426));
#67947=CARTESIAN_POINT('Ctrl Pts',(1.74157631895577,106.706591081943,14.3633098133132));
#67948=CARTESIAN_POINT('Ctrl Pts',(1.69739482677731,106.716253628718,14.4260586078122));
#67949=CARTESIAN_POINT('Ctrl Pts',(1.68101580228434,106.719835741556,14.4493209285561));
#67950=CARTESIAN_POINT('Ctrl Pts',(1.66417143699621,106.723414890053,14.4722328507827));
#67951=CARTESIAN_POINT('Ctrl Pts',(1.64687919716595,106.726989669104,14.4947756854846));
#67952=CARTESIAN_POINT('Ctrl Pts',(1.59212670309234,106.73830850754,14.5661531609034));
#67953=CARTESIAN_POINT('Ctrl Pts',(1.53295032325131,106.749564422212,14.6338678838562));
#67954=CARTESIAN_POINT('Ctrl Pts',(1.46981441294025,106.760746735467,14.6972127195225));
#67955=CARTESIAN_POINT('Ctrl Pts',(1.45922353259919,106.762622538652,14.707838646534));
#67956=CARTESIAN_POINT('Ctrl Pts',(1.44852128540073,106.764496274647,14.7183417158395));
#67957=CARTESIAN_POINT('Ctrl Pts',(1.43770991924172,106.766367897714,14.7287187245816));
#67958=CARTESIAN_POINT('Ctrl Pts',(1.43768550379726,106.766372124424,14.7287421591112));
#67959=CARTESIAN_POINT('Ctrl Pts',(1.43766108779333,106.766376351121,14.7287655930306));
#67960=CARTESIAN_POINT('Ctrl Pts',(1.43763667123001,106.766380577807,14.7287890263397));
#67961=CARTESIAN_POINT('Ctrl Pts',(1.39173214752141,106.774326986706,14.772844976286));
#67962=CARTESIAN_POINT('Ctrl Pts',(1.3438467780252,106.782231140677,14.8147462663298));
#67963=CARTESIAN_POINT('Ctrl Pts',(1.29414526465123,106.790120931987,14.8542823463259));
#67964=CARTESIAN_POINT('Ctrl Pts',(1.24453721148936,106.797995887098,14.8937440814948));
#67965=CARTESIAN_POINT('Ctrl Pts',(1.19311947451598,106.805856534675,14.930848854179));
#67966=CARTESIAN_POINT('Ctrl Pts',(1.14010096732926,106.813724233105,14.9653624716543));
#67967=CARTESIAN_POINT('Ctrl Pts',(1.13168593824299,106.814972984053,14.9708404285101));
#67968=CARTESIAN_POINT('Ctrl Pts',(1.12323068167995,106.816221899543,14.9762530709656));
#67969=CARTESIAN_POINT('Ctrl Pts',(1.11473614598593,106.817471050163,14.9815994224094));
#67970=CARTESIAN_POINT('Ctrl Pts',(1.0403589062157,106.828408478475,15.0284114999091));
#67971=CARTESIAN_POINT('Ctrl Pts',(0.96293079169232,106.839370468413,15.0701586979578));
#67972=CARTESIAN_POINT('Ctrl Pts',(0.883215959514714,106.850336159934,15.1066484684882));
#67973=CARTESIAN_POINT('Ctrl Pts',(0.842924095903791,106.855878768945,15.1250922237749));
#67974=CARTESIAN_POINT('Ctrl Pts',(0.802047275557933,106.861422426754,15.1421931927125));
#67975=CARTESIAN_POINT('Ctrl Pts',(0.760679432527574,106.866965072867,15.1579281494837));
#67976=CARTESIAN_POINT('Ctrl Pts',(0.702198564405304,106.874800597579,15.1801723339623));
#67977=CARTESIAN_POINT('Ctrl Pts',(0.642742727877497,106.882633065654,15.1996849416091));
#67978=CARTESIAN_POINT('Ctrl Pts',(0.582623353521924,106.890440017239,15.2164953412303));
#67979=CARTESIAN_POINT('Ctrl Pts',(0.555253859136353,106.893994151324,15.2241483173796));
#67980=CARTESIAN_POINT('Ctrl Pts',(0.527746220400075,106.897543084433,15.2312415876166));
#67981=CARTESIAN_POINT('Ctrl Pts',(0.500126557908841,106.901085136587,15.2377793389447));
#67982=CARTESIAN_POINT('Ctrl Pts',(0.413926382623553,106.912139779874,15.2581834735218));
#67983=CARTESIAN_POINT('Ctrl Pts',(0.3265326132082,106.923170028877,15.2729182309128));
#67984=CARTESIAN_POINT('Ctrl Pts',(0.238655941651049,106.934183156336,15.2816536572493));
#67985=CARTESIAN_POINT('Ctrl Pts',(0.238567491824711,106.934194241294,15.2816624496504));
#67986=CARTESIAN_POINT('Ctrl Pts',(0.238479041466734,106.93420532624,15.2816712359778));
#67987=CARTESIAN_POINT('Ctrl Pts',(0.238390590577828,106.934216411174,15.2816800162313));
#67988=CARTESIAN_POINT('Ctrl Pts',(0.16178467325091,106.943816897281,15.2892844550426));
#67989=CARTESIAN_POINT('Ctrl Pts',(0.0847827294383409,106.953408057825,
15.2923311531031));
#67990=CARTESIAN_POINT('Ctrl Pts',(0.00793992072725377,106.962985676773,
15.2909356875329));
#67991=CARTESIAN_POINT('Ctrl Pts',(-0.0439573489995137,106.969454106055,
15.289993233004));
#67992=CARTESIAN_POINT('Ctrl Pts',(-0.0957784160519001,106.975915923052,
15.2870246406397));
#67993=CARTESIAN_POINT('Ctrl Pts',(-0.147337536445514,106.982367944768,
15.2820732147274));
#67994=CARTESIAN_POINT('Ctrl Pts',(-0.219145308937171,106.991353848794,
15.2751772308025));
#67995=CARTESIAN_POINT('Ctrl Pts',(-0.290452604006382,107.000321661448,
15.2644381955568));
#67996=CARTESIAN_POINT('Ctrl Pts',(-0.360897333028724,107.009280080517,
15.2499534424375));
#67997=CARTESIAN_POINT('Ctrl Pts',(-0.424928366238981,107.017422873269,
15.2367874650691));
#67998=CARTESIAN_POINT('Ctrl Pts',(-0.488246064484556,107.025557783316,
15.2205264383419));
#67999=CARTESIAN_POINT('Ctrl Pts',(-0.550570205952548,107.033690822623,
15.2012250032835));
#68000=CARTESIAN_POINT('Ctrl Pts',(-0.634697004798602,107.044669017359,
15.1751714082183));
#68001=CARTESIAN_POINT('Ctrl Pts',(-0.71700725972373,107.055643099448,15.1435756551976));
#68002=CARTESIAN_POINT('Ctrl Pts',(-0.796660794646603,107.066609435735,
15.1066058385688));
#68003=CARTESIAN_POINT('Ctrl Pts',(-0.842119199686749,107.072867942118,
15.085507102647));
#68004=CARTESIAN_POINT('Ctrl Pts',(-0.886715293108071,107.079124367692,
15.0626565498559));
#68005=CARTESIAN_POINT('Ctrl Pts',(-0.930281051229547,107.085376307396,
15.0380949762599));
#68006=CARTESIAN_POINT('Ctrl Pts',(-0.963052477241712,107.090079197654,
15.0196190486839));
#68007=CARTESIAN_POINT('Ctrl Pts',(-0.995239509619407,107.094779353001,
15.000175776424));
#68008=CARTESIAN_POINT('Ctrl Pts',(-1.02676916585278,107.099475324812,14.9797868477451));
#68009=CARTESIAN_POINT('Ctrl Pts',(-1.02693329067948,107.099499769276,14.9796807149867));
#68010=CARTESIAN_POINT('Ctrl Pts',(-1.02709739887614,107.099524213803,14.9795745558479));
#68011=CARTESIAN_POINT('Ctrl Pts',(-1.02726149043209,107.099548658391,14.9794683703343));
#68012=CARTESIAN_POINT('Ctrl Pts',(-1.07822398336964,107.107140500326,14.9464899610819));
#68013=CARTESIAN_POINT('Ctrl Pts',(-1.12757710569181,107.114737912216,14.9109662585429));
#68014=CARTESIAN_POINT('Ctrl Pts',(-1.17516702871453,107.122326054767,14.8732558902454));
#68015=CARTESIAN_POINT('Ctrl Pts',(-1.20436144204537,107.126981060617,14.8501221676208));
#68016=CARTESIAN_POINT('Ctrl Pts',(-1.23289331627348,107.131632666299,14.8261658916509));
#68017=CARTESIAN_POINT('Ctrl Pts',(-1.26073663596602,107.136278282374,14.8014714572102));
#68018=CARTESIAN_POINT('Ctrl Pts',(-1.28430373824257,107.140210417996,14.780569629822));
#68019=CARTESIAN_POINT('Ctrl Pts',(-1.30751037372541,107.144131041719,14.759331799902));
#68020=CARTESIAN_POINT('Ctrl Pts',(-1.33017835559884,107.14805176292,14.7375275760134));
#68021=CARTESIAN_POINT('Ctrl Pts',(-1.39939450961625,107.160023593676,14.670948886859));
#68022=CARTESIAN_POINT('Ctrl Pts',(-1.46355113224768,107.171991306496,14.5991087040727));
#68023=CARTESIAN_POINT('Ctrl Pts',(-1.52211657808587,107.183947453271,14.5229809858679));
#68024=CARTESIAN_POINT('Ctrl Pts',(-1.58262960160205,107.196301198395,14.4443216614826));
#68025=CARTESIAN_POINT('Ctrl Pts',(-1.6371726339279,107.208642419216,14.3610858047828));
#68026=CARTESIAN_POINT('Ctrl Pts',(-1.68519607156579,107.220962124354,14.2743884519512));
#68027=CARTESIAN_POINT('Ctrl Pts',(-1.7329289728637,107.233207296676,14.1882156082513));
#68028=CARTESIAN_POINT('Ctrl Pts',(-1.77422038552428,107.245431073975,14.0986242296114));
#68029=CARTESIAN_POINT('Ctrl Pts',(-1.80857598691776,107.257626277559,14.0067323324837));
#68030=CARTESIAN_POINT('Ctrl Pts',(-1.84162758138612,107.269358597965,13.9183282994992));
#68031=CARTESIAN_POINT('Ctrl Pts',(-1.86825969015914,107.28106441381,13.8277961289283));
#68032=CARTESIAN_POINT('Ctrl Pts',(-1.88807920419422,107.292740261752,13.7361361881972));
#68033=CARTESIAN_POINT('Ctrl Pts',(-1.89639863050633,107.297641308084,13.6976610711315));
#68034=CARTESIAN_POINT('Ctrl Pts',(-1.90351700382206,107.302536603697,13.6589911103909));
#68035=CARTESIAN_POINT('Ctrl Pts',(-1.90961068327992,107.307438130595,13.6202521027464));
#68036=CARTESIAN_POINT('Ctrl Pts',(-1.91045184120514,107.308114726439,13.614904656508));
#68037=CARTESIAN_POINT('Ctrl Pts',(-1.91127349823806,107.308791451028,13.6095558177041));
#68038=CARTESIAN_POINT('Ctrl Pts',(-1.91207613960894,107.309468345496,13.6042058428203));
#68039=CARTESIAN_POINT('Ctrl Pts',(-1.92274394036054,107.31846486072,13.5331000312374));
#68040=CARTESIAN_POINT('Ctrl Pts',(-1.92945891623361,107.32746221094,13.4615841732368));
#68041=CARTESIAN_POINT('Ctrl Pts',(-1.93189267743231,107.336451252017,13.3900567083924));
#68042=CARTESIAN_POINT('Ctrl Pts',(-1.93252994110109,107.338804970738,13.3713277325629));
#68043=CARTESIAN_POINT('Ctrl Pts',(-1.93287369565044,107.341158084246,13.3525982357956));
#68044=CARTESIAN_POINT('Ctrl Pts',(-1.93291812964871,107.34351035279,13.3338759519325));
#68045=CARTESIAN_POINT('Ctrl Pts',(-1.93291846211627,107.343527953119,13.3337358665865));
#68046=CARTESIAN_POINT('Ctrl Pts',(-1.93291877782965,107.343545553549,13.3335957804611));
#68047=CARTESIAN_POINT('Ctrl Pts',(-1.93291907678648,107.34356315408,13.3334556935608));
#68048=CARTESIAN_POINT('Ctrl Pts',(-1.93305037040335,107.351292823189,13.2719333813634));
#68049=CARTESIAN_POINT('Ctrl Pts',(-1.92994528317225,107.359041997369,13.2102611881824));
#68050=CARTESIAN_POINT('Ctrl Pts',(-1.92371562688559,107.366795633922,13.1488127563905));
#68051=CARTESIAN_POINT('Ctrl Pts',(-1.92038329339603,107.370943166556,13.1159430991063));
#68052=CARTESIAN_POINT('Ctrl Pts',(-1.91615784140607,107.375091977645,13.0831375621709));
#68053=CARTESIAN_POINT('Ctrl Pts',(-1.91106244729389,107.379239775609,13.050453402942));
#68054=CARTESIAN_POINT('Ctrl Pts',(-1.90307811136313,107.385739255647,12.999238266065));
#68055=CARTESIAN_POINT('Ctrl Pts',(-1.893292919909,107.392265624772,12.9483253686079));
#68056=CARTESIAN_POINT('Ctrl Pts',(-1.88163058522903,107.398805824831,12.8978460125036));
#68057=CARTESIAN_POINT('Ctrl Pts',(-1.87123302293243,107.404636744576,12.8528411087524));
#68058=CARTESIAN_POINT('Ctrl Pts',(-1.85934308089877,107.410478566673,12.8081815907255));
#68059=CARTESIAN_POINT('Ctrl Pts',(-1.84591326539498,107.416317549966,12.7639945706258));
#68060=CARTESIAN_POINT('Ctrl Pts',(-1.82674217848543,107.424652709607,12.7009175162639));
#68061=CARTESIAN_POINT('Ctrl Pts',(-1.80438503606112,107.432976658583,12.6388114571308));
#68062=CARTESIAN_POINT('Ctrl Pts',(-1.77891111747281,107.441269651585,12.5780305378066));
#68063=CARTESIAN_POINT('Ctrl Pts',(-1.76555453484415,107.44561786546,12.5461616532302));
#68064=CARTESIAN_POINT('Ctrl Pts',(-1.75134133701015,107.449957452586,12.5146579041327));
#68065=CARTESIAN_POINT('Ctrl Pts',(-1.73628373074468,107.454284801398,12.4835755667181));
#68066=CARTESIAN_POINT('Ctrl Pts',(-1.71707431732516,107.459805322448,12.4439229513611));
#68067=CARTESIAN_POINT('Ctrl Pts',(-1.69648973490362,107.465306489921,12.4049524071892));
#68068=CARTESIAN_POINT('Ctrl Pts',(-1.67455499375723,107.470782377846,12.3667726720596));
#68069=CARTESIAN_POINT('Ctrl Pts',(-1.64128786324746,107.479087334675,12.308867715584));
#68070=CARTESIAN_POINT('Ctrl Pts',(-1.60490998011633,107.487334292046,12.2527786019574));
#68071=CARTESIAN_POINT('Ctrl Pts',(-1.56572551425112,107.495541702607,12.1987701848449));
#68072=CARTESIAN_POINT('Ctrl Pts',(-1.54602678476878,107.4996677142,12.1716191908227));
#68073=CARTESIAN_POINT('Ctrl Pts',(-1.52561823215195,107.50378383509,12.1449933966371));
#68074=CARTESIAN_POINT('Ctrl Pts',(-1.50453495600743,107.507893035257,12.1189230461787));
#68075=CARTESIAN_POINT('Ctrl Pts',(-1.46636396394904,107.515332687704,12.071723022165));
#68076=CARTESIAN_POINT('Ctrl Pts',(-1.42598401004741,107.522749727454,12.0263448236212));
#68077=CARTESIAN_POINT('Ctrl Pts',(-1.38366043994489,107.530166144122,11.9829630156392));
#68078=CARTESIAN_POINT('Ctrl Pts',(-1.35422042767174,107.535324957455,11.9527868996754));
#68079=CARTESIAN_POINT('Ctrl Pts',(-1.32383955943577,107.540483607884,11.9235757200112));
#68080=CARTESIAN_POINT('Ctrl Pts',(-1.29259847812592,107.545651394958,11.8953762726244));
#68081=CARTESIAN_POINT('Ctrl Pts',(-1.25244841288815,107.552292874044,11.8591352206258));
#68082=CARTESIAN_POINT('Ctrl Pts',(-1.21101867279548,107.558981745805,11.8244489763536));
#68083=CARTESIAN_POINT('Ctrl Pts',(-1.16828471652994,107.565690386974,11.7915833615631));
#68084=CARTESIAN_POINT('Ctrl Pts',(-1.13463751899251,107.57097253247,11.7657061451834));
#68085=CARTESIAN_POINT('Ctrl Pts',(-1.10018238305018,107.576266803463,11.7409585249536));
#68086=CARTESIAN_POINT('Ctrl Pts',(-1.0649253297805,107.581556823008,11.7174838721533));
#68087=CARTESIAN_POINT('Ctrl Pts',(-1.05993500493425,107.582305578605,11.7141612421471));
#68088=CARTESIAN_POINT('Ctrl Pts',(-1.05492874948117,107.583054228879,11.7108642014886));
#68089=CARTESIAN_POINT('Ctrl Pts',(-1.0499066660986,107.583802780861,11.7075929425082));
#68090=CARTESIAN_POINT('Ctrl Pts',(-0.991219818328679,107.592550177683,
11.6693658038541));
#68091=CARTESIAN_POINT('Ctrl Pts',(-0.930228297682015,107.601305122401,
11.6345713200927));
#68092=CARTESIAN_POINT('Ctrl Pts',(-0.867464676749782,107.61005406824,11.603355212156));
#68093=CARTESIAN_POINT('Ctrl Pts',(-0.830320208917726,107.615231827783,
11.5848810435234));
#68094=CARTESIAN_POINT('Ctrl Pts',(-0.792558630281349,107.62040709212,11.5676605321247));
#68095=CARTESIAN_POINT('Ctrl Pts',(-0.754283093784006,107.625578556984,
11.5517120295663));
#68096=CARTESIAN_POINT('Ctrl Pts',(-0.668001388472514,107.637236206968,
11.5157605021986));
#68097=CARTESIAN_POINT('Ctrl Pts',(-0.579101139665477,107.648875775813,
11.486264133236));
#68098=CARTESIAN_POINT('Ctrl Pts',(-0.488564333837079,107.660508081308,
11.4633640719517));
#68099=CARTESIAN_POINT('Ctrl Pts',(-0.40313283342547,107.671484449455,11.4417553286662));
#68100=CARTESIAN_POINT('Ctrl Pts',(-0.316235351384715,107.682455293058,
11.4260209618426));
#68101=CARTESIAN_POINT('Ctrl Pts',(-0.228746918708682,107.693422325914,
11.4163187295061));
#68102=CARTESIAN_POINT('Ctrl Pts',(-0.203667267928375,107.696566162713,
11.4135374635565));
#68103=CARTESIAN_POINT('Ctrl Pts',(-0.178539198357052,107.699709669414,
11.4112519413924));
#68104=CARTESIAN_POINT('Ctrl Pts',(-0.153383473816096,107.70285287079,11.4094659507271));
#68105=CARTESIAN_POINT('Ctrl Pts',(-0.153323789078853,107.702860328383,
11.4094617132669));
#68106=CARTESIAN_POINT('Ctrl Pts',(-0.153264104180559,107.702867785979,
11.4094574786036));
#68107=CARTESIAN_POINT('Ctrl Pts',(-0.153204419121579,107.702875243578,
11.4094532467374));
#68108=CARTESIAN_POINT('Ctrl Pts',(-0.0503082794465152,107.7157320319,11.4021575733437));
#68109=CARTESIAN_POINT('Ctrl Pts',(0.0530647704723847,107.728598333694,
11.4031794466173));
#68110=CARTESIAN_POINT('Ctrl Pts',(0.155564843474227,107.741471740227,11.4123192936204));
#68111=CARTESIAN_POINT('Ctrl Pts',(0.195744104762457,107.746518019216,11.4159020452236));
#68112=CARTESIAN_POINT('Ctrl Pts',(0.235789349262896,107.751565405274,11.4207316333851));
#68113=CARTESIAN_POINT('Ctrl Pts',(0.275620013322703,107.756613811943,11.4267939874474));
#68114=CARTESIAN_POINT('Ctrl Pts',(0.353137764528065,107.766438933904,11.4385924363313));
#68115=CARTESIAN_POINT('Ctrl Pts',(0.429860535829397,107.776236805584,11.4551752460502));
#68116=CARTESIAN_POINT('Ctrl Pts',(0.505205833897759,107.785978354576,11.4765543596553));
#68117=CARTESIAN_POINT('Ctrl Pts',(0.53888822020398,107.790333219773,11.4861116854845));
#68118=CARTESIAN_POINT('Ctrl Pts',(0.572295512101532,107.794676919606,11.4966276750502));
#68119=CARTESIAN_POINT('Ctrl Pts',(0.605387977521011,107.799028791502,11.5080363533329));
#68120=CARTESIAN_POINT('Ctrl Pts',(0.6219342621262,107.801204734275,11.5137407103652));
#68121=CARTESIAN_POINT('Ctrl Pts',(0.638401807431331,107.803382708495,11.5196682310407));
#68122=CARTESIAN_POINT('Ctrl Pts',(0.654782616705315,107.805560803768,11.5258234700986));
#68123=CARTESIAN_POINT('Ctrl Pts',(0.671163226945381,107.807738872576,11.5319786343677));
#68124=CARTESIAN_POINT('Ctrl Pts',(0.68745698972609,107.809917050831,11.538361487542));
#68125=CARTESIAN_POINT('Ctrl Pts',(0.703660466053377,107.812100528228,11.5449548006635));
#68126=CARTESIAN_POINT('Ctrl Pts',(0.726758869241025,107.815213122109,11.554353709993));
#68127=CARTESIAN_POINT('Ctrl Pts',(0.749668765831185,107.818327248075,11.5642092253437));
#68128=CARTESIAN_POINT('Ctrl Pts',(0.772370087930443,107.821440878198,11.5745244080491));
#68129=CARTESIAN_POINT('Ctrl Pts',(0.77240211744071,107.821445271248,11.574538961838));
#68130=CARTESIAN_POINT('Ctrl Pts',(0.772434146546288,107.821449664299,11.5745535165468));
#68131=CARTESIAN_POINT('Ctrl Pts',(0.772466175247419,107.82145405735,11.5745680721755));
#68132=CARTESIAN_POINT('Ctrl Pts',(0.813409826174717,107.827069881514,11.5931751514367));
#68133=CARTESIAN_POINT('Ctrl Pts',(0.853691310046216,107.832686373679,11.6132853975448));
#68134=CARTESIAN_POINT('Ctrl Pts',(0.893223189291165,107.838316104378,11.6347820257333));
#68135=CARTESIAN_POINT('Ctrl Pts',(0.963932215868106,107.848385769298,11.6732321496062));
#68136=CARTESIAN_POINT('Ctrl Pts',(1.03222649571,107.858477387079,11.7161771247585));
#68137=CARTESIAN_POINT('Ctrl Pts',(1.09753010505694,107.86855227438,11.7632718359109));
#68138=CARTESIAN_POINT('Ctrl Pts',(1.12048666829478,107.872093958978,11.7798273176912));
#68139=CARTESIAN_POINT('Ctrl Pts',(1.14307328065565,107.875633516843,11.7968953253573));
#68140=CARTESIAN_POINT('Ctrl Pts',(1.16526381138637,107.879169075699,11.8144598343174));
#68141=CARTESIAN_POINT('Ctrl Pts',(1.18956780137538,107.883041366457,11.8336972133196));
#68142=CARTESIAN_POINT('Ctrl Pts',(1.21339758945319,107.886909049586,11.8535306653475));
#68143=CARTESIAN_POINT('Ctrl Pts',(1.2367205136842,107.890770253688,11.8739392041113));
#68144=CARTESIAN_POINT('Ctrl Pts',(1.29270144708995,107.900038122827,11.9229248732377));
#68145=CARTESIAN_POINT('Ctrl Pts',(1.34576573083898,107.909268748033,11.9752294206335));
#68146=CARTESIAN_POINT('Ctrl Pts',(1.39556867414692,107.918505973281,12.030421414051));
#68147=CARTESIAN_POINT('Ctrl Pts',(1.41884597613203,107.922823342242,12.0562174938127));
#68148=CARTESIAN_POINT('Ctrl Pts',(1.44141140271464,107.927142246835,12.0826448212329));
#68149=CARTESIAN_POINT('Ctrl Pts',(1.4632323950436,107.931467654987,12.109662182857));
#68150=CARTESIAN_POINT('Ctrl Pts',(1.47718970054447,107.934234304738,12.1269432287567));
#68151=CARTESIAN_POINT('Ctrl Pts',(1.49084195922481,107.937003551222,12.1444649320569));
#68152=CARTESIAN_POINT('Ctrl Pts',(1.50418026134739,107.939776614462,12.1622156871461));
#68153=CARTESIAN_POINT('Ctrl Pts',(1.50419212819256,107.939779081606,12.1622314796706));
#68154=CARTESIAN_POINT('Ctrl Pts',(1.50420399479058,107.939781548754,12.1622472723778));
#68155=CARTESIAN_POINT('Ctrl Pts',(1.50421586114142,107.939784015905,12.1622630652677));
#68156=CARTESIAN_POINT('Ctrl Pts',(1.5489167875955,107.949077852235,12.2217553910282));
#68157=CARTESIAN_POINT('Ctrl Pts',(1.59011255430665,107.958419810004,12.2838443321159));
#68158=CARTESIAN_POINT('Ctrl Pts',(1.62752645131653,107.96776315549,12.3481295844515));
#68159=CARTESIAN_POINT('Ctrl Pts',(1.66449871912309,107.976996213233,12.4116560212923));
#68160=CARTESIAN_POINT('Ctrl Pts',(1.69777693953788,107.986230607277,12.4773274505966));
#68161=CARTESIAN_POINT('Ctrl Pts',(1.72707490853383,107.995415020297,12.5447116847064));
#68162=CARTESIAN_POINT('Ctrl Pts',(1.7585214679531,108.005272979729,12.6170375965179));
#68163=CARTESIAN_POINT('Ctrl Pts',(1.78539617584054,108.015077634329,12.6913676067518));
#68164=CARTESIAN_POINT('Ctrl Pts',(1.8075555410359,108.024873771686,12.76706296488));
#68165=CARTESIAN_POINT('Ctrl Pts',(1.82900486110536,108.03435601469,12.8403328419703));
#68166=CARTESIAN_POINT('Ctrl Pts',(1.84603718829411,108.043830316501,12.9148818596889));
#68167=CARTESIAN_POINT('Ctrl Pts',(1.85854169112516,108.053343116012,12.9901727679075));
#68168=CARTESIAN_POINT('Ctrl Pts',(1.86057427055602,108.054889400648,13.0024111394321));
#68169=CARTESIAN_POINT('Ctrl Pts',(1.86248710821986,108.056436628437,13.0146687422829));
#68170=CARTESIAN_POINT('Ctrl Pts',(1.86427970516388,108.057984960076,13.0269431330409));
#68171=CARTESIAN_POINT('Ctrl Pts',(1.86428039852866,108.05798555896,13.026947880695));
#68172=CARTESIAN_POINT('Ctrl Pts',(1.86428109187545,108.057986157845,13.0269526283516));
#68173=CARTESIAN_POINT('Ctrl Pts',(1.86428178520429,108.05798675673,13.0269573760111));
#68174=CARTESIAN_POINT('Ctrl Pts',(1.87524500381698,108.067456586847,13.1020294419768));
#68175=CARTESIAN_POINT('Ctrl Pts',(1.88171525716222,108.076972609446,13.1777724884613));
#68176=CARTESIAN_POINT('Ctrl Pts',(1.88361208860195,108.08648032582,13.2536471959942));
#68177=CARTESIAN_POINT('Ctrl Pts',(1.88450005735865,108.090931198424,13.2891666250286));
#68178=CARTESIAN_POINT('Ctrl Pts',(1.88438573730388,108.095380157836,13.3247141603359));
#68179=CARTESIAN_POINT('Ctrl Pts',(1.88326117130547,108.099821126105,13.3602305922588));
#68180=CARTESIAN_POINT('Ctrl Pts',(1.88179566098341,108.105608500832,13.4065148456144));
#68181=CARTESIAN_POINT('Ctrl Pts',(1.87861456796639,108.111382822336,13.452750260111));
#68182=CARTESIAN_POINT('Ctrl Pts',(1.87374192211305,108.117154216983,13.4988132921293));
#68183=CARTESIAN_POINT('Ctrl Pts',(1.87374121925935,108.117155049476,13.498819936481));
#68184=CARTESIAN_POINT('Ctrl Pts',(1.87374051637044,108.11715588197,13.4988265808292));
#68185=CARTESIAN_POINT('Ctrl Pts',(1.87373981344633,108.117156714463,13.4988332251737));
#68186=CARTESIAN_POINT('Ctrl Pts',(1.86375552053862,108.128981402164,13.5932091071049));
#68187=CARTESIAN_POINT('Ctrl Pts',(1.84667352779593,108.140789842786,13.6868306513806));
#68188=CARTESIAN_POINT('Ctrl Pts',(1.82273984890812,108.152631737893,13.7786480261527));
#68189=CARTESIAN_POINT('Ctrl Pts',(1.81189394076528,108.157998071551,13.8202564565725));
#68190=CARTESIAN_POINT('Ctrl Pts',(1.79964082232468,108.16337136398,13.8614950815876));
#68191=CARTESIAN_POINT('Ctrl Pts',(1.78600211636631,108.168756676845,13.902269462313));
#68192=CARTESIAN_POINT('Ctrl Pts',(1.77969626305583,108.171246575304,13.9211214900981));
#68193=CARTESIAN_POINT('Ctrl Pts',(1.77309559706695,108.17373968257,13.9398740648559));
#68194=CARTESIAN_POINT('Ctrl Pts',(1.76619994546931,108.176235268159,13.958517662311));
#68195=CARTESIAN_POINT('Ctrl Pts',(1.75527788476314,108.180188039978,13.9880473594402));
#68196=CARTESIAN_POINT('Ctrl Pts',(1.74361576800181,108.184147036455,14.0173037180304));
#68197=CARTESIAN_POINT('Ctrl Pts',(1.73122901172699,108.188109234452,14.0462548285743));
#68198=CARTESIAN_POINT('Ctrl Pts',(1.71413999127076,108.193575563255,14.086196368501));
#68199=CARTESIAN_POINT('Ctrl Pts',(1.6956690756824,108.199045451061,14.1255533276468));
#68200=CARTESIAN_POINT('Ctrl Pts',(1.67584846591692,108.204503272049,14.1642316908938));
#68201=CARTESIAN_POINT('Ctrl Pts',(1.62818322275471,108.217628416411,14.2572466692973));
#68202=CARTESIAN_POINT('Ctrl Pts',(1.57270897662728,108.230685549007,14.3463428601481));
#68203=CARTESIAN_POINT('Ctrl Pts',(1.51031547041863,108.243711872239,14.4303274257314));
#68204=CARTESIAN_POINT('Ctrl Pts',(1.48941061563552,108.248076323159,14.4584663339965));
#68205=CARTESIAN_POINT('Ctrl Pts',(1.46772898050822,108.252437365451,14.486031857037));
#68206=CARTESIAN_POINT('Ctrl Pts',(1.44530377793378,108.256796548177,14.5129803988635));
#68207=CARTESIAN_POINT('Ctrl Pts',(1.42296634031131,108.26113867048,14.5398234728589));
#68208=CARTESIAN_POINT('Ctrl Pts',(1.3998915975729,108.265478636989,14.5660535371844));
#68209=CARTESIAN_POINT('Ctrl Pts',(1.37610597632969,108.269816897345,14.5916302585667));
#68210=CARTESIAN_POINT('Ctrl Pts',(1.35231945319316,108.274155322197,14.6172079497565));
#68211=CARTESIAN_POINT('Ctrl Pts',(1.32782193232556,108.27849211975,14.6421322449387));
#68212=CARTESIAN_POINT('Ctrl Pts',(1.30265205719123,108.282831974951,14.6663616227905));
#68213=CARTESIAN_POINT('Ctrl Pts',(1.27998541948397,108.286740215458,14.6881812991579));
#68214=CARTESIAN_POINT('Ctrl Pts',(1.25677702100915,108.290653156273,14.7094391604563));
#68215=CARTESIAN_POINT('Ctrl Pts',(1.23304717436089,108.294570971721,14.7301047171995));
#68216=CARTESIAN_POINT('Ctrl Pts',(1.20407315493938,108.29935460402,14.7553372545736));
#68217=CARTESIAN_POINT('Ctrl Pts',(1.1743217523591,108.304145503826,14.7796867837824));
#68218=CARTESIAN_POINT('Ctrl Pts',(1.14385301557154,108.308943972914,14.8031180912194));
#68219=CARTESIAN_POINT('Ctrl Pts',(1.08843558416345,108.317671569118,14.8457356398806));
#68220=CARTESIAN_POINT('Ctrl Pts',(1.03063671059079,108.326414274237,14.8853033104582));
#68221=CARTESIAN_POINT('Ctrl Pts',(0.97081961488415,108.335150275283,14.9215703550054));
#68222=CARTESIAN_POINT('Ctrl Pts',(0.928186359654004,108.341376658525,14.9474188544745));
#68223=CARTESIAN_POINT('Ctrl Pts',(0.884526485399702,108.347600678116,14.9715929539637));
#68224=CARTESIAN_POINT('Ctrl Pts',(0.839979531862484,108.353827252736,14.9940174782538));
#68225=CARTESIAN_POINT('Ctrl Pts',(0.822017863373078,108.356337854702,15.0030592160012));
#68226=CARTESIAN_POINT('Ctrl Pts',(0.803911953720946,108.35884887504,15.011816520812));
#68227=CARTESIAN_POINT('Ctrl Pts',(0.7856708619492,108.361360648253,15.0202863087384));
#68228=CARTESIAN_POINT('Ctrl Pts',(0.702703679152465,108.372785115053,15.0588100140042));
#68229=CARTESIAN_POINT('Ctrl Pts',(0.616939738427914,108.384218522087,15.0913759547903));
#68230=CARTESIAN_POINT('Ctrl Pts',(0.529219838814109,108.395639467232,15.1176260166494));
#68231=CARTESIAN_POINT('Ctrl Pts',(0.484383276888817,108.401477092634,15.1310432974405));
#68232=CARTESIAN_POINT('Ctrl Pts',(0.439035184854932,108.407311285814,15.1428104264786));
#68233=CARTESIAN_POINT('Ctrl Pts',(0.393286543835379,108.413137886914,15.1528779590084));
#68234=CARTESIAN_POINT('Ctrl Pts',(0.391555418960531,108.413358365028,15.1532589136248));
#68235=CARTESIAN_POINT('Ctrl Pts',(0.3898237207389,108.413578832247,15.1536374345775));
#68236=CARTESIAN_POINT('Ctrl Pts',(0.388091457000056,108.413799288348,15.1540135197612));
#68237=CARTESIAN_POINT('Ctrl Pts',(0.324523358755103,108.421889266079,15.1678145474989));
#68238=CARTESIAN_POINT('Ctrl Pts',(0.26019742050251,108.429961888862,15.1783321900859));
#68239=CARTESIAN_POINT('Ctrl Pts',(0.195517808938001,108.438053322813,15.1855237469954));
#68240=CARTESIAN_POINT('Ctrl Pts',(0.183082805712587,108.439608944513,15.1869063624936));
#68241=CARTESIAN_POINT('Ctrl Pts',(0.170634865978392,108.441165588903,15.1881664611473));
#68242=CARTESIAN_POINT('Ctrl Pts',(0.158176642001111,108.442723116671,15.1893032368294));
#68243=CARTESIAN_POINT('Ctrl Pts',(0.126371161183714,108.446699439429,15.1922053918412));
#68244=CARTESIAN_POINT('Ctrl Pts',(0.0944986060005764,108.4506815256,15.1943037817774));
#68245=CARTESIAN_POINT('Ctrl Pts',(0.0625846769082255,108.454666905654,
15.195607396074));
#68246=CARTESIAN_POINT('Ctrl Pts',(0.0152080268535606,108.460583255081,
15.1975426287481));
#68247=CARTESIAN_POINT('Ctrl Pts',(-0.032258804083024,108.466505164633,
15.1977244485999));
#68248=CARTESIAN_POINT('Ctrl Pts',(-0.079733805609635,108.472412900431,
15.1961669242321));
#68249=CARTESIAN_POINT('Ctrl Pts',(-0.0797457843910396,108.472414391057,
15.1961665312412));
#68250=CARTESIAN_POINT('Ctrl Pts',(-0.0797577631728505,108.472415881682,
15.1961661381395));
#68251=CARTESIAN_POINT('Ctrl Pts',(-0.0797697419552132,108.472417372307,
15.1961657449271));
#68252=CARTESIAN_POINT('Ctrl Pts',(-0.152296998582491,108.481442570844,
15.1937849840778));
#68253=CARTESIAN_POINT('Ctrl Pts',(-0.224813819289416,108.490440401394,
15.1873581350595));
#68254=CARTESIAN_POINT('Ctrl Pts',(-0.296746304465991,108.499444664769,
15.1768154422734));
#68255=CARTESIAN_POINT('Ctrl Pts',(-0.347536648869933,108.505802427007,
15.1693714203376));
#68256=CARTESIAN_POINT('Ctrl Pts',(-0.398034968456748,108.512163966197,
15.1598757348434));
#68257=CARTESIAN_POINT('Ctrl Pts',(-0.448029752902181,108.518547390497,
15.1483127290138));
#68258=CARTESIAN_POINT('Ctrl Pts',(-0.482363440440263,108.522931177681,
15.1403718881128));
#68259=CARTESIAN_POINT('Ctrl Pts',(-0.516459656282199,108.527325447624,
15.1314561566781));
#68260=CARTESIAN_POINT('Ctrl Pts',(-0.550247651254368,108.531747944161,
15.1215771816121));
#68261=CARTESIAN_POINT('Ctrl Pts',(-0.550248083214224,108.531748000701,
15.1215770553152));
#68262=CARTESIAN_POINT('Ctrl Pts',(-0.550248515174057,108.53174805724,15.1215769290181));
#68263=CARTESIAN_POINT('Ctrl Pts',(-0.550248947133812,108.531748113779,
15.1215768027208));
#68264=CARTESIAN_POINT('Ctrl Pts',(-0.618316268900948,108.540657420602,
15.1016751421431));
#68265=CARTESIAN_POINT('Ctrl Pts',(-0.685276377078738,108.549720929029,
15.0778455464417));
#68266=CARTESIAN_POINT('Ctrl Pts',(-0.750740232549232,108.558866557164,
15.0503067853443));
#68267=CARTESIAN_POINT('Ctrl Pts',(-0.816138006644147,108.568002953401,
15.022795822781));
#68268=CARTESIAN_POINT('Ctrl Pts',(-0.880041776071536,108.577221298021,
14.9915831209971));
#68269=CARTESIAN_POINT('Ctrl Pts',(-0.942045786141081,108.586445406733,
14.9569354411003));
#68270=CARTESIAN_POINT('Ctrl Pts',(-1.01109530809121,108.596717650356,14.9183507474511));
#68271=CARTESIAN_POINT('Ctrl Pts',(-1.07780018936664,108.606993481739,14.8754981788652));
#68272=CARTESIAN_POINT('Ctrl Pts',(-1.14169435252236,108.617166231207,14.8286943605301));
#68273=CARTESIAN_POINT('Ctrl Pts',(-1.1623256668463,108.620450994344,14.8135814888695));
#68274=CARTESIAN_POINT('Ctrl Pts',(-1.18266355547137,108.623724954356,14.7980568093125));
#68275=CARTESIAN_POINT('Ctrl Pts',(-1.20269131967569,108.626984363034,14.7821315275056));
#68276=CARTESIAN_POINT('Ctrl Pts',(-1.27896116548536,108.639396861744,14.7214847785473));
#68277=CARTESIAN_POINT('Ctrl Pts',(-1.35075853641657,108.651601151534,14.6550100057487));
#68278=CARTESIAN_POINT('Ctrl Pts',(-1.41733223837496,108.663665506402,14.5835154665705));
#68279=CARTESIAN_POINT('Ctrl Pts',(-1.44916094053487,108.669433440985,14.5493341257914));
#68280=CARTESIAN_POINT('Ctrl Pts',(-1.47979587266395,108.675169475196,14.5140046271308));
#68281=CARTESIAN_POINT('Ctrl Pts',(-1.50915546850041,108.680881530702,14.4776111778369));
#68282=CARTESIAN_POINT('Ctrl Pts',(-1.57562356625245,108.693813229961,14.3952189215307));
#68283=CARTESIAN_POINT('Ctrl Pts',(-1.63555150521017,108.706623910656,14.3073783843346));
#68284=CARTESIAN_POINT('Ctrl Pts',(-1.68793735961649,108.719397688634,14.2151411815396));
#68285=CARTESIAN_POINT('Ctrl Pts',(-1.70429293358189,108.723385835299,14.1863434763237));
#68286=CARTESIAN_POINT('Ctrl Pts',(-1.71991364783203,108.727370439896,14.1571169868998));
#68287=CARTESIAN_POINT('Ctrl Pts',(-1.73476979970958,108.731354210771,14.1274930723761));
#68288=CARTESIAN_POINT('Ctrl Pts',(-1.76521444237875,108.739518133822,14.0667849226769));
#68289=CARTESIAN_POINT('Ctrl Pts',(-1.79245154811977,108.747681757492,14.0043990366965));
#68290=CARTESIAN_POINT('Ctrl Pts',(-1.8162652288592,108.755931073961,13.9407080569616));
#68291=CARTESIAN_POINT('Ctrl Pts',(-1.83105790375132,108.761055416474,13.9011442462643));
#68292=CARTESIAN_POINT('Ctrl Pts',(-1.84453056491651,108.766212918018,13.8610765079872));
#68293=CARTESIAN_POINT('Ctrl Pts',(-1.85664051206695,108.77142507718,13.8205896755338));
#68294=CARTESIAN_POINT('Ctrl Pts',(-1.85664298319636,108.771426140762,13.8205814138791));
#68295=CARTESIAN_POINT('Ctrl Pts',(-1.85664545426903,108.771427204345,13.8205731522046));
#68296=CARTESIAN_POINT('Ctrl Pts',(-1.85664792528492,108.771428267931,13.8205648905105));
#68297=CARTESIAN_POINT('Ctrl Pts',(-1.87611417489621,108.779807015837,13.7554806471141));
#68298=CARTESIAN_POINT('Ctrl Pts',(-1.89205583967587,108.788296679808,13.6891770610977));
#68299=CARTESIAN_POINT('Ctrl Pts',(-1.90444564021192,108.7968262807,13.6221275369253));
#68300=CARTESIAN_POINT('Ctrl Pts',(-1.91679911494914,108.805330873556,13.5552745960247));
#68301=CARTESIAN_POINT('Ctrl Pts',(-1.92562303307632,108.813874603247,13.4876802910133));
#68302=CARTESIAN_POINT('Ctrl Pts',(-1.93091198941321,108.822405534247,13.4197745662474));
#68303=CARTESIAN_POINT('Ctrl Pts',(-1.9328938959672,108.825602291222,13.3943285628406));
#68304=CARTESIAN_POINT('Ctrl Pts',(-1.93437952954262,108.828797478379,13.3688384235775));
#68305=CARTESIAN_POINT('Ctrl Pts',(-1.93536875477021,108.831989255394,13.3433253517718));
#68306=CARTESIAN_POINT('Ctrl Pts',(-1.93536888315373,108.831989669629,13.3433220406371));
#68307=CARTESIAN_POINT('Ctrl Pts',(-1.93536901152889,108.831990083864,13.343318729502));
#68308=CARTESIAN_POINT('Ctrl Pts',(-1.93536913989568,108.831990498099,13.3433154183666));
#68309=CARTESIAN_POINT('Ctrl Pts',(-1.93589688961357,108.833693526245,13.3297024681694));
#68310=CARTESIAN_POINT('Ctrl Pts',(-1.93628326895919,108.835395388104,13.3160849175915));
#68311=CARTESIAN_POINT('Ctrl Pts',(-1.93652779389579,108.837095796902,13.3024650858162));
#68312=CARTESIAN_POINT('Ctrl Pts',(-1.93786738009383,108.846411182846,13.2278512696566));
#68313=CARTESIAN_POINT('Ctrl Pts',(-1.93495108223821,108.855684228379,13.1531655757965));
#68314=CARTESIAN_POINT('Ctrl Pts',(-1.92777629531796,108.864964810249,13.0788321969946));
#68315=CARTESIAN_POINT('Ctrl Pts',(-1.92068525514588,108.874137065759,13.005366464692));
#68316=CARTESIAN_POINT('Ctrl Pts',(-1.90943317625142,108.883317050789,12.9322452604249));
#68317=CARTESIAN_POINT('Ctrl Pts',(-1.89401259176596,108.892534598748,12.8599152995615));
#68318=CARTESIAN_POINT('Ctrl Pts',(-1.89401126364815,108.892535392621,12.8599090700499));
#68319=CARTESIAN_POINT('Ctrl Pts',(-1.89400993549962,108.892536186495,12.8599028405442));
#68320=CARTESIAN_POINT('Ctrl Pts',(-1.89400860732034,108.892536980369,12.8598966110442));
#68321=CARTESIAN_POINT('Ctrl Pts',(-1.87503209950633,108.903879546833,12.7708919439851));
#68322=CARTESIAN_POINT('Ctrl Pts',(-1.84977984652267,108.915329006507,12.6830647589565));
#68323=CARTESIAN_POINT('Ctrl Pts',(-1.81850801035019,108.926765430093,12.5972872809673));
#68324=CARTESIAN_POINT('Ctrl Pts',(-1.81553173600613,108.92785388342,12.5891234716653));
#68325=CARTESIAN_POINT('Ctrl Pts',(-1.81250094854636,108.928942213636,12.5809782651924));
#68326=CARTESIAN_POINT('Ctrl Pts',(-1.8094158780891,108.930030314201,12.5728524357855));
#68327=CARTESIAN_POINT('Ctrl Pts',(-1.79554110192141,108.934923930729,12.5363073825172));
#68328=CARTESIAN_POINT('Ctrl Pts',(-1.78056790567763,108.939813294932,12.5001524243863));
#68329=CARTESIAN_POINT('Ctrl Pts',(-1.76451512912029,108.944690359364,12.4644529204725));
#68330=CARTESIAN_POINT('Ctrl Pts',(-1.72367364891042,108.957098588542,12.3736262290656));
#68331=CARTESIAN_POINT('Ctrl Pts',(-1.67583869639274,108.969427642048,12.2857384594742));
#68332=CARTESIAN_POINT('Ctrl Pts',(-1.62153010177169,108.981793910678,12.2018922735153));
#68333=CARTESIAN_POINT('Ctrl Pts',(-1.57377007371127,108.992669046388,12.1281563165807));
#68334=CARTESIAN_POINT('Ctrl Pts',(-1.52100199589187,109.003574081424,12.0575494940714));
#68335=CARTESIAN_POINT('Ctrl Pts',(-1.46364032579349,109.014577888671,11.9908697307493));
#68336=CARTESIAN_POINT('Ctrl Pts',(-1.46363051150188,109.014579771367,11.9908583221791));
#68337=CARTESIAN_POINT('Ctrl Pts',(-1.46362069707465,109.014581654067,11.9908469137213));
#68338=CARTESIAN_POINT('Ctrl Pts',(-1.46361088251184,109.014583536771,11.990835505376));
#68339=CARTESIAN_POINT('Ctrl Pts',(-1.4089382030819,109.025071265528,11.9272845540605));
#68340=CARTESIAN_POINT('Ctrl Pts',(-1.35005376806083,109.035687412997,11.8672224646944));
#68341=CARTESIAN_POINT('Ctrl Pts',(-1.28748464177007,109.046295375921,11.8110940219998));
#68342=CARTESIAN_POINT('Ctrl Pts',(-1.27388731706961,109.048600664884,11.7988963662949));
#68343=CARTESIAN_POINT('Ctrl Pts',(-1.26011615904058,109.050905544747,11.786884552742));
#68344=CARTESIAN_POINT('Ctrl Pts',(-1.24617688277292,109.053208576314,11.7750632427495));
#68345=CARTESIAN_POINT('Ctrl Pts',(-1.14591915656587,109.06977304522,11.6900389102171));
#68346=CARTESIAN_POINT('Ctrl Pts',(-1.03692821812283,109.086244866285,11.6148358074028));
#68347=CARTESIAN_POINT('Ctrl Pts',(-0.921408887350246,109.102683591447,
11.5508140451168));
#68348=CARTESIAN_POINT('Ctrl Pts',(-0.807228492933731,109.118931782205,
11.4875343323607));
#68349=CARTESIAN_POINT('Ctrl Pts',(-0.686667685469148,109.135149189964,
11.4351822760625));
#68350=CARTESIAN_POINT('Ctrl Pts',(-0.561923213141406,109.151403428664,
11.3951093109741));
#68351=CARTESIAN_POINT('Ctrl Pts',(-0.533602355987048,109.15509364406,11.3860115072892));
#68352=CARTESIAN_POINT('Ctrl Pts',(-0.505066213971739,109.158785746996,
11.3775466115163));
#68353=CARTESIAN_POINT('Ctrl Pts',(-0.476341145705833,109.162480477521,
11.3697303378323));
#68354=CARTESIAN_POINT('Ctrl Pts',(-0.432229202362458,109.168154328043,
11.3577271976233));
#68355=CARTESIAN_POINT('Ctrl Pts',(-0.387670939531217,109.173834579638,
11.3472537403331));
#68356=CARTESIAN_POINT('Ctrl Pts',(-0.342778193468239,109.179540904526,
11.3383573875759));
#68357=CARTESIAN_POINT('Ctrl Pts',(-0.342773072460125,109.179541555458,
11.3383563727506));
#68358=CARTESIAN_POINT('Ctrl Pts',(-0.342767951447331,109.179542206391,
11.3383553579457));
#68359=CARTESIAN_POINT('Ctrl Pts',(-0.342762830429772,109.179542857324,
11.3383543431613));
#68360=CARTESIAN_POINT('Ctrl Pts',(-0.253722983770747,109.190860722285,
11.3207101439316));
#68361=CARTESIAN_POINT('Ctrl Pts',(-0.163252302171303,109.202310914098,
11.3092405498241));
#68362=CARTESIAN_POINT('Ctrl Pts',(-0.0722659009461916,109.213799137132,
11.3039408459732));
#68363=CARTESIAN_POINT('Ctrl Pts',(-0.0536508068134595,109.216149536205,
11.3028565687106));
#68364=CARTESIAN_POINT('Ctrl Pts',(-0.0350142409579838,109.218501515008,
11.3020304193361));
#68365=CARTESIAN_POINT('Ctrl Pts',(-0.0163642026663661,109.220854247431,
11.3014621481135));
#68366=CARTESIAN_POINT('Ctrl Pts',(0.0945107911799775,109.234841306805,
11.2980837599663));
#68367=CARTESIAN_POINT('Ctrl Pts',(0.205867162649476,109.248853458614,11.3038180654636));
#68368=CARTESIAN_POINT('Ctrl Pts',(0.316203639275899,109.262743079122,11.3186132619521));
#68369=CARTESIAN_POINT('Ctrl Pts',(0.344610819783086,109.266319094679,11.322422426701));
#68370=CARTESIAN_POINT('Ctrl Pts',(0.372951158686283,109.269887196702,11.3268323794333));
#68371=CARTESIAN_POINT('Ctrl Pts',(0.40120053760262,109.273445370479,11.3318428876719));
#68372=CARTESIAN_POINT('Ctrl Pts',(0.504283837842697,109.286429312423,11.3501264657517));
#68373=CARTESIAN_POINT('Ctrl Pts',(0.606178065701835,109.299282835421,11.3764115366991));
#68374=CARTESIAN_POINT('Ctrl Pts',(0.705579404323949,109.312191801006,11.4105266508771));
#68375=CARTESIAN_POINT('Ctrl Pts',(0.711582751676879,109.312971438438,11.4125870344014));
#68376=CARTESIAN_POINT('Ctrl Pts',(0.71757702088544,109.313751280418,11.4146759831112));
#68377=CARTESIAN_POINT('Ctrl Pts',(0.723561930260544,109.314531368777,11.4167934613312));
#68378=CARTESIAN_POINT('Ctrl Pts',(0.797385807564586,109.324153761308,11.4429125623083));
#68379=CARTESIAN_POINT('Ctrl Pts',(0.869777372373823,109.333813896558,11.4733732610354));
#68380=CARTESIAN_POINT('Ctrl Pts',(0.940120873681946,109.343572377364,11.508052956718));
#68381=CARTESIAN_POINT('Ctrl Pts',(0.947088368344305,109.344538950845,11.5114879662081));
#68382=CARTESIAN_POINT('Ctrl Pts',(0.954035798632474,109.345506490686,11.5149643365429));
#68383=CARTESIAN_POINT('Ctrl Pts',(0.96096258594782,109.346475056762,11.5184819285432));
#68384=CARTESIAN_POINT('Ctrl Pts',(0.960979521509151,109.346477424845,11.5184905288354));
#68385=CARTESIAN_POINT('Ctrl Pts',(0.960996456953629,109.346479792936,11.5184991293772));
#68386=CARTESIAN_POINT('Ctrl Pts',(0.961013392281206,109.346482161034,11.5185077301684));
#68387=CARTESIAN_POINT('Ctrl Pts',(1.03876129819005,109.357353795348,11.5579928538976));
#68388=CARTESIAN_POINT('Ctrl Pts',(1.11404612503515,109.368383165716,11.6027406483499));
#68389=CARTESIAN_POINT('Ctrl Pts',(1.18625174548857,109.379455654256,11.6522472692857));
#68390=CARTESIAN_POINT('Ctrl Pts',(1.20861419916872,109.382884861159,11.6675797255486));
#68391=CARTESIAN_POINT('Ctrl Pts',(1.23068129245706,109.386318178422,11.6833682556536));
#68392=CARTESIAN_POINT('Ctrl Pts',(1.25243477358313,109.389752134003,11.6995968924701));
#68393=CARTESIAN_POINT('Ctrl Pts',(1.32179139372386,109.400700613991,11.7513386524469));
#68394=CARTESIAN_POINT('Ctrl Pts',(1.38797012139924,109.411655731262,11.8075590966998));
#68395=CARTESIAN_POINT('Ctrl Pts',(1.45048149457184,109.422526164979,11.8678281572102));
#68396=CARTESIAN_POINT('Ctrl Pts',(1.53309961114421,109.436893066784,11.9474827226795));
#68397=CARTESIAN_POINT('Ctrl Pts',(1.60933543245218,109.451116239369,12.0342334673502));
#68398=CARTESIAN_POINT('Ctrl Pts',(1.67803652371654,109.465353016301,12.1269321145783));
#68399=CARTESIAN_POINT('Ctrl Pts',(1.7320388580821,109.476543801978,12.1997976724716));
#68400=CARTESIAN_POINT('Ctrl Pts',(1.78138165387847,109.487744706282,12.2763416981877));
#68401=CARTESIAN_POINT('Ctrl Pts',(1.82544946795883,109.499017374168,12.3559056472522));
#68402=CARTESIAN_POINT('Ctrl Pts',(1.8369529107494,109.501959986431,12.376674985495));
#68403=CARTESIAN_POINT('Ctrl Pts',(1.84809716987093,109.504907498156,12.3976500241351));
#68404=CARTESIAN_POINT('Ctrl Pts',(1.85887186978288,109.507861025223,12.4188189068126));
#68405=CARTESIAN_POINT('Ctrl Pts',(1.86940297836426,109.510747779796,12.4395092094517));
#68406=CARTESIAN_POINT('Ctrl Pts',(1.87958062550558,109.513640095786,12.460383958756));
#68407=CARTESIAN_POINT('Ctrl Pts',(1.88939488094984,109.516538702891,12.4814308649676));
#68408=CARTESIAN_POINT('Ctrl Pts',(1.88940003301704,109.516540224537,12.4814419136993));
#68409=CARTESIAN_POINT('Ctrl Pts',(1.88940518498505,109.516541746184,12.4814529624812));
#68410=CARTESIAN_POINT('Ctrl Pts',(1.8894103368539,109.516543267832,12.4814640113134));
#68411=CARTESIAN_POINT('Ctrl Pts',(1.92307171724716,109.526485441465,12.5536550852641));
#68412=CARTESIAN_POINT('Ctrl Pts',(1.95249726178874,109.536480542927,12.62799404341));
#68413=CARTESIAN_POINT('Ctrl Pts',(1.97753897570652,109.546486591178,12.703907048022));
#68414=CARTESIAN_POINT('Ctrl Pts',(2.00001983487993,109.555469385341,12.7720569187423));
#68415=CARTESIAN_POINT('Ctrl Pts',(2.0189701699992,109.564460801653,12.8414756753979));
#68416=CARTESIAN_POINT('Ctrl Pts',(2.03430731340211,109.573438968279,12.911800097432));
#68417=CARTESIAN_POINT('Ctrl Pts',(2.05096107398141,109.583187865678,12.9881615199386));
#68418=CARTESIAN_POINT('Ctrl Pts',(2.06335606598736,109.592922388582,13.0655990543191));
#68419=CARTESIAN_POINT('Ctrl Pts',(2.07140518948593,109.602706524858,13.143617414013));
#68420=CARTESIAN_POINT('Ctrl Pts',(2.07140601901899,109.602707533199,13.143625454492));
#68421=CARTESIAN_POINT('Ctrl Pts',(2.07140684850574,109.602708541541,13.1436334949769));
#68422=CARTESIAN_POINT('Ctrl Pts',(2.07140767794618,109.602709549882,13.1436415354678));
#68423=CARTESIAN_POINT('Ctrl Pts',(2.08102833810477,109.61440528097,13.2369029998119));
#68424=CARTESIAN_POINT('Ctrl Pts',(2.08442071776682,109.626117496683,13.3309604660696));
#68425=CARTESIAN_POINT('Ctrl Pts',(2.08148699424942,109.637856538144,13.4249853359634));
#68426=CARTESIAN_POINT('Ctrl Pts',(2.08047818792699,109.641893189578,13.4573172454469));
#68427=CARTESIAN_POINT('Ctrl Pts',(2.07872114074448,109.645932962924,13.4896448314478));
#68428=CARTESIAN_POINT('Ctrl Pts',(2.07621144714014,109.649976082837,13.5219328815354));
#68429=CARTESIAN_POINT('Ctrl Pts',(2.06893545016503,109.661697724157,13.6155410233275));
#68430=CARTESIAN_POINT('Ctrl Pts',(2.05533102326315,109.673448715969,13.7088219604897));
#68431=CARTESIAN_POINT('Ctrl Pts',(2.03530678847665,109.685235629954,13.8008634064405));
#68432=CARTESIAN_POINT('Ctrl Pts',(2.03280776174858,109.68670663813,13.8123501891302));
#68433=CARTESIAN_POINT('Ctrl Pts',(2.03020879341823,109.688178184181,13.8238175846766));
#68434=CARTESIAN_POINT('Ctrl Pts',(2.02750975357541,109.689650261466,13.8352637537059));
#68435=CARTESIAN_POINT('Ctrl Pts',(2.02750691238552,109.689651811073,13.8352758027091));
#68436=CARTESIAN_POINT('Ctrl Pts',(2.02750407108507,109.689653360682,13.8352878516887));
#68437=CARTESIAN_POINT('Ctrl Pts',(2.02750122967404,109.689654910292,13.8352999006448));
#68438=CARTESIAN_POINT('Ctrl Pts',(2.00450040737611,109.702198787307,13.9328345040158));
#68439=CARTESIAN_POINT('Ctrl Pts',(1.97425423397393,109.714849273242,14.0288264559821));
#68440=CARTESIAN_POINT('Ctrl Pts',(1.93724533476024,109.727468592401,14.1223759642247));
#68441=CARTESIAN_POINT('Ctrl Pts',(1.89512619194701,109.741830405835,14.2288429270768));
#68442=CARTESIAN_POINT('Ctrl Pts',(1.8442349654792,109.75615667757,14.3321889440122));
#68443=CARTESIAN_POINT('Ctrl Pts',(1.78528329627254,109.770497721719,14.4311299418159));
#68444=CARTESIAN_POINT('Ctrl Pts',(1.77340675816491,109.773386901273,14.4510628215229));
#68445=CARTESIAN_POINT('Ctrl Pts',(1.76120291576132,109.776276684223,14.4708168462382));
#68446=CARTESIAN_POINT('Ctrl Pts',(1.74867736162986,109.779167487636,14.4903813935025));
#68447=CARTESIAN_POINT('Ctrl Pts',(1.6843329681792,109.79401768829,14.5908854441533));
#68448=CARTESIAN_POINT('Ctrl Pts',(1.61149537262497,109.808896191927,14.6863869329));
#68449=CARTESIAN_POINT('Ctrl Pts',(1.53103586007233,109.823840129088,14.7753075840577));
#68450=CARTESIAN_POINT('Ctrl Pts',(1.51740666653029,109.82637151171,14.7903700263478));
#68451=CARTESIAN_POINT('Ctrl Pts',(1.50355887156844,109.82890477356,14.8052437100646));
#68452=CARTESIAN_POINT('Ctrl Pts',(1.48949682534355,109.831440097097,14.8199210570519));
#68453=CARTESIAN_POINT('Ctrl Pts',(1.42564669235199,109.842951988212,14.8865650249433));
#68454=CARTESIAN_POINT('Ctrl Pts',(1.35738064405652,109.854505653173,14.9491533697211));
#68455=CARTESIAN_POINT('Ctrl Pts',(1.28516978592211,109.86610476067,15.0069531561418));
#68456=CARTESIAN_POINT('Ctrl Pts',(1.28515132482487,109.866107726045,15.0069679329705));
#68457=CARTESIAN_POINT('Ctrl Pts',(1.28513286346812,109.866110691424,15.006982709488));
#68458=CARTESIAN_POINT('Ctrl Pts',(1.2851144018518,109.866113656806,15.0069974856946));
#68459=CARTESIAN_POINT('Ctrl Pts',(1.20743211661619,109.878591312462,15.069172404177));
#68460=CARTESIAN_POINT('Ctrl Pts',(1.12515570427157,109.891138404837,15.1258417777281));
#68461=CARTESIAN_POINT('Ctrl Pts',(1.03914322942434,109.90365553316,15.1766500823808));
#68462=CARTESIAN_POINT('Ctrl Pts',(0.937625917716596,109.918429032235,15.2366172267971));
#68463=CARTESIAN_POINT('Ctrl Pts',(0.830857999498407,109.933167531805,15.2884484472141));
#68464=CARTESIAN_POINT('Ctrl Pts',(0.720252908317178,109.947923312942,15.3315176108421));
#68465=CARTESIAN_POINT('Ctrl Pts',(0.690590419332554,109.951880573777,15.3430680609891));
#68466=CARTESIAN_POINT('Ctrl Pts',(0.660651839016121,109.955839082895,15.3539880557953));
#68467=CARTESIAN_POINT('Ctrl Pts',(0.630464239915361,109.959799860039,15.3642649019636));
#68468=CARTESIAN_POINT('Ctrl Pts',(0.526021692407841,109.973503290169,15.3998205614443));
#68469=CARTESIAN_POINT('Ctrl Pts',(0.418598095206419,109.987234664124,15.4276730546173));
#68470=CARTESIAN_POINT('Ctrl Pts',(0.309471377177917,110.001015880522,15.4472650485884));
#68471=CARTESIAN_POINT('Ctrl Pts',(0.271024458714651,110.005871202049,15.4541675909571));
#68472=CARTESIAN_POINT('Ctrl Pts',(0.232366308112867,110.010732711996,15.4600452356261));
#68473=CARTESIAN_POINT('Ctrl Pts',(0.193553207676388,110.015601372545,15.4648751047488));
#68474=CARTESIAN_POINT('Ctrl Pts',(0.11364529300297,110.025624908602,15.4748187775139));
#68475=CARTESIAN_POINT('Ctrl Pts',(0.0330870109350791,110.03567774002,15.4803178638995));
#68476=CARTESIAN_POINT('Ctrl Pts',(-0.047587460874768,110.045760037852,
15.4811903732368));
#68477=CARTESIAN_POINT('Ctrl Pts',(-0.0476041706067929,110.045762126152,
15.4811905539557));
#68478=CARTESIAN_POINT('Ctrl Pts',(-0.0476208803467128,110.045764214453,
15.4811907344762));
#68479=CARTESIAN_POINT('Ctrl Pts',(-0.0476375900947904,110.045766302757,
15.4811909147984));
#68480=CARTESIAN_POINT('Ctrl Pts',(-0.146456125117576,110.058116163592,
15.4822573087886));
#68481=CARTESIAN_POINT('Ctrl Pts',(-0.245555396409884,110.070523073124,
15.476388413267));
#68482=CARTESIAN_POINT('Ctrl Pts',(-0.344037521982087,110.082932043234,
15.4637870451847));
#68483=CARTESIAN_POINT('Ctrl Pts',(-0.463325542175896,110.097962603027,
15.448523440327));
#68484=CARTESIAN_POINT('Ctrl Pts',(-0.581754791070992,110.113002077922,
15.4233778358814));
#68485=CARTESIAN_POINT('Ctrl Pts',(-0.697729150556525,110.12808094041,15.3886750338168));
#68486=CARTESIAN_POINT('Ctrl Pts',(-0.797186004854783,110.141012214497,
15.3589147355579));
#68487=CARTESIAN_POINT('Ctrl Pts',(-0.894835413450012,110.153972851852,
15.322119651773));
#68488=CARTESIAN_POINT('Ctrl Pts',(-0.989551672779695,110.166966655232,
15.2785458398567));
#68489=CARTESIAN_POINT('Ctrl Pts',(-1.00574172623382,110.169187713926,15.271097674683));
#68490=CARTESIAN_POINT('Ctrl Pts',(-1.02184612180391,110.171409741364,15.2634515657377));
#68491=CARTESIAN_POINT('Ctrl Pts',(-1.03785929845104,110.173632756148,15.2556089330049));
#68492=CARTESIAN_POINT('Ctrl Pts',(-1.06048518812931,110.176773774845,15.2445276499522));
#68493=CARTESIAN_POINT('Ctrl Pts',(-1.08292833471847,110.179916666637,15.2330543039541));
#68494=CARTESIAN_POINT('Ctrl Pts',(-1.10517223570307,110.183061325066,15.2211936368503));
#68495=CARTESIAN_POINT('Ctrl Pts',(-1.10518397338107,110.183062984442,15.2211873782048));
#68496=CARTESIAN_POINT('Ctrl Pts',(-1.10519571100572,110.183064643818,15.2211811194503));
#68497=CARTESIAN_POINT('Ctrl Pts',(-1.10520744857709,110.183066303196,15.2211748605868));
#68498=CARTESIAN_POINT('Ctrl Pts',(-1.19925586538353,110.196362222771,15.1710251161729));
#68499=CARTESIAN_POINT('Ctrl Pts',(-1.28987922969665,110.209709506862,15.1138739398531));
#68500=CARTESIAN_POINT('Ctrl Pts',(-1.37612755368538,110.223084635313,15.0504439106069));
#68501=CARTESIAN_POINT('Ctrl Pts',(-1.38880111623854,110.225050012949,15.0411233301454));
#68502=CARTESIAN_POINT('Ctrl Pts',(-1.40138025994434,110.227015991325,15.0316672540107));
#68503=CARTESIAN_POINT('Ctrl Pts',(-1.41386202424372,110.22898249533,15.0220780525104));
#68504=CARTESIAN_POINT('Ctrl Pts',(-1.49237304676439,110.241351919761,14.9617614180278));
#68505=CARTESIAN_POINT('Ctrl Pts',(-1.56703798599791,110.253742879956,14.896176250949));
#68506=CARTESIAN_POINT('Ctrl Pts',(-1.63721950063078,110.266154511041,14.8258150679101));
#68507=CARTESIAN_POINT('Ctrl Pts',(-1.72392691560699,110.281488754718,14.7388856773451));
#68508=CARTESIAN_POINT('Ctrl Pts',(-1.80382090971275,110.296861122966,14.6446231324412));
#68509=CARTESIAN_POINT('Ctrl Pts',(-1.87552555125901,110.312277975576,14.5440909255201));
#68510=CARTESIAN_POINT('Ctrl Pts',(-1.89151977978687,110.315716813823,14.5216665042102));
#68511=CARTESIAN_POINT('Ctrl Pts',(-1.90710568589463,110.319157644916,14.4989316743978));
#68512=CARTESIAN_POINT('Ctrl Pts',(-1.92226692633959,110.322600156949,14.4759011327845));
#68513=CARTESIAN_POINT('Ctrl Pts',(-1.92227108889527,110.322601102099,14.475894809693));
#68514=CARTESIAN_POINT('Ctrl Pts',(-1.92227525141932,110.322602047249,14.4758884865785));
#68515=CARTESIAN_POINT('Ctrl Pts',(-1.92227941391178,110.3226029924,14.4758821634412));
#68516=CARTESIAN_POINT('Ctrl Pts',(-1.98371355793695,110.336552448123,14.3825591039405));
#68517=CARTESIAN_POINT('Ctrl Pts',(-2.0382585472013,110.350531220208,14.2842470159127));
#68518=CARTESIAN_POINT('Ctrl Pts',(-2.085372516468,110.364537239114,14.1821958687918));
#68519=CARTESIAN_POINT('Ctrl Pts',(-2.10194678452092,110.369464429824,14.1462951986972));
#68520=CARTESIAN_POINT('Ctrl Pts',(-2.11760181028108,110.374394990735,14.1099320549485));
#68521=CARTESIAN_POINT('Ctrl Pts',(-2.13231535993761,110.379328825668,14.0731615550672));
#68522=CARTESIAN_POINT('Ctrl Pts',(-2.18231562772883,110.396095212681,13.9482063346211));
#68523=CARTESIAN_POINT('Ctrl Pts',(-2.22144860440119,110.412899907065,13.8185482593629));
#68524=CARTESIAN_POINT('Ctrl Pts',(-2.24891684882211,110.429768454545,13.6861326704635));
#68525=CARTESIAN_POINT('Ctrl Pts',(-2.25313778887605,110.432360579714,13.6657848734078));
#68526=CARTESIAN_POINT('Ctrl Pts',(-2.25708319521983,110.434954212933,13.6453719205305));
#68527=CARTESIAN_POINT('Ctrl Pts',(-2.26075007217476,110.437549447166,13.6249008325395));
#68528=CARTESIAN_POINT('Ctrl Pts',(-2.26815586153436,110.44279089876,13.5835565039769));
#68529=CARTESIAN_POINT('Ctrl Pts',(-2.27442596979226,110.44803909271,13.5419732460962));
#68530=CARTESIAN_POINT('Ctrl Pts',(-2.27953531506399,110.453295211892,13.5002048223747));
#68531=CARTESIAN_POINT('Ctrl Pts',(-2.28308796134232,110.456949913475,13.4711622685457));
#68532=CARTESIAN_POINT('Ctrl Pts',(-2.286079380829,110.460608471516,13.4420299700733));
#68533=CARTESIAN_POINT('Ctrl Pts',(-2.28850068218742,110.464270298831,13.4128278836824));
#68534=CARTESIAN_POINT('Ctrl Pts',(-2.28850195542795,110.464272224401,13.4128125277749));
#68535=CARTESIAN_POINT('Ctrl Pts',(-2.28850322851069,110.464274149973,13.4127971718496));
#68536=CARTESIAN_POINT('Ctrl Pts',(-2.28850450143566,110.464276075545,13.4127818159066));
#68537=CARTESIAN_POINT('Ctrl Pts',(-2.2991622457932,110.480398200416,13.2842120107848));
#68538=CARTESIAN_POINT('Ctrl Pts',(-2.29876151461231,110.496569795702,13.1544009523245));
#68539=CARTESIAN_POINT('Ctrl Pts',(-2.2875131865112,110.512782139525,13.025148513299));
#68540=CARTESIAN_POINT('Ctrl Pts',(-2.27611672148484,110.529207994791,12.894193860511));
#68541=CARTESIAN_POINT('Ctrl Pts',(-2.25358266164367,110.545675397593,12.7638131799088));
#68542=CARTESIAN_POINT('Ctrl Pts',(-2.22012284844778,110.562172038801,12.6359232236228));
#68543=CARTESIAN_POINT('Ctrl Pts',(-2.18891553345408,110.57755813422,12.5166427564252));
#68544=CARTESIAN_POINT('Ctrl Pts',(-2.14820301977644,110.592969364365,12.3995305454992));
#68545=CARTESIAN_POINT('Ctrl Pts',(-2.09817411773941,110.608397046164,12.2861639713865));
#68546=CARTESIAN_POINT('Ctrl Pts',(-2.09817273107111,110.608397473778,12.2861608291662));
#68547=CARTESIAN_POINT('Ctrl Pts',(-2.09817134439567,110.608397901392,12.2861576869487));
#68548=CARTESIAN_POINT('Ctrl Pts',(-2.09816995771305,110.608398329007,12.2861545447341));
#68549=CARTESIAN_POINT('Ctrl Pts',(-2.05908247704408,110.62045182211,12.1975825444839));
#68550=CARTESIAN_POINT('Ctrl Pts',(-2.01430181816575,110.632535849416,12.1112862642052));
#68551=CARTESIAN_POINT('Ctrl Pts',(-1.96422019338439,110.644693528793,12.02794157505));
#68552=CARTESIAN_POINT('Ctrl Pts',(-1.91397081635425,110.656891931251,11.944317716457));
#68553=CARTESIAN_POINT('Ctrl Pts',(-1.85837309022311,110.669166915175,11.8636481585629));
#68554=CARTESIAN_POINT('Ctrl Pts',(-1.79784476165745,110.681487677843,11.7866307540655));
#68555=CARTESIAN_POINT('Ctrl Pts',(-1.79783778251977,110.681489098472,11.7866218736771));
#68556=CARTESIAN_POINT('Ctrl Pts',(-1.79783080331657,110.681490519101,11.7866129933372));
#68557=CARTESIAN_POINT('Ctrl Pts',(-1.79782382404781,110.681491939732,11.7866041130458));
#68558=CARTESIAN_POINT('Ctrl Pts',(-1.7358533973767,110.694106020649,11.7077540982695));
#68559=CARTESIAN_POINT('Ctrl Pts',(-1.66871801896252,110.706756334567,11.6327293597556));
#68560=CARTESIAN_POINT('Ctrl Pts',(-1.59693074248384,110.719401143423,11.562124819429));
#68561=CARTESIAN_POINT('Ctrl Pts',(-1.52872908249229,110.731414371902,11.4950468205215));
#68562=CARTESIAN_POINT('Ctrl Pts',(-1.45632803878547,110.743422408375,11.4319598983437));
#68563=CARTESIAN_POINT('Ctrl Pts',(-1.38018946334844,110.755388637441,11.3733977294143));
#68564=CARTESIAN_POINT('Ctrl Pts',(-1.38016583383902,110.755392351145,11.3733795547202));
#68565=CARTESIAN_POINT('Ctrl Pts',(-1.38014220396964,110.755396064845,11.3733613804617));
#68566=CARTESIAN_POINT('Ctrl Pts',(-1.38011857374031,110.75539977854,11.3733432066391));
#68567=CARTESIAN_POINT('Ctrl Pts',(-1.30196435758779,110.767682392561,11.313235416559));
#68568=CARTESIAN_POINT('Ctrl Pts',(-1.21984993539952,110.779927172049,11.2578792232138));
#68569=CARTESIAN_POINT('Ctrl Pts',(-1.13445157810722,110.792197271441,11.2077439862546));
#68570=CARTESIAN_POINT('Ctrl Pts',(-1.04906646440958,110.804465467984,11.1576165242781));
#68571=CARTESIAN_POINT('Ctrl Pts',(-0.960399632900019,110.816759314713,
11.1127059378167));
#68572=CARTESIAN_POINT('Ctrl Pts',(-0.86907193265452,110.829148517403,11.0734487355745));
#68573=CARTESIAN_POINT('Ctrl Pts',(-0.869057767339681,110.829150439021,
11.0734426466154));
#68574=CARTESIAN_POINT('Ctrl Pts',(-0.869043601960864,110.829152360641,
11.0734365577924));
#68575=CARTESIAN_POINT('Ctrl Pts',(-0.869029436517997,110.829154282264,
11.0734304691054));
#68576=CARTESIAN_POINT('Ctrl Pts',(-0.841101772249262,110.832942828244,
11.0614264105134));
#68577=CARTESIAN_POINT('Ctrl Pts',(-0.812930052409786,110.836742231314,
11.0499537942301));
#68578=CARTESIAN_POINT('Ctrl Pts',(-0.784532884087689,110.840553326691,
11.0390191405254));
#68579=CARTESIAN_POINT('Ctrl Pts',(-0.695612383247482,110.852487069725,
11.004779286998));
#68580=CARTESIAN_POINT('Ctrl Pts',(-0.60447439323736,110.864536520627,10.9758112663676));
#68581=CARTESIAN_POINT('Ctrl Pts',(-0.511741795115254,110.876623330507,
10.9523249234607));
#68582=CARTESIAN_POINT('Ctrl Pts',(-0.440408054463211,110.885921003372,
10.9342582594427));
#68583=CARTESIAN_POINT('Ctrl Pts',(-0.368132052889044,110.895240438188,
10.9194367423256));
#68584=CARTESIAN_POINT('Ctrl Pts',(-0.29522758730732,110.904542379711,10.9079600696815));
#68585=CARTESIAN_POINT('Ctrl Pts',(-0.295187514083616,110.904547492687,
10.9079537613262));
#68586=CARTESIAN_POINT('Ctrl Pts',(-0.295147440669938,110.904552605657,
10.9079474539813));
#68587=CARTESIAN_POINT('Ctrl Pts',(-0.295107367066453,110.904557718623,
10.9079411476467));
#68588=CARTESIAN_POINT('Ctrl Pts',(-0.19616115143769,110.917182203022,10.89237010119));
#68589=CARTESIAN_POINT('Ctrl Pts',(-0.0960277085892771,110.929773050324,
10.8829525041896));
#68590=CARTESIAN_POINT('Ctrl Pts',(0.0045203639492899,110.942329915504,
10.8797700252342));
#68591=CARTESIAN_POINT('Ctrl Pts',(0.00456871948157908,110.942335954346,
10.8797684947179));
#68592=CARTESIAN_POINT('Ctrl Pts',(0.004617075109645,110.94234199318,10.8797669656437));
#68593=CARTESIAN_POINT('Ctrl Pts',(0.00466543083367732,110.942348032006,
10.8797654380116));
#68594=CARTESIAN_POINT('Ctrl Pts',(0.105219794853847,110.95490560042,10.8765887701901));
#68595=CARTESIAN_POINT('Ctrl Pts',(0.20618849603257,110.967429568142,10.8796480880734));
#68596=CARTESIAN_POINT('Ctrl Pts',(0.306777259267146,110.979927951317,10.8890214945142));
#68597=CARTESIAN_POINT('Ctrl Pts',(0.306819736736933,110.979933229239,10.8890254527952));
#68598=CARTESIAN_POINT('Ctrl Pts',(0.306862214139012,110.979938507157,10.8890294122022));
#68599=CARTESIAN_POINT('Ctrl Pts',(0.30690469147322,110.97994378507,10.8890333727351));
#68600=CARTESIAN_POINT('Ctrl Pts',(0.404730243812092,110.992098850771,10.8981545036191));
#68601=CARTESIAN_POINT('Ctrl Pts',(0.502216743195765,111.004240432774,10.913253758302));
#68602=CARTESIAN_POINT('Ctrl Pts',(0.598599075847304,111.016457344285,10.9342321298295));
#68603=CARTESIAN_POINT('Ctrl Pts',(0.662418877813026,111.024546802713,10.9481230108615));
#68604=CARTESIAN_POINT('Ctrl Pts',(0.725756424234182,111.032669579998,10.9645909835171));
#68605=CARTESIAN_POINT('Ctrl Pts',(0.788409092860007,111.040853078828,10.9836101491186));
#68606=CARTESIAN_POINT('Ctrl Pts',(0.825776009236343,111.045733830488,10.994953442009));
#68607=CARTESIAN_POINT('Ctrl Pts',(0.862899977419791,111.050636232305,11.0072045053116));
#68608=CARTESIAN_POINT('Ctrl Pts',(0.899737380831095,111.055557395671,11.0203552379715));
#68609=CARTESIAN_POINT('Ctrl Pts',(0.899763975116234,111.055560948441,11.0203647319722));
#68610=CARTESIAN_POINT('Ctrl Pts',(0.89979056925204,111.055564501221,11.0203742264418));
#68611=CARTESIAN_POINT('Ctrl Pts',(0.899817163238463,111.055568054011,11.0203837213803));
#68612=CARTESIAN_POINT('Ctrl Pts',(0.995769942590633,111.068386742687,11.0546420580142));
#68613=CARTESIAN_POINT('Ctrl Pts',(1.08975364505154,111.081297354889,11.0949830330797));
#68614=CARTESIAN_POINT('Ctrl Pts',(1.18105978369377,111.094208322136,11.1411116544715));
#68615=CARTESIAN_POINT('Ctrl Pts',(1.27231753550347,111.107112447338,11.1872158304327));
#68616=CARTESIAN_POINT('Ctrl Pts',(1.36089921071295,111.120016402732,11.239104209367));
#68617=CARTESIAN_POINT('Ctrl Pts',(1.44603641190564,111.132819799862,11.2964523654609));
#68618=CARTESIAN_POINT('Ctrl Pts',(1.44608155348979,111.1328265885,11.2964827726927));
#68619=CARTESIAN_POINT('Ctrl Pts',(1.44612669410611,111.13283337711,11.2965131814593));
#68620=CARTESIAN_POINT('Ctrl Pts',(1.44617183375462,111.132840165691,11.2965435917605));
#68621=CARTESIAN_POINT('Ctrl Pts',(1.51563559984642,111.14328686715,11.3433409001863));
#68622=CARTESIAN_POINT('Ctrl Pts',(1.58282234530331,111.153668629732,11.393782710617));
#68623=CARTESIAN_POINT('Ctrl Pts',(1.64746239050899,111.1640970458,11.4475182852451));
#68624=CARTESIAN_POINT('Ctrl Pts',(1.66204961579713,111.166450411336,11.459644714467));
#68625=CARTESIAN_POINT('Ctrl Pts',(1.676507349584,111.168806202672,11.4719390412158));
#68626=CARTESIAN_POINT('Ctrl Pts',(1.69083281828931,111.171165781603,11.4843975467765));
#68627=CARTESIAN_POINT('Ctrl Pts',(1.69086858377381,111.171171672614,11.4844286511331));
#68628=CARTESIAN_POINT('Ctrl Pts',(1.69090434843375,111.171177563648,11.484459756513));
#68629=CARTESIAN_POINT('Ctrl Pts',(1.6909401122692,111.171183454705,11.4844908629163));
#68630=CARTESIAN_POINT('Ctrl Pts',(1.74635565641906,111.180311562881,11.5326897836048));
#68631=CARTESIAN_POINT('Ctrl Pts',(1.79978000550124,111.18949556541,11.5833355296906));
#68632=CARTESIAN_POINT('Ctrl Pts',(1.85083037852574,111.198601923597,11.6364041098969));
#68633=CARTESIAN_POINT('Ctrl Pts',(1.87146057282596,111.202281934685,11.6578498909173));
#68634=CARTESIAN_POINT('Ctrl Pts',(1.89170248915674,111.205949118275,11.679690867053));
#68635=CARTESIAN_POINT('Ctrl Pts',(1.9115288023957,111.209594155977,11.7019231056942));
#68636=CARTESIAN_POINT('Ctrl Pts',(1.91155359787195,111.209598714588,11.7019509101044));
#68637=CARTESIAN_POINT('Ctrl Pts',(1.9115783926982,111.209603273164,11.7019787151265));
#68638=CARTESIAN_POINT('Ctrl Pts',(1.91160318687453,111.209607831706,11.7020065207606));
#68639=CARTESIAN_POINT('Ctrl Pts',(1.95919582421182,111.218357991857,11.7553796774532));
#68640=CARTESIAN_POINT('Ctrl Pts',(2.00440512406786,111.22698198537,11.81102038669));
#68641=CARTESIAN_POINT('Ctrl Pts',(2.04710225378665,111.235599353169,11.8686802785851));
#68642=CARTESIAN_POINT('Ctrl Pts',(2.06145000751985,111.23849509515,11.8880560524285));
#68643=CARTESIAN_POINT('Ctrl Pts',(2.07551435835042,111.241390157184,11.9076601534837));
#68644=CARTESIAN_POINT('Ctrl Pts',(2.08929110769117,111.244289249369,11.9274842264238));
#68645=CARTESIAN_POINT('Ctrl Pts',(2.90681173597704,103.854552771039,14.4175227442231));
#68646=CARTESIAN_POINT('Ctrl Pts',(2.63264798485741,103.95385495439,15.1646348490477));
#68647=CARTESIAN_POINT('Ctrl Pts',(1.49083056653157,104.151063919667,16.4244092746339));
#68648=CARTESIAN_POINT('Ctrl Pts',(-1.05817372960175,104.448274315067,16.6201105460967));
#68649=CARTESIAN_POINT('Ctrl Pts',(-3.05249466751713,104.745106921702,15.0266860645816));
#68650=CARTESIAN_POINT('Ctrl Pts',(-3.42901662081578,105.043546951771,12.4890643696838));
#68651=CARTESIAN_POINT('Ctrl Pts',(-1.96751718769065,105.343083663407,10.3654093854579));
#68652=CARTESIAN_POINT('Ctrl Pts',(0.130224879799022,105.593176463126,9.90337622186573));
#68653=CARTESIAN_POINT('Ctrl Pts',(1.66609337331968,105.793269206908,10.4586464905891));
#68654=CARTESIAN_POINT('Ctrl Pts',(2.58745819416953,105.943284758349,11.2626524023438));
#68655=CARTESIAN_POINT('Ctrl Pts',(3.1477791609849,106.093175311736,12.349176213815));
#68656=CARTESIAN_POINT('Ctrl Pts',(3.30881198513969,106.281690758094,13.8782839209593));
#68657=CARTESIAN_POINT('Ctrl Pts',(2.52885555445624,106.508484576144,15.6360413544147));
#68658=CARTESIAN_POINT('Ctrl Pts',(0.552586543155371,106.772829197388,16.6810916807751));
#68659=CARTESIAN_POINT('Ctrl Pts',(-2.01179905013733,107.079459120307,16.2278473478844));
#68660=CARTESIAN_POINT('Ctrl Pts',(-3.68191758413864,107.426772062514,13.5565035374946));
#68661=CARTESIAN_POINT('Ctrl Pts',(-2.42805946625477,107.747949405601,10.9257775430486));
#68662=CARTESIAN_POINT('Ctrl Pts',(-0.46995553826754,108.001722082342,10.1586505583125));
#68663=CARTESIAN_POINT('Ctrl Pts',(1.07508180875167,108.190346887958,10.3385354236562));
#68664=CARTESIAN_POINT('Ctrl Pts',(2.33593740943957,108.377152545808,11.2353671016102));
#68665=CARTESIAN_POINT('Ctrl Pts',(2.8928771135283,108.53122080733,12.3796729815658));
#68666=CARTESIAN_POINT('Ctrl Pts',(2.97090758485472,108.653462194652,13.3640168289253));
#68667=CARTESIAN_POINT('Ctrl Pts',(2.80613213962208,108.775015492972,14.3320426466057));
#68668=CARTESIAN_POINT('Ctrl Pts',(2.28979959784192,108.895510736219,15.1834259478592));
#68669=CARTESIAN_POINT('Ctrl Pts',(1.52256885958377,109.014906219318,15.7681537405536));
#68670=CARTESIAN_POINT('Ctrl Pts',(0.971903944637074,109.089062781808,16.0028169166292));
#68671=CARTESIAN_POINT('Ctrl Pts',(0.508529708149316,109.148105042691,16.1043440298024));
#68672=CARTESIAN_POINT('Ctrl Pts',(0.0385556231530761,109.206954544851,
16.1465900629988));
#68673=CARTESIAN_POINT('Ctrl Pts',(-1.26134894552435,109.368002063753,16.0269418470898));
#68674=CARTESIAN_POINT('Ctrl Pts',(-2.42146781906107,109.540766094044,14.9954976241844));
#68675=CARTESIAN_POINT('Ctrl Pts',(-2.72256324956282,109.710470239931,13.6548996602733));
#68676=CARTESIAN_POINT('Ctrl Pts',(-2.70272022843698,109.822784912802,12.7494026467838));
#68677=CARTESIAN_POINT('Ctrl Pts',(-2.19786584670101,109.98014059768,11.5475342367803));
#68678=CARTESIAN_POINT('Ctrl Pts',(-0.787693309640737,110.180194811126,
10.6109538898846));
#68679=CARTESIAN_POINT('Ctrl Pts',(1.01870577211658,110.393928793874,10.7498948506012));
#68680=CARTESIAN_POINT('Ctrl Pts',(2.10419463547849,110.568274228434,11.7517884366777));
#68681=CARTESIAN_POINT('Ctrl Pts',(2.46316648785379,110.705500429676,12.8070638438925));
#68682=CARTESIAN_POINT('Ctrl Pts',(2.46375808236071,110.841235052451,13.9109031113142));
#68683=CARTESIAN_POINT('Ctrl Pts',(1.77979820499809,111.008121570367,15.1476579499127));
#68684=CARTESIAN_POINT('Ctrl Pts',(0.380213540866219,111.187691809938,15.7426116475981));
#68685=CARTESIAN_POINT('Ctrl Pts',(-0.923082425093289,111.347830969033,
15.503160237289));
#68686=CARTESIAN_POINT('Ctrl Pts',(-1.83584649687992,111.489617699394,14.768741531006));
#68687=CARTESIAN_POINT('Ctrl Pts',(-2.27775706335791,111.629132182632,13.7020687273194));
#68688=CARTESIAN_POINT('Ctrl Pts',(-2.17729566802582,111.743561512123,12.7616840700015));
#68689=CARTESIAN_POINT('Ctrl Pts',(-1.83989547207112,111.834049994605,12.1130192209344));
#68690=CARTESIAN_POINT('Ctrl Pts',(-1.47795183257781,111.901395372625,11.7069533144105));
#68691=CARTESIAN_POINT('Ctrl Pts',(-1.03001366334317,111.968239986844,11.4052174233104));
#68692=CARTESIAN_POINT('Ctrl Pts',(-0.609463651730633,112.023527612806,
11.2548334453014));
#68693=CARTESIAN_POINT('Ctrl Pts',(-0.260452763356783,112.067519905567,
11.199801986779));
#68694=CARTESIAN_POINT('Ctrl Pts',(0.0914627850391553,112.111354672102,
11.1885457737289));
#68695=CARTESIAN_POINT('Ctrl Pts',(0.5262964590746,112.165851041506,11.25685877975));
#68696=CARTESIAN_POINT('Ctrl Pts',(0.928356282889431,112.219973850279,11.4290887639811));
#68697=CARTESIAN_POINT('Ctrl Pts',(1.21506878098601,112.263049928539,11.622452038207));
#68698=CARTESIAN_POINT('Ctrl Pts',(1.8673642460961,112.37037650421,12.1870800767796));
#68699=CARTESIAN_POINT('Ctrl Pts',(2.32564333624236,112.550119454129,13.7487515890008));
#68700=CARTESIAN_POINT('Ctrl Pts',(0.857942820871301,112.798018163271,15.4593287880594));
#68701=CARTESIAN_POINT('Ctrl Pts',(-1.33588576058301,113.041155186133,15.1515921963496));
#68702=CARTESIAN_POINT('Ctrl Pts',(-2.14355161351861,113.254060359302,13.4006149978819));
#68703=CARTESIAN_POINT('Ctrl Pts',(-1.53367476616883,113.438784209471,11.9546519400679));
#68704=CARTESIAN_POINT('Ctrl Pts',(-0.369804341368539,113.596407856987,
11.3032888791665));
#68705=CARTESIAN_POINT('Ctrl Pts',(0.838022111309818,113.740581086973,11.4927043608578));
#68706=CARTESIAN_POINT('Ctrl Pts',(1.63927578177115,113.871676899798,12.2235980999995));
#68707=CARTESIAN_POINT('Ctrl Pts',(1.95948343014593,113.989837235801,13.1464677838519));
#68708=CARTESIAN_POINT('Ctrl Pts',(1.79717931737704,114.108329735318,14.1132911901071));
#68709=CARTESIAN_POINT('Ctrl Pts',(1.18918375849656,114.227310414659,14.8871680207432));
#68710=CARTESIAN_POINT('Ctrl Pts',(0.279975681687718,114.346930556551,15.2773039793232));
#68711=CARTESIAN_POINT('Ctrl Pts',(-0.712306032734786,114.467345568773,
15.1836650206917));
#68712=CARTESIAN_POINT('Ctrl Pts',(-1.40463281222753,114.568468484755,14.7149792157192));
#68713=CARTESIAN_POINT('Ctrl Pts',(-1.73026114226455,114.639733774504,14.23957264692));
#68714=CARTESIAN_POINT('Ctrl Pts',(-1.86164459924767,114.680598472528,13.9390965480409));
#68715=CARTESIAN_POINT('Ctrl Pts',(-2.09935034112274,114.783008522088,13.1499718822202));
#68716=CARTESIAN_POINT('Ctrl Pts',(-1.76503529547132,114.917638441435,11.9842552755218));
#68717=CARTESIAN_POINT('Ctrl Pts',(-0.567487175863522,115.086316822326,
11.2599496856478));
#68718=CARTESIAN_POINT('Ctrl Pts',(0.665519304553295,115.235790922527,11.1971637803623));
#68719=CARTESIAN_POINT('Ctrl Pts',(1.92016243365841,115.409510586213,12.0066278758882));
#68720=CARTESIAN_POINT('Ctrl Pts',(2.33861956090724,115.609211184837,13.6750014934849));
#68721=CARTESIAN_POINT('Ctrl Pts',(1.6301418363172,115.779470559898,14.9552947116152));
#68722=CARTESIAN_POINT('Ctrl Pts',(0.635494893866887,115.918122660083,15.4956801563099));
#68723=CARTESIAN_POINT('Ctrl Pts',(-0.499791186913486,116.058458118718,
15.643431048584));
#68724=CARTESIAN_POINT('Ctrl Pts',(-1.89423469946485,116.23707880032,15.0005349982472));
#68725=CARTESIAN_POINT('Ctrl Pts',(-2.60953214547825,116.456826834462,13.2493627101195));
#68726=CARTESIAN_POINT('Ctrl Pts',(-1.90299736565981,116.688139689368,11.3891119411448));
#68727=CARTESIAN_POINT('Ctrl Pts',(-0.637255827920347,116.848579631347,
10.8064219699136));
#68728=CARTESIAN_POINT('Ctrl Pts',(0.0392219119147239,116.932968917921,
10.7964020467747));
#68729=CARTESIAN_POINT('Ctrl Pts',(2.71505794088331,104.1994437308,14.3468610267603));
#68730=CARTESIAN_POINT('Ctrl Pts',(2.44854735935264,104.292313447051,15.0416272092801));
#68731=CARTESIAN_POINT('Ctrl Pts',(1.36756482302596,104.475801927177,16.1958735715385));
#68732=CARTESIAN_POINT('Ctrl Pts',(-0.983662767649807,104.749721435673,
16.3386992894006));
#68733=CARTESIAN_POINT('Ctrl Pts',(-2.78217366894562,105.020910301127,14.8550186522848));
#68734=CARTESIAN_POINT('Ctrl Pts',(-3.08800545020851,105.291383777472,12.5508031196169));
#68735=CARTESIAN_POINT('Ctrl Pts',(-1.74472357217229,105.56087112011,10.6608062718286));
#68736=CARTESIAN_POINT('Ctrl Pts',(0.135625608828576,105.784400237312,10.2757794639132));
#68737=CARTESIAN_POINT('Ctrl Pts',(1.49502657686255,105.962468409704,10.7887768814312));
#68738=CARTESIAN_POINT('Ctrl Pts',(2.30264041650804,106.095612653712,11.5134951068175));
#68739=CARTESIAN_POINT('Ctrl Pts',(2.78524563770895,106.228317938575,12.4819913514941));
#68740=CARTESIAN_POINT('Ctrl Pts',(2.90874630672134,106.394841463325,13.8343063389686));
#68741=CARTESIAN_POINT('Ctrl Pts',(2.20004500026988,106.594606461261,15.3723449650755));
#68742=CARTESIAN_POINT('Ctrl Pts',(0.451984644705152,106.826764135065,16.2654245396575));
#68743=CARTESIAN_POINT('Ctrl Pts',(-1.78882197927717,107.095458932795,15.8367470047943));
#68744=CARTESIAN_POINT('Ctrl Pts',(-3.21619776564414,107.399246079781,13.4802679274698));
#68745=CARTESIAN_POINT('Ctrl Pts',(-2.0882346499087,107.680042569535,11.1962729879085));
#68746=CARTESIAN_POINT('Ctrl Pts',(-0.365742139369948,107.902133889693,
10.549148540978));
#68747=CARTESIAN_POINT('Ctrl Pts',(0.985322022483406,108.067401390196,10.7259094226531));
#68748=CARTESIAN_POINT('Ctrl Pts',(2.08025913738351,108.231343450877,11.5284561491254));
#68749=CARTESIAN_POINT('Ctrl Pts',(2.5554633745237,108.366841980157,12.5415462205961));
#68750=CARTESIAN_POINT('Ctrl Pts',(2.61143887944914,108.474561818227,13.409667832991));
#68751=CARTESIAN_POINT('Ctrl Pts',(2.45344216292041,108.581827780697,14.2614262617206));
#68752=CARTESIAN_POINT('Ctrl Pts',(1.98585296195543,108.688410614965,15.0075574214225));
#68753=CARTESIAN_POINT('Ctrl Pts',(1.29777849423895,108.794308983379,15.5157261953399));
#68754=CARTESIAN_POINT('Ctrl Pts',(0.805428609191861,108.860210108581,15.7167319489964));
#68755=CARTESIAN_POINT('Ctrl Pts',(0.391781166622539,108.912760257788,15.8007187722551));
#68756=CARTESIAN_POINT('Ctrl Pts',(-0.0274075049062522,108.965196661223,
15.8318584187781));
#68757=CARTESIAN_POINT('Ctrl Pts',(-1.18527549088678,109.108927758844,15.7073432711166));
#68758=CARTESIAN_POINT('Ctrl Pts',(-2.21381540198591,109.264023600951,14.7672557840495));
#68759=CARTESIAN_POINT('Ctrl Pts',(-2.4666221194252,109.417455916768,13.5512181994124));
#68760=CARTESIAN_POINT('Ctrl Pts',(-2.43525232684139,109.519304698459,12.7307790999533));
#68761=CARTESIAN_POINT('Ctrl Pts',(-1.95826944884497,109.662664632789,11.6435908816576));
#68762=CARTESIAN_POINT('Ctrl Pts',(-0.650482528322692,109.846363248703,
10.8039310880342));
#68763=CARTESIAN_POINT('Ctrl Pts',(1.02182660581755,110.044567718633,10.9591201241675));
#68764=CARTESIAN_POINT('Ctrl Pts',(2.02377124064189,110.207984441163,11.9142507291509));
#68765=CARTESIAN_POINT('Ctrl Pts',(2.34515085280631,110.337721417545,12.9176288954705));
#68766=CARTESIAN_POINT('Ctrl Pts',(2.32669728841621,110.466814757994,13.9667344923216));
#68767=CARTESIAN_POINT('Ctrl Pts',(1.65024421515736,110.627010942262,15.1422811214735));
#68768=CARTESIAN_POINT('Ctrl Pts',(0.279841231730215,110.801635822459,15.6967579505581));
#68769=CARTESIAN_POINT('Ctrl Pts',(-0.997723993787982,110.959225644215,
15.437098270253));
#68770=CARTESIAN_POINT('Ctrl Pts',(-1.89073077452904,111.100228398427,14.689633673013));
#68771=CARTESIAN_POINT('Ctrl Pts',(-2.31361461167824,111.240471817201,13.6092790523088));
#68772=CARTESIAN_POINT('Ctrl Pts',(-2.19227242180266,111.356767594283,12.6561660152691));
#68773=CARTESIAN_POINT('Ctrl Pts',(-1.83243226651477,111.449499794301,11.9992928382035));
#68774=CARTESIAN_POINT('Ctrl Pts',(-1.45059332214956,111.518902314342,11.5892585743851));
#68775=CARTESIAN_POINT('Ctrl Pts',(-0.979851457299495,111.588174909696,
11.2869954931243));
#68776=CARTESIAN_POINT('Ctrl Pts',(-0.538407219059272,111.645794817927,
11.140130616902));
#68777=CARTESIAN_POINT('Ctrl Pts',(-0.172120535377108,111.691835651858,
11.0908611006565));
#68778=CARTESIAN_POINT('Ctrl Pts',(0.19719169622667,111.73784065953,11.0874665918825));
#68779=CARTESIAN_POINT('Ctrl Pts',(0.65349947446874,111.795278306845,11.1698210577316));
#68780=CARTESIAN_POINT('Ctrl Pts',(1.07509744453089,111.852641265216,11.3619597323698));
#68781=CARTESIAN_POINT('Ctrl Pts',(1.37521290996629,111.898488472078,11.5747499552319));
#68782=CARTESIAN_POINT('Ctrl Pts',(2.05657697613875,112.013038804026,12.1930111133316));
#68783=CARTESIAN_POINT('Ctrl Pts',(2.5198426174308,112.207309807241,13.8895055813126));
#68784=CARTESIAN_POINT('Ctrl Pts',(0.863358025389426,112.4810590135,15.7453375640381));
#68785=CARTESIAN_POINT('Ctrl Pts',(-1.60009927363686,112.754983055442,15.3477610936586));
#68786=CARTESIAN_POINT('Ctrl Pts',(-2.48158913313704,112.999225065672,13.3196393176612));
#68787=CARTESIAN_POINT('Ctrl Pts',(-1.73154951128389,113.213913880982,11.6578741429386));
#68788=CARTESIAN_POINT('Ctrl Pts',(-0.348206397242804,113.398792298062,
10.9293842108788));
#68789=CARTESIAN_POINT('Ctrl Pts',(1.07234040692998,113.569220429567,11.1898313111311));
#68790=CARTESIAN_POINT('Ctrl Pts',(2.00084073465665,113.725049090902,12.0830127970274));
#68791=CARTESIAN_POINT('Ctrl Pts',(2.35323487848361,113.866053623984,13.193307214017));
#68792=CARTESIAN_POINT('Ctrl Pts',(2.12830650217169,114.007886824867,14.3442064957623));
#68793=CARTESIAN_POINT('Ctrl Pts',(1.37491864048594,114.150614707706,15.2521168057112));
#68794=CARTESIAN_POINT('Ctrl Pts',(0.271426623166744,114.294299038404,15.6911251296496));
#68795=CARTESIAN_POINT('Ctrl Pts',(-0.916803365805068,114.439000041518,
15.5469928482248));
#68796=CARTESIAN_POINT('Ctrl Pts',(-1.73268742066223,114.560474348342,14.962515710009));
#68797=CARTESIAN_POINT('Ctrl Pts',(-2.10810420031903,114.645998554686,14.3822819218351));
#68798=CARTESIAN_POINT('Ctrl Pts',(-2.25611753397905,114.695011815457,14.0181352682096));
#68799=CARTESIAN_POINT('Ctrl Pts',(-2.51617452672619,114.817785799399,13.0655010803562));
#68800=CARTESIAN_POINT('Ctrl Pts',(-2.07923546760282,114.97881806575,11.6838635643743));
#68801=CARTESIAN_POINT('Ctrl Pts',(-0.633626624243302,115.17950681556,10.8596907877631));
#68802=CARTESIAN_POINT('Ctrl Pts',(0.827782894109682,115.356601837116,10.8224739007951));
#68803=CARTESIAN_POINT('Ctrl Pts',(2.27930210313871,115.561175716011,11.8129702385169));
#68804=CARTESIAN_POINT('Ctrl Pts',(2.71753295138253,115.794337474248,13.7715057220754));
#68805=CARTESIAN_POINT('Ctrl Pts',(1.86214478959958,115.991188085206,15.2298020769417));
#68806=CARTESIAN_POINT('Ctrl Pts',(0.708060464255386,116.150212355569,15.8225350252024));
#68807=CARTESIAN_POINT('Ctrl Pts',(-0.589859124811868,116.310255772754,
15.9613469133736));
#68808=CARTESIAN_POINT('Ctrl Pts',(-2.14762077271569,116.512258718969,15.1970536166379));
#68809=CARTESIAN_POINT('Ctrl Pts',(-2.90049964340585,116.757632216301,13.2238631994602));
#68810=CARTESIAN_POINT('Ctrl Pts',(-2.07350245045037,117.012892421133,11.1917174196688));
#68811=CARTESIAN_POINT('Ctrl Pts',(-0.685204826526019,117.187183007416,
10.5894830032886));
#68812=CARTESIAN_POINT('Ctrl Pts',(0.0464586395786999,117.278479420639,
10.5932235447126));
#68813=CARTESIAN_POINT('Ctrl Pts',(2.52330414578958,104.544334690561,14.2761993092975));
#68814=CARTESIAN_POINT('Ctrl Pts',(2.26444673384787,104.630771939713,14.9186195695124));
#68815=CARTESIAN_POINT('Ctrl Pts',(1.24429907952034,104.800539934689,15.9673378684431));
#68816=CARTESIAN_POINT('Ctrl Pts',(-0.909151805697865,105.051168556281,
16.0572880327045));
#68817=CARTESIAN_POINT('Ctrl Pts',(-2.51185267037412,105.296713680551,14.6833512399881));
#68818=CARTESIAN_POINT('Ctrl Pts',(-2.74699427960123,105.539220603172,12.61254186955));
#68819=CARTESIAN_POINT('Ctrl Pts',(-1.52192995665394,105.778658576813,10.9562031581992));
#68820=CARTESIAN_POINT('Ctrl Pts',(0.141026337858125,105.975624011497,10.6481827059608));
#68821=CARTESIAN_POINT('Ctrl Pts',(1.32395978040542,106.131667612499,11.1189072722733));
#68822=CARTESIAN_POINT('Ctrl Pts',(2.01782263884653,106.247940549075,11.7643378112914));
#68823=CARTESIAN_POINT('Ctrl Pts',(2.42271211443298,106.363460565413,12.6148064891733));
#68824=CARTESIAN_POINT('Ctrl Pts',(2.50868062830299,106.507992168557,13.7903287569779));
#68825=CARTESIAN_POINT('Ctrl Pts',(1.87123444608351,106.68072834638,15.1086485757361));
#68826=CARTESIAN_POINT('Ctrl Pts',(0.35138274625492,106.880699072743,15.8497573985399));
#68827=CARTESIAN_POINT('Ctrl Pts',(-1.56584490841702,107.111458745282,15.4456466617042));
#68828=CARTESIAN_POINT('Ctrl Pts',(-2.75047794714966,107.371720097048,13.4040323174451));
#68829=CARTESIAN_POINT('Ctrl Pts',(-1.74840983356265,107.61213573347,11.4667684327686));
#68830=CARTESIAN_POINT('Ctrl Pts',(-0.261528740472371,107.802545697043,
10.9396465236436));
#68831=CARTESIAN_POINT('Ctrl Pts',(0.895562236215122,107.944455892434,11.11328342165));
#68832=CARTESIAN_POINT('Ctrl Pts',(1.82458086532744,108.085534355947,11.8215451966406));
#68833=CARTESIAN_POINT('Ctrl Pts',(2.21804963551908,108.202463152983,12.7034194596264));
#68834=CARTESIAN_POINT('Ctrl Pts',(2.25197017404353,108.295661441802,13.4553188370568));
#68835=CARTESIAN_POINT('Ctrl Pts',(2.10075218621871,108.388640068422,14.1908098768355));
#68836=CARTESIAN_POINT('Ctrl Pts',(1.6819063260689,108.481310493711,14.8316888949858));
#68837=CARTESIAN_POINT('Ctrl Pts',(1.07298812889412,108.573711747439,15.263298650126));
#68838=CARTESIAN_POINT('Ctrl Pts',(0.638953273746623,108.631357435354,15.4306469813635));
#68839=CARTESIAN_POINT('Ctrl Pts',(0.275032625095737,108.677415472885,15.4970935147077));
#68840=CARTESIAN_POINT('Ctrl Pts',(-0.0933706329656045,108.723438777596,
15.5171267745574));
#68841=CARTESIAN_POINT('Ctrl Pts',(-1.10920203624921,108.849853453934,15.3877446951435));
#68842=CARTESIAN_POINT('Ctrl Pts',(-2.00616298491076,108.987281107858,14.5390139439145));
#68843=CARTESIAN_POINT('Ctrl Pts',(-2.21068098928759,109.124441593605,13.4475367385515));
#68844=CARTESIAN_POINT('Ctrl Pts',(-2.16778442524582,109.215824484117,12.7121555531227));
#68845=CARTESIAN_POINT('Ctrl Pts',(-1.71867305098895,109.345188667898,11.7396475265348));
#68846=CARTESIAN_POINT('Ctrl Pts',(-0.513271747004666,109.51253168628,10.9969082861839));
#68847=CARTESIAN_POINT('Ctrl Pts',(1.02494743951852,109.695206643391,11.1683453977339));
#68848=CARTESIAN_POINT('Ctrl Pts',(1.94334784580527,109.847694653892,12.0767130216241));
#68849=CARTESIAN_POINT('Ctrl Pts',(2.22713521775881,109.969942405414,13.0281939470486));
#68850=CARTESIAN_POINT('Ctrl Pts',(2.18963649447169,110.092394463537,14.022565873329));
#68851=CARTESIAN_POINT('Ctrl Pts',(1.52069022531662,110.245900314157,15.1369042930342));
#68852=CARTESIAN_POINT('Ctrl Pts',(0.179468922594197,110.41557983498,15.6509042535181));
#68853=CARTESIAN_POINT('Ctrl Pts',(-1.07236556248268,110.570620319398,15.371036303217));
#68854=CARTESIAN_POINT('Ctrl Pts',(-1.94561505217817,110.710839097462,14.6105258150201));
#68855=CARTESIAN_POINT('Ctrl Pts',(-2.34947215999859,110.851811451771,13.5164893772982));
#68856=CARTESIAN_POINT('Ctrl Pts',(-2.20724917557952,110.969973676442,12.5506479605367));
#68857=CARTESIAN_POINT('Ctrl Pts',(-1.82496906095844,111.064949593997,11.8855664554727));
#68858=CARTESIAN_POINT('Ctrl Pts',(-1.42323481172131,111.136409256059,11.4715638343598));
#68859=CARTESIAN_POINT('Ctrl Pts',(-0.929689251255833,111.208109832547,
11.1687735629382));
#68860=CARTESIAN_POINT('Ctrl Pts',(-0.467350786387917,111.268062023047,
11.0254277885027));
#68861=CARTESIAN_POINT('Ctrl Pts',(-0.0837883073974405,111.316151398149,
10.9819202145342));
#68862=CARTESIAN_POINT('Ctrl Pts',(0.302920607414179,111.364326646958,10.9863874100361));
#68863=CARTESIAN_POINT('Ctrl Pts',(0.780702489862876,111.424705572184,11.0827833357131));
#68864=CARTESIAN_POINT('Ctrl Pts',(1.22183860617235,111.485308680154,11.2948307007585));
#68865=CARTESIAN_POINT('Ctrl Pts',(1.53535703894656,111.533927015618,11.5270478722568));
#68866=CARTESIAN_POINT('Ctrl Pts',(2.24578970618141,111.655701103841,12.1989421498836));
#68867=CARTESIAN_POINT('Ctrl Pts',(2.71404189861924,111.864500160352,14.0302595736244));
#68868=CARTESIAN_POINT('Ctrl Pts',(0.868773229907559,112.164099863729,16.0313463400168));
#68869=CARTESIAN_POINT('Ctrl Pts',(-1.86431278669073,112.468810924751,15.5439299909674));
#68870=CARTESIAN_POINT('Ctrl Pts',(-2.81962665275547,112.744389772042,13.2386636374405));
#68871=CARTESIAN_POINT('Ctrl Pts',(-1.92942425639895,112.989043552493,11.3610963458093));
#68872=CARTESIAN_POINT('Ctrl Pts',(-0.32660845311707,113.201176739136,10.5554795425911));
#68873=CARTESIAN_POINT('Ctrl Pts',(1.30665870255015,113.397859772161,10.8869582614042));
#68874=CARTESIAN_POINT('Ctrl Pts',(2.36240568754215,113.578421282006,11.9424274940553));
#68875=CARTESIAN_POINT('Ctrl Pts',(2.74698632682127,113.742270012166,13.2401466441822));
#68876=CARTESIAN_POINT('Ctrl Pts',(2.45943368696635,113.907443914416,14.5751218014176));
#68877=CARTESIAN_POINT('Ctrl Pts',(1.56065352247533,114.073919000753,15.6170655906792));
#68878=CARTESIAN_POINT('Ctrl Pts',(0.262877564645767,114.241667520256,16.104946279976));
#68879=CARTESIAN_POINT('Ctrl Pts',(-1.12130069887536,114.410654514264,15.910320675758));
#68880=CARTESIAN_POINT('Ctrl Pts',(-2.06074202909693,114.552480211929,15.2100522042989));
#68881=CARTESIAN_POINT('Ctrl Pts',(-2.48594725837351,114.652263334868,14.5249911967502));
#68882=CARTESIAN_POINT('Ctrl Pts',(-2.65059046871045,114.709425158385,14.0971739883781));
#68883=CARTESIAN_POINT('Ctrl Pts',(-2.93299871232966,114.852563076709,12.9810302784921));
#68884=CARTESIAN_POINT('Ctrl Pts',(-2.39343563973433,115.039997690066,11.3834718532269));
#68885=CARTESIAN_POINT('Ctrl Pts',(-0.699766072623095,115.272696808793,
10.4594318898784));
#68886=CARTESIAN_POINT('Ctrl Pts',(0.990046483666062,115.477412751704,10.447784021228));
#68887=CARTESIAN_POINT('Ctrl Pts',(2.638441772619,115.712840845808,11.6193126011455));
#68888=CARTESIAN_POINT('Ctrl Pts',(3.09644634185781,115.979463763659,13.868009950666));
#68889=CARTESIAN_POINT('Ctrl Pts',(2.09414774288195,116.202905610514,15.5043094422683));
#68890=CARTESIAN_POINT('Ctrl Pts',(0.780626034643881,116.382302051056,16.1493898940948));
#68891=CARTESIAN_POINT('Ctrl Pts',(-0.679927062710262,116.56205342679,16.2792627781633));
#68892=CARTESIAN_POINT('Ctrl Pts',(-2.40100684596654,116.787438637619,15.3935722350285));
#68893=CARTESIAN_POINT('Ctrl Pts',(-3.19146714133348,117.058437598141,13.1983636888011));
#68894=CARTESIAN_POINT('Ctrl Pts',(-2.24400753524095,117.337645152896,10.994322898193));
#68895=CARTESIAN_POINT('Ctrl Pts',(-0.733153825131694,117.525786383484,
10.3725440366635));
#68896=CARTESIAN_POINT('Ctrl Pts',(0.0536953672426754,117.623989923356,
10.3900450426506));
#68897=CARTESIAN_POINT('Ctrl Pts',(2.33155035069585,104.889225650322,14.2055375918348));
#68898=CARTESIAN_POINT('Ctrl Pts',(2.08034610834311,104.969230432376,14.7956119297448));
#68899=CARTESIAN_POINT('Ctrl Pts',(1.12103333601473,105.125277942201,15.7388021653477));
#68900=CARTESIAN_POINT('Ctrl Pts',(-0.834640843745923,105.352615676887,
15.7758767760086));
#68901=CARTESIAN_POINT('Ctrl Pts',(-2.24153167180261,105.572517059975,14.5116838276913));
#68902=CARTESIAN_POINT('Ctrl Pts',(-2.40598310899397,105.787057428874,12.6742806194831));
#68903=CARTESIAN_POINT('Ctrl Pts',(-1.29913634113558,105.996446033516,11.2516000445698));
#68904=CARTESIAN_POINT('Ctrl Pts',(0.146427066887681,106.166847785682,11.0205859480082));
#68905=CARTESIAN_POINT('Ctrl Pts',(1.15289298394829,106.300866815296,11.4490376631154));
#68906=CARTESIAN_POINT('Ctrl Pts',(1.73300486118504,106.400268444437,12.0151805157652));
#68907=CARTESIAN_POINT('Ctrl Pts',(2.06017859115705,106.498603192252,12.7476216268525));
#68908=CARTESIAN_POINT('Ctrl Pts',(2.10861494988465,106.621142873788,13.7463511749871));
#68909=CARTESIAN_POINT('Ctrl Pts',(1.54242389189715,106.766850231498,14.8449521863969));
#68910=CARTESIAN_POINT('Ctrl Pts',(0.250780847804702,106.934634010421,15.4340902574224));
#68911=CARTESIAN_POINT('Ctrl Pts',(-1.34286783755684,107.127458557769,15.0545463186142));
#68912=CARTESIAN_POINT('Ctrl Pts',(-2.28475812865515,107.344194114315,13.3277967074203));
#68913=CARTESIAN_POINT('Ctrl Pts',(-1.40858501721658,107.544228897403,11.7372638776285));
#68914=CARTESIAN_POINT('Ctrl Pts',(-0.157315341574774,107.702957504394,
11.3301445063092));
#68915=CARTESIAN_POINT('Ctrl Pts',(0.805802449946862,107.821510394672,11.500657420647));
#68916=CARTESIAN_POINT('Ctrl Pts',(1.56890259327139,107.939725261016,12.1146342441558));
#68917=CARTESIAN_POINT('Ctrl Pts',(1.88063589651449,108.03808432581,12.8652926986567));
#68918=CARTESIAN_POINT('Ctrl Pts',(1.89250146863796,108.116761065377,13.5009698411227));
#68919=CARTESIAN_POINT('Ctrl Pts',(1.74806220951704,108.195452356148,14.1201934919506));
#68920=CARTESIAN_POINT('Ctrl Pts',(1.3779596901824,108.274210372457,14.6558203685491));
#68921=CARTESIAN_POINT('Ctrl Pts',(0.848197763549307,108.3531145115,15.0108711049122));
#68922=CARTESIAN_POINT('Ctrl Pts',(0.472477938301414,108.402504762127,15.1445620137306));
#68923=CARTESIAN_POINT('Ctrl Pts',(0.158284083568963,108.442070687982,15.1934682571603));
#68924=CARTESIAN_POINT('Ctrl Pts',(-0.159333761024929,108.481680893968,
15.2023951303368));
#68925=CARTESIAN_POINT('Ctrl Pts',(-1.03312858161163,108.590779149026,15.0681461191704));
#68926=CARTESIAN_POINT('Ctrl Pts',(-1.79851056783559,108.710538614764,14.3107721037796));
#68927=CARTESIAN_POINT('Ctrl Pts',(-1.95473985914995,108.831427270441,13.3438552776906));
#68928=CARTESIAN_POINT('Ctrl Pts',(-1.90031652365022,108.912344269774,12.6935320062921));
#68929=CARTESIAN_POINT('Ctrl Pts',(-1.47907665313292,109.027712703007,11.8357041714121));
#68930=CARTESIAN_POINT('Ctrl Pts',(-0.376060965686619,109.178700123857,
11.1898854843336));
#68931=CARTESIAN_POINT('Ctrl Pts',(1.0280682732195,109.345845568149,11.3775706713003));
#68932=CARTESIAN_POINT('Ctrl Pts',(1.86292445096866,109.487404866621,12.2391753140972));
#68933=CARTESIAN_POINT('Ctrl Pts',(2.10911958271135,109.602163393282,13.1387589986266));
#68934=CARTESIAN_POINT('Ctrl Pts',(2.05257570052719,109.71797416908,14.0783972543364));
#68935=CARTESIAN_POINT('Ctrl Pts',(1.39113623547589,109.864789686052,15.131527464595));
#68936=CARTESIAN_POINT('Ctrl Pts',(0.0790966134581977,110.029523847502,
15.6050505564782));
#68937=CARTESIAN_POINT('Ctrl Pts',(-1.14700713117737,110.18201499458,15.304974336181));
#68938=CARTESIAN_POINT('Ctrl Pts',(-2.00049932982729,110.321449796495,14.5314179570271));
#68939=CARTESIAN_POINT('Ctrl Pts',(-2.38532970831892,110.46315108634,13.4236997022875));
#68940=CARTESIAN_POINT('Ctrl Pts',(-2.22222592935636,110.583179758602,12.4451299058044));
#68941=CARTESIAN_POINT('Ctrl Pts',(-1.81750585540209,110.680399393693,11.7718400727418));
#68942=CARTESIAN_POINT('Ctrl Pts',(-1.39587630129307,110.753916197775,11.3538690943344));
#68943=CARTESIAN_POINT('Ctrl Pts',(-0.879527045212157,110.828044755399,
11.0505516327519));
#68944=CARTESIAN_POINT('Ctrl Pts',(-0.39629435371655,110.890329228167,10.9107249601033));
#68945=CARTESIAN_POINT('Ctrl Pts',(0.00454392058224056,110.94046714444,
10.8729793284117));
#68946=CARTESIAN_POINT('Ctrl Pts',(0.408649518601699,110.990812634386,10.8853082281896));
#68947=CARTESIAN_POINT('Ctrl Pts',(0.907905505257022,111.054132837524,10.9957456136948));
#68948=CARTESIAN_POINT('Ctrl Pts',(1.36857976781383,111.117976095091,11.2277016691471));
#68949=CARTESIAN_POINT('Ctrl Pts',(1.69550116792685,111.169365559157,11.4793457892818));
#68950=CARTESIAN_POINT('Ctrl Pts',(2.43500243622407,111.298363403658,12.2048731864356));
#68951=CARTESIAN_POINT('Ctrl Pts',(2.90824117980769,111.521690513464,14.1710135659361));
#68952=CARTESIAN_POINT('Ctrl Pts',(0.87418843442569,111.84714071396,16.3173551159956));
#68953=CARTESIAN_POINT('Ctrl Pts',(-2.12852629974458,112.18263879406,15.7400988882763));
#68954=CARTESIAN_POINT('Ctrl Pts',(-3.15766417237389,112.489554478412,13.1576879572197));
#68955=CARTESIAN_POINT('Ctrl Pts',(-2.12729900151401,112.764173224004,11.0643185486799));
#68956=CARTESIAN_POINT('Ctrl Pts',(-0.305010508991329,113.003561180212,
10.1815748743034));
#68957=CARTESIAN_POINT('Ctrl Pts',(1.54097699817032,113.226499114754,10.5840852116775));
#68958=CARTESIAN_POINT('Ctrl Pts',(2.72397064042765,113.431793473111,11.8018421910831));
#68959=CARTESIAN_POINT('Ctrl Pts',(3.14073777515895,113.618486400348,13.2869860743474));
#68960=CARTESIAN_POINT('Ctrl Pts',(2.79056087176101,113.807001003966,14.8060371070729));
#68961=CARTESIAN_POINT('Ctrl Pts',(1.74638840446472,113.9972232938,15.9820143756473));
#68962=CARTESIAN_POINT('Ctrl Pts',(0.254328506124801,114.189036002109,16.5187674303024));
#68963=CARTESIAN_POINT('Ctrl Pts',(-1.32579803194563,114.382308987009,16.2736485032911));
#68964=CARTESIAN_POINT('Ctrl Pts',(-2.38879663753162,114.544486075516,15.4575886985887));
#68965=CARTESIAN_POINT('Ctrl Pts',(-2.86379031642799,114.658528115049,14.6677004716653));
#68966=CARTESIAN_POINT('Ctrl Pts',(-3.04506340344182,114.723838501314,14.1762127085468));
#68967=CARTESIAN_POINT('Ctrl Pts',(-3.34982289793312,114.88734035402,12.8965594766281));
#68968=CARTESIAN_POINT('Ctrl Pts',(-2.70763581186582,115.101177314382,11.0830801420794));
#68969=CARTESIAN_POINT('Ctrl Pts',(-0.765905521002873,115.365886802026,
10.0591729919936));
#68970=CARTESIAN_POINT('Ctrl Pts',(1.15231007322245,115.598223666293,10.0730941416609));
#68971=CARTESIAN_POINT('Ctrl Pts',(2.9975814420993,115.864505975606,11.4256549637742));
#68972=CARTESIAN_POINT('Ctrl Pts',(3.4753597323331,116.164590053071,13.9645141792565));
#68973=CARTESIAN_POINT('Ctrl Pts',(2.32615069616434,116.414623135822,15.7788168075948));
#68974=CARTESIAN_POINT('Ctrl Pts',(0.853191605032384,116.614391746542,16.4762447629873));
#68975=CARTESIAN_POINT('Ctrl Pts',(-0.769995000608643,116.813851080826,
16.5971786429528));
#68976=CARTESIAN_POINT('Ctrl Pts',(-2.65439291921737,117.062618556269,15.5900908534192));
#68977=CARTESIAN_POINT('Ctrl Pts',(-3.4824346392611,117.359242979981,13.1728641781418));
#68978=CARTESIAN_POINT('Ctrl Pts',(-2.41451262003151,117.662397884661,10.796928376717));
#68979=CARTESIAN_POINT('Ctrl Pts',(-0.781102823737367,117.864389759553,
10.1556050700385));
#68980=CARTESIAN_POINT('Ctrl Pts',(0.0609320949066517,117.969500426075,
10.1868665405886));
#68981=CARTESIAN_POINT('Origin',(2.375,22.1,13.3));
#68982=CARTESIAN_POINT('Origin',(1.7,145.,13.3));
#68983=CARTESIAN_POINT('',(-1.7,145.,13.3));
#68984=CARTESIAN_POINT('Origin',(0.,145.,13.3));
#68985=CARTESIAN_POINT('Origin',(0.,144.85,13.3));
#68986=CARTESIAN_POINT('',(-2.,144.7,13.3));
#68987=CARTESIAN_POINT('Origin',(0.,144.7,13.3));
#68988=CARTESIAN_POINT('',(-1.85,144.85,13.3));
#68989=CARTESIAN_POINT('Origin',(0.,132.35,13.3));
#68990=CARTESIAN_POINT('',(-2.,120.,13.3));
#68991=CARTESIAN_POINT('Origin',(0.,120.,13.3));
#68992=CARTESIAN_POINT('',(-2.,132.35,13.3));
#68993=CARTESIAN_POINT('Origin',(2.5,120.,13.3));
#68994=CARTESIAN_POINT('Origin',(0.,20.25,13.3));
#68995=CARTESIAN_POINT('',(-2.2,20.1,13.3));
#68996=CARTESIAN_POINT('',(-2.35,20.25,13.3));
#68997=CARTESIAN_POINT('Origin',(0.,20.1,13.3));
#68998=CARTESIAN_POINT('Origin',(2.,20.1,13.3));
#68999=CARTESIAN_POINT('',(-2.,20.1,13.3));
#69000=CARTESIAN_POINT('Origin',(0.,20.1,13.3));
#69001=CARTESIAN_POINT('Origin',(0.,15.45,13.3));
#69002=CARTESIAN_POINT('',(-2.,10.8,13.3));
#69003=CARTESIAN_POINT('Origin',(0.,10.8,13.3));
#69004=CARTESIAN_POINT('',(-2.,15.45,13.3));
#69005=CARTESIAN_POINT('Origin',(0.,10.65,13.3));
#69006=CARTESIAN_POINT('',(-1.7,10.5,13.3));
#69007=CARTESIAN_POINT('',(-1.85,10.65,13.3));
#69008=CARTESIAN_POINT('Origin',(0.,10.5,13.3));
#69009=CARTESIAN_POINT('Origin',(0.,10.5,13.3));
#69010=CARTESIAN_POINT('',(0.,0.,0.));
#69011=CARTESIAN_POINT('Origin',(8.,139.,13.3));
#69012=CARTESIAN_POINT('',(7.37215620887551,138.292054261923,14.6788810071715));
#69013=CARTESIAN_POINT('',(7.33808558140337,139.,14.85));
#69014=CARTESIAN_POINT('Ctrl Pts',(7.37215620887549,138.292054261923,14.6788810071716));
#69015=CARTESIAN_POINT('Ctrl Pts',(7.36858316305761,138.329261989146,14.697984216059));
#69016=CARTESIAN_POINT('Ctrl Pts',(7.36520732362226,138.367331819182,14.7156231689265));
#69017=CARTESIAN_POINT('Ctrl Pts',(7.3466854762311,138.596916234109,14.8108668747228));
#69018=CARTESIAN_POINT('Ctrl Pts',(7.33808558140337,138.804765733125,14.85));
#69019=CARTESIAN_POINT('Ctrl Pts',(7.33808558140337,139.,14.85));
#69020=CARTESIAN_POINT('',(6.96320280119572,137.910875006907,14.4028629785336));
#69021=CARTESIAN_POINT('Origin',(5.32918064872639,139.,13.3));
#69022=CARTESIAN_POINT('',(7.43743486603367,137.788415340765,14.2667277866632));
#69023=CARTESIAN_POINT('Origin',(10.8050674972932,139.,13.3));
#69024=CARTESIAN_POINT('',(7.4970972452634,137.464107065927,13.5086453811229));
#69025=CARTESIAN_POINT('Ctrl Pts',(7.4970972452634,137.464107065927,13.5086453811229));
#69026=CARTESIAN_POINT('Ctrl Pts',(7.49347284068085,137.481798737663,13.6388783796458));
#69027=CARTESIAN_POINT('Ctrl Pts',(7.48629498464008,137.516874519344,13.7699539370805));
#69028=CARTESIAN_POINT('Ctrl Pts',(7.46572064431159,137.624316026987,14.0289417164261));
#69029=CARTESIAN_POINT('Ctrl Pts',(7.45185181981712,137.699915413076,14.1558122257263));
#69030=CARTESIAN_POINT('Ctrl Pts',(7.43743486603368,137.788415340765,14.2667277866631));
#69031=CARTESIAN_POINT('',(7.05,137.45,13.3));
#69032=CARTESIAN_POINT('Origin',(7.05,139.,13.3));
#69033=CARTESIAN_POINT('',(7.4970972452634,137.464107065927,13.0913546188771));
#69034=CARTESIAN_POINT('Origin',(7.05,139.,13.3));
#69035=CARTESIAN_POINT('',(7.43743486603367,137.788415340765,12.3332722133368));
#69036=CARTESIAN_POINT('Ctrl Pts',(7.43743486603368,137.788415340765,12.3332722133368));
#69037=CARTESIAN_POINT('Ctrl Pts',(7.45185181981712,137.699915413076,12.4441877742737));
#69038=CARTESIAN_POINT('Ctrl Pts',(7.46572064431159,137.624316026987,12.5710582835739));
#69039=CARTESIAN_POINT('Ctrl Pts',(7.48629498464007,137.516874519344,12.8300460629195));
#69040=CARTESIAN_POINT('Ctrl Pts',(7.49347284068085,137.481798737663,12.9611216203542));
#69041=CARTESIAN_POINT('Ctrl Pts',(7.4970972452634,137.464107065927,13.0913546188771));
#69042=CARTESIAN_POINT('',(6.96320280119572,137.910875006907,12.1971370214664));
#69043=CARTESIAN_POINT('Origin',(10.8050674972932,139.,13.3));
#69044=CARTESIAN_POINT('',(7.37215620887551,138.292054261923,11.9211189928285));
#69045=CARTESIAN_POINT('Origin',(5.32918064872639,139.,13.3));
#69046=CARTESIAN_POINT('',(7.37215620887551,139.707945738077,11.9211189928285));
#69047=CARTESIAN_POINT('Ctrl Pts',(7.37215620887549,139.707945738077,11.9211189928284));
#69048=CARTESIAN_POINT('Ctrl Pts',(7.36858316305761,139.670738010854,11.902015783941));
#69049=CARTESIAN_POINT('Ctrl Pts',(7.36520732362226,139.632668180818,11.8843768310735));
#69050=CARTESIAN_POINT('Ctrl Pts',(7.3466854762311,139.403083765891,11.7891331252772));
#69051=CARTESIAN_POINT('Ctrl Pts',(7.33808558140337,139.195234266875,11.75));
#69052=CARTESIAN_POINT('Ctrl Pts',(7.33808558140337,139.,11.75));
#69053=CARTESIAN_POINT('Ctrl Pts',(7.33808558140337,138.804765733125,11.75));
#69054=CARTESIAN_POINT('Ctrl Pts',(7.3466854762311,138.596916234109,11.7891331252772));
#69055=CARTESIAN_POINT('Ctrl Pts',(7.36520732362226,138.367331819182,11.8843768310735));
#69056=CARTESIAN_POINT('Ctrl Pts',(7.36858316305761,138.329261989146,11.902015783941));
#69057=CARTESIAN_POINT('Ctrl Pts',(7.37215620887549,138.292054261923,11.9211189928284));
#69058=CARTESIAN_POINT('',(6.96320280119572,140.089124993093,12.1971370214664));
#69059=CARTESIAN_POINT('Origin',(5.32918064872639,139.,13.3));
#69060=CARTESIAN_POINT('',(7.43743486603367,140.211584659235,12.3332722133368));
#69061=CARTESIAN_POINT('Origin',(10.8050674972932,139.,13.3));
#69062=CARTESIAN_POINT('',(7.4970972452634,140.535892934073,13.0913546188771));
#69063=CARTESIAN_POINT('Ctrl Pts',(7.4970972452634,140.535892934073,13.0913546188771));
#69064=CARTESIAN_POINT('Ctrl Pts',(7.49347284068085,140.518201262337,12.9611216203542));
#69065=CARTESIAN_POINT('Ctrl Pts',(7.48629498464008,140.483125480656,12.8300460629195));
#69066=CARTESIAN_POINT('Ctrl Pts',(7.46572064431159,140.375683973014,12.5710582835739));
#69067=CARTESIAN_POINT('Ctrl Pts',(7.45185181981713,140.300084586924,12.4441877742737));
#69068=CARTESIAN_POINT('Ctrl Pts',(7.43743486603368,140.211584659235,12.3332722133369));
#69069=CARTESIAN_POINT('',(7.05,140.55,13.3));
#69070=CARTESIAN_POINT('Origin',(7.05,139.,13.3));
#69071=CARTESIAN_POINT('',(7.4970972452634,140.535892934073,13.5086453811229));
#69072=CARTESIAN_POINT('Origin',(7.05,139.,13.3));
#69073=CARTESIAN_POINT('',(7.43743486603367,140.211584659235,14.2667277866632));
#69074=CARTESIAN_POINT('Ctrl Pts',(7.43743486603368,140.211584659235,14.2667277866631));
#69075=CARTESIAN_POINT('Ctrl Pts',(7.45185181981713,140.300084586924,14.1558122257262));
#69076=CARTESIAN_POINT('Ctrl Pts',(7.46572064431159,140.375683973013,14.0289417164261));
#69077=CARTESIAN_POINT('Ctrl Pts',(7.48629498464008,140.483125480656,13.7699539370805));
#69078=CARTESIAN_POINT('Ctrl Pts',(7.49347284068085,140.518201262337,13.6388783796458));
#69079=CARTESIAN_POINT('Ctrl Pts',(7.4970972452634,140.535892934073,13.5086453811229));
#69080=CARTESIAN_POINT('',(6.96320280119572,140.089124993093,14.4028629785336));
#69081=CARTESIAN_POINT('Origin',(10.8050674972932,139.,13.3));
#69082=CARTESIAN_POINT('',(7.37215620887551,139.707945738077,14.6788810071715));
#69083=CARTESIAN_POINT('Origin',(5.32918064872639,139.,13.3));
#69084=CARTESIAN_POINT('Ctrl Pts',(7.33808558140337,139.,14.85));
#69085=CARTESIAN_POINT('Ctrl Pts',(7.33808558140337,139.195234266875,14.85));
#69086=CARTESIAN_POINT('Ctrl Pts',(7.3466854762311,139.403083765891,14.8108668747228));
#69087=CARTESIAN_POINT('Ctrl Pts',(7.36520732362226,139.632668180818,14.7156231689265));
#69088=CARTESIAN_POINT('Ctrl Pts',(7.36858316305761,139.670738010854,14.697984216059));
#69089=CARTESIAN_POINT('Ctrl Pts',(7.37215620887549,139.707945738077,14.6788810071716));
#69090=CARTESIAN_POINT('',(1.27968746184371,139.,14.85));
#69091=CARTESIAN_POINT('',(8.,139.,14.85));
#69092=CARTESIAN_POINT('',(1.27968746184371,139.,11.75));
#69093=CARTESIAN_POINT('Ctrl Pts',(1.27968746184371,139.,11.75));
#69094=CARTESIAN_POINT('Ctrl Pts',(1.27968746184371,139.104803598436,11.75));
#69095=CARTESIAN_POINT('Ctrl Pts',(1.29297627000471,139.209518837456,11.7607265104896));
#69096=CARTESIAN_POINT('Ctrl Pts',(1.34103210887612,139.413055498266,11.8024328148038));
#69097=CARTESIAN_POINT('Ctrl Pts',(1.37566593328622,139.511905723271,11.8334254159452));
#69098=CARTESIAN_POINT('Ctrl Pts',(1.49608242611994,139.793364432057,11.9529188207752));
#69099=CARTESIAN_POINT('Ctrl Pts',(1.59729725054086,139.961362416936,12.0693313952581));
#69100=CARTESIAN_POINT('Ctrl Pts',(1.7703084453967,140.227330013039,12.3352989913604));
#69101=CARTESIAN_POINT('Ctrl Pts',(1.85621230875305,140.345671919208,12.5035840227375));
#69102=CARTESIAN_POINT('Ctrl Pts',(1.97644875243109,140.507202212245,12.8835230759381));
#69103=CARTESIAN_POINT('Ctrl Pts',(2.01,140.55,13.0955898084708));
#69104=CARTESIAN_POINT('Ctrl Pts',(2.01,140.55,13.5044101915292));
#69105=CARTESIAN_POINT('Ctrl Pts',(1.97644875243109,140.507202212245,13.7164769240619));
#69106=CARTESIAN_POINT('Ctrl Pts',(1.85621230875305,140.345671919208,14.0964159772625));
#69107=CARTESIAN_POINT('Ctrl Pts',(1.7703084453967,140.227330013039,14.2647010086396));
#69108=CARTESIAN_POINT('Ctrl Pts',(1.59729725054085,139.961362416936,14.5306686047419));
#69109=CARTESIAN_POINT('Ctrl Pts',(1.49608242611994,139.793364432057,14.6470811792249));
#69110=CARTESIAN_POINT('Ctrl Pts',(1.37566593328622,139.511905723271,14.7665745840548));
#69111=CARTESIAN_POINT('Ctrl Pts',(1.34103210887612,139.413055498266,14.7975671851962));
#69112=CARTESIAN_POINT('Ctrl Pts',(1.29297627000471,139.209518837456,14.8392734895104));
#69113=CARTESIAN_POINT('Ctrl Pts',(1.27968746184371,139.104803598436,14.85));
#69114=CARTESIAN_POINT('Ctrl Pts',(1.27968746184371,139.,14.85));
#69115=CARTESIAN_POINT('Ctrl Pts',(1.27968746184371,139.,14.85));
#69116=CARTESIAN_POINT('Ctrl Pts',(1.27968746184371,138.895196401564,14.85));
#69117=CARTESIAN_POINT('Ctrl Pts',(1.29297627000471,138.790481162544,14.8392734895104));
#69118=CARTESIAN_POINT('Ctrl Pts',(1.34103210887612,138.586944501734,14.7975671851962));
#69119=CARTESIAN_POINT('Ctrl Pts',(1.37566593328622,138.488094276729,14.7665745840548));
#69120=CARTESIAN_POINT('Ctrl Pts',(1.49608242611994,138.206635567943,14.6470811792249));
#69121=CARTESIAN_POINT('Ctrl Pts',(1.59729725054086,138.038637583064,14.5306686047419));
#69122=CARTESIAN_POINT('Ctrl Pts',(1.7703084453967,137.772669986961,14.2647010086396));
#69123=CARTESIAN_POINT('Ctrl Pts',(1.85621230875305,137.654328080792,14.0964159772625));
#69124=CARTESIAN_POINT('Ctrl Pts',(1.97644875243109,137.492797787755,13.7164769240619));
#69125=CARTESIAN_POINT('Ctrl Pts',(2.01,137.45,13.5044101915292));
#69126=CARTESIAN_POINT('Ctrl Pts',(2.01,137.45,13.0955898084708));
#69127=CARTESIAN_POINT('Ctrl Pts',(1.97644875243109,137.492797787755,12.8835230759381));
#69128=CARTESIAN_POINT('Ctrl Pts',(1.85621230875305,137.654328080792,12.5035840227375));
#69129=CARTESIAN_POINT('Ctrl Pts',(1.7703084453967,137.772669986961,12.3352989913604));
#69130=CARTESIAN_POINT('Ctrl Pts',(1.59729725054086,138.038637583064,12.0693313952581));
#69131=CARTESIAN_POINT('Ctrl Pts',(1.49608242611994,138.206635567943,11.9529188207752));
#69132=CARTESIAN_POINT('Ctrl Pts',(1.37566593328622,138.488094276729,11.8334254159452));
#69133=CARTESIAN_POINT('Ctrl Pts',(1.34103210887612,138.586944501734,11.8024328148038));
#69134=CARTESIAN_POINT('Ctrl Pts',(1.29297627000471,138.790481162544,11.7607265104896));
#69135=CARTESIAN_POINT('Ctrl Pts',(1.27968746184371,138.895196401564,11.75));
#69136=CARTESIAN_POINT('Ctrl Pts',(1.27968746184371,139.,11.75));
#69137=CARTESIAN_POINT('Origin',(6.96320280119572,133.2,14.4028629785336));
#69138=CARTESIAN_POINT('',(7.37215620887551,133.2,14.6788810071715));
#69139=CARTESIAN_POINT('',(7.37215620887551,138.6,14.6788810071715));
#69140=CARTESIAN_POINT('',(6.96320280119572,133.2,14.4028629785336));
#69141=CARTESIAN_POINT('',(7.64921699387799,133.2,14.8658797465221));
#69142=CARTESIAN_POINT('',(6.96320280119572,133.2,14.4028629785336));
#69143=CARTESIAN_POINT('Origin',(7.75872111940616,133.2,14.1744979081055));
#69144=CARTESIAN_POINT('',(7.43743486603367,133.2,14.2667277866632));
#69145=CARTESIAN_POINT('',(6.96320280119572,133.2,14.4028629785336));
#69146=CARTESIAN_POINT('',(7.43743486603367,138.6,14.2667277866632));
#69147=CARTESIAN_POINT('Origin',(7.64921699387799,133.2,11.7341202534779));
#69148=CARTESIAN_POINT('',(6.96320280119572,133.2,12.1971370214664));
#69149=CARTESIAN_POINT('',(6.96320280119572,133.2,12.1971370214664));
#69150=CARTESIAN_POINT('',(7.37215620887551,133.2,11.9211189928285));
#69151=CARTESIAN_POINT('',(6.96320280119572,133.2,12.1971370214664));
#69152=CARTESIAN_POINT('',(7.37215620887551,138.6,11.9211189928285));
#69153=CARTESIAN_POINT('Origin',(7.64921699387799,133.2,11.7341202534779));
#69154=CARTESIAN_POINT('',(7.37215620887551,144.,11.9211189928285));
#69155=CARTESIAN_POINT('',(7.37215620887551,138.6,11.9211189928285));
#69156=CARTESIAN_POINT('',(6.96320280119572,144.,12.1971370214664));
#69157=CARTESIAN_POINT('',(6.96320280119572,144.,12.1971370214664));
#69158=CARTESIAN_POINT('',(6.96320280119572,133.2,12.1971370214664));
#69159=CARTESIAN_POINT('Origin',(6.96320280119572,133.2,12.1971370214664));
#69160=CARTESIAN_POINT('',(7.43743486603367,133.2,12.3332722133368));
#69161=CARTESIAN_POINT('',(7.43743486603367,138.6,12.3332722133368));
#69162=CARTESIAN_POINT('',(7.75872111940616,133.2,12.4255020918945));
#69163=CARTESIAN_POINT('Origin',(6.96320280119572,133.2,12.1971370214664));
#69164=CARTESIAN_POINT('',(7.43743486603367,144.,12.3332722133368));
#69165=CARTESIAN_POINT('',(7.75872111940616,144.,12.4255020918945));
#69166=CARTESIAN_POINT('',(7.43743486603367,138.6,12.3332722133368));
#69167=CARTESIAN_POINT('Origin',(7.05,133.2,13.3));
#69168=CARTESIAN_POINT('',(7.4970972452634,133.2,13.5086453811229));
#69169=CARTESIAN_POINT('',(7.4970972452634,138.6,13.5086453811229));
#69170=CARTESIAN_POINT('',(7.05,133.2,13.3));
#69171=CARTESIAN_POINT('',(7.8,133.2,13.65));
#69172=CARTESIAN_POINT('',(7.05,133.2,13.3));
#69173=CARTESIAN_POINT('Origin',(7.05,133.2,13.3));
#69174=CARTESIAN_POINT('',(7.05,144.,13.3));
#69175=CARTESIAN_POINT('',(7.05,133.2,13.3));
#69176=CARTESIAN_POINT('',(7.4970972452634,144.,13.5086453811229));
#69177=CARTESIAN_POINT('',(7.8,144.,13.65));
#69178=CARTESIAN_POINT('',(7.4970972452634,138.6,13.5086453811229));
#69179=CARTESIAN_POINT('Origin',(7.8,133.2,12.95));
#69180=CARTESIAN_POINT('',(7.4970972452634,133.2,13.0913546188771));
#69181=CARTESIAN_POINT('',(7.05,133.2,13.3));
#69182=CARTESIAN_POINT('',(7.4970972452634,138.6,13.0913546188771));
#69183=CARTESIAN_POINT('Origin',(7.8,133.2,12.95));
#69184=CARTESIAN_POINT('',(7.4970972452634,144.,13.0913546188771));
#69185=CARTESIAN_POINT('',(7.4970972452634,138.6,13.0913546188771));
#69186=CARTESIAN_POINT('',(7.05,144.,13.3));
#69187=CARTESIAN_POINT('Origin',(7.3335859289189,133.2,12.1384740970763));
#69188=CARTESIAN_POINT('Origin',(0.,133.2,13.3));
#69189=CARTESIAN_POINT('Origin',(7.3335859289189,144.,12.1384740970763));
#69190=CARTESIAN_POINT('Origin',(0.,144.,13.3));
#69191=CARTESIAN_POINT('Origin',(7.31008487907097,133.2,10.5567976631721));
#69192=CARTESIAN_POINT('',(7.06568821984138,144.,10.7848359934202));
#69193=CARTESIAN_POINT('',(7.06568821984138,133.2,10.7848359934202));
#69194=CARTESIAN_POINT('',(7.06568821984138,138.6,10.7848359934202));
#69195=CARTESIAN_POINT('',(6.70494843988083,144.,11.1214301896566));
#69196=CARTESIAN_POINT('',(6.70494843988083,144.,11.1214301896566));
#69197=CARTESIAN_POINT('',(6.70494843988083,133.2,11.1214301896566));
#69198=CARTESIAN_POINT('',(6.70494843988083,133.2,11.1214301896566));
#69199=CARTESIAN_POINT('',(6.70494843988083,133.2,11.1214301896566));
#69200=CARTESIAN_POINT('Origin',(7.06159463349152,133.2,11.005548816766));
#69201=CARTESIAN_POINT('',(7.19463815697102,133.2,11.1817030920438));
#69202=CARTESIAN_POINT('Origin',(0.,133.2,13.3));
#69203=CARTESIAN_POINT('',(7.52639677513343,133.2,11.2225372245787));
#69204=CARTESIAN_POINT('Origin',(6.70494843988083,133.2,11.1214301896566));
#69205=CARTESIAN_POINT('',(7.19463815697102,144.,11.1817030920438));
#69206=CARTESIAN_POINT('',(7.19463815697102,138.6,11.1817030920438));
#69207=CARTESIAN_POINT('',(7.52639677513343,144.,11.2225372245787));
#69208=CARTESIAN_POINT('Origin',(7.06159463349152,144.,11.005548816766));
#69209=CARTESIAN_POINT('Origin',(0.,144.,13.3));
#69210=CARTESIAN_POINT('Origin',(6.79095421376043,133.2,9.44702181856561));
#69211=CARTESIAN_POINT('',(6.58523953715999,144.,9.7104846792046));
#69212=CARTESIAN_POINT('',(6.58523953715999,133.2,9.7104846792046));
#69213=CARTESIAN_POINT('',(6.58523953715999,138.6,9.7104846792046));
#69214=CARTESIAN_POINT('',(6.28159599552799,144.,10.0993669768362));
#69215=CARTESIAN_POINT('',(6.28159599552799,144.,10.0993669768362));
#69216=CARTESIAN_POINT('',(6.28159599552799,133.2,10.0993669768362));
#69217=CARTESIAN_POINT('',(6.28159599552799,133.2,10.0993669768362));
#69218=CARTESIAN_POINT('',(6.28159599552799,133.2,10.0993669768362));
#69219=CARTESIAN_POINT('Origin',(6.61572344209863,133.2,9.92912053943386));
#69220=CARTESIAN_POINT('',(6.77468557884867,133.2,10.0822934708492));
#69221=CARTESIAN_POINT('Origin',(0.,133.2,13.3));
#69222=CARTESIAN_POINT('',(7.10874756357811,133.2,10.0707263854975));
#69223=CARTESIAN_POINT('Origin',(6.28159599552799,133.2,10.0993669768362));
#69224=CARTESIAN_POINT('',(6.77468557884867,144.,10.0822934708492));
#69225=CARTESIAN_POINT('',(6.77468557884867,138.6,10.0822934708492));
#69226=CARTESIAN_POINT('',(7.10874756357811,144.,10.0707263854975));
#69227=CARTESIAN_POINT('Origin',(6.61572344209863,144.,9.92912053943386));
#69228=CARTESIAN_POINT('Origin',(0.,144.,13.3));
#69229=CARTESIAN_POINT('Origin',(6.10460771782222,133.2,8.43211908408747));
#69230=CARTESIAN_POINT('',(5.9426404019167,144.,8.72451914510537));
#69231=CARTESIAN_POINT('',(5.9426404019167,133.2,8.72451914510537));
#69232=CARTESIAN_POINT('',(5.9426404019167,138.6,8.72451914510537));
#69233=CARTESIAN_POINT('',(5.70356981034338,144.,9.15611397133807));
#69234=CARTESIAN_POINT('',(5.70356981034338,144.,9.15611397133807));
#69235=CARTESIAN_POINT('',(5.70356981034338,133.2,9.15611397133807));
#69236=CARTESIAN_POINT('',(5.70356981034338,133.2,9.15611397133807));
#69237=CARTESIAN_POINT('',(5.70356981034338,133.2,9.15611397133807));
#69238=CARTESIAN_POINT('Origin',(6.00695118323399,133.2,8.93569450172839));
#69239=CARTESIAN_POINT('',(6.18791775788269,133.2,9.06211446335793));
#69240=CARTESIAN_POINT('Origin',(0.,133.2,13.3));
#69241=CARTESIAN_POINT('',(6.51605739442695,133.2,8.99843098014994));
#69242=CARTESIAN_POINT('Origin',(5.70356981034338,133.2,9.15611397133807));
#69243=CARTESIAN_POINT('',(6.18791775788269,144.,9.06211446335793));
#69244=CARTESIAN_POINT('',(6.18791775788269,138.6,9.06211446335793));
#69245=CARTESIAN_POINT('',(6.51605739442695,144.,8.99843098014994));
#69246=CARTESIAN_POINT('Origin',(6.00695118323399,144.,8.93569450172839));
#69247=CARTESIAN_POINT('Origin',(0.,144.,13.3));
#69248=CARTESIAN_POINT('Origin',(5.26794551983978,133.2,7.53707973332964));
#69249=CARTESIAN_POINT('',(5.15371373748547,144.,7.851217134804));
#69250=CARTESIAN_POINT('',(5.15371373748547,133.2,7.851217134804));
#69251=CARTESIAN_POINT('',(5.15371373748547,138.6,7.851217134804));
#69252=CARTESIAN_POINT('',(4.98510280736516,144.,8.31489719263484));
#69253=CARTESIAN_POINT('',(4.98510280736516,144.,8.31489719263484));
#69254=CARTESIAN_POINT('',(4.98510280736516,133.2,8.31489719263484));
#69255=CARTESIAN_POINT('',(4.98510280736516,133.2,8.31489719263484));
#69256=CARTESIAN_POINT('',(4.98510280736516,133.2,8.31489719263484));
#69257=CARTESIAN_POINT('Origin',(5.25026785031011,133.2,8.04973214968988));
#69258=CARTESIAN_POINT('',(5.448782865196,133.2,8.14628626251453));
#69259=CARTESIAN_POINT('Origin',(0.,133.2,13.3));
#69260=CARTESIAN_POINT('',(5.76292026667036,133.2,8.03205448016022));
#69261=CARTESIAN_POINT('Origin',(4.98510280736516,133.2,8.31489719263484));
#69262=CARTESIAN_POINT('',(5.448782865196,144.,8.14628626251453));
#69263=CARTESIAN_POINT('',(5.448782865196,138.6,8.14628626251453));
#69264=CARTESIAN_POINT('',(5.76292026667036,144.,8.03205448016022));
#69265=CARTESIAN_POINT('Origin',(5.25026785031011,144.,8.04973214968988));
#69266=CARTESIAN_POINT('Origin',(0.,144.,13.3));
#69267=CARTESIAN_POINT('Origin',(4.30156901985006,133.2,6.78394260557304));
#69268=CARTESIAN_POINT('',(4.23788553664207,144.,7.11208224211731));
#69269=CARTESIAN_POINT('',(4.23788553664207,133.2,7.11208224211731));
#69270=CARTESIAN_POINT('',(4.23788553664207,138.6,7.11208224211731));
#69271=CARTESIAN_POINT('',(4.14388602866193,144.,7.59643018965662));
#69272=CARTESIAN_POINT('',(4.14388602866193,144.,7.59643018965662));
#69273=CARTESIAN_POINT('',(4.14388602866193,133.2,7.59643018965662));
#69274=CARTESIAN_POINT('',(4.14388602866193,133.2,7.59643018965662));
#69275=CARTESIAN_POINT('',(4.14388602866193,133.2,7.59643018965662));
#69276=CARTESIAN_POINT('Origin',(4.36430549827161,133.2,7.29304881676602));
#69277=CARTESIAN_POINT('',(4.57548085489463,133.2,7.3573595980833));
#69278=CARTESIAN_POINT('Origin',(0.,133.2,13.3));
#69279=CARTESIAN_POINT('',(4.86788091591252,133.2,7.19539228217777));
#69280=CARTESIAN_POINT('Origin',(4.14388602866193,133.2,7.59643018965662));
#69281=CARTESIAN_POINT('',(4.57548085489463,144.,7.3573595980833));
#69282=CARTESIAN_POINT('',(4.57548085489463,138.6,7.3573595980833));
#69283=CARTESIAN_POINT('',(4.86788091591252,144.,7.19539228217777));
#69284=CARTESIAN_POINT('Origin',(4.36430549827161,144.,7.29304881676602));
#69285=CARTESIAN_POINT('Origin',(0.,144.,13.3));
#69286=CARTESIAN_POINT('Origin',(3.22927361450254,133.2,6.19125243642189));
#69287=CARTESIAN_POINT('',(3.21770652915082,144.,6.52531442115133));
#69288=CARTESIAN_POINT('',(3.21770652915082,133.2,6.52531442115133));
#69289=CARTESIAN_POINT('',(3.21770652915082,138.6,6.52531442115133));
#69290=CARTESIAN_POINT('',(3.2006330231638,144.,7.01840400447201));
#69291=CARTESIAN_POINT('',(3.2006330231638,144.,7.01840400447201));
#69292=CARTESIAN_POINT('',(3.2006330231638,133.2,7.01840400447201));
#69293=CARTESIAN_POINT('',(3.2006330231638,133.2,7.01840400447201));
#69294=CARTESIAN_POINT('',(3.2006330231638,133.2,7.01840400447201));
#69295=CARTESIAN_POINT('Origin',(3.37087946056613,133.2,6.68427655790137));
#69296=CARTESIAN_POINT('',(3.5895153207954,133.2,6.71476046284001));
#69297=CARTESIAN_POINT('Origin',(0.,133.2,13.3));
#69298=CARTESIAN_POINT('',(3.85297818143439,133.2,6.50904578623957));
#69299=CARTESIAN_POINT('Origin',(3.2006330231638,133.2,7.01840400447201));
#69300=CARTESIAN_POINT('',(3.5895153207954,144.,6.71476046284001));
#69301=CARTESIAN_POINT('',(3.5895153207954,138.6,6.71476046284001));
#69302=CARTESIAN_POINT('',(3.85297818143439,144.,6.50904578623957));
#69303=CARTESIAN_POINT('Origin',(3.37087946056613,144.,6.68427655790137));
#69304=CARTESIAN_POINT('Origin',(0.,144.,13.3));
#69305=CARTESIAN_POINT('Origin',(2.07746277542129,133.2,5.77360322486657));
#69306=CARTESIAN_POINT('',(2.11829690795615,144.,6.10536184302898));
#69307=CARTESIAN_POINT('',(2.11829690795615,133.2,6.10536184302898));
#69308=CARTESIAN_POINT('',(2.11829690795615,138.6,6.10536184302898));
#69309=CARTESIAN_POINT('',(2.17856981034338,144.,6.59505156011917));
#69310=CARTESIAN_POINT('',(2.17856981034338,144.,6.59505156011917));
#69311=CARTESIAN_POINT('',(2.17856981034338,133.2,6.59505156011917));
#69312=CARTESIAN_POINT('',(2.17856981034338,133.2,6.59505156011917));
#69313=CARTESIAN_POINT('',(2.17856981034338,133.2,6.59505156011917));
#69314=CARTESIAN_POINT('Origin',(2.29445118323398,133.2,6.23840536650849));
#69315=CARTESIAN_POINT('',(2.51516400657983,133.2,6.23431178015862));
#69316=CARTESIAN_POINT('Origin',(0.,133.2,13.3));
#69317=CARTESIAN_POINT('',(2.74320233682789,133.2,5.98991512092903));
#69318=CARTESIAN_POINT('Origin',(2.17856981034338,133.2,6.59505156011917));
#69319=CARTESIAN_POINT('',(2.51516400657983,144.,6.23431178015862));
#69320=CARTESIAN_POINT('',(2.51516400657983,138.6,6.23431178015862));
#69321=CARTESIAN_POINT('',(2.74320233682789,144.,5.98991512092903));
#69322=CARTESIAN_POINT('Origin',(2.29445118323398,144.,6.23840536650849));
#69323=CARTESIAN_POINT('Origin',(0.,144.,13.3));
#69324=CARTESIAN_POINT('Origin',(0.874497908105503,133.2,5.54127888059385));
#69325=CARTESIAN_POINT('',(0.96672778666323,144.,5.86256513396634));
#69326=CARTESIAN_POINT('',(0.96672778666323,133.2,5.86256513396634));
#69327=CARTESIAN_POINT('',(0.966727786663231,138.6,5.86256513396633));
#69328=CARTESIAN_POINT('',(1.10286297853363,144.,6.33679719880428));
#69329=CARTESIAN_POINT('',(1.10286297853363,144.,6.33679719880428));
#69330=CARTESIAN_POINT('',(1.10286297853363,133.2,6.33679719880428));
#69331=CARTESIAN_POINT('',(1.10286297853363,133.2,6.33679719880428));
#69332=CARTESIAN_POINT('',(1.10286297853363,133.2,6.33679719880428));
#69333=CARTESIAN_POINT('Origin',(1.16152590292371,133.2,5.9664140710811));
#69334=CARTESIAN_POINT('',(1.37888100717151,133.2,5.92784379112449));
#69335=CARTESIAN_POINT('Origin',(0.,133.2,13.3));
#69336=CARTESIAN_POINT('',(1.5658797465221,133.2,5.65078300612201));
#69337=CARTESIAN_POINT('Origin',(1.10286297853363,133.2,6.33679719880428));
#69338=CARTESIAN_POINT('',(1.37888100717151,144.,5.92784379112449));
#69339=CARTESIAN_POINT('',(1.3788810071715,138.6,5.92784379112449));
#69340=CARTESIAN_POINT('',(1.5658797465221,144.,5.65078300612201));
#69341=CARTESIAN_POINT('Origin',(1.16152590292371,144.,5.9664140710811));
#69342=CARTESIAN_POINT('Origin',(0.,144.,13.3));
#69343=CARTESIAN_POINT('Origin',(-0.350000000000001,133.2,5.5));
#69344=CARTESIAN_POINT('',(-0.208645381122922,144.,5.8029027547366));
#69345=CARTESIAN_POINT('',(-0.208645381122922,133.2,5.8029027547366));
#69346=CARTESIAN_POINT('',(-0.208645381122922,138.6,5.8029027547366));
#69347=CARTESIAN_POINT('',(-2.22044604925031E-15,144.,6.25));
#69348=CARTESIAN_POINT('',(-2.22044604925031E-15,144.,6.25));
#69349=CARTESIAN_POINT('',(-2.22044604925031E-15,133.2,6.25));
#69350=CARTESIAN_POINT('',(-2.22044604925031E-15,133.2,6.25));
#69351=CARTESIAN_POINT('',(-2.22044604925031E-15,133.2,6.25));
#69352=CARTESIAN_POINT('Origin',(-2.22044604925031E-15,133.2,5.875));
#69353=CARTESIAN_POINT('',(0.208645381122917,133.2,5.8029027547366));
#69354=CARTESIAN_POINT('Origin',(0.,133.2,13.3));
#69355=CARTESIAN_POINT('',(0.349999999999997,133.2,5.5));
#69356=CARTESIAN_POINT('Origin',(-2.22044604925031E-15,133.2,6.25));
#69357=CARTESIAN_POINT('',(0.208645381122917,144.,5.8029027547366));
#69358=CARTESIAN_POINT('',(0.208645381122917,138.6,5.8029027547366));
#69359=CARTESIAN_POINT('',(0.349999999999997,144.,5.5));
#69360=CARTESIAN_POINT('Origin',(-2.22044604925031E-15,144.,5.875));
#69361=CARTESIAN_POINT('Origin',(0.,144.,13.3));
#69362=CARTESIAN_POINT('Origin',(-1.5658797465221,133.2,5.65078300612201));
#69363=CARTESIAN_POINT('',(-1.37888100717151,144.,5.92784379112449));
#69364=CARTESIAN_POINT('',(-1.37888100717151,133.2,5.92784379112449));
#69365=CARTESIAN_POINT('',(-1.37888100717151,138.6,5.92784379112449));
#69366=CARTESIAN_POINT('',(-1.10286297853363,144.,6.33679719880428));
#69367=CARTESIAN_POINT('',(-1.10286297853363,144.,6.33679719880428));
#69368=CARTESIAN_POINT('',(-1.10286297853363,133.2,6.33679719880428));
#69369=CARTESIAN_POINT('',(-1.10286297853363,133.2,6.33679719880428));
#69370=CARTESIAN_POINT('',(-1.10286297853363,133.2,6.33679719880428));
#69371=CARTESIAN_POINT('Origin',(-1.16152590292371,133.2,5.9664140710811));
#69372=CARTESIAN_POINT('',(-0.966727786663231,133.2,5.86256513396633));
#69373=CARTESIAN_POINT('Origin',(0.,133.2,13.3));
#69374=CARTESIAN_POINT('',(-0.874497908105503,133.2,5.54127888059384));
#69375=CARTESIAN_POINT('Origin',(-1.10286297853363,133.2,6.33679719880428));
#69376=CARTESIAN_POINT('',(-0.966727786663231,144.,5.86256513396633));
#69377=CARTESIAN_POINT('',(-0.966727786663235,138.6,5.86256513396633));
#69378=CARTESIAN_POINT('',(-0.874497908105503,144.,5.54127888059384));
#69379=CARTESIAN_POINT('Origin',(-1.16152590292371,144.,5.9664140710811));
#69380=CARTESIAN_POINT('Origin',(0.,144.,13.3));
#69381=CARTESIAN_POINT('Origin',(-2.7432023368279,133.2,5.98991512092903));
#69382=CARTESIAN_POINT('',(-2.51516400657983,144.,6.23431178015862));
#69383=CARTESIAN_POINT('',(-2.51516400657983,133.2,6.23431178015862));
#69384=CARTESIAN_POINT('',(-2.51516400657984,138.6,6.23431178015862));
#69385=CARTESIAN_POINT('',(-2.17856981034338,144.,6.59505156011917));
#69386=CARTESIAN_POINT('',(-2.17856981034338,144.,6.59505156011917));
#69387=CARTESIAN_POINT('',(-2.17856981034338,133.2,6.59505156011917));
#69388=CARTESIAN_POINT('',(-2.17856981034338,133.2,6.59505156011917));
#69389=CARTESIAN_POINT('',(-2.17856981034338,133.2,6.59505156011917));
#69390=CARTESIAN_POINT('Origin',(-2.29445118323399,133.2,6.23840536650849));
#69391=CARTESIAN_POINT('',(-2.11829690795616,133.2,6.10536184302898));
#69392=CARTESIAN_POINT('Origin',(0.,133.2,13.3));
#69393=CARTESIAN_POINT('',(-2.07746277542129,133.2,5.77360322486657));
#69394=CARTESIAN_POINT('Origin',(-2.17856981034338,133.2,6.59505156011917));
#69395=CARTESIAN_POINT('',(-2.11829690795616,144.,6.10536184302898));
#69396=CARTESIAN_POINT('',(-2.11829690795616,138.6,6.10536184302898));
#69397=CARTESIAN_POINT('',(-2.07746277542129,144.,5.77360322486657));
#69398=CARTESIAN_POINT('Origin',(-2.29445118323399,144.,6.23840536650849));
#69399=CARTESIAN_POINT('Origin',(0.,144.,13.3));
#69400=CARTESIAN_POINT('Origin',(-3.85297818143439,133.2,6.50904578623957));
#69401=CARTESIAN_POINT('',(-3.5895153207954,144.,6.71476046284001));
#69402=CARTESIAN_POINT('',(-3.5895153207954,133.2,6.71476046284001));
#69403=CARTESIAN_POINT('',(-3.5895153207954,138.6,6.71476046284001));
#69404=CARTESIAN_POINT('',(-3.20063302316381,144.,7.01840400447201));
#69405=CARTESIAN_POINT('',(-3.20063302316381,144.,7.01840400447201));
#69406=CARTESIAN_POINT('',(-3.20063302316381,133.2,7.01840400447201));
#69407=CARTESIAN_POINT('',(-3.20063302316381,133.2,7.01840400447201));
#69408=CARTESIAN_POINT('',(-3.20063302316381,133.2,7.01840400447201));
#69409=CARTESIAN_POINT('Origin',(-3.37087946056614,133.2,6.68427655790137));
#69410=CARTESIAN_POINT('',(-3.21770652915082,133.2,6.52531442115133));
#69411=CARTESIAN_POINT('Origin',(0.,133.2,13.3));
#69412=CARTESIAN_POINT('',(-3.22927361450254,133.2,6.19125243642189));
#69413=CARTESIAN_POINT('Origin',(-3.20063302316381,133.2,7.01840400447201));
#69414=CARTESIAN_POINT('',(-3.21770652915082,144.,6.52531442115133));
#69415=CARTESIAN_POINT('',(-3.21770652915082,138.6,6.52531442115133));
#69416=CARTESIAN_POINT('',(-3.22927361450254,144.,6.19125243642189));
#69417=CARTESIAN_POINT('Origin',(-3.37087946056614,144.,6.68427655790137));
#69418=CARTESIAN_POINT('Origin',(0.,144.,13.3));
#69419=CARTESIAN_POINT('Origin',(-4.86788091591252,133.2,7.19539228217778));
#69420=CARTESIAN_POINT('',(-4.57548085489463,144.,7.3573595980833));
#69421=CARTESIAN_POINT('',(-4.57548085489463,133.2,7.3573595980833));
#69422=CARTESIAN_POINT('',(-4.57548085489463,138.6,7.3573595980833));
#69423=CARTESIAN_POINT('',(-4.14388602866194,144.,7.59643018965662));
#69424=CARTESIAN_POINT('',(-4.14388602866194,144.,7.59643018965662));
#69425=CARTESIAN_POINT('',(-4.14388602866194,133.2,7.59643018965662));
#69426=CARTESIAN_POINT('',(-4.14388602866194,133.2,7.59643018965662));
#69427=CARTESIAN_POINT('',(-4.14388602866194,133.2,7.59643018965662));
#69428=CARTESIAN_POINT('Origin',(-4.36430549827161,133.2,7.29304881676602));
#69429=CARTESIAN_POINT('',(-4.23788553664207,133.2,7.11208224211731));
#69430=CARTESIAN_POINT('Origin',(0.,133.2,13.3));
#69431=CARTESIAN_POINT('',(-4.30156901985006,133.2,6.78394260557305));
#69432=CARTESIAN_POINT('Origin',(-4.14388602866194,133.2,7.59643018965662));
#69433=CARTESIAN_POINT('',(-4.23788553664207,144.,7.11208224211731));
#69434=CARTESIAN_POINT('',(-4.23788553664207,138.6,7.11208224211731));
#69435=CARTESIAN_POINT('',(-4.30156901985006,144.,6.78394260557305));
#69436=CARTESIAN_POINT('Origin',(-4.36430549827161,144.,7.29304881676602));
#69437=CARTESIAN_POINT('Origin',(0.,144.,13.3));
#69438=CARTESIAN_POINT('Origin',(-5.76292026667036,133.2,8.03205448016022));
#69439=CARTESIAN_POINT('',(-5.44878286519601,144.,8.14628626251454));
#69440=CARTESIAN_POINT('',(-5.44878286519601,133.2,8.14628626251454));
#69441=CARTESIAN_POINT('',(-5.44878286519601,138.6,8.14628626251453));
#69442=CARTESIAN_POINT('',(-4.98510280736516,144.,8.31489719263484));
#69443=CARTESIAN_POINT('',(-4.98510280736516,144.,8.31489719263484));
#69444=CARTESIAN_POINT('',(-4.98510280736516,133.2,8.31489719263484));
#69445=CARTESIAN_POINT('',(-4.98510280736516,133.2,8.31489719263484));
#69446=CARTESIAN_POINT('',(-4.98510280736516,133.2,8.31489719263484));
#69447=CARTESIAN_POINT('Origin',(-5.25026785031012,133.2,8.04973214968989));
#69448=CARTESIAN_POINT('',(-5.15371373748547,133.2,7.851217134804));
#69449=CARTESIAN_POINT('Origin',(0.,133.2,13.3));
#69450=CARTESIAN_POINT('',(-5.26794551983978,133.2,7.53707973332964));
#69451=CARTESIAN_POINT('Origin',(-4.98510280736516,133.2,8.31489719263484));
#69452=CARTESIAN_POINT('',(-5.15371373748547,144.,7.851217134804));
#69453=CARTESIAN_POINT('',(-5.15371373748547,138.6,7.851217134804));
#69454=CARTESIAN_POINT('',(-5.26794551983978,144.,7.53707973332964));
#69455=CARTESIAN_POINT('Origin',(-5.25026785031012,144.,8.04973214968989));
#69456=CARTESIAN_POINT('Origin',(0.,144.,13.3));
#69457=CARTESIAN_POINT('Origin',(-6.51605739442696,133.2,8.99843098014994));
#69458=CARTESIAN_POINT('',(-6.18791775788269,144.,9.06211446335793));
#69459=CARTESIAN_POINT('',(-6.18791775788269,133.2,9.06211446335793));
#69460=CARTESIAN_POINT('',(-6.18791775788269,138.6,9.06211446335793));
#69461=CARTESIAN_POINT('',(-5.70356981034338,144.,9.15611397133807));
#69462=CARTESIAN_POINT('',(-5.70356981034338,144.,9.15611397133807));
#69463=CARTESIAN_POINT('',(-5.70356981034338,133.2,9.15611397133807));
#69464=CARTESIAN_POINT('',(-5.70356981034338,133.2,9.15611397133807));
#69465=CARTESIAN_POINT('',(-5.70356981034338,133.2,9.15611397133807));
#69466=CARTESIAN_POINT('Origin',(-6.00695118323399,133.2,8.93569450172839));
#69467=CARTESIAN_POINT('',(-5.9426404019167,133.2,8.72451914510537));
#69468=CARTESIAN_POINT('Origin',(0.,133.2,13.3));
#69469=CARTESIAN_POINT('',(-6.10460771782223,133.2,8.43211908408748));
#69470=CARTESIAN_POINT('Origin',(-5.70356981034338,133.2,9.15611397133807));
#69471=CARTESIAN_POINT('',(-5.9426404019167,144.,8.72451914510537));
#69472=CARTESIAN_POINT('',(-5.9426404019167,138.6,8.72451914510537));
#69473=CARTESIAN_POINT('',(-6.10460771782223,144.,8.43211908408748));
#69474=CARTESIAN_POINT('Origin',(-6.00695118323399,144.,8.93569450172839));
#69475=CARTESIAN_POINT('Origin',(0.,144.,13.3));
#69476=CARTESIAN_POINT('Origin',(-7.10874756357811,133.2,10.0707263854975));
#69477=CARTESIAN_POINT('',(-6.77468557884867,144.,10.0822934708492));
#69478=CARTESIAN_POINT('',(-6.77468557884867,133.2,10.0822934708492));
#69479=CARTESIAN_POINT('',(-6.77468557884867,138.6,10.0822934708492));
#69480=CARTESIAN_POINT('',(-6.28159599552799,144.,10.0993669768362));
#69481=CARTESIAN_POINT('',(-6.28159599552799,144.,10.0993669768362));
#69482=CARTESIAN_POINT('',(-6.28159599552799,133.2,10.0993669768362));
#69483=CARTESIAN_POINT('',(-6.28159599552799,133.2,10.0993669768362));
#69484=CARTESIAN_POINT('',(-6.28159599552799,133.2,10.0993669768362));
#69485=CARTESIAN_POINT('Origin',(-6.61572344209863,133.2,9.92912053943387));
#69486=CARTESIAN_POINT('',(-6.58523953715999,133.2,9.7104846792046));
#69487=CARTESIAN_POINT('Origin',(0.,133.2,13.3));
#69488=CARTESIAN_POINT('',(-6.79095421376043,133.2,9.44702181856561));
#69489=CARTESIAN_POINT('Origin',(-6.28159599552799,133.2,10.0993669768362));
#69490=CARTESIAN_POINT('',(-6.58523953715999,144.,9.7104846792046));
#69491=CARTESIAN_POINT('',(-6.58523953715999,138.6,9.7104846792046));
#69492=CARTESIAN_POINT('',(-6.79095421376043,144.,9.44702181856561));
#69493=CARTESIAN_POINT('Origin',(-6.61572344209863,144.,9.92912053943387));
#69494=CARTESIAN_POINT('Origin',(0.,144.,13.3));
#69495=CARTESIAN_POINT('Origin',(-7.52639677513343,133.2,11.2225372245787));
#69496=CARTESIAN_POINT('',(-7.19463815697102,144.,11.1817030920438));
#69497=CARTESIAN_POINT('',(-7.19463815697102,133.2,11.1817030920438));
#69498=CARTESIAN_POINT('',(-7.19463815697102,138.6,11.1817030920438));
#69499=CARTESIAN_POINT('',(-6.70494843988083,144.,11.1214301896566));
#69500=CARTESIAN_POINT('',(-6.70494843988083,144.,11.1214301896566));
#69501=CARTESIAN_POINT('',(-6.70494843988083,133.2,11.1214301896566));
#69502=CARTESIAN_POINT('',(-6.70494843988083,133.2,11.1214301896566));
#69503=CARTESIAN_POINT('',(-6.70494843988083,133.2,11.1214301896566));
#69504=CARTESIAN_POINT('Origin',(-7.06159463349151,133.2,11.005548816766));
#69505=CARTESIAN_POINT('',(-7.06568821984138,133.2,10.7848359934202));
